#54233 = CARTESIAN_POINT ( 'NONE',  ( -4.589925132946514275, -63.93473983707485786, 3.864926970398267603 ) ) ;
#54234 = CARTESIAN_POINT ( 'NONE',  ( 51.48757442383973881, 38.95383793068620548, -37.45149417477089315 ) ) ;
#54235 = CARTESIAN_POINT ( 'NONE',  ( -40.15309039158411508, 485.1828724906129082, -4.320808352504673877 ) ) ;
#54236 = CARTESIAN_POINT ( 'NONE',  ( 7.737898857161403576, 302.4298210949973509, -10.02991386142804231 ) ) ;
#54237 = CARTESIAN_POINT ( 'NONE',  ( 62.59984008646965492, -56.86289542963405808, 88.13664758048848569 ) ) ;
#54238 = VERTEX_POINT ( 'NONE', #90437 ) ;
#54239 = FACE_OUTER_BOUND ( 'NONE', #92124, .T. ) ;
#54240 = CARTESIAN_POINT ( 'NONE',  ( -76.12537862032631608, -38.35598417008158378, -28.58435412235099804 ) ) ;
#54241 = CARTESIAN_POINT ( 'NONE',  ( -42.68083702883377839, 436.2686870323770449, 7.148029379848837905 ) ) ;
#54242 = CARTESIAN_POINT ( 'NONE',  ( -9.383347720677482684, 51.32558664833128148, 3.724917079647517948 ) ) ;
#54243 = AXIS2_PLACEMENT_3D ( 'NONE', #80493, #62751, #48655 ) ;
#54244 = ORIENTED_EDGE ( 'NONE', *, *, #53710, .F. ) ;
#54245 =( NAMED_UNIT ( * ) PLANE_ANGLE_UNIT ( ) SI_UNIT ( $, .RADIAN. ) );
#54246 = DIRECTION ( 'NONE',  ( 0.5735764363510491570, -0.8191520442889895781, 1.003171929053522035E-16 ) ) ;
#54247 = CARTESIAN_POINT ( 'NONE',  ( -72.10178200369317381, -60.00000000000000711, -25.50777580964439650 ) ) ;
#54248 = AXIS2_PLACEMENT_3D ( 'NONE', #55413, #76648, #79175 ) ;
#54249 = FACE_OUTER_BOUND ( 'NONE', #82041, .T. ) ;
#54250 = EDGE_CURVE ( 'NONE', #70585, #86317, #73253, .T. ) ;
#54251 = MECHANICAL_DESIGN_GEOMETRIC_PRESENTATION_REPRESENTATION (  '', ( #35371 ), #81817 ) ;
#54252 = FACE_OUTER_BOUND ( 'NONE', #95799, .T. ) ;
#54253 = VECTOR ( 'NONE', #14178, 1000.000000000000227 ) ;
#54254 = CARTESIAN_POINT ( 'NONE',  ( 5.727634848076682772, 4.575561887447793019, -6.326622577870439912 ) ) ;
#54255 = CARTESIAN_POINT ( 'NONE',  ( 86.05395271266333168, -39.20869856352000937, 187.0836467292549514 ) ) ;
#54256 = CARTESIAN_POINT ( 'NONE',  ( 67.48317336153286305, 6.856755485862130937E-15, 0.000000000000000000 ) ) ;
#54257 = CARTESIAN_POINT ( 'NONE',  ( -9.993721417938997931, 7.509139500188190652, 0.000000000000000000 ) ) ;
#54258 = CARTESIAN_POINT ( 'NONE',  ( 87.04245038058458306, 5.000000000000023093, 6.123233995736781074E-16 ) ) ;
#54259 = CARTESIAN_POINT ( 'NONE',  ( 61.40732561923240951, -29.45172577994906860, -24.51876011215350104 ) ) ;
#54260 = PRESENTATION_STYLE_ASSIGNMENT (( #96359 ) ) ;
#54261 = CARTESIAN_POINT ( 'NONE',  ( 5.947762761376474749, -2.501851166488376688, 6.500000000000000000 ) ) ;
#54262 = CARTESIAN_POINT ( 'NONE',  ( 34.17980567228813271, 435.1524039838096201, 10.79291224410167338 ) ) ;
#54263 =( BOUNDED_SURFACE ( )  B_SPLINE_SURFACE ( 3, 2, ( 
 ( #46301, #45765, #12322 ),
 ( #102944, #28553, #70581 ),
 ( #11786, #79190, #78126 ),
 ( #77605, #20493, #22041 ),
 ( #45247, #78641, #53331 ),
 ( #103988, #53848, #54352 ),
 ( #4245, #86779, #61434 ),
 ( #29108, #12848, #38234 ),
 ( #4779, #52787, #44716 ),
 ( #103468, #71098, #29617 ),
 ( #86250, #3723, #11247 ),
 ( #94330, #30132, #60898 ),
 ( #63018, #95916, #62489 ),
 ( #3179, #28029, #54897 ),
 ( #95380, #68994, #21518 ),
 ( #44176, #77065, #101869 ),
 ( #93788, #36653, #19947 ),
 ( #65666, #55942, #88881 ),
 ( #88359, #6888, #56492 ),
 ( #14970, #47867, #5827 ),
 ( #13907, #55426, #30673 ),
 ( #105069, #48403, #81293 ),
 ( #105584, #80773, #38748 ),
 ( #64610, #31724, #98547 ),
 ( #81819, #96970, #32249 ),
 ( #106641, #32792, #14435 ),
 ( #24698, #97479, #46821 ),
 ( #89421, #23634, #39809 ),
 ( #89936, #15513, #72683 ),
 ( #7409, #39283, #40322 ),
 ( #47345, #57022, #73199 ),
 ( #106101, #72161, #65130 ),
 ( #16043, #7943, #48923 ),
 ( #98026, #24178, #40849 ),
 ( #73742, #87828, #79718 ),
 ( #71617, #104519, #63559 ),
 ( #96452, #22589, #80237 ),
 ( #6341, #31209, #64094 ),
 ( #23105, #18200, #67794 ),
 ( #50521, #82374, #83971 ),
 ( #75337, #68332, #57548 ),
 ( #41914, #2513, #50006 ),
 ( #83436, #1438, #90469 ),
 ( #26320, #16581, #99615 ),
 ( #58648, #33319, #59717 ),
 ( #91550, #99072, #9534 ),
 ( #10082, #74800, #25236 ),
 ( #17658, #92592, #67275 ),
 ( #9008, #75879, #42446 ),
 ( #51597, #18748, #42991 ),
 ( #34399, #100155, #59181 ),
 ( #1979, #8481, #92060 ),
 ( #84516, #66191, #49467 ),
 ( #10605, #66731, #34926 ),
 ( #882, #100680, #33859 ),
 ( #51054, #26846, #43523 ),
 ( #76399, #58093, #91022 ),
 ( #35460, #101229, #41386 ),
 ( #74277, #17128, #351 ),
 ( #25792, #82911, #11126 ),
 ( #94748, #20898, #53210 ),
 ( #78530, #70458, #94200 ),
 ( #3055, #53732, #37056 ),
 ( #12730, #45133, #44596 ),
 ( #61851, #68877, #86660 ),
 ( #103355, #77486, #3598 ),
 ( #101750, #102282, #86130 ),
 ( #36535, #69400, #19304 ),
 ( #27384, #36005, #44052 ),
 ( #27920, #20370, #45653 ),
 ( #28430, #60783, #93673 ),
 ( #4661, #12203, #28985 ),
 ( #19824, #60264, #78010 ),
 ( #61311, #4127, #52659 ),
 ( #69924, #85590, #37595 ),
 ( #29503, #93133, #102823 ),
 ( #11664, #52128, #85044 ),
 ( #76942, #51393, #91868 ),
 ( #27170, #50330, #51925 ),
 ( #101555, #17993, #50854 ) ),
 .UNSPECIFIED., .F., .F., .F. ) 
 B_SPLINE_SURFACE_WITH_KNOTS ( ( 4, 2, 2, 2, 2, 2, 2, 2, 2, 2, 2, 2, 2, 2, 2, 2, 2, 2, 2, 2, 2, 2, 2, 2, 2, 2, 2, 2, 2, 2, 2, 2, 2, 2, 2, 2, 2, 2, 2, 4 ),
 ( 3, 3 ),
 ( 0.07172314469012842919, 0.08973265255323484291, 0.1077421604163412705, 0.1257516682794476703, 0.1347564222110008703, 0.1437611761425540979, 0.1617706840056605255, 0.1707754379372137254, 0.1797801918687669254, 0.1820313803516552253, 0.1842825688345435253, 0.1887849458003201253, 0.1932873227660967252, 0.1955385112489850252, 0.1977896997318733252, 0.1989152939733174752, 0.1994780910940395502, 0.2000408882147616252, 0.2022920766976499252, 0.2045432651805382251, 0.2051060623012603001, 0.2053874608616213515, 0.2056688594219823751, 0.2067944536634265251, 0.2079200479048706751, 0.2080607471850511869, 0.2082014464652316987, 0.2084828450255927501, 0.2090456421463148251, 0.2101712363877589751, 0.2104526349481199987, 0.2107340335084810501, 0.2112968306292031251, 0.2124224248706472751, 0.2129852219913693501, 0.2130555716314596060, 0.2131259212715498896, 0.2132666205517304014, 0.2135480191120914251, 0.2157992075949797528 ),
 ( 0.000000000000000000, 1.000000000000000000 ),
 .UNSPECIFIED. ) 
 GEOMETRIC_REPRESENTATION_ITEM ( )  RATIONAL_B_SPLINE_SURFACE ( (
 ( 1.000000000000000000, 0.7071066916777324352, 1.000000000000000000),
 ( 1.000000000000000000, 0.7071066384723879716, 1.000000000000000000),
 ( 1.000000000000000000, 0.7071067819036740421, 1.000000000000000000),
 ( 1.000000000000000000, 0.7071067819036740421, 1.000000000000000000),
 ( 1.000000000000000000, 0.7071067821253883556, 1.000000000000000000),
 ( 1.000000000000000000, 0.7071067821253883556, 1.000000000000000000),
 ( 1.000000000000000000, 0.7071082347912200916, 1.000000000000000000),
 ( 1.000000000000000000, 0.7071090860269371170, 1.000000000000000000),
 ( 1.000000000000000000, 0.7071085999063239091, 1.000000000000000000),
 ( 1.000000000000000000, 0.7071071393025897267, 1.000000000000000000),
 ( 1.000000000000000000, 0.7071064603873742360, 1.000000000000000000),
 ( 1.000000000000000000, 0.7071084468636777975, 1.000000000000000000),
 ( 1.000000000000000000, 0.7071099459167716761, 1.000000000000000000),
 ( 1.000000000000000000, 0.7071070620195699652, 1.000000000000000000),
 ( 1.000000000000000000, 0.7071067638254444621, 1.000000000000000000),
 ( 1.000000000000000000, 0.7071094983174432969, 1.000000000000000000),
 ( 1.000000000000000000, 0.7071073521351076696, 1.000000000000000000),
 ( 1.000000000000000000, 0.7071067110094644281, 1.000000000000000000),
 ( 1.000000000000000000, 0.7071074718365022438, 1.000000000000000000),
 ( 1.000000000000000000, 0.7071137944410639253, 1.000000000000000000),
 ( 1.000000000000000000, 0.7071181761060342241, 1.000000000000000000),
 ( 1.000000000000000000, 0.7071288868279509421, 1.000000000000000000),
 ( 1.000000000000000000, 0.7071314869358752420, 1.000000000000000000),
 ( 1.000000000000000000, 0.7071211158780618122, 1.000000000000000000),
 ( 1.000000000000000000, 0.7071075228484042796, 1.000000000000000000),
 ( 1.000000000000000000, 0.7071064472611667817, 1.000000000000000000),
 ( 1.000000000000000000, 0.7071094939932405232, 1.000000000000000000),
 ( 1.000000000000000000, 0.7071117979890746419, 1.000000000000000000),
 ( 1.000000000000000000, 0.7071112387139774080, 1.000000000000000000),
 ( 1.000000000000000000, 0.7071089882604711940, 1.000000000000000000),
 ( 1.000000000000000000, 0.7071080815320003321, 1.000000000000000000),
 ( 1.000000000000000000, 0.7071071532410159177, 1.000000000000000000),
 ( 1.000000000000000000, 0.7071069183921528944, 1.000000000000000000),
 ( 1.000000000000000000, 0.7071067316882134746, 1.000000000000000000),
 ( 1.000000000000000000, 0.7071072160745824897, 1.000000000000000000),
 ( 1.000000000000000000, 0.7071281552871109266, 1.000000000000000000),
 ( 1.000000000000000000, 0.7071788308493717201, 1.000000000000000000),
 ( 1.000000000000000000, 0.7072040914959526470, 1.000000000000000000),
 ( 1.000000000000000000, 0.7071729554399738271, 1.000000000000000000),
 ( 1.000000000000000000, 0.7071271541534743799, 1.000000000000000000),
 ( 1.000000000000000000, 0.7071184695976129309, 1.000000000000000000),
 ( 1.000000000000000000, 0.7071100320398184813, 1.000000000000000000),
 ( 1.000000000000000000, 0.7071080004622726234, 1.000000000000000000),
 ( 1.000000000000000000, 0.7071063588341449657, 1.000000000000000000),
 ( 1.000000000000000000, 0.7071068098800528112, 1.000000000000000000),
 ( 1.000000000000000000, 0.7071083434742995166, 1.000000000000000000),
 ( 1.000000000000000000, 0.7071118442609979349, 1.000000000000000000),
 ( 1.000000000000000000, 0.7071122315782686352, 1.000000000000000000),
 ( 1.000000000000000000, 0.7071084657487585190, 1.000000000000000000),
 ( 1.000000000000000000, 0.7071069086593241293, 1.000000000000000000),
 ( 1.000000000000000000, 0.7071067970953980319, 1.000000000000000000),
 ( 1.000000000000000000, 0.7071067683750767996, 1.000000000000000000),
 ( 1.000000000000000000, 0.7071066806290805529, 1.000000000000000000),
 ( 1.000000000000000000, 0.7071060773180442016, 1.000000000000000000),
 ( 1.000000000000000000, 0.7071053327435640190, 1.000000000000000000),
 ( 1.000000000000000000, 0.7071028992638964672, 1.000000000000000000),
 ( 1.000000000000000000, 0.7071010927699721282, 1.000000000000000000),
 ( 1.000000000000000000, 0.7070987750015783613, 1.000000000000000000),
 ( 1.000000000000000000, 0.7071026859636611039, 1.000000000000000000),
 ( 1.000000000000000000, 0.7071061702207726007, 1.000000000000000000),
 ( 1.000000000000000000, 0.7071067000110781153, 1.000000000000000000),
 ( 1.000000000000000000, 0.7071068455174084333, 1.000000000000000000),
 ( 1.000000000000000000, 0.7071077971994959022, 1.000000000000000000),
 ( 1.000000000000000000, 0.7071127875002619634, 1.000000000000000000),
 ( 1.000000000000000000, 0.7071176651463569884, 1.000000000000000000),
 ( 1.000000000000000000, 0.7071258132918983863, 1.000000000000000000),
 ( 1.000000000000000000, 0.7071208017052891259, 1.000000000000000000),
 ( 1.000000000000000000, 0.7071102148083360239, 1.000000000000000000),
 ( 1.000000000000000000, 0.7071068024654432183, 1.000000000000000000),
 ( 1.000000000000000000, 0.7071067786309011005, 1.000000000000000000),
 ( 1.000000000000000000, 0.7071068737807520987, 1.000000000000000000),
 ( 1.000000000000000000, 0.7071072399035752687, 1.000000000000000000),
 ( 1.000000000000000000, 0.7071075080362204668, 1.000000000000000000),
 ( 1.000000000000000000, 0.7071085168092843265, 1.000000000000000000),
 ( 1.000000000000000000, 0.7071094604126808569, 1.000000000000000000),
 ( 1.000000000000000000, 0.7071127524153103527, 1.000000000000000000),
 ( 1.000000000000000000, 0.7071155430753355287, 1.000000000000000000),
 ( 1.000000000000000000, 0.7071398610474239899, 1.000000000000000000),
 ( 1.000000000000000000, 0.7071223203621870290, 1.000000000000000000),
 ( 1.000000000000000000, 0.7071067811865479058, 1.000000000000000000) ) ) 
 REPRESENTATION_ITEM ( '' )  SURFACE ( )  );
#54264 = CARTESIAN_POINT ( 'NONE',  ( -100.8172700586428618, -29.99999999999999645, 180.0901824726140035 ) ) ;
#54265 = EDGE_CURVE ( 'NONE', #41982, #42449, #91851, .T. ) ;
#54266 = CARTESIAN_POINT ( 'NONE',  ( -32.17646412119387378, 464.6980787822280377, 10.84896803612861227 ) ) ;
#54267 = CARTESIAN_POINT ( 'NONE',  ( 19.20286887953066923, -57.67181979952086124, 42.11251578178057287 ) ) ;
#54268 = CARTESIAN_POINT ( 'NONE',  ( 10.12220134229128732, 44.02984809270889599, 12.90779740156146538 ) ) ;
#54269 = CARTESIAN_POINT ( 'NONE',  ( -19.51721550458913512, 41.98713167543638036, -83.66826477877489765 ) ) ;
#54270 = FACE_OUTER_BOUND ( 'NONE', #24020, .T. ) ;
#54271 = CARTESIAN_POINT ( 'NONE',  ( 2.848917157793759055E-13, 44.08548369317517768, 16.24999999999732836 ) ) ;
#54272 = DIRECTION ( 'NONE',  ( 0.000000000000000000, 0.000000000000000000, -1.000000000000000000 ) ) ;
#54273 = DIRECTION ( 'NONE',  ( -0.000000000000000000, -1.000000000000000000, -0.000000000000000000 ) ) ;
#54274 = EDGE_CURVE ( 'NONE', #35120, #61182, #94580, .T. ) ;
#54275 = CARTESIAN_POINT ( 'NONE',  ( -86.77107750842486666, -57.39365593820878075, 193.7434059132478978 ) ) ;
#54276 = ORIENTED_EDGE ( 'NONE', *, *, #16673, .F. ) ;
#54277 = CARTESIAN_POINT ( 'NONE',  ( 38.94709829052286665, 485.6592143718137891, -4.427571171338303913 ) ) ;
#54278 = CARTESIAN_POINT ( 'NONE',  ( 42.10086803841213765, 435.6552064019005570, 19.95582312411065828 ) ) ;
#54279 = CARTESIAN_POINT ( 'NONE',  ( -12.35491406422132776, -35.99458353833710333, 29.94231072834120155 ) ) ;
#54280 = CIRCLE ( 'NONE', #35410, 60.00000000000000000 ) ;
#54281 = EDGE_CURVE ( 'NONE', #102808, #42645, #18160, .T. ) ;
#54283 = CARTESIAN_POINT ( 'NONE',  ( 40.53597741959072920, 485.1143729953953994, -4.195250914663321673 ) ) ;
#54282 = CARTESIAN_POINT ( 'NONE',  ( -103.9455512838813718, -60.00000000000002842, 141.2845372866246123 ) ) ;
#54284 = ORIENTED_EDGE ( 'NONE', *, *, #56506, .F. ) ;
#54286 =( NAMED_UNIT ( * ) PLANE_ANGLE_UNIT ( ) SI_UNIT ( $, .RADIAN. ) );
#54285 = B_SPLINE_CURVE_WITH_KNOTS ( 'NONE', 3,
 ( #55254, #54719, #27990, #5655 ),
 .UNSPECIFIED., .F., .F.,
 ( 4, 4 ),
 ( 0.000000000000000000, 0.001193002000561244275 ),
 .UNSPECIFIED. ) ;
#54287 = CARTESIAN_POINT ( 'NONE',  ( 42.61340452791776556, 486.8925439250688783, 7.464118458850346194 ) ) ;
#54288 = DIRECTION ( 'NONE',  ( -1.000000000000000000, -1.224606353822377258E-16, -0.000000000000000000 ) ) ;
#54289 = CARTESIAN_POINT ( 'NONE',  ( 53.78349330513380266, -4.000000000000000888, 4.898587196589422689E-16 ) ) ;
#54290 = VERTEX_POINT ( 'NONE', #59677 ) ;
#54291 = CARTESIAN_POINT ( 'NONE',  ( 32.45420636192083919, 439.3281579392075855, 23.70224716321920511 ) ) ;
#54292 = CARTESIAN_POINT ( 'NONE',  ( -34.62906189774859200, 434.6650141781096295, 8.921436296112648989 ) ) ;
#54294 = CYLINDRICAL_SURFACE ( 'NONE', #39056, 5.000000000000002665 ) ;
#54293 =( LENGTH_UNIT ( ) NAMED_UNIT ( * ) SI_UNIT ( .MILLI., .METRE. ) );
#54295 = DIRECTION ( 'NONE',  ( 0.000000000000000000, -1.000000000000000000, 0.000000000000000000 ) ) ;
#54296 = ORIENTED_EDGE ( 'NONE', *, *, #36439, .T. ) ;
#54297 = AXIS2_PLACEMENT_3D ( 'NONE', #27682, #93444, #61079 ) ;
#54298 = ADVANCED_FACE ( 'NONE', ( #35424 ), #90980, .T. ) ;
#54299 = VERTEX_POINT ( 'NONE', #17627 ) ;
#54300 = CARTESIAN_POINT ( 'NONE',  ( -28.61915886549734367, 318.3715675768729056, 12.26331061709428205 ) ) ;
#54301 = VERTEX_POINT ( 'NONE', #101190 ) ;
#54302 = PRESENTATION_STYLE_ASSIGNMENT (( #21464 ) ) ;
#54303 = CARTESIAN_POINT ( 'NONE',  ( 21.08349330513380693, 1.593028355512270962E-15, 0.000000000000000000 ) ) ;
#54304 = CARTESIAN_POINT ( 'NONE',  ( 27.33349330513380693, 1.593028355512270962E-15, 0.000000000000000000 ) ) ;
#54305 = ORIENTED_EDGE ( 'NONE', *, *, #98498, .F. ) ;
#54306 = AXIS2_PLACEMENT_3D ( 'NONE', #32253, #25242, #49474 ) ;
#54307 = DIRECTION ( 'NONE',  ( -1.000000000000000000, -1.224606353822377258E-16, -0.000000000000000000 ) ) ;
#54308 = CARTESIAN_POINT ( 'NONE',  ( -6.914762185086790858, 41.79847498657338889, -69.55926089113090427 ) ) ;
#54309 = CARTESIAN_POINT ( 'NONE',  ( -76.85716460373025427, -60.00000000000000711, 196.0240674832539582 ) ) ;
#54310 = CARTESIAN_POINT ( 'NONE',  ( 17.81438722625302518, 5.000000000000003553, 0.000000000000000000 ) ) ;
#54311 = CARTESIAN_POINT ( 'NONE',  ( 24.77227526506132094, -60.00000000000001421, 41.10247213741922678 ) ) ;
#54312 = DIRECTION ( 'NONE',  ( 0.5735764363510468256, 0.8191520442889913545, 0.000000000000000000 ) ) ;
#54313 = CARTESIAN_POINT ( 'NONE',  ( -6.340295924924054916, 41.77218093381596020, -58.92363190012176233 ) ) ;
#54314 = AXIS2_PLACEMENT_3D ( 'NONE', #86097, #93640, #19789 ) ;
#54316 = CARTESIAN_POINT ( 'NONE',  ( 11.44797993206735853, -49.91577255025450199, 32.23882742997456319 ) ) ;
#54315 = CARTESIAN_POINT ( 'NONE',  ( -109.5929118004772818, -60.00000000000001421, 123.9174817212569621 ) ) ;
#54317 = CYLINDRICAL_SURFACE ( 'NONE', #91326, 5.000000000000002665 ) ;
#54318 = CARTESIAN_POINT ( 'NONE',  ( -48.17436038642846796, -56.82532612053482524, 53.30083711335295504 ) ) ;
#54319 = CARTESIAN_POINT ( 'NONE',  ( -7.109733192396789470, 41.69026681596732686, -59.69141549319190432 ) ) ;
#54320 = VERTEX_POINT ( 'NONE', #51019 ) ;
#54321 = CARTESIAN_POINT ( 'NONE',  ( 1.248924154308308054, 10.99719009875376230, -50.37041816597272259 ) ) ;
#54322 = AXIS2_PLACEMENT_3D ( 'NONE', #98499, #16527, #104473 ) ;
#54323 = CONICAL_SURFACE ( 'NONE', #95705, 3.309500000000001663, 0.9599310885968770357 ) ;
#54324 = DIRECTION ( 'NONE',  ( -0.000000000000000000, -0.000000000000000000, -1.000000000000000000 ) ) ;
#54325 = CARTESIAN_POINT ( 'NONE',  ( 4.472135954999580498, -10.00000000000000888, 4.000000000000000000 ) ) ;
#54326 = ORIENTED_EDGE ( 'NONE', *, *, #57418, .F. ) ;
#54327 = CARTESIAN_POINT ( 'NONE',  ( -5.719235665873437569, -7.817867488105560092, 13.77080619359168878 ) ) ;
#54328 = AXIS2_PLACEMENT_3D ( 'NONE', #21495, #23617, #39262 ) ;
#54329 = ORIENTED_EDGE ( 'NONE', *, *, #21272, .F. ) ;
#54330 = CARTESIAN_POINT ( 'NONE',  ( 89.79167478614425590, -30.00000000002385647, -11.58638050850938761 ) ) ;
#54331 = CARTESIAN_POINT ( 'NONE',  ( 46.00000000000000000, 459.9277931459794786, 6.461582622334601567 ) ) ;
#54332 = CARTESIAN_POINT ( 'NONE',  ( 0.000000000000000000, 0.000000000000000000, -6.418875477074183600 ) ) ;
#54333 = AXIS2_PLACEMENT_3D ( 'NONE', #65443, #56801, #89727 ) ;
#54334 = CARTESIAN_POINT ( 'NONE',  ( 51.76085035120648570, 42.00000000008225953, -29.83308852628573860 ) ) ;
#54335 = CARTESIAN_POINT ( 'NONE',  ( 100.1645178837010377, -30.00000000000000355, 184.8515023625643323 ) ) ;
#54336 = EDGE_CURVE ( 'NONE', #6761, #36922, #52267, .T. ) ;
#54337 = DIRECTION ( 'NONE',  ( -1.000000000000000000, -0.000000000000000000, -0.000000000000000000 ) ) ;
#54338 = ORIENTED_EDGE ( 'NONE', *, *, #90893, .T. ) ;
#54339 = VERTEX_POINT ( 'NONE', #100646 ) ;
#54340 = VERTEX_POINT ( 'NONE', #28808 ) ;
#54341 = CARTESIAN_POINT ( 'NONE',  ( -27.85348497893874509, 36.60125607490498112, 7.792768389110043437 ) ) ;
#54342 = LINE ( 'NONE', #96441, #95540 ) ;
#54343 = EDGE_CURVE ( 'NONE', #4192, #68930, #4014, .T. ) ;
#54344 = CARTESIAN_POINT ( 'NONE',  ( 3.364021409948656505, 294.8518027753228807, 9.936999415087239385 ) ) ;
#54345 = EDGE_LOOP ( 'NONE', ( #99023, #46376, #37145, #52782, #58958 ) ) ;
#54346 = DIRECTION ( 'NONE',  ( 0.000000000000000000, 0.000000000000000000, 1.000000000000000000 ) ) ;
#54347 = ORIENTED_EDGE ( 'NONE', *, *, #23274, .T. ) ;
#54348 = CARTESIAN_POINT ( 'NONE',  ( 101.7179331410454637, -38.44840262328585112, 199.8206546545780498 ) ) ;
#54349 = CARTESIAN_POINT ( 'NONE',  ( 11.60150500652189187, 15.64056042777739108, 9.649354197112575804 ) ) ;
#54350 = CARTESIAN_POINT ( 'NONE',  ( 86.16765823093783183, -60.13206058599219261, 8.614730465306884355 ) ) ;
#54351 = CARTESIAN_POINT ( 'NONE',  ( 6.169949891408688991, -6.308465495018778846, 2.073417244831591955 ) ) ;
#54352 = CARTESIAN_POINT ( 'NONE',  ( 42.78192394157753142, 397.2994584770452775, 19.86614811632973598 ) ) ;
#54353 = DIRECTION ( 'NONE',  ( -1.000000000000000000, -1.224606353822377258E-16, -0.000000000000000000 ) ) ;
#54354 = CARTESIAN_POINT ( 'NONE',  ( 0.000000000000000000, 4.000000000000003553, -10.00000000000003730 ) ) ;
#54355 = AXIS2_PLACEMENT_3D ( 'NONE', #56847, #105929, #6172 ) ;
#54356 = CARTESIAN_POINT ( 'NONE',  ( 3.105144143682717406, -0.5701562126480363979, 103.2828762868857098 ) ) ;
#54357 = ORIENTED_EDGE ( 'NONE', *, *, #32190, .T. ) ;
#54358 = ADVANCED_FACE ( 'NONE', ( #17091 ), #48800, .T. ) ;
#54359 = CARTESIAN_POINT ( 'NONE',  ( -3.313708498984765161, -10.15625000409677092, 7.999999999999998224 ) ) ;
#54360 = CARTESIAN_POINT ( 'NONE',  ( 57.70539558375507738, 6.856755485862130937E-15, 0.000000000000000000 ) ) ;
#54361 = CARTESIAN_POINT ( 'NONE',  ( -3.794355794024275585, 18.81003929889839554, 5.000000000000000000 ) ) ;
#54362 = ORIENTED_EDGE ( 'NONE', *, *, #58663, .F. ) ;
#54363 = DIRECTION ( 'NONE',  ( 0.000000000000000000, -1.000000000000000000, 0.000000000000000000 ) ) ;
#54364 = CARTESIAN_POINT ( 'NONE',  ( -33.40011937205945713, 300.9684309835628824, 3.319491984095645609 ) ) ;
#54365 = CARTESIAN_POINT ( 'NONE',  ( 26.84999999999999787, -3.309499999999999886, 4.475777889183790779E-16 ) ) ;
#54366 = SURFACE_SIDE_STYLE ('',( #99759 ) ) ;
#54367 = CARTESIAN_POINT ( 'NONE',  ( -3.313708498984760720, -21.03124999999999645, -8.000000000000000000 ) ) ;
#54368 = CARTESIAN_POINT ( 'NONE',  ( -37.98285244702580599, -27.77434865196162406, 44.84875665863523153 ) ) ;
#54369 = EDGE_CURVE ( 'NONE', #38361, #7404, #42408, .T. ) ;
#54370 = DIRECTION ( 'NONE',  ( 0.000000000000000000, -1.000000000000000000, 0.000000000000000000 ) ) ;
#54371 = VERTEX_POINT ( 'NONE', #1398 ) ;
#54372 = CARTESIAN_POINT ( 'NONE',  ( 84.73931994313983296, -39.38290620261815889, 182.5232074107245239 ) ) ;
#54373 = CARTESIAN_POINT ( 'NONE',  ( -37.72638201607069419, 27.54978895746880951, 13.45617127781066813 ) ) ;
#54374 = EDGE_CURVE ( 'NONE', #10253, #92720, #40990, .T. ) ;
#54375 = VECTOR ( 'NONE', #2039, 1000.000000000000000 ) ;
#54376 = DIRECTION ( 'NONE',  ( -1.000000000000000000, -1.224606353822377258E-16, -0.000000000000000000 ) ) ;
#54377 = VERTEX_POINT ( 'NONE', #38465 ) ;
#54378 = CARTESIAN_POINT ( 'NONE',  ( 94.43512559729094846, -57.67054883863127657, -0.6433801497298585748 ) ) ;
#54379 = DIRECTION ( 'NONE',  ( 0.4999999999999993339, 0.000000000000000000, 0.8660254037844390407 ) ) ;
#54380 = CARTESIAN_POINT ( 'NONE',  ( 11.46641754970814020, -5.000000000000002665, -75.26692388747053997 ) ) ;
#54381 = CARTESIAN_POINT ( 'NONE',  ( 3.490407211888509836E-12, -4.332980043422162808, 17.83347932686506354 ) ) ;
#54382 = CARTESIAN_POINT ( 'NONE',  ( 29.59409995734579368, 13.24979100942362109, 39.60535821593451544 ) ) ;
#54383 = EDGE_CURVE ( 'NONE', #80103, #72660, #9147, .T. ) ;
#54384 = AXIS2_PLACEMENT_3D ( 'NONE', #45278, #37204, #5345 ) ;
#54385 = DIRECTION ( 'NONE',  ( 0.04963565690953686271, 2.337787107298208023E-22, 0.9987673911192530563 ) ) ;
#54386 = AXIS2_PLACEMENT_3D ( 'NONE', #85011, #11095, #3023 ) ;
#54387 = CARTESIAN_POINT ( 'NONE',  ( 21.47514250170511474, -26.66870654467904345, 37.19702469120311150 ) ) ;
#54388 = SURFACE_STYLE_USAGE ( .BOTH. , #95411 ) ;
#54389 = CARTESIAN_POINT ( 'NONE',  ( 49.62245147187759642, -29.61487503896438156, 46.01461058099387458 ) ) ;
#54391 = CARTESIAN_POINT ( 'NONE',  ( -13.36211432089984008, 5.554967171257831460, 6.704703839142655220 ) ) ;
#54390 = DIRECTION ( 'NONE',  ( 0.000000000000000000, 0.000000000000000000, -1.000000000000000000 ) ) ;
#54392 = CARTESIAN_POINT ( 'NONE',  ( 42.99999999999997158, 487.9285348210859752, 8.903916466042435474 ) ) ;
#54393 = CARTESIAN_POINT ( 'NONE',  ( -15.39919601875319444, 44.07709767825076597, -5.261523372194803372 ) ) ;
#54394 = FACE_OUTER_BOUND ( 'NONE', #6775, .T. ) ;
#54395 = DIRECTION ( 'NONE',  ( 0.000000000000000000, 0.000000000000000000, 1.000000000000000000 ) ) ;
#54396 = AXIS2_PLACEMENT_3D ( 'NONE', #66409, #58324, #48618 ) ;
#54397 = MECHANICAL_DESIGN_GEOMETRIC_PRESENTATION_REPRESENTATION (  '', ( #83680 ), #81971 ) ;
#54398 = CARTESIAN_POINT ( 'NONE',  ( -84.68040789762383724, -38.00000000000000711, 42.85769669637753765 ) ) ;
#54399 = PRODUCT_DEFINITION_SHAPE ( 'NONE', 'NONE',  #106798 ) ;
#54400 = ORIENTED_EDGE ( 'NONE', *, *, #15396, .T. ) ;
#54401 = CARTESIAN_POINT ( 'NONE',  ( -9.784430647098096401, -3.383477514783840956, 15.02353616751815402 ) ) ;
#54402 = CARTESIAN_POINT ( 'NONE',  ( 1.224646799147357595E-15, 4.000000000000003553, 10.00000000000003730 ) ) ;
#54403 = CIRCLE ( 'NONE', #39058, 1.000000000000002887 ) ;
#54404 = DIRECTION ( 'NONE',  ( 0.000000000000000000, -1.000000000000000000, 0.000000000000000000 ) ) ;
#54405 = EDGE_CURVE ( 'NONE', #64598, #99558, #14314, .T. ) ;
#54407 = CARTESIAN_POINT ( 'NONE',  ( -9.323832755003198969, -21.77035872086719337, -30.31131560807224901 ) ) ;
#54406 = FACE_OUTER_BOUND ( 'NONE', #68603, .T. ) ;
#54408 = B_SPLINE_CURVE_WITH_KNOTS ( 'NONE', 3,
 ( #16528, #18148, #17611, #26794 ),
 .UNSPECIFIED., .F., .F.,
 ( 4, 4 ),
 ( 1.430489624538199204E-17, 0.001025896622541432783 ),
 .UNSPECIFIED. ) ;
#54409 = ORIENTED_EDGE ( 'NONE', *, *, #1301, .T. ) ;
#54410 = DIRECTION ( 'NONE',  ( -1.000000000000000000, -0.000000000000000000, -0.000000000000000000 ) ) ;
#54411 = DIRECTION ( 'NONE',  ( 0.000000000000000000, 0.8802307401770304018, 0.4745459346021176361 ) ) ;
#54412 = EDGE_LOOP ( 'NONE', ( #67969, #92428 ) ) ;
#54413 = ADVANCED_FACE ( 'NONE', ( #30373 ), #29330, .T. ) ;
#54414 = CARTESIAN_POINT ( 'NONE',  ( 6.289692432696588398, 5.239086202714920759, 4.583616368337912306 ) ) ;
#54415 = DIRECTION ( 'NONE',  ( 0.000000000000000000, -1.000000000000000000, 0.000000000000000000 ) ) ;
#54416 = CARTESIAN_POINT ( 'NONE',  ( -92.61211680020106485, -60.00000000000000000, -10.18716978393410599 ) ) ;
#54417 = VERTEX_POINT ( 'NONE', #46014 ) ;
#54418 = DIRECTION ( 'NONE',  ( 0.000000000000000000, -1.000000000000000000, 0.000000000000000000 ) ) ;
#54419 = SURFACE_SIDE_STYLE ('',( #21584 ) ) ;
#54420 = CARTESIAN_POINT ( 'NONE',  ( -9.334514330295430540, 28.21377262318213042, -3.588704711590614771 ) ) ;
#54421 = CARTESIAN_POINT ( 'NONE',  ( 13.58349330513380160, 1.593028355512270567E-15, 0.000000000000000000 ) ) ;
#54422 = CARTESIAN_POINT ( 'NONE',  ( -84.44835114658116026, -29.00614591161477662, 166.8971789934990682 ) ) ;
#54423 = VERTEX_POINT ( 'NONE', #78893 ) ;
#54424 = FACE_OUTER_BOUND ( 'NONE', #80495, .T. ) ;
#54425 = EDGE_CURVE ( 'NONE', #55271, #63533, #62220, .T. ) ;
#54426 = ORIENTED_EDGE ( 'NONE', *, *, #54948, .F. ) ;
#54427 = MECHANICAL_DESIGN_GEOMETRIC_PRESENTATION_REPRESENTATION (  '', ( #981 ), #9707 ) ;
#54428 = ORIENTED_EDGE ( 'NONE', *, *, #13163, .F. ) ;
#54429 = FACE_OUTER_BOUND ( 'NONE', #64970, .T. ) ;
#54430 = CARTESIAN_POINT ( 'NONE',  ( -6.060168961275133270, -62.82544565322023544, 14.37957135237512674 ) ) ;
#54431 = ORIENTED_EDGE ( 'NONE', *, *, #97106, .F. ) ;
#54432 =( LENGTH_UNIT ( ) NAMED_UNIT ( * ) SI_UNIT ( .MILLI., .METRE. ) );
#54433 = LINE ( 'NONE', #46893, #73643 ) ;
#54434 = CARTESIAN_POINT ( 'NONE',  ( -113.8744714263418842, -57.67115484533559311, 181.1306260539751918 ) ) ;
#54435 = CARTESIAN_POINT ( 'NONE',  ( -5.477432325710315908, -68.16479535570475434, 2.459915882346688232 ) ) ;
#54436 = CARTESIAN_POINT ( 'NONE',  ( 0.000000000000000000, -48.44948974278317877, 120.5000000000000000 ) ) ;
#54437 = CARTESIAN_POINT ( 'NONE',  ( -9.797372177749755551, 101.5349050515243619, 2.014953862275849161 ) ) ;
#54438 = CARTESIAN_POINT ( 'NONE',  ( -13.45079846400083312, -54.00000000000000711, 23.11721482942554928 ) ) ;
#54439 = CARTESIAN_POINT ( 'NONE',  ( -17.86230688873610006, 36.34004572609662631, -23.65428218925779902 ) ) ;
#54440 = CARTESIAN_POINT ( 'NONE',  ( 86.58060678326373250, -14.21045842199439235, 15.94037124058900901 ) ) ;
#54441 = CARTESIAN_POINT ( 'NONE',  ( -37.55014638933011639, -30.00000000000003553, 45.10809268468624111 ) ) ;
#54442 = CARTESIAN_POINT ( 'NONE',  ( -54.63826354663243734, -32.56309779981316410, 56.78580405707901235 ) ) ;
#54443 = ORIENTED_EDGE ( 'NONE', *, *, #52806, .F. ) ;
#54444 = CARTESIAN_POINT ( 'NONE',  ( 5.744562646538029504, 13.27049502477010101, -4.000000000000000000 ) ) ;
#54445 = ORIENTED_EDGE ( 'NONE', *, *, #36894, .T. ) ;
#54446 = CARTESIAN_POINT ( 'NONE',  ( -101.0425723163289007, -45.26379046336233358, 191.2487722153988727 ) ) ;
#54447 = CARTESIAN_POINT ( 'NONE',  ( -0.7854097470862259067, 51.35442182215429341, 9.986069114443392181 ) ) ;
#54448 = ORIENTED_EDGE ( 'NONE', *, *, #19349, .T. ) ;
#54449 = CARTESIAN_POINT ( 'NONE',  ( 18.93747938551456755, 49.20024086922183670, 62.06708146542941762 ) ) ;
#54450 = PRESENTATION_LAYER_ASSIGNMENT (  '', '', ( #73395 ) ) ;
#54451 = CARTESIAN_POINT ( 'NONE',  ( -11.28908492393962959, -60.00000000000002132, 39.66396576309020361 ) ) ;
#54452 = CARTESIAN_POINT ( 'NONE',  ( 9.165151389911681434, 85.00000000000001421, -4.000000000000000000 ) ) ;
#54453 = CARTESIAN_POINT ( 'NONE',  ( -7.188101187500000044, -15.78125000204838635, -8.802885111219163269E-16 ) ) ;
#54454 =( NAMED_UNIT ( * ) SI_UNIT ( $, .STERADIAN. ) SOLID_ANGLE_UNIT ( ) );
#54455 = PRESENTATION_STYLE_ASSIGNMENT (( #63119 ) ) ;
#54456 = CARTESIAN_POINT ( 'NONE',  ( -38.68218982724705057, 320.0845437455996603, 16.10279619727025135 ) ) ;
#54457 = CARTESIAN_POINT ( 'NONE',  ( -9.144505990959208575, 13.07246590495299721, 1.301042606982603743E-15 ) ) ;
#54458 = CARTESIAN_POINT ( 'NONE',  ( -1.100320091651754373, 34.84262691055438665, 27.88550462674917796 ) ) ;
#54459 = EDGE_CURVE ( 'NONE', #67790, #17802, #12714, .T. ) ;
#54460 = AXIS2_PLACEMENT_3D ( 'NONE', #34831, #66624, #68228 ) ;
#54461 = CARTESIAN_POINT ( 'NONE',  ( 5.656854249492378806, -24.68749999999999289, 5.656854249492381470 ) ) ;
#54462 = CARTESIAN_POINT ( 'NONE',  ( -26.45657344687305113, -18.61827304227935898, 28.46810496584365779 ) ) ;
#54463 = ORIENTED_EDGE ( 'NONE', *, *, #60113, .F. ) ;
#54464 = ORIENTED_EDGE ( 'NONE', *, *, #73366, .F. ) ;
#54465 = CARTESIAN_POINT ( 'NONE',  ( 48.15947195856908536, -22.22280960889669998, 42.58632823541661594 ) ) ;
#54466 = AXIS2_PLACEMENT_3D ( 'NONE', #75492, #34548, #65814 ) ;
#54467 = DIRECTION ( 'NONE',  ( 0.000000000000000000, 0.000000000000000000, 1.000000000000000000 ) ) ;
#54468 = EDGE_CURVE ( 'NONE', #34259, #45881, #16086, .T. ) ;
#54469 = CARTESIAN_POINT ( 'NONE',  ( 104.3757837139179117, -2.002967142162725287E-29, 5.000000000000011546 ) ) ;
#54470 = CARTESIAN_POINT ( 'NONE',  ( -104.5228042232798060, -38.40271399333908420, 197.9462138014538652 ) ) ;
#54471 = CIRCLE ( 'NONE', #20066, 3.309499999999999886 ) ;
#54472 = ORIENTED_EDGE ( 'NONE', *, *, #59776, .T. ) ;
#54473 = CONICAL_SURFACE ( 'NONE', #64814, 3.309500000000001663, 0.9599310885968770357 ) ;
#54474 = CARTESIAN_POINT ( 'NONE',  ( 89.02348576509739075, -38.38241123853795500, -18.01053637648232097 ) ) ;
#54475 = CARTESIAN_POINT ( 'NONE',  ( 12.29569164674513715, 5.691851931703239664, -8.450287346665382060 ) ) ;
#54476 = FACE_OUTER_BOUND ( 'NONE', #20209, .T. ) ;
#54477 = SURFACE_STYLE_USAGE ( .BOTH. , #97081 ) ;
#54479 =( LENGTH_UNIT ( ) NAMED_UNIT ( * ) SI_UNIT ( .MILLI., .METRE. ) );
#54478 = AXIS2_PLACEMENT_3D ( 'NONE', #46686, #54226, #96322 ) ;
#54480 = CARTESIAN_POINT ( 'NONE',  ( 5.231947904347590494, 41.12212780562299486, -70.85062122746499824 ) ) ;
#54481 = CARTESIAN_POINT ( 'NONE',  ( -32.10935363747667992, 436.4604647151550125, 19.52607623436714235 ) ) ;
#54482 =( GEOMETRIC_REPRESENTATION_CONTEXT ( 3 ) GLOBAL_UNCERTAINTY_ASSIGNED_CONTEXT ( ( #54740 ) ) GLOBAL_UNIT_ASSIGNED_CONTEXT ( ( #42655, #59935, #67478 ) ) REPRESENTATION_CONTEXT ( 'NONE', 'WORKASPACE' ) );
#54483 = CARTESIAN_POINT ( 'NONE',  ( -32.94539137533611495, 488.0149952105289799, 9.145905951731817751 ) ) ;
#54484 = CARTESIAN_POINT ( 'NONE',  ( 12.50000000000000711, -3.000000000000000000, -79.51734232575269345 ) ) ;
#54485 = CARTESIAN_POINT ( 'NONE',  ( 87.14226255876803862, -60.00000000000000000, 201.0601579501399385 ) ) ;
#54486 = VECTOR ( 'NONE', #79877, 1000.000000000000000 ) ;
#54487 =( NAMED_UNIT ( * ) SI_UNIT ( $, .STERADIAN. ) SOLID_ANGLE_UNIT ( ) );
#54488 = ORIENTED_EDGE ( 'NONE', *, *, #58723, .T. ) ;
#54489 = CARTESIAN_POINT ( 'NONE',  ( -33.79918201874539818, 300.9799874190337050, -0.6176716706728464512 ) ) ;
#54490 = EDGE_CURVE ( 'NONE', #35664, #55329, #3233, .T. ) ;
#54491 = CARTESIAN_POINT ( 'NONE',  ( 7.551892080562057075, 33.00987702539382695, 2.647003822403975359 ) ) ;
#54492 = CARTESIAN_POINT ( 'NONE',  ( -7.003653396366583905, 28.94293794440322642, -3.866846144092863202 ) ) ;
#54493 = VERTEX_POINT ( 'NONE', #27552 ) ;
#54495 = CARTESIAN_POINT ( 'NONE',  ( -6.231493956936419387, 147.8264543773111654, -5.000000000000000000 ) ) ;
#54494 = CARTESIAN_POINT ( 'NONE',  ( -91.47160050282491284, -38.38034665535289491, -5.985717668559722426 ) ) ;
#54496 = CARTESIAN_POINT ( 'NONE',  ( 46.00000000000000000, 438.4646224975062978, 9.895601460515761616 ) ) ;
#54497 = CARTESIAN_POINT ( 'NONE',  ( 5.947762761376473861, -4.378239541354662201, 5.416666666666666963 ) ) ;
#54498 = AXIS2_PLACEMENT_3D ( 'NONE', #43777, #76665, #65928 ) ;
#54499 = CARTESIAN_POINT ( 'NONE',  ( 5.290067270632322405, -1.200000000000000030E-05, 7.281152949374479100 ) ) ;
#54500 = CARTESIAN_POINT ( 'NONE',  ( 4.401442555609581635E-16, -11.65625000204838635, -7.188101187500000044 ) ) ;
#54501 = CARTESIAN_POINT ( 'NONE',  ( 8.737863884121436442, -3.000000000000002665, -90.03618980231149749 ) ) ;
#54502 = PRESENTATION_STYLE_ASSIGNMENT (( #70187 ) ) ;
#54504 = ORIENTED_EDGE ( 'NONE', *, *, #64030, .T. ) ;
#54503 = CARTESIAN_POINT ( 'NONE',  ( 6.575925811255158848, -3.850887307289502459, 6.669932470447524686 ) ) ;
#54505 = CARTESIAN_POINT ( 'NONE',  ( 82.99793886178632363, -42.97529097282338739, 175.1910793254024838 ) ) ;
#54507 = CIRCLE ( 'NONE', #8096, 0.5000000000000004441 ) ;
#54506 = CARTESIAN_POINT ( 'NONE',  ( 8.959992805873426391, 136.1288340877951839, -1.733336949948533988E-30 ) ) ;
#54508 = B_SPLINE_CURVE_WITH_KNOTS ( 'NONE', 3,
 ( #103819, #38578, #31036, #6715 ),
 .UNSPECIFIED., .F., .F.,
 ( 4, 4 ),
 ( 0.000000000000000000, 1.000000000000000000 ),
 .UNSPECIFIED. ) ;
#54509 = CARTESIAN_POINT ( 'NONE',  ( -34.79310559888947552, 439.9468627087276786, 24.33501443703186595 ) ) ;
#54510 = ORIENTED_EDGE ( 'NONE', *, *, #106717, .T. ) ;
#54511 = CARTESIAN_POINT ( 'NONE',  ( -37.61437702004904793, 372.0126153848854074, 4.442514472280413962 ) ) ;
#54512 = CARTESIAN_POINT ( 'NONE',  ( -46.77666182531606154, 18.74137236369755755, 15.58806238567861158 ) ) ;
#54513 = DIRECTION ( 'NONE',  ( 1.000000000000000000, -0.000000000000000000, -0.000000000000000000 ) ) ;
#54514 = DIRECTION ( 'NONE',  ( 0.000000000000000000, 0.000000000000000000, 1.000000000000000000 ) ) ;
#54515 = CARTESIAN_POINT ( 'NONE',  ( -34.19924320383960037, 42.71174251760211860, -63.48381379246026768 ) ) ;
#54516 = AXIS2_PLACEMENT_3D ( 'NONE', #46398, #46911, #104621 ) ;
#54517 = CYLINDRICAL_SURFACE ( 'NONE', #66361, 7.500000000000000000 ) ;
#54518 = EDGE_CURVE ( 'NONE', #21525, #2814, #21291, .T. ) ;
#54519 = ORIENTED_EDGE ( 'NONE', *, *, #76351, .F. ) ;
#54520 = CARTESIAN_POINT ( 'NONE',  ( -5.286264417172181318, 298.2069408986629355, 8.503413131156435156 ) ) ;
#54521 = CARTESIAN_POINT ( 'NONE',  ( 31.08349330513380337, 1.593028355512270567E-15, 0.000000000000000000 ) ) ;
#54522 = DIRECTION ( 'NONE',  ( 0.000000000000000000, 1.224646799147353207E-16, 1.000000000000000000 ) ) ;
#54524 = CARTESIAN_POINT ( 'NONE',  ( -13.46505580176244443, 5.376787718356499823, -6.519559750597839098 ) ) ;
#54523 = CARTESIAN_POINT ( 'NONE',  ( 34.86892506086162058, 473.1724825694047354, 16.84267233553793730 ) ) ;
#54525 = CARTESIAN_POINT ( 'NONE',  ( 2.977408999572650927, -21.87500000204838813, -7.188101187500001821 ) ) ;
#54526 = CARTESIAN_POINT ( 'NONE',  ( 9.789044728060206424, 294.6486233851416614, -2.043184600578050070 ) ) ;
#54527 = DIRECTION ( 'NONE',  ( -0.9133097175882186614, 0.1295276157526884797, -0.3861190962855272080 ) ) ;
#54528 = PRESENTATION_LAYER_ASSIGNMENT (  '', '', ( #95920 ) ) ;
#54529 = ITEM_DEFINED_TRANSFORMATION ( 'NONE', 'NONE', #95513,  #10728 ) ;
#54530 = EDGE_LOOP ( 'NONE', ( #23820, #27378, #69918, #72584 ) ) ;
#54531 = FILL_AREA_STYLE ('',( #21697 ) ) ;
#54532 = DIRECTION ( 'NONE',  ( 0.1091179629861610406, 0.9940288075069810825, 0.000000000000000000 ) ) ;
#54533 = CARTESIAN_POINT ( 'NONE',  ( -9.875464623904795403, 7.754124812996235683, -5.000000000000000000 ) ) ;
#54534 = CARTESIAN_POINT ( 'NONE',  ( 44.78945892759311675, 1.340359594676612611E-15, 0.000000000000000000 ) ) ;
#54535 = ADVANCED_FACE ( 'NONE', ( #36175, #102993 ), #68509, .F. ) ;
#54536 = CARTESIAN_POINT ( 'NONE',  ( -15.26104615578577928, 3.717029890783185575, 4.293899008437970899 ) ) ;
#54537 = ORIENTED_EDGE ( 'NONE', *, *, #73138, .T. ) ;
#54538 = SURFACE_STYLE_FILL_AREA ( #6003 ) ;
#54539 = DIRECTION ( 'NONE',  ( -0.8660191070795881796, -2.771849051803015643E-05, -0.5000109052858326963 ) ) ;
#54540 = CIRCLE ( 'NONE', #76898, 4.000000000000000888 ) ;
#54541 = VERTEX_POINT ( 'NONE', #4294 ) ;
#54542 = ADVANCED_FACE ( 'NONE', ( #52840 ), #33362, .T. ) ;
#54543 = LINE ( 'NONE', #87486, #16166 ) ;
#54544 = CARTESIAN_POINT ( 'NONE',  ( -3.473068986403389236, -0.8450860966016455755, 103.7454523020564920 ) ) ;
#54545 = CARTESIAN_POINT ( 'NONE',  ( -37.21429643540999876, 40.15975205826806160, -56.67536727291939513 ) ) ;
#54546 = UNCERTAINTY_MEASURE_WITH_UNIT (LENGTH_MEASURE( 1.000000000000000082E-05 ), #1217, 'distance_accuracy_value', 'NONE');
#54547 = CARTESIAN_POINT ( 'NONE',  ( -111.0778047984082804, -60.00000000000001421, 152.9011151817173015 ) ) ;
#54548 = PRODUCT_DEFINITION_SHAPE ( 'NONE', 'NONE',  #106817 ) ;
#54549 = VECTOR ( 'NONE', #37853, 1000.000000000000000 ) ;
#54550 = CIRCLE ( 'NONE', #83909, 3.500000000000000000 ) ;
#54551 = DIRECTION ( 'NONE',  ( -1.000000000000000000, -1.224606353822377258E-16, -0.000000000000000000 ) ) ;
#54552 = AXIS2_PLACEMENT_3D ( 'NONE', #106180, #47948, #14514 ) ;
#54553 = DIRECTION ( 'NONE',  ( 0.5735764363510554853, 0.8191520442889852482, 0.000000000000000000 ) ) ;
#54554 = DIRECTION ( 'NONE',  ( 0.000000000000000000, 0.000000000000000000, -1.000000000000000000 ) ) ;
#54555 = B_SPLINE_CURVE_WITH_KNOTS ( 'NONE', 3,
 ( #64254, #16741, #48027, #49632, #73363, #49087, #63725, #22746, #105227, #41545, #39447, #30840, #31373, #89577, #55583, #15146, #81989, #80937, #72836, #105747 ),
 .UNSPECIFIED., .F., .F.,
 ( 4, 2, 2, 2, 2, 2, 2, 2, 2, 4 ),
 ( 0.002407757697027169443, 0.002911641504507399801, 0.003415525311987630593, 0.004423292926948105622, 0.004927176734428342919, 0.005179118638168462435, 0.005431060541908580216, 0.005683002445648699733, 0.005934944349388818381, 0.006438828156869064352 ),
 .UNSPECIFIED. ) ;
#54556 = CARTESIAN_POINT ( 'NONE',  ( -13.00000000000003730, -10.00000000000000888, -4.000000000000000000 ) ) ;
#54557 = CARTESIAN_POINT ( 'NONE',  ( -82.22483725259803578, -60.77147558768366054, 188.6628005082894788 ) ) ;
#54558 = CARTESIAN_POINT ( 'NONE',  ( 39.07650750593464295, 42.03392408367576394, -56.77868393786336298 ) ) ;
#54559 = EDGE_CURVE ( 'NONE', #90625, #68858, #60432, .T. ) ;
#54560 = AXIS2_PLACEMENT_3D ( 'NONE', #85358, #59500, #92373 ) ;
#54561 =( BOUNDED_SURFACE ( )  B_SPLINE_SURFACE ( 3, 3, ( 
 ( #55993, #87351, #104038, #80286 ),
 ( #94920, #86826, #63613, #15025 ),
 ( #96502, #12895, #72730, #21057 ),
 ( #78696, #6399, #95427, #55472 ),
 ( #53896, #72215, #88934, #14480 ),
 ( #31773, #39334, #79766, #63069 ) ),
 .UNSPECIFIED., .F., .F., .F. ) 
 B_SPLINE_SURFACE_WITH_KNOTS ( ( 4, 1, 1, 4 ),
 ( 4, 4 ),
 ( 0.000000000000000000, 0.4213833399777465738, 0.5213833399777465516, 0.9843640123765011740 ),
 ( 0.000000000000000000, 1.000000000000000000 ),
 .UNSPECIFIED. ) 
 GEOMETRIC_REPRESENTATION_ITEM ( )  RATIONAL_B_SPLINE_SURFACE ( (
 ( 1.000000000000000000, 0.3333333333333334259, 0.3333333333333334259, 1.000000000000000000),
 ( 1.000000000000000000, 0.3333333333333334259, 0.3333333333333334259, 1.000000000000000000),
 ( 1.000000000000000000, 0.3333333333333334259, 0.3333333333333334259, 1.000000000000000000),
 ( 1.000000000000000000, 0.3333333333333334259, 0.3333333333333334259, 1.000000000000000000),
 ( 1.000000000000000000, 0.3333333333333334259, 0.3333333333333334259, 1.000000000000000000),
 ( 1.000000000000000000, 0.3333333333333334259, 0.3333333333333334259, 1.000000000000000000) ) ) 
 REPRESENTATION_ITEM ( '' )  SURFACE ( )  );
#54562 = ORIENTED_EDGE ( 'NONE', *, *, #79405, .T. ) ;
#54563 = DIRECTION ( 'NONE',  ( 1.000000000000000000, -0.000000000000000000, -0.000000000000000000 ) ) ;
#54564 = DIRECTION ( 'NONE',  ( 0.000000000000000000, -1.000000000000000000, 0.000000000000000000 ) ) ;
#54565 = CARTESIAN_POINT ( 'NONE',  ( -86.03344881383972620, -52.70846120426877235, 32.67016257065858298 ) ) ;
#54566 = CARTESIAN_POINT ( 'NONE',  ( -31.96880777819857045, 486.7849213999251674, 6.761697820930809399 ) ) ;
#54567 = CARTESIAN_POINT ( 'NONE',  ( -3.208653136615946977, 114.8595236971249705, -4.999999999999998224 ) ) ;
#54568 = CARTESIAN_POINT ( 'NONE',  ( 3.363266691732269109, 121.3108357054893958, -5.000000000000000000 ) ) ;
#54569 = CARTESIAN_POINT ( 'NONE',  ( -5.022013495303277786, 18.64316884711714550, 38.36535705883633085 ) ) ;
#54570 = CARTESIAN_POINT ( 'NONE',  ( 103.0033180414816343, -14.21045842199429643, 193.8537495780579150 ) ) ;
#54571 = CARTESIAN_POINT ( 'NONE',  ( -110.8742113967375928, -60.00000000000001421, 132.3764718065442594 ) ) ;
#54572 = CARTESIAN_POINT ( 'NONE',  ( -62.04700422542156701, -60.34632947214632992, 88.28556169221526773 ) ) ;
#54573 = VERTEX_POINT ( 'NONE', #85209 ) ;
#54574 = CARTESIAN_POINT ( 'NONE',  ( -62.81225381387285722, 38.95404345811080304, -10.80315792554570109 ) ) ;
#54575 = CARTESIAN_POINT ( 'NONE',  ( 100.7783224761645045, -60.00000000000495959, 204.1744434044741467 ) ) ;
#54576 = VERTEX_POINT ( 'NONE', #35637 ) ;
#54577 = CARTESIAN_POINT ( 'NONE',  ( 20.00100000000000122, 12.99999999999999289, 4.000000000000000000 ) ) ;
#54578 = CARTESIAN_POINT ( 'NONE',  ( -7.188101187500000933, -18.87500000204838457, -2.977408999572651371 ) ) ;
#54579 = CARTESIAN_POINT ( 'NONE',  ( 15.11650669486618881, 1.474610560812782335E-15, 0.000000000000000000 ) ) ;
#54580 = ORIENTED_EDGE ( 'NONE', *, *, #93204, .F. ) ;
#54581 = CARTESIAN_POINT ( 'NONE',  ( -8.000000000000000000, -27.03125000409677270, -3.313708498984762496 ) ) ;
#54582 = EDGE_LOOP ( 'NONE', ( #27922, #50471, #90561, #29828 ) ) ;
#54583 = DIRECTION ( 'NONE',  ( 0.000000000000000000, 0.000000000000000000, -1.000000000000000000 ) ) ;
#54584 = CARTESIAN_POINT ( 'NONE',  ( -40.66024587926896317, 485.8034863302605686, -4.843677042986813674 ) ) ;
#54585 = CARTESIAN_POINT ( 'NONE',  ( -92.04536671911790791, -60.00000000000000000, 5.198000682803741945 ) ) ;
#54586 = CARTESIAN_POINT ( 'NONE',  ( 36.36817526240515974, 355.1924107066273564, 1.711800795617328674 ) ) ;
#54587 = CARTESIAN_POINT ( 'NONE',  ( 7.188101187500001821, -31.43750000204839168, -2.977408999572650483 ) ) ;
#54588 = CARTESIAN_POINT ( 'NONE',  ( 32.10528697966002909, 486.1671898930081852, 5.449875171707255106 ) ) ;
#54589 = AXIS2_PLACEMENT_3D ( 'NONE', #19159, #10997, #36923 ) ;
#54590 = FACE_OUTER_BOUND ( 'NONE', #49562, .T. ) ;
#54591 = CARTESIAN_POINT ( 'NONE',  ( 7.996668422910687468, 48.00000000000000000, -78.85453279917973646 ) ) ;
#54592 = CARTESIAN_POINT ( 'NONE',  ( -7.002619243997878939, 106.0500731801381704, -3.868708944012999140 ) ) ;
#54593 = EDGE_CURVE ( 'NONE', #37271, #29166, #75761, .T. ) ;
#54594 = CARTESIAN_POINT ( 'NONE',  ( 30.49216875706506613, 308.5483047407621484, -8.695710891432577583 ) ) ;
#54595 = ORIENTED_EDGE ( 'NONE', *, *, #84019, .F. ) ;
#54596 = CARTESIAN_POINT ( 'NONE',  ( -9.306447067397133566, 53.68077726991365495, -1.766059074214993974 ) ) ;
#54597 = PRESENTATION_STYLE_ASSIGNMENT (( #79427 ) ) ;
#54598 = CARTESIAN_POINT ( 'NONE',  ( 33.35568202832040896, -42.96150302412274868, 35.15671921136284084 ) ) ;
#54599 = CARTESIAN_POINT ( 'NONE',  ( -17.78317311657527000, -3.867350551647862515E-12, 13.66642973271121342 ) ) ;
#54600 = ORIENTED_EDGE ( 'NONE', *, *, #1884, .F. ) ;
#54601 = ADVANCED_FACE ( 'NONE', ( #60949 ), #74591, .T. ) ;
#54602 = EDGE_CURVE ( 'NONE', #104211, #2575, #77119, .T. ) ;
#54603 = ORIENTED_EDGE ( 'NONE', *, *, #81449, .T. ) ;
#54605 = DIRECTION ( 'NONE',  ( -1.000000000000000000, -0.000000000000000000, -0.000000000000000000 ) ) ;
#54604 = CARTESIAN_POINT ( 'NONE',  ( 7.435358954047280200, -4.999999999999999112, -15.55677955364923726 ) ) ;
#54606 = DIRECTION ( 'NONE',  ( -1.000000000000000000, -1.224606353822377258E-16, -0.000000000000000000 ) ) ;
#54607 =( NAMED_UNIT ( * ) SI_UNIT ( $, .STERADIAN. ) SOLID_ANGLE_UNIT ( ) );
#54609 = CONICAL_SURFACE ( 'NONE', #87364, 4.000000000000001776, 0.9599310885968808105 ) ;
#54608 = CARTESIAN_POINT ( 'NONE',  ( -49.24259736700098244, 13.36037099746783596, -15.29523612018324741 ) ) ;
#54610 = DIRECTION ( 'NONE',  ( -1.000000000000000000, -1.224606353822377258E-16, -0.000000000000000000 ) ) ;
#54611 = ORIENTED_EDGE ( 'NONE', *, *, #93699, .T. ) ;
#54612 = CARTESIAN_POINT ( 'NONE',  ( 100.7803950627615279, -60.00000000000000711, 85.61164634517442096 ) ) ;
#54613 = DIRECTION ( 'NONE',  ( 0.000000000000000000, 0.000000000000000000, 1.000000000000000000 ) ) ;
#54614 = CARTESIAN_POINT ( 'NONE',  ( 106.4000000000000057, 0.000000000000000000, 4.171999999999999709 ) ) ;
#54615 = DIRECTION ( 'NONE',  ( 0.000000000000000000, -1.000000000000000000, 0.000000000000000000 ) ) ;
#54616 = CARTESIAN_POINT ( 'NONE',  ( -12.90950653571874440, 8.668901470952793176, -9.019737229616362484 ) ) ;
#54617 = ORIENTED_EDGE ( 'NONE', *, *, #52938, .T. ) ;
#54618 = EDGE_CURVE ( 'NONE', #62868, #8297, #53381, .T. ) ;
#54619 = CARTESIAN_POINT ( 'NONE',  ( -90.65468487766462147, -30.00000000010611956, 35.87486351368138315 ) ) ;
#54620 = ORIENTED_EDGE ( 'NONE', *, *, #16070, .T. ) ;
#54621 = SURFACE_STYLE_FILL_AREA ( #46559 ) ;
#54622 =( NAMED_UNIT ( * ) PLANE_ANGLE_UNIT ( ) SI_UNIT ( $, .RADIAN. ) );
#54623 = DIRECTION ( 'NONE',  ( 0.000000000000000000, -1.000000000000000000, 0.000000000000000000 ) ) ;
#54624 = CARTESIAN_POINT ( 'NONE',  ( 16.14328335387614644, 20.70972091798899228, -4.174903250152583567 ) ) ;
#54626 = SURFACE_STYLE_FILL_AREA ( #20757 ) ;
#54625 = CIRCLE ( 'NONE', #4692, 5.000000000000000888 ) ;
#54627 = CONICAL_SURFACE ( 'NONE', #75264, 4.172000000000009479, 0.9599310885968813656 ) ;
#54628 = CARTESIAN_POINT ( 'NONE',  ( -5.082755093536325042, -29.46875000204838813, -5.082755093536325930 ) ) ;
#54629 = CARTESIAN_POINT ( 'NONE',  ( 25.53945892759312031, 1.340359594676612611E-15, 0.000000000000000000 ) ) ;
#54630 = DIRECTION ( 'NONE',  ( 0.000000000000000000, -1.000000000000000000, 0.000000000000000000 ) ) ;
#54631 = EDGE_CURVE ( 'NONE', #80260, #3027, #10637, .T. ) ;
#54632 = DIRECTION ( 'NONE',  ( -0.000000000000000000, -0.000000000000000000, -1.000000000000000000 ) ) ;
#54633 = VERTEX_POINT ( 'NONE', #85622 ) ;
#54634 = PRESENTATION_LAYER_ASSIGNMENT (  '', '', ( #101162 ) ) ;
#54635 = VECTOR ( 'NONE', #62291, 1000.000000000000000 ) ;
#54636 =( GEOMETRIC_REPRESENTATION_CONTEXT ( 3 ) GLOBAL_UNCERTAINTY_ASSIGNED_CONTEXT ( ( #67505 ) ) GLOBAL_UNIT_ASSIGNED_CONTEXT ( ( #27572, #18392, #93327 ) ) REPRESENTATION_CONTEXT ( 'NONE', 'WORKASPACE' ) );
#54637 = CONICAL_SURFACE ( 'NONE', #28924, 4.000000000000001776, 0.9599310885968808105 ) ;
#54639 = ORIENTED_EDGE ( 'NONE', *, *, #26635, .F. ) ;
#54638 = DIRECTION ( 'NONE',  ( 0.000000000000000000, -1.000000000000000000, 0.000000000000000000 ) ) ;
#54640 = CARTESIAN_POINT ( 'NONE',  ( 76.89198577027414672, -56.84083229141209159, 144.4104520508552696 ) ) ;
#54641 = CARTESIAN_POINT ( 'NONE',  ( 14.59561887823619131, 1.699647480220895179, -3.448601310181623081 ) ) ;
#54642 = ORIENTED_EDGE ( 'NONE', *, *, #84789, .F. ) ;
#54643 = CARTESIAN_POINT ( 'NONE',  ( -12.50000000000000533, 35.89804743376623719, -55.74191270041429647 ) ) ;
#54644 = CONICAL_SURFACE ( 'NONE', #68459, 3.309500000000001663, 0.9599310885968770357 ) ;
#54645 = CARTESIAN_POINT ( 'NONE',  ( 7.212994264445060644, -87.01711344340040455, 3.463766307298588032 ) ) ;
#54646 = CARTESIAN_POINT ( 'NONE',  ( -7.188101187500000933, -21.50000000204839523, -2.977408999572651371 ) ) ;
#54647 = CARTESIAN_POINT ( 'NONE',  ( -4.852941176470598528, -3.000000000000002665, -70.80672828634229177 ) ) ;
#54648 = FACE_OUTER_BOUND ( 'NONE', #41453, .T. ) ;
#54649 = ORIENTED_EDGE ( 'NONE', *, *, #16241, .F. ) ;
#54650 = SURFACE_STYLE_USAGE ( .BOTH. , #78945 ) ;
#54651 = DIRECTION ( 'NONE',  ( 0.000000000000000000, 1.000000000000000000, 0.000000000000000000 ) ) ;
#54652 = CARTESIAN_POINT ( 'NONE',  ( -5.192560085536414682, -12.64305442631242826, 3.013051918867554413 ) ) ;
#54653 = CARTESIAN_POINT ( 'NONE',  ( -9.165151389911683211, 84.73289218717086158, -3.999999999999998224 ) ) ;
#54654 = DIRECTION ( 'NONE',  ( 0.000000000000000000, -0.9846968979781752784, 0.1742756985702797745 ) ) ;
#54655 = AXIS2_PLACEMENT_3D ( 'NONE', #83817, #50907, #51451 ) ;
#54656 = CARTESIAN_POINT ( 'NONE',  ( -5.656854249492381470, -10.25000000409677092, 5.656854249492379694 ) ) ;
#54657 = CARTESIAN_POINT ( 'NONE',  ( -33.81503581996810226, -23.50581328268117076, 33.08946069656037992 ) ) ;
#54658 = FACE_OUTER_BOUND ( 'NONE', #15850, .T. ) ;
#54659 = DIRECTION ( 'NONE',  ( 0.000000000000000000, -1.000000000000000000, 0.000000000000000000 ) ) ;
#54660 = VECTOR ( 'NONE', #91115, 1000.000000000000000 ) ;
#54661 = B_SPLINE_CURVE_WITH_KNOTS ( 'NONE', 3,
 ( #16805, #49146, #41610, #33015, #1114, #17883 ),
 .UNSPECIFIED., .F., .F.,
 ( 4, 2, 4 ),
 ( 0.01390592816464531790, 0.01784842065628996707, 0.02179091314793461798 ),
 .UNSPECIFIED. ) ;
#54662 = CARTESIAN_POINT ( 'NONE',  ( 7.499999999943863571, 33.41357786079682768, -51.06910100954272735 ) ) ;
#54663 = DIRECTION ( 'NONE',  ( -0.9576481418713199689, -0.1523715402840224442, 0.2443214073344433801 ) ) ;
#54664 = APPLICATION_PROTOCOL_DEFINITION ( 'draft international standard', 'automotive_design', 1998, #38327 ) ;
#54665 = CARTESIAN_POINT ( 'NONE',  ( -9.624613452210644127, -12.93026283660781317, 16.83029889311164240 ) ) ;
#54666 = EDGE_LOOP ( 'NONE', ( #83967, #68986, #14962, #89143, #29867, #60994 ) ) ;
#54667 = CARTESIAN_POINT ( 'NONE',  ( -2.996823056566161547, -53.47853005769305668, 40.67684663563603209 ) ) ;
#54668 = DIRECTION ( 'NONE',  ( 1.000000000000000000, 0.000000000000000000, -3.673940397442057649E-17 ) ) ;
#54669 = CIRCLE ( 'NONE', #4726, 4.172000000000001485 ) ;
#54670 = CARTESIAN_POINT ( 'NONE',  ( -1.313689454042652249, 14.06550833390138777, -6.880078840050021682 ) ) ;
#54671 = CARTESIAN_POINT ( 'NONE',  ( 27.22613109232188933, -23.01811225391248072, -37.39308776158987513 ) ) ;
#54672 = CARTESIAN_POINT ( 'NONE',  ( -66.94430381114793249, -30.00000000000000000, 85.89596885270491100 ) ) ;
#54673 = CARTESIAN_POINT ( 'NONE',  ( 7.122964895856751077, -30.00000000000000355, -0.9654893961775683486 ) ) ;
#54674 = EDGE_CURVE ( 'NONE', #84521, #5811, #55633, .T. ) ;
#54675 = EDGE_LOOP ( 'NONE', ( #53262, #11387 ) ) ;
#54676 = DIRECTION ( 'NONE',  ( -1.734723475976807094E-16, -0.000000000000000000, -1.000000000000000000 ) ) ;
#54677 = CARTESIAN_POINT ( 'NONE',  ( 87.40653855078360834, -57.59069015034623362, 203.2446439553187076 ) ) ;
#54678 = CARTESIAN_POINT ( 'NONE',  ( 63.67661289323277174, -60.22834765982614869, -28.64704440831590659 ) ) ;
#54679 = EDGE_CURVE ( 'NONE', #337, #104099, #102171, .T. ) ;
#54680 =( GEOMETRIC_REPRESENTATION_CONTEXT ( 3 ) GLOBAL_UNCERTAINTY_ASSIGNED_CONTEXT ( ( #5989 ) ) GLOBAL_UNIT_ASSIGNED_CONTEXT ( ( #90708, #50745, #58329 ) ) REPRESENTATION_CONTEXT ( 'NONE', 'WORKASPACE' ) );
#54681 = ADVANCED_FACE ( 'NONE', ( #12237 ), #43653, .T. ) ;
#54682 = CARTESIAN_POINT ( 'NONE',  ( -0.8808064505793062882, -6.997019658119252306, -5.875704392893994488 ) ) ;
#54683 = PLANE ( 'NONE',  #79384 ) ;
#54684 = LINE ( 'NONE', #78445, #82206 ) ;
#54685 = CARTESIAN_POINT ( 'NONE',  ( -68.90087116575429604, -60.00000000000000711, 135.5803340585387389 ) ) ;
#54686 = FILL_AREA_STYLE_COLOUR ( '', #52017 ) ;
#54687 = CARTESIAN_POINT ( 'NONE',  ( 32.33349330513380693, 1.593028355512270962E-15, 0.000000000000000000 ) ) ;
#54688 = EDGE_CURVE ( 'NONE', #56644, #25211, #28233, .T. ) ;
#54689 = CARTESIAN_POINT ( 'NONE',  ( 62.59524157948160905, 49.99999999997998401, 18.50207713769105311 ) ) ;
#54690 = CARTESIAN_POINT ( 'NONE',  ( -85.61816920359592586, -42.90765739005369994, 187.3767756352330309 ) ) ;
#54691 = VERTEX_POINT ( 'NONE', #10117 ) ;
#54692 = CARTESIAN_POINT ( 'NONE',  ( 35.53798519183398952, 391.1361556355759603, 6.673662436208735116 ) ) ;
#54693 = ADVANCED_FACE ( 'NONE', ( #20403 ), #59986, .T. ) ;
#54694 = ADVANCED_FACE ( 'NONE', ( #21430 ), #30580, .F. ) ;
#54695 = CARTESIAN_POINT ( 'NONE',  ( 12.13202714166731155, -4.667418019610191315, -76.82053255073324749 ) ) ;
#54696 = CARTESIAN_POINT ( 'NONE',  ( -82.96269021345402450, -45.26010578133133322, -14.54628423973963613 ) ) ;
#54697 = DIRECTION ( 'NONE',  ( -1.000000000000000000, -1.224606353822377258E-16, -0.000000000000000000 ) ) ;
#54698 = FACE_OUTER_BOUND ( 'NONE', #7775, .T. ) ;
#54699 = CONICAL_SURFACE ( 'NONE', #23721, 4.000000000000007105, 0.9599310885968835860 ) ;
#54700 = ORIENTED_EDGE ( 'NONE', *, *, #66250, .T. ) ;
#54701 = AXIS2_PLACEMENT_3D ( 'NONE', #90550, #10156, #50596 ) ;
#54702 = CARTESIAN_POINT ( 'NONE',  ( 19.11706402096854873, 50.00000000000000711, 60.42677271361581148 ) ) ;
#54703 = CARTESIAN_POINT ( 'NONE',  ( 13.51444770131055506, 24.63227180702373076, 1.633238822480681751 ) ) ;
#54704 = CARTESIAN_POINT ( 'NONE',  ( -11.19959342721765694, -8.673617379884035472E-16, 19.43146043914803300 ) ) ;
#54705 = CARTESIAN_POINT ( 'NONE',  ( -36.29689614689283417, 464.0084101677746844, 19.58142058293961796 ) ) ;
#54706 = CARTESIAN_POINT ( 'NONE',  ( 73.45964196357411424, -30.00000000000000355, -28.33384050355910588 ) ) ;
#54707 = CARTESIAN_POINT ( 'NONE',  ( -78.24281470800275429, -46.43791216846317127, 142.3052197231980642 ) ) ;
#54708 = ORIENTED_EDGE ( 'NONE', *, *, #12450, .T. ) ;
#54709 = CARTESIAN_POINT ( 'NONE',  ( 42.51305782314333470, 484.3273291304252552, -1.912516135257525063 ) ) ;
#54710 = CARTESIAN_POINT ( 'NONE',  ( 4.472135954999578722, 249.9999999999999432, 4.000000000000002665 ) ) ;
#54711 = CARTESIAN_POINT ( 'NONE',  ( 97.15025092940463480, -57.62288696014798006, 204.4334119669128143 ) ) ;
#54712 = CIRCLE ( 'NONE', #52966, 4.000000000000007105 ) ;
#54713 = CONICAL_SURFACE ( 'NONE', #32431, 4.000000000000001776, 0.9599310885968808105 ) ;
#54714 = CARTESIAN_POINT ( 'NONE',  ( 62.27995339080301562, 50.00000000000000711, 9.818926026722518685 ) ) ;
#54715 = CARTESIAN_POINT ( 'NONE',  ( 37.19218851650311564, 306.1703911487554137, 0.6387774021538068503 ) ) ;
#54716 = CARTESIAN_POINT ( 'NONE',  ( 0.000000000000000000, 0.000000000000000000, -6.499999999999999112 ) ) ;
#54717 = ORIENTED_EDGE ( 'NONE', *, *, #14774, .F. ) ;
#54718 = CARTESIAN_POINT ( 'NONE',  ( 41.85000000000000142, -3.309499999999999886, 4.475777889183790779E-16 ) ) ;
#54719 = CARTESIAN_POINT ( 'NONE',  ( 41.98109406947479272, 462.0607394890938622, 3.143716936936550965 ) ) ;
#54720 = CARTESIAN_POINT ( 'NONE',  ( 15.70480526265250987, 44.04604958794632807, 4.578183157293787886 ) ) ;
#54721 = CARTESIAN_POINT ( 'NONE',  ( -2.977408999572654480, -25.62500000204838813, 7.188101187499999156 ) ) ;
#54722 = EDGE_LOOP ( 'NONE', ( #75198, #4229, #94356, #57367, #83310, #70962, #74639, #39681, #63862 ) ) ;
#54723 = CARTESIAN_POINT ( 'NONE',  ( -33.00000000000000000, 490.5636507776930557, 7.413185101875094496 ) ) ;
#54724 = CIRCLE ( 'NONE', #63397, 2.000000000000001776 ) ;
#54725 = DIRECTION ( 'NONE',  ( -0.5735764363510494901, -0.8191520442889894671, 0.000000000000000000 ) ) ;
#54726 = CARTESIAN_POINT ( 'NONE',  ( 9.349999999999997868, 1.533819458162526451E-15, 0.000000000000000000 ) ) ;
#54727 = CARTESIAN_POINT ( 'NONE',  ( 26.34246982073403487, 37.12886783033192728, 7.802669617497731913 ) ) ;
#54728 = CARTESIAN_POINT ( 'NONE',  ( 4.898587196589412829E-16, -13.81250000409676915, -8.000000000000000000 ) ) ;
#54729 = CIRCLE ( 'NONE', #68543, 13.50000000000000000 ) ;
#54730 = CARTESIAN_POINT ( 'NONE',  ( 17.26604493211178593, 43.28473347087221157, -6.503856858636642535 ) ) ;
#54731 = EDGE_LOOP ( 'NONE', ( #37808, #70137, #103587, #32442, #41688, #55469 ) ) ;
#54732 = DIRECTION ( 'NONE',  ( 1.000000000000000000, 1.224606353822377258E-16, 0.000000000000000000 ) ) ;
#54734 = CARTESIAN_POINT ( 'NONE',  ( 27.64130989961823914, -32.52850770992262852, 31.18481338930833857 ) ) ;
#54733 = CARTESIAN_POINT ( 'NONE',  ( -52.32131825073019371, -14.21045842199420584, 63.24190059944674402 ) ) ;
#54735 = CARTESIAN_POINT ( 'NONE',  ( 24.46939029779937158, 27.46660112286070188, -31.99934855281030721 ) ) ;
#54736 = MANIFOLD_SOLID_BREP ( 'Fillet3', #42920 ) ;
#54737 = ORIENTED_EDGE ( 'NONE', *, *, #60022, .F. ) ;
#54738 = ADVANCED_FACE ( 'NONE', ( #5227 ), #72071, .T. ) ;
#54739 = STYLED_ITEM ( 'NONE', ( #103182 ), #42201 ) ;
#54740 = UNCERTAINTY_MEASURE_WITH_UNIT (LENGTH_MEASURE( 1.000000000000000082E-05 ), #42655, 'distance_accuracy_value', 'NONE');
#54741 = ORIENTED_EDGE ( 'NONE', *, *, #63229, .F. ) ;
#54742 = CARTESIAN_POINT ( 'NONE',  ( -16.66764709352487372, -4.285714285714296246, -19.00223544648545015 ) ) ;
#54743 = CARTESIAN_POINT ( 'NONE',  ( 5.796661515964135868E-15, 60.00000000000000000, -23.66666666666665719 ) ) ;
#54744 = CARTESIAN_POINT ( 'NONE',  ( 7.126148245860624009, 41.12758397993106740, -58.55282951229289523 ) ) ;
#54745 = CARTESIAN_POINT ( 'NONE',  ( 14.54015256618498242, 142.2617268803927288, 0.000000000000000000 ) ) ;
#54746 =( LENGTH_UNIT ( ) NAMED_UNIT ( * ) SI_UNIT ( .MILLI., .METRE. ) );
#54747 = DIRECTION ( 'NONE',  ( 0.000000000000000000, 0.000000000000000000, 1.000000000000000000 ) ) ;
#54749 = ORIENTED_EDGE ( 'NONE', *, *, #44874, .T. ) ;
#54748 = COLOUR_RGB ( '', 0.40784314, 0.44705882, 0.49803922) ;
#54750 = CARTESIAN_POINT ( 'NONE',  ( 17.50000000000002487, 46.94999999999998153, 62.61746187599675295 ) ) ;
#54751 = CARTESIAN_POINT ( 'NONE',  ( 20.19615384615384457, 1.411358822780289120E-15, 0.000000000000000000 ) ) ;
#54752 = CARTESIAN_POINT ( 'NONE',  ( -10.14845555286485634, 12.14994169254081413, -10.55496323469460940 ) ) ;
#54753 = DIRECTION ( 'NONE',  ( -1.224646799147353207E-16, 1.000000000000000000, 0.000000000000000000 ) ) ;
#54754 = CARTESIAN_POINT ( 'NONE',  ( 81.59386212306293373, -29.99999999999999289, -6.572264366181854278 ) ) ;
#54755 = DIRECTION ( 'NONE',  ( -0.5166563581656308246, 0.4014477553983988312, -0.7562446080816809246 ) ) ;
#54756 = ORIENTED_EDGE ( 'NONE', *, *, #18507, .T. ) ;
#54757 = ORIENTED_EDGE ( 'NONE', *, *, #58917, .T. ) ;
#54758 = B_SPLINE_CURVE_WITH_KNOTS ( 'NONE', 3,
 ( #41874, #1938, #59675, #34889, #35421, #842, #103183, #100643, #26802, #92555, #18704, #84474, #27348, #80472, #39517, #21237, #29851, #7118, #22816, #6585, #87012, #54067, #38982, #37952, #97193, #31442, #13615, #88587, #54594, #13082, #72393, #5538, #96153, #70811, #64321, #71856, #104761, #38463, #63261, #103704, #46012, #62728, #78891, #14668, #46530, #5018, #72908, #71330, #22286, #105297, #96678, #23339 ),
 .UNSPECIFIED., .F., .F.,
 ( 4, 2, 2, 2, 2, 2, 2, 2, 2, 2, 2, 2, 2, 2, 2, 2, 2, 2, 2, 2, 2, 2, 2, 2, 2, 4 ),
 ( 0.0004542633818371057141, 0.01826920472356173900, 0.03608414606528637103, 0.05389908740701100653, 0.06280655807787331735, 0.07171402874873562816, 0.08952897009046026366, 0.09843644076132258836, 0.1073439114321848992, 0.1162513821030472100, 0.1207051174384784625, 0.1251588527739097012, 0.1273857204416252442, 0.1296125881093407872, 0.1318394557770563302, 0.1329528896109141711, 0.1340663234447720120, 0.1351797572786298252, 0.1362931911124876661, 0.1385200587802032646, 0.1396334926140610777, 0.1407469264479188908, 0.1418603602817767317, 0.1424170771987056106, 0.1426954356571700777, 0.1429737941156345449 ),
 .UNSPECIFIED. ) ;
#54759 = VERTEX_POINT ( 'NONE', #104981 ) ;
#54760 = CARTESIAN_POINT ( 'NONE',  ( 0.000000000000000000, 0.000000000000000000, -10.42450674750459072 ) ) ;
#54761 = LINE ( 'NONE', #53199, #44921 ) ;
#54762 = CARTESIAN_POINT ( 'NONE',  ( 44.46823338009918558, -5.000000000000000888, 6.123233995736769241E-16 ) ) ;
#54763 = DIRECTION ( 'NONE',  ( -1.000000000000000000, -1.224606353822377258E-16, -0.000000000000000000 ) ) ;
#54764 = CARTESIAN_POINT ( 'NONE',  ( -19.99999999999999289, 4.000000000000000888, -1.500000000000001332 ) ) ;
#54765 = CARTESIAN_POINT ( 'NONE',  ( 6.562934840145646653, -7.579717272840345466, 0.5631738335430743758 ) ) ;
#54766 = AXIS2_PLACEMENT_3D ( 'NONE', #57529, #331, #74255 ) ;
#54767 = ORIENTED_EDGE ( 'NONE', *, *, #50152, .F. ) ;
#54768 = EDGE_CURVE ( 'NONE', #29831, #45028, #51295, .T. ) ;
#54769 = CARTESIAN_POINT ( 'NONE',  ( 7.996668422910687468, 48.00000000000000000, -78.85453279917973646 ) ) ;
#54770 = ORIENTED_EDGE ( 'NONE', *, *, #57320, .F. ) ;
#54771 = CYLINDRICAL_SURFACE ( 'NONE', #63904, 5.000000000000002665 ) ;
#54772 = DIRECTION ( 'NONE',  ( -0.3820442156493231156, 0.000000000000000000, -0.9241440457465999181 ) ) ;
#54773 = DIRECTION ( 'NONE',  ( 0.000000000000000000, 0.000000000000000000, 1.000000000000000000 ) ) ;
#54774 = VECTOR ( 'NONE', #38315, 1000.000000000000000 ) ;
#54776 = EDGE_CURVE ( 'NONE', #36626, #86195, #84745, .T. ) ;
#54775 = B_SPLINE_CURVE_WITH_KNOTS ( 'NONE', 3,
 ( #34744, #76214, #58455, #2321, #92936, #67082, #99965, #25598, #43333, #67616, #68135, #66541, #35809, #84322, #35265, #43856, #101029, #51938 ),
 .UNSPECIFIED., .F., .F.,
 ( 4, 2, 2, 2, 2, 2, 2, 2, 4 ),
 ( 0.007188321694818354014, 0.007693711742174220297, 0.008199101789530087447, 0.008704491836885952863, 0.009209881884241818278, 0.009715271931597681959, 0.01022066197895354737, 0.01072605202630941626, 0.01123144207366528168 ),
 .UNSPECIFIED. ) ;
#54777 = CARTESIAN_POINT ( 'NONE',  ( 3.010530670969122191, 299.5657343207403756, -10.00571837425012056 ) ) ;
#54778 = CARTESIAN_POINT ( 'NONE',  ( 63.15375676826720763, -53.38644956618764326, 87.98034761718228935 ) ) ;
#54779 = AXIS2_PLACEMENT_3D ( 'NONE', #41544, #74957, #100834 ) ;
#54780 = EDGE_LOOP ( 'NONE', ( #85695, #74139, #80881, #68255, #29365, #89290 ) ) ;
#54781 = CARTESIAN_POINT ( 'NONE',  ( 41.30899790313412723, 464.6556986078166460, 16.43539577153557474 ) ) ;
#54782 = DIRECTION ( 'NONE',  ( 0.000000000000000000, -1.000000000000000000, 0.000000000000000000 ) ) ;
#54783 = CARTESIAN_POINT ( 'NONE',  ( -6.984567718307133077, 9.026830075772876327, 0.5333114754527584767 ) ) ;
#54784 = DIRECTION ( 'NONE',  ( -1.000000000000000000, -1.224606353822377258E-16, -0.000000000000000000 ) ) ;
#54785 = ORIENTED_EDGE ( 'NONE', *, *, #56927, .T. ) ;
#54786 = SURFACE_SIDE_STYLE ('',( #21936 ) ) ;
#54787 = CARTESIAN_POINT ( 'NONE',  ( 29.83349330513380337, -4.000000000000000000, 4.898587196589415787E-16 ) ) ;
#54788 = CARTESIAN_POINT ( 'NONE',  ( -13.27149476923476712, -60.00000000000002842, -36.51807098106452543 ) ) ;
#54789 = AXIS2_PLACEMENT_3D ( 'NONE', #67868, #84051, #3675 ) ;
#54790 = VECTOR ( 'NONE', #30729, 1000.000000000000000 ) ;
#54791 = DIRECTION ( 'NONE',  ( 1.000000000000000000, 0.000000000000000000, 0.000000000000000000 ) ) ;
#54792 = CARTESIAN_POINT ( 'NONE',  ( -1.469576158976823947E-15, -29.56250000409677270, 8.000000000000000000 ) ) ;
#54793 = CARTESIAN_POINT ( 'NONE',  ( 8.000000000000000000, -4.999999999999998224, -2.094395098902536834 ) ) ;
#54794 = CIRCLE ( 'NONE', #78980, 5.000000000000002665 ) ;
#54795 = CARTESIAN_POINT ( 'NONE',  ( 86.46880582727897036, -17.03922905361648077, 183.6885730758262412 ) ) ;
#54796 = CARTESIAN_POINT ( 'NONE',  ( 0.000000000000000000, 15.00000000000000000, 0.000000000000000000 ) ) ;
#54797 = CARTESIAN_POINT ( 'NONE',  ( -8.757836645904029993, 19.71581191399078037, -6.344007692567969030E-13 ) ) ;
#54798 = CARTESIAN_POINT ( 'NONE',  ( -18.99999999999999645, 4.000000000000000888, -2.500000000000000000 ) ) ;
#54799 = CARTESIAN_POINT ( 'NONE',  ( 50.48997130883752504, -27.63153651148716250, -27.86727969785274084 ) ) ;
#54800 = CARTESIAN_POINT ( 'NONE',  ( 6.632170054159806760, 303.7449822509489081, 9.914291111224208919 ) ) ;
#54801 = VERTEX_POINT ( 'NONE', #106553 ) ;
#54802 = CARTESIAN_POINT ( 'NONE',  ( 13.66195738444678831, -51.55796608476862986, 23.93843443166228724 ) ) ;
#54803 = CARTESIAN_POINT ( 'NONE',  ( 34.25394585371702050, 436.6001602354167517, 6.438439818649023039 ) ) ;
#54804 = CARTESIAN_POINT ( 'NONE',  ( -99.16400268747783286, -30.00000000000000355, 146.3272739617164859 ) ) ;
#54805 =( GEOMETRIC_REPRESENTATION_CONTEXT ( 3 ) GLOBAL_UNCERTAINTY_ASSIGNED_CONTEXT ( ( #38764 ) ) GLOBAL_UNIT_ASSIGNED_CONTEXT ( ( #93981, #52991, #102603 ) ) REPRESENTATION_CONTEXT ( 'NONE', 'WORKASPACE' ) );
#54806 = EDGE_CURVE ( 'NONE', #38839, #51964, #1018, .T. ) ;
#54807 = CARTESIAN_POINT ( 'NONE',  ( -37.20102314025923107, 438.1443282426989185, 4.012575796191243604 ) ) ;
#54808 = CARTESIAN_POINT ( 'NONE',  ( 45.09708299774578677, -57.68305803399005072, 65.37286121897045632 ) ) ;
#54810 = CARTESIAN_POINT ( 'NONE',  ( 92.53532739719321398, 1.030564683017419500E-14, 0.000000000000000000 ) ) ;
#54809 = CARTESIAN_POINT ( 'NONE',  ( -0.1699383547153779650, 25.17130188398262192, -40.74124215288320272 ) ) ;
#54811 = EDGE_CURVE ( 'NONE', #70572, #45089, #17882, .T. ) ;
#54812 = EDGE_CURVE ( 'NONE', #28267, #41081, #94661, .T. ) ;
#54813 = CIRCLE ( 'NONE', #47954, 2.000000000000000000 ) ;
#54814 = CARTESIAN_POINT ( 'NONE',  ( -40.85671901238235648, 460.0093920008615100, 2.030256043170402869 ) ) ;
#54815 = CARTESIAN_POINT ( 'NONE',  ( -17.75781974272246444, 50.00000000000000000, 62.25693441398608741 ) ) ;
#54816 = SURFACE_STYLE_USAGE ( .BOTH. , #103906 ) ;
#54817 = CARTESIAN_POINT ( 'NONE',  ( -18.99999999999999289, -4.000000000000000000, -1.500000000000001332 ) ) ;
#54818 = FILL_AREA_STYLE_COLOUR ( '', #64732 ) ;
#54819 = APPLICATION_CONTEXT ( 'automotive_design' ) ;
#54820 = DIRECTION ( 'NONE',  ( 1.000000000000000000, 1.224606353822377258E-16, 0.000000000000000000 ) ) ;
#54821 = DIRECTION ( 'NONE',  ( 0.000000000000000000, 1.000000000000000000, 0.000000000000000000 ) ) ;
#54822 = VERTEX_POINT ( 'NONE', #39068 ) ;
#54823 = SURFACE_STYLE_USAGE ( .BOTH. , #95838 ) ;
#54824 = CARTESIAN_POINT ( 'NONE',  ( -1.896692290086544386, -49.86802981722174621, 102.2313487884823076 ) ) ;
#54825 = CARTESIAN_POINT ( 'NONE',  ( -11.32722631842166017, -39.47613668441685064, 30.49643211446674584 ) ) ;
#54826 = ADVANCED_FACE ( 'NONE', ( #20806 ), #85085, .T. ) ;
#54828 = CARTESIAN_POINT ( 'NONE',  ( 4.154708322984369194E-08, -57.67120202538961138, 41.61186700422869933 ) ) ;
#54827 = CARTESIAN_POINT ( 'NONE',  ( -106.0333887696626078, -59.99999999999998579, 181.9111336990339680 ) ) ;
#54829 = VERTEX_POINT ( 'NONE', #103261 ) ;
#54830 = CARTESIAN_POINT ( 'NONE',  ( 98.31310517497099966, 1.030564683017419500E-14, 0.000000000000000000 ) ) ;
#54831 = CONICAL_SURFACE ( 'NONE', #22153, 3.309500000000001663, 0.9599310885968770357 ) ;
#54832 = DIRECTION ( 'NONE',  ( -1.000000000000000000, -1.224606353822377258E-16, -0.000000000000000000 ) ) ;
#54833 = VECTOR ( 'NONE', #55283, 1000.000000000000000 ) ;
#54834 = CARTESIAN_POINT ( 'NONE',  ( 15.05785784214663003, 3.824195276769948748, -4.604276673498405970 ) ) ;
#54835 = CARTESIAN_POINT ( 'NONE',  ( 69.44492854271774718, -60.00000000000000711, 138.4067570271645025 ) ) ;
#54836 = CARTESIAN_POINT ( 'NONE',  ( -39.24156521425334176, 307.7088117867400001, -7.003459073692002157 ) ) ;
#54837 = ORIENTED_EDGE ( 'NONE', *, *, #72954, .F. ) ;
#54838 = CARTESIAN_POINT ( 'NONE',  ( 0.000000000000000000, 0.000000000000000000, 4.000000000000000000 ) ) ;
#54839 = SURFACE_SIDE_STYLE ('',( #39744 ) ) ;
#54840 = AXIS2_PLACEMENT_3D ( 'NONE', #24136, #100106, #41868 ) ;
#54841 = FILL_AREA_STYLE ('',( #93732 ) ) ;
#54842 = DIRECTION ( 'NONE',  ( 0.000000000000000000, 0.000000000000000000, 1.000000000000000000 ) ) ;
#54843 = CARTESIAN_POINT ( 'NONE',  ( -3.857142857142854986, -1.200583151104943846, 103.1763305333244176 ) ) ;
#54844 = VERTEX_POINT ( 'NONE', #103781 ) ;
#54845 = VERTEX_POINT ( 'NONE', #47130 ) ;
#54846 = CARTESIAN_POINT ( 'NONE',  ( -24.03059336844976457, 306.3081475125345605, 9.259463793422938238 ) ) ;
#54847 = VERTEX_POINT ( 'NONE', #63878 ) ;
#54848 = CARTESIAN_POINT ( 'NONE',  ( 19.73463816634111012, 304.7971333121959105, 8.925379062039139555 ) ) ;
#54849 = CARTESIAN_POINT ( 'NONE',  ( -41.50820411079202188, 461.5963371455320612, 2.703439750996428081 ) ) ;
#54850 =( NAMED_UNIT ( * ) SI_UNIT ( $, .STERADIAN. ) SOLID_ANGLE_UNIT ( ) );
#54851 = ORIENTED_EDGE ( 'NONE', *, *, #13664, .T. ) ;
#54852 = CARTESIAN_POINT ( 'NONE',  ( -6.192998293236303908, 41.95244004339406274, -69.88363007943512173 ) ) ;
#54853 = CARTESIAN_POINT ( 'NONE',  ( -110.5746535952040972, -60.00000000005854872, 130.2065959066731011 ) ) ;
#54854 = CARTESIAN_POINT ( 'NONE',  ( 46.00000000000000000, 488.0072389889706983, 1.487873763369907731 ) ) ;
#54855 = CARTESIAN_POINT ( 'NONE',  ( 92.33617079703029162, -59.99999999999995737, 202.4045417339447397 ) ) ;
#54856 = DIRECTION ( 'NONE',  ( 0.5735764363510466035, -0.8191520442889914655, 1.003171929053524500E-16 ) ) ;
#54857 = CARTESIAN_POINT ( 'NONE',  ( 13.69330508143927538, 1.340359594676612611E-15, 0.000000000000000000 ) ) ;
#54858 = AXIS2_PLACEMENT_3D ( 'NONE', #106176, #56027, #98625 ) ;
#54860 = CARTESIAN_POINT ( 'NONE',  ( 11.08465001081330925, -18.58647777032097181, 27.00989251387364476 ) ) ;
#54859 = CARTESIAN_POINT ( 'NONE',  ( -100.4058209406884856, -60.00000000000003553, 69.07134566225379047 ) ) ;
#54861 = AXIS2_PLACEMENT_3D ( 'NONE', #17664, #92600, #85054 ) ;
#54862 = CARTESIAN_POINT ( 'NONE',  ( -7.566827944241370396, 52.14989601952419207, 2.016859383240065196 ) ) ;
#54863 = EDGE_CURVE ( 'NONE', #34686, #87879, #38601, .T. ) ;
#54864 = CARTESIAN_POINT ( 'NONE',  ( -44.62962198081419984, -32.61883708493877521, 41.38836346102954167 ) ) ;
#54865 = CARTESIAN_POINT ( 'NONE',  ( -6.738100187484505454, 41.71798639774085160, -59.05424569925489209 ) ) ;
#54866 = ORIENTED_EDGE ( 'NONE', *, *, #7740, .F. ) ;
#54867 = CARTESIAN_POINT ( 'NONE',  ( 40.85671901238074355, 460.0093920008611121, 2.030256043169934799 ) ) ;
#54868 = CIRCLE ( 'NONE', #27385, 4.000000000000001776 ) ;
#54869 = FACE_OUTER_BOUND ( 'NONE', #74788, .T. ) ;
#54870 = CARTESIAN_POINT ( 'NONE',  ( 42.23079339798727716, 460.7352525929352964, 2.726051457480584972 ) ) ;
#54871 = ORIENTED_EDGE ( 'NONE', *, *, #89579, .F. ) ;
#54872 = CARTESIAN_POINT ( 'NONE',  ( -10.66614630375940109, -11.24660294604464461, 17.92171734272679018 ) ) ;
#54873 = VERTEX_POINT ( 'NONE', #37503 ) ;
#54874 = CARTESIAN_POINT ( 'NONE',  ( 81.20698152405282144, -30.00000000003515055, 192.9746070141664234 ) ) ;
#54875 = DIRECTION ( 'NONE',  ( -1.000000000000000000, -0.000000000000000000, -0.000000000000000000 ) ) ;
#54876 = DIRECTION ( 'NONE',  ( -1.000000000000000000, -1.224606353822377258E-16, -0.000000000000000000 ) ) ;
#54877 =( NAMED_UNIT ( * ) SI_UNIT ( $, .STERADIAN. ) SOLID_ANGLE_UNIT ( ) );
#54878 = CARTESIAN_POINT ( 'NONE',  ( 98.91475564777206841, -30.00000000000000000, 189.0293257016073483 ) ) ;
#54879 = ADVANCED_FACE ( 'NONE', ( #46091 ), #37945, .F. ) ;
#54880 = CARTESIAN_POINT ( 'NONE',  ( -0.3375650005721265723, 36.31234776228274086, 29.71522679684275658 ) ) ;
#54881 = ORIENTED_EDGE ( 'NONE', *, *, #36673, .T. ) ;
#54882 = TOROIDAL_SURFACE ( 'NONE', #106545, 11.00000000000000533, 4.000000000000000000 ) ;
#54883 = ORIENTED_EDGE ( 'NONE', *, *, #28750, .T. ) ;
#54884 = ORIENTED_EDGE ( 'NONE', *, *, #84729, .T. ) ;
#54886 = AXIS2_PLACEMENT_3D ( 'NONE', #40355, #98057, #72198 ) ;
#54885 = CARTESIAN_POINT ( 'NONE',  ( 14.83349330513380337, 1.593028355512270567E-15, 0.000000000000000000 ) ) ;
#54887 = CARTESIAN_POINT ( 'NONE',  ( -7.500000000000000000, 4.330127018922188320, -10.00000000000000000 ) ) ;
#54888 = CARTESIAN_POINT ( 'NONE',  ( 20.17756551592414738, 302.8253764644769035, 1.931382329378719565 ) ) ;
#54889 = ORIENTED_EDGE ( 'NONE', *, *, #88197, .F. ) ;
#54890 = CARTESIAN_POINT ( 'NONE',  ( -16.01731089354314364, 3.899811580358419238, -1.614417983583379623 ) ) ;
#54891 = ORIENTED_EDGE ( 'NONE', *, *, #17907, .T. ) ;
#54892 = CARTESIAN_POINT ( 'NONE',  ( 14.85284876471456350, 1.482358050883964840E-15, 0.000000000000000000 ) ) ;
#54893 = CARTESIAN_POINT ( 'NONE',  ( 95.07921971528816130, -38.48855209000599586, 201.2237972424360635 ) ) ;
#54894 = FACE_OUTER_BOUND ( 'NONE', #69446, .T. ) ;
#54895 = CARTESIAN_POINT ( 'NONE',  ( 83.25488535439697557, -37.82197581851302459, -5.752366542783479808 ) ) ;
#54896 = CARTESIAN_POINT ( 'NONE',  ( 73.65690706782872610, -38.00000000000002842, 114.0709836083384658 ) ) ;
#54897 = CARTESIAN_POINT ( 'NONE',  ( 42.19505042255748606, 346.2110904243742198, 13.96664619797273765 ) ) ;
#54898 = DIRECTION ( 'NONE',  ( -0.2276885448028014569, 0.1882482561681204369, 0.9553640775197926871 ) ) ;
#54899 = EDGE_CURVE ( 'NONE', #97033, #90932, #72970, .T. ) ;
#54900 = CIRCLE ( 'NONE', #46303, 4.000000000000001776 ) ;
#54901 = EDGE_CURVE ( 'NONE', #94858, #71278, #97086, .T. ) ;
#54902 = DIRECTION ( 'NONE',  ( -1.000000000000000000, -1.224606353822377258E-16, -0.000000000000000000 ) ) ;
#54903 = CARTESIAN_POINT ( 'NONE',  ( -39.69724611604759446, 460.7042697230087356, 2.103486822546675405 ) ) ;
#54905 = EDGE_LOOP ( 'NONE', ( #43036, #90735, #21400, #79347, #47271 ) ) ;
#54904 =( BOUNDED_SURFACE ( )  B_SPLINE_SURFACE ( 3, 2, ( 
 ( #78127, #87295, #105070 ),
 ( #37718, #13908, #46302 ),
 ( #71099, #86780, #61977 ),
 ( #102946, #5315, #46822 ) ),
 .UNSPECIFIED., .F., .F., .F. ) 
 B_SPLINE_SURFACE_WITH_KNOTS ( ( 4, 4 ),
 ( 3, 3 ),
 ( -6.748074321549779597E-16, 0.001833990318204585914 ),
 ( 0.000000000000000000, 1.000000000000000000 ),
 .UNSPECIFIED. ) 
 GEOMETRIC_REPRESENTATION_ITEM ( )  RATIONAL_B_SPLINE_SURFACE ( (
 ( 1.000000000000000000, 0.7977970988453257917, 1.000000000000000000),
 ( 1.000000000000000000, 0.7897979397240961763, 1.000000000000000000),
 ( 1.000000000000000000, 0.7817839364700170934, 1.000000000000000000),
 ( 1.000000000000000000, 0.7737149417968423037, 1.000000000000000000) ) ) 
 REPRESENTATION_ITEM ( '' )  SURFACE ( )  );
#54906 = EDGE_CURVE ( 'NONE', #1493, #105760, #29380, .T. ) ;
#54907 = CARTESIAN_POINT ( 'NONE',  ( -43.00000000000000000, 450.0000000000002274, -1.797577426246302013 ) ) ;
#54908 = CARTESIAN_POINT ( 'NONE',  ( -37.24172479535138791, 460.4836853723022614, 2.466600708395719987 ) ) ;
#54909 = CARTESIAN_POINT ( 'NONE',  ( -2.845099737707079246, 79.92971061019304102, 5.000000000000000000 ) ) ;
#54910 = VERTEX_POINT ( 'NONE', #22896 ) ;
#54911 = CARTESIAN_POINT ( 'NONE',  ( 0.000000000000000000, 0.000000000000000000, -6.838999999999999524 ) ) ;
#54912 = CONICAL_SURFACE ( 'NONE', #36034, 4.250000000000000000, 0.9599310885968754814 ) ;
#54913 = CARTESIAN_POINT ( 'NONE',  ( -24.95548294633412922, 304.5552599523065851, 10.31336939286802057 ) ) ;
#54914 = CARTESIAN_POINT ( 'NONE',  ( -3.352941176470589646, -48.79941684889505638, 104.5794940929807524 ) ) ;
#54915 = UNCERTAINTY_MEASURE_WITH_UNIT (LENGTH_MEASURE( 1.000000000000000082E-05 ), #57288, 'distance_accuracy_value', 'NONE');
#54916 = CARTESIAN_POINT ( 'NONE',  ( -8.000000000000000000, -16.34374999999999289, -3.313708498984762496 ) ) ;
#54917 = CARTESIAN_POINT ( 'NONE',  ( -12.85249586701553071, -16.98649936182289721, 34.86928669122507074 ) ) ;
#54918 = B_SPLINE_CURVE_WITH_KNOTS ( 'NONE', 3,
 ( #101800, #70509, #103397, #27966, #62420, #87224, #60831, #21446, #52711, #43568, #85639, #11712, #23033, #38677, #5240, #30065, #48325, #46751 ),
 .UNSPECIFIED., .F., .F.,
 ( 4, 2, 2, 2, 2, 2, 2, 2, 4 ),
 ( 9.813077866773594792E-18, 0.001533449630763184185, 0.003066899261526358830, 0.004600348892289532823, 0.006133798523052707251, 0.007667248153815881678, 0.009200697784579056973, 0.01073414741534223227, 0.01226759704610540583 ),
 .UNSPECIFIED. ) ;
#54920 = VECTOR ( 'NONE', #84356, 999.9999999999998863 ) ;
#54919 = DIRECTION ( 'NONE',  ( 0.000000000000000000, -1.000000000000000000, 0.000000000000000000 ) ) ;
#54921 = ORIENTED_EDGE ( 'NONE', *, *, #66094, .F. ) ;
#54922 = CARTESIAN_POINT ( 'NONE',  ( 85.02428816751515228, -39.35071464379650052, 183.7559687439404854 ) ) ;
#54923 = CARTESIAN_POINT ( 'NONE',  ( -49.27018817646332849, 7.792903869376758053, 15.76322754694117378 ) ) ;
#54924 = AXIS2_PLACEMENT_3D ( 'NONE', #64779, #90646, #73914 ) ;
#54925 = PRESENTATION_STYLE_ASSIGNMENT (( #22613 ) ) ;
#54926 = EDGE_LOOP ( 'NONE', ( #46175, #54770 ) ) ;
#54927 = CARTESIAN_POINT ( 'NONE',  ( 93.86644721295161276, -57.67548266447655436, 8.769766783338946325 ) ) ;
#54928 = CARTESIAN_POINT ( 'NONE',  ( 0.000000000000000000, 0.000000000000000000, -4.289342857142857568 ) ) ;
#54929 = DIRECTION ( 'NONE',  ( -0.5735764363510497121, 0.8191520442889892450, 1.003171929053521665E-16 ) ) ;
#54930 = CARTESIAN_POINT ( 'NONE',  ( -3.503743025706806513, -21.47813235944761345, -38.54973997311672207 ) ) ;
#54931 = CARTESIAN_POINT ( 'NONE',  ( 19.42789538572690233, -25.34295863529625592, 36.70993147433372883 ) ) ;
#54932 = CARTESIAN_POINT ( 'NONE',  ( 10.00000000000000000, -5.000000000000000000, 2.617993873628172263 ) ) ;
#54933 = CARTESIAN_POINT ( 'NONE',  ( 49.52626439931135138, -29.59496896688949619, 45.86522708161003692 ) ) ;
#54934 = CIRCLE ( 'NONE', #84285, 5.000000000000011546 ) ;
#54936 = CARTESIAN_POINT ( 'NONE',  ( -12.81127490048529616, 6.521419762692401534, 7.655175377805322867 ) ) ;
#54935 = CARTESIAN_POINT ( 'NONE',  ( 33.85195725564128821, 465.2464970902066739, 17.18122764674265568 ) ) ;
#54937 = SURFACE_STYLE_FILL_AREA ( #80812 ) ;
#54938 = CARTESIAN_POINT ( 'NONE',  ( 39.13885763974980136, 324.4948203046521371, 17.18769520460729439 ) ) ;
#54939 = CARTESIAN_POINT ( 'NONE',  ( -14.17377942356327125, -24.37016208792438121, -30.50618185950635564 ) ) ;
#54940 = CARTESIAN_POINT ( 'NONE',  ( -3.898086217683917276, 13.33789614101572418, -12.77952306666689886 ) ) ;
#54941 = AXIS2_PLACEMENT_3D ( 'NONE', #77666, #69050, #52847 ) ;
#54942 = CARTESIAN_POINT ( 'NONE',  ( -102.6774475846397650, -37.99999999999999289, 166.4555440054269013 ) ) ;
#54943 = ORIENTED_EDGE ( 'NONE', *, *, #37072, .F. ) ;
#54944 = CARTESIAN_POINT ( 'NONE',  ( -9.474490489458172959, -1.979363373267127857, 15.47598927252669654 ) ) ;
#54945 = DIRECTION ( 'NONE',  ( 0.000000000000000000, -1.000000000000000000, 0.000000000000000000 ) ) ;
#54946 = EDGE_CURVE ( 'NONE', #74465, #87270, #91934, .T. ) ;
#54947 = CARTESIAN_POINT ( 'NONE',  ( 5.728413875956868573, -61.41935773546600785, 1.802282772585246384 ) ) ;
#54948 = EDGE_CURVE ( 'NONE', #93080, #19141, #69537, .T. ) ;
#54949 = CARTESIAN_POINT ( 'NONE',  ( -43.48600344072682589, -21.77010246326202036, -26.80835130359935192 ) ) ;
#54950 = VERTEX_POINT ( 'NONE', #71406 ) ;
#54951 = AXIS2_PLACEMENT_3D ( 'NONE', #17192, #37119, #11721 ) ;
#54952 = DIRECTION ( 'NONE',  ( -0.000000000000000000, -0.000000000000000000, 1.000000000000000000 ) ) ;
#54953 = AXIS2_PLACEMENT_3D ( 'NONE', #51088, #66221, #18784 ) ;
#54954 = VERTEX_POINT ( 'NONE', #104304 ) ;
#54955 = ADVANCED_FACE ( 'NONE', ( #30454 ), #45484, .F. ) ;
#54956 = CARTESIAN_POINT ( 'NONE',  ( 30.04470542674661360, 7.904892719711591020, -42.05337092467530624 ) ) ;
#54957 = CYLINDRICAL_SURFACE ( 'NONE', #63291, 4.000000000000002665 ) ;
#54958 = CARTESIAN_POINT ( 'NONE',  ( -91.91080975627225769, -59.99999999999999289, -14.28697677751371842 ) ) ;
#54959 = VERTEX_POINT ( 'NONE', #64401 ) ;
#54960 = CARTESIAN_POINT ( 'NONE',  ( 8.000000000000000000, -27.68750000409677270, 0.000000000000000000 ) ) ;
#54961 =( NAMED_UNIT ( * ) SI_UNIT ( $, .STERADIAN. ) SOLID_ANGLE_UNIT ( ) );
#54962 = CARTESIAN_POINT ( 'NONE',  ( -4.284822031654945462, -48.90716638558773610, 104.4267991316944943 ) ) ;
#54964 = PLANE ( 'NONE',  #32352 ) ;
#54963 = DIRECTION ( 'NONE',  ( -0.000000000000000000, -1.000000000000000000, -0.000000000000000000 ) ) ;
#54965 = CARTESIAN_POINT ( 'NONE',  ( -79.19495016516171404, -60.32924324703077446, 166.8371806976799974 ) ) ;
#54966 = ORIENTED_EDGE ( 'NONE', *, *, #71544, .F. ) ;
#54967 = CARTESIAN_POINT ( 'NONE',  ( -40.43320803012392162, 490.2964122661026067, 11.44029694117851470 ) ) ;
#54968 = ORIENTED_EDGE ( 'NONE', *, *, #56763, .F. ) ;
#54969 = EDGE_LOOP ( 'NONE', ( #30971, #64466, #5776, #49128 ) ) ;
#54970 = FACE_OUTER_BOUND ( 'NONE', #37398, .T. ) ;
#54971 = FACE_OUTER_BOUND ( 'NONE', #51341, .T. ) ;
#54972 = ORIENTED_EDGE ( 'NONE', *, *, #68350, .T. ) ;
#54973 = CARTESIAN_POINT ( 'NONE',  ( 15.43446081147247106, 46.13172121994917063, -5.765148793919847137 ) ) ;
#54974 = CARTESIAN_POINT ( 'NONE',  ( -9.606080321247050691, 15.83563386295778308, -2.802461721338014300 ) ) ;
#54975 = CARTESIAN_POINT ( 'NONE',  ( -106.5151323516585649, -57.65184864013982491, 200.5412705504392079 ) ) ;
#54976 = CARTESIAN_POINT ( 'NONE',  ( -4.472135954999578722, -65.00000000000000000, 4.000000000000002665 ) ) ;
#54977 = AXIS2_PLACEMENT_3D ( 'NONE', #2117, #26987, #93280 ) ;
#54978 = CARTESIAN_POINT ( 'NONE',  ( 0.000000000000000000, 0.000000000000000000, 0.000000000000000000 ) ) ;
#54979 = CARTESIAN_POINT ( 'NONE',  ( 46.00000000000000000, 488.3725375423206287, 3.127739281036224117 ) ) ;
#54980 = CARTESIAN_POINT ( 'NONE',  ( 91.01458086108723933, -60.00000000000020606, -21.64996939806972520 ) ) ;
#54981 = CARTESIAN_POINT ( 'NONE',  ( -46.52099778141491271, -60.00000000000009948, 69.35786614446448084 ) ) ;
#54982 = EDGE_CURVE ( 'NONE', #59572, #63953, #67833, .T. ) ;
#54983 = CARTESIAN_POINT ( 'NONE',  ( -54.73520214394920202, -60.32528689200320571, 68.31679214792625032 ) ) ;
#54984 = AXIS2_PLACEMENT_3D ( 'NONE', #46523, #63786, #69748 ) ;
#54985 = ORIENTED_EDGE ( 'NONE', *, *, #102067, .F. ) ;
#54986 = SURFACE_SIDE_STYLE ('',( #78735 ) ) ;
#54987 = ORIENTED_EDGE ( 'NONE', *, *, #60017, .F. ) ;
#54988 = CARTESIAN_POINT ( 'NONE',  ( -100.2331735737419507, -45.25801489425005997, 192.3635796437690146 ) ) ;
#54989 = CARTESIAN_POINT ( 'NONE',  ( -30.00306714711500433, 17.76853250946121676, -39.63934773235520481 ) ) ;
#54990 = PRESENTATION_LAYER_ASSIGNMENT (  '', '', ( #18945 ) ) ;
#54991 = VERTEX_POINT ( 'NONE', #49243 ) ;
#54992 = CARTESIAN_POINT ( 'NONE',  ( 18.93607640110042212, 49.18420685015853167, 62.07208393010721892 ) ) ;
#54993 = CARTESIAN_POINT ( 'NONE',  ( 84.77039385422880002, -38.35861834270041015, -23.06278009602441514 ) ) ;
#54994 = FILL_AREA_STYLE_COLOUR ( '', #36444 ) ;
#54995 = CARTESIAN_POINT ( 'NONE',  ( 7.188101187500001821, -10.43750000204838457, -2.977408999572650483 ) ) ;
#54996 = DIRECTION ( 'NONE',  ( 0.000000000000000000, -1.000000000000000000, 0.000000000000000000 ) ) ;
#54997 = CARTESIAN_POINT ( 'NONE',  ( -40.93435977689158989, 414.3154843149413296, 27.72243992809649527 ) ) ;
#54998 = DIRECTION ( 'NONE',  ( 0.000000000000000000, -1.000000000000000000, 0.000000000000000000 ) ) ;
#54999 = ADVANCED_FACE ( 'NONE', ( #99380 ), #97803, .F. ) ;
#55000 = CARTESIAN_POINT ( 'NONE',  ( -0.8400705922950577609, 34.28427440775693924, 29.42928587081339487 ) ) ;
#55001 = ADVANCED_FACE ( 'NONE', ( #35779 ), #70985, .F. ) ;
#55002 = CARTESIAN_POINT ( 'NONE',  ( 82.70911704725124025, 1.016364837396684119E-14, 0.000000000000000000 ) ) ;
#55003 = CARTESIAN_POINT ( 'NONE',  ( -28.09024253349489086, -42.96081926787068994, 33.13080107984512068 ) ) ;
#55004 = EDGE_LOOP ( 'NONE', ( #93244, #27916, #47398, #71225, #103107 ) ) ;
#55005 = EDGE_LOOP ( 'NONE', ( #66777, #14855, #20109, #68964, #85093 ) ) ;
#55006 = CARTESIAN_POINT ( 'NONE',  ( 47.84836796458573360, -60.27567004627039893, 53.82506687556728764 ) ) ;
#55007 = CARTESIAN_POINT ( 'NONE',  ( 8.455951367436818379E-15, 13.70447791526914294, 49.24999999999998579 ) ) ;
#55008 = CIRCLE ( 'NONE', #32662, 4.000000000000000888 ) ;
#55009 = CARTESIAN_POINT ( 'NONE',  ( 15.75384615384615294, 1.411358822780289120E-15, 0.000000000000000000 ) ) ;
#55010 = CARTESIAN_POINT ( 'NONE',  ( -108.8686793369359691, -38.35655312135317985, 190.5485178590994337 ) ) ;
#55011 = ORIENTED_EDGE ( 'NONE', *, *, #66554, .F. ) ;
#55012 = CARTESIAN_POINT ( 'NONE',  ( 89.32126971945325522, -38.38618640067141285, -17.46414196423140908 ) ) ;
#55013 = CARTESIAN_POINT ( 'NONE',  ( 10.02943974854914622, 14.35851092449367528, -10.48560778031837692 ) ) ;
#55014 = CARTESIAN_POINT ( 'NONE',  ( -19.40660811090403826, 49.94503873469690092, 60.93944725389842176 ) ) ;
#55015 = CARTESIAN_POINT ( 'NONE',  ( 13.50000000000000533, -7.794228634059977345, -1.205771365940065953 ) ) ;
#55016 = DIRECTION ( 'NONE',  ( 0.000000000000000000, -0.000000000000000000, 1.000000000000000000 ) ) ;
#55017 = CARTESIAN_POINT ( 'NONE',  ( 0.000000000000000000, 6.123233995736770227E-16, -5.000000000000002665 ) ) ;
#55018 = VECTOR ( 'NONE', #64982, 1000.000000000000000 ) ;
#55019 = CARTESIAN_POINT ( 'NONE',  ( 22.88936581297007677, 28.17682283790767173, 30.74716342950124570 ) ) ;
#55020 = CARTESIAN_POINT ( 'NONE',  ( 33.47662383457161184, 484.3276029205048872, 3.198141044865411509 ) ) ;
#55021 = CARTESIAN_POINT ( 'NONE',  ( 3.313708498984799800, -16.90625000409677270, -7.999999999999961808 ) ) ;
#55022 = CARTESIAN_POINT ( 'NONE',  ( 10.50000000000000000, -5.000000000000000000, -8.595933841506987250 ) ) ;
#55023 = CARTESIAN_POINT ( 'NONE',  ( 94.29025393882723449, -60.00000000000000711, 202.5621357744927025 ) ) ;
#55024 = ADVANCED_FACE ( 'NONE', ( #35231 ), #67052, .T. ) ;
#55025 = CARTESIAN_POINT ( 'NONE',  ( -16.12403420814926491, 34.43109856403526692, 24.14991543090281567 ) ) ;
#55026 = EDGE_LOOP ( 'NONE', ( #62782, #7062 ) ) ;
#55027 = CARTESIAN_POINT ( 'NONE',  ( 58.81832265629508782, -42.96300998799636517, 70.77614602442089620 ) ) ;
#55028 = EDGE_CURVE ( 'NONE', #63428, #105869, #58960, .T. ) ;
#55029 = CARTESIAN_POINT ( 'NONE',  ( -33.01596977466600435, 300.1579362232981225, -0.8105850584072464837 ) ) ;
#55030 = CARTESIAN_POINT ( 'NONE',  ( 3.498313567329702778, -49.14282678961173900, 104.2430177423136826 ) ) ;
#55031 = AXIS2_PLACEMENT_3D ( 'NONE', #42926, #50463, #83373 ) ;
#55032 = CARTESIAN_POINT ( 'NONE',  ( -13.50000000000000000, -7.794228634059985339, -11.79422863405993382 ) ) ;
#55033 = EDGE_LOOP ( 'NONE', ( #69472, #35454, #80145, #60372 ) ) ;
#55035 = CARTESIAN_POINT ( 'NONE',  ( -9.901632022247257581, -50.20920921090512934, 28.42038564161779135 ) ) ;
#55034 = CARTESIAN_POINT ( 'NONE',  ( -110.9034503428022589, -38.35606005712202204, 177.3331091593476287 ) ) ;
#55036 = CARTESIAN_POINT ( 'NONE',  ( -7.500000000000001776, 0.000000000000000000, 5.000000000000000000 ) ) ;
#55037 = CARTESIAN_POINT ( 'NONE',  ( 25.96281893151035547, 308.9845124497657594, 9.902154178306897592 ) ) ;
#55038 = SURFACE_SIDE_STYLE ('',( #35188 ) ) ;
#55039 = CARTESIAN_POINT ( 'NONE',  ( 8.000000000000000000, -30.49999999999999645, 0.000000000000000000 ) ) ;
#55040 = CARTESIAN_POINT ( 'NONE',  ( 6.145467200820246667, -3.000000000000002665, -92.99666842291070168 ) ) ;
#55041 = EDGE_CURVE ( 'NONE', #93551, #29166, #33442, .T. ) ;
#55042 = CIRCLE ( 'NONE', #84399, 3.000000000000025313 ) ;
#55043 = EDGE_CURVE ( 'NONE', #42532, #32237, #9223, .T. ) ;
#55044 = CARTESIAN_POINT ( 'NONE',  ( 30.64177940627106977, 12.99790429510469281, -41.66010176663461095 ) ) ;
#55045 = STYLED_ITEM ( 'NONE', ( #54455 ), #32445 ) ;
#55046 = EDGE_LOOP ( 'NONE', ( #21485, #39123, #94564, #87959 ) ) ;
#55047 = CARTESIAN_POINT ( 'NONE',  ( 82.82797534076844670, -46.49035231702586657, 178.5343783493842693 ) ) ;
#55048 = CARTESIAN_POINT ( 'NONE',  ( 8.350192200756456629, 120.7540425153082424, -0.000000000000000000 ) ) ;
#55049 = CARTESIAN_POINT ( 'NONE',  ( 12.33349330513380693, 1.593028355512270962E-15, 0.000000000000000000 ) ) ;
#55050 = ORIENTED_EDGE ( 'NONE', *, *, #19197, .F. ) ;
#55051 = CARTESIAN_POINT ( 'NONE',  ( -34.73480652773373833, 320.8284291698271318, -5.623717432936989447 ) ) ;
#55052 = CARTESIAN_POINT ( 'NONE',  ( 6.904524730080239259, -5.000000000010798473, -16.27804637754277550 ) ) ;
#55053 = FACE_OUTER_BOUND ( 'NONE', #72983, .T. ) ;
#55054 = SURFACE_SIDE_STYLE ('',( #49083 ) ) ;
#55055 = CARTESIAN_POINT ( 'NONE',  ( -4.472135954999578722, 249.9999999999999432, -4.000000000000002665 ) ) ;
#55056 = CIRCLE ( 'NONE', #68884, 5.000000000000001776 ) ;
#55057 = ORIENTED_EDGE ( 'NONE', *, *, #24679, .T. ) ;
#55058 =( NAMED_UNIT ( * ) PLANE_ANGLE_UNIT ( ) SI_UNIT ( $, .RADIAN. ) );
#55059 = VECTOR ( 'NONE', #49767, 1000.000000000000000 ) ;
#55060 = CARTESIAN_POINT ( 'NONE',  ( -81.59233676157388970, -29.99999999999999289, -7.131517857166998375 ) ) ;
#55061 = CARTESIAN_POINT ( 'NONE',  ( -5.000000000000000000, -25.25113514762997013, -2.443230580349978531 ) ) ;
#55062 = CARTESIAN_POINT ( 'NONE',  ( 14.61381071247569885, 22.25732077882019411, -3.894453577683311352 ) ) ;
#55064 = CARTESIAN_POINT ( 'NONE',  ( -11.40808538165298991, 18.21887386053882452, -8.554671220380841490 ) ) ;
#55063 = CARTESIAN_POINT ( 'NONE',  ( -1.778128680800643568, -18.09823649448113159, 35.01458484713825925 ) ) ;
#55065 = AXIS2_PLACEMENT_3D ( 'NONE', #82751, #73579, #59020 ) ;
#55066 = CARTESIAN_POINT ( 'NONE',  ( -2.977408999572654480, -19.62500000204838457, 7.188101187499999156 ) ) ;
#55067 = FACE_OUTER_BOUND ( 'NONE', #89886, .T. ) ;
#55068 = CARTESIAN_POINT ( 'NONE',  ( 8.572527594031464315E-16, 60.00000000000000000, -6.999999999999992895 ) ) ;
#55069 = CIRCLE ( 'NONE', #67188, 1.000000000000000000 ) ;
#55070 = VERTEX_POINT ( 'NONE', #96099 ) ;
#55071 = DIRECTION ( 'NONE',  ( 0.000000000000000000, -1.000000000000000000, 0.000000000000000000 ) ) ;
#55072 = DIRECTION ( 'NONE',  ( 0.000000000000000000, -1.000000000000000000, 0.000000000000000000 ) ) ;
#55073 = CARTESIAN_POINT ( 'NONE',  ( -3.309912378723064652, 32.69790338586646072, -5.000000000000000000 ) ) ;
#55074 = CARTESIAN_POINT ( 'NONE',  ( -4.250000000000000000, 5.204748896376250699E-16, -10.00000000000000000 ) ) ;
#55075 = EDGE_CURVE ( 'NONE', #30348, #39260, #71284, .T. ) ;
#55076 = CARTESIAN_POINT ( 'NONE',  ( -15.36579003345534034, 3.191525062052813499, 3.226546488166880611 ) ) ;
#55077 = ORIENTED_EDGE ( 'NONE', *, *, #99242, .F. ) ;
#55078 = CARTESIAN_POINT ( 'NONE',  ( 11.46409645960816626, 12.99999999999817923, -10.00000000000000178 ) ) ;
#55079 = LINE ( 'NONE', #64269, #99565 ) ;
#55080 = EDGE_LOOP ( 'NONE', ( #17010, #83818, #87559, #84606, #42621, #31968 ) ) ;
#55081 = CIRCLE ( 'NONE', #105087, 6.499999999999999112 ) ;
#55082 = EDGE_CURVE ( 'NONE', #42431, #64475, #77795, .T. ) ;
#55083 = MANIFOLD_SOLID_BREP ( 'Fillet1', #46316 ) ;
#55084 =( NAMED_UNIT ( * ) PLANE_ANGLE_UNIT ( ) SI_UNIT ( $, .RADIAN. ) );
#55085 = DIRECTION ( 'NONE',  ( 0.000000000000000000, -1.000000000000000000, 0.000000000000000000 ) ) ;
#55086 = CARTESIAN_POINT ( 'NONE',  ( 6.692429545713704186, 4.002214399422197033, -6.852332219948823244 ) ) ;
#55087 = CARTESIAN_POINT ( 'NONE',  ( -111.0802930874671404, -59.99999999999999289, 152.9258238175857514 ) ) ;
#55088 = FACE_OUTER_BOUND ( 'NONE', #33844, .T. ) ;
#55089 = CARTESIAN_POINT ( 'NONE',  ( 6.463178677061750754, 2.643201791673480905, 6.839998497243177766 ) ) ;
#55090 = CARTESIAN_POINT ( 'NONE',  ( 5.290067270632157204, 54.20842449845687838, -6.031152949374584793 ) ) ;
#55091 = CARTESIAN_POINT ( 'NONE',  ( -85.58345756656004255, -25.26006554871649357, 173.5983781047130776 ) ) ;
#55092 = ORIENTED_EDGE ( 'NONE', *, *, #34064, .F. ) ;
#55093 = CARTESIAN_POINT ( 'NONE',  ( 36.39385630396220250, 42.41148509302271208, -60.46671959672418950 ) ) ;
#55094 = VERTEX_POINT ( 'NONE', #70231 ) ;
#55095 = CARTESIAN_POINT ( 'NONE',  ( -19.99999999999999289, 5.000000000000000888, 25.00000000000000000 ) ) ;
#55096 = EDGE_CURVE ( 'NONE', #69241, #46447, #48867, .T. ) ;
#55097 = CARTESIAN_POINT ( 'NONE',  ( 24.83349330513380337, 1.593028355512270567E-15, 0.000000000000000000 ) ) ;
#55098 = B_SPLINE_CURVE_WITH_KNOTS ( 'NONE', 3,
 ( #65998, #105912, #41193, #90815, #74078, #163, #40130, #49808, #73008, #98873 ),
 .UNSPECIFIED., .F., .F.,
 ( 4, 2, 2, 2, 4 ),
 ( 0.000000000000000000, 0.2500000000000000000, 0.5000000000000000000, 0.7500000000000000000, 1.000000000000000000 ),
 .UNSPECIFIED. ) ;
#55099 = CARTESIAN_POINT ( 'NONE',  ( -82.46547003015899691, -37.82730713131258682, 15.76482451545277819 ) ) ;
#55101 = B_SPLINE_CURVE_WITH_KNOTS ( 'NONE', 3,
 ( #23035, #95846, #5759, #87226, #31657, #55356, #88285, #21976, #46753, #71027 ),
 .UNSPECIFIED., .F., .F.,
 ( 4, 2, 2, 2, 4 ),
 ( 9.528354594820111479E-17, 0.002534017993125006665, 0.003167522491406251500, 0.003801026989687495469, 0.005068035986249990778 ),
 .UNSPECIFIED. ) ;
#55100 = CARTESIAN_POINT ( 'NONE',  ( -80.00000000000000000, -52.00000000000000000, -21.09707704303352926 ) ) ;
#55102 = CARTESIAN_POINT ( 'NONE',  ( -7.212994264445060644, -62.98288655659961677, 3.463766307298588920 ) ) ;
#55103 = CARTESIAN_POINT ( 'NONE',  ( 9.075140000865630441, 14.05259049545391115, -5.000000000000000888 ) ) ;
#55104 = SURFACE_STYLE_USAGE ( .BOTH. , #86465 ) ;
#55105 = CARTESIAN_POINT ( 'NONE',  ( 7.754160006507071046, 42.00000000000000711, -59.23741894013591036 ) ) ;
#55106 = CARTESIAN_POINT ( 'NONE',  ( 111.5326445490954228, -59.99999999999995737, 193.8609935400126005 ) ) ;
#55107 = VECTOR ( 'NONE', #80677, 1000.000000000000000 ) ;
#55108 = CARTESIAN_POINT ( 'NONE',  ( -106.4977058212534189, -30.00000000000001776, 137.1023255444873428 ) ) ;
#55109 = EDGE_CURVE ( 'NONE', #80390, #52295, #43477, .T. ) ;
#55110 = CARTESIAN_POINT ( 'NONE',  ( -64.25203903599586397, -36.00863644870968727, 82.20997637332776264 ) ) ;
#55111 = ORIENTED_EDGE ( 'NONE', *, *, #49160, .T. ) ;
#55112 = CARTESIAN_POINT ( 'NONE',  ( 52.56491209535275289, 39.42572890907100458, -38.23519342730396176 ) ) ;
#55113 = CARTESIAN_POINT ( 'NONE',  ( 72.30394896831228380, -59.99999999998524203, 178.8862666714183831 ) ) ;
#55114 = ORIENTED_EDGE ( 'NONE', *, *, #31611, .F. ) ;
#55115 = CARTESIAN_POINT ( 'NONE',  ( 13.45844644947841751, -54.52725136547403650, 23.14343646736056570 ) ) ;
#55116 = CARTESIAN_POINT ( 'NONE',  ( -2.977408999572650039, -22.06250000204838813, -7.188101187500000933 ) ) ;
#55117 = CARTESIAN_POINT ( 'NONE',  ( 32.17606763898039191, 486.0066785907656026, 5.076925403379587642 ) ) ;
#55118 = VERTEX_POINT ( 'NONE', #5494 ) ;
#55119 = CARTESIAN_POINT ( 'NONE',  ( -11.07117956952426319, 45.30041971330288675, 15.14528042430103660 ) ) ;
#55120 = ORIENTED_EDGE ( 'NONE', *, *, #2297, .T. ) ;
#55121 = CARTESIAN_POINT ( 'NONE',  ( 27.33349330513380337, 1.593028355512270567E-15, 0.000000000000000000 ) ) ;
#55122 = SURFACE_SIDE_STYLE ('',( #103694 ) ) ;
#55123 = CARTESIAN_POINT ( 'NONE',  ( -91.48089212003628745, -59.99999999999998579, -15.71179409066253108 ) ) ;
#55124 = CARTESIAN_POINT ( 'NONE',  ( 16.14595037822608603, 7.274337365584589321, 6.616591826375515240 ) ) ;
#55125 = CARTESIAN_POINT ( 'NONE',  ( -5.082755093536326818, -24.59375000204838813, 5.082755093536325042 ) ) ;
#55126 = AXIS2_PLACEMENT_3D ( 'NONE', #11176, #44104, #76995 ) ;
#55127 = CARTESIAN_POINT ( 'NONE',  ( 0.000000000000000000, 0.000000000000000000, -12.27439246179028309 ) ) ;
#55128 = DIRECTION ( 'NONE',  ( 1.000000000000000000, 0.000000000000000000, 0.000000000000000000 ) ) ;
#55129 = VECTOR ( 'NONE', #64464, 1000.000000000000000 ) ;
#55130 = CARTESIAN_POINT ( 'NONE',  ( 1.224646799147352073E-15, 49.99999999999999289, -75.00000000000001421 ) ) ;
#55131 = DIRECTION ( 'NONE',  ( 0.000000000000000000, 0.000000000000000000, -1.000000000000000000 ) ) ;
#55132 = EDGE_CURVE ( 'NONE', #48079, #106696, #4967, .T. ) ;
#55133 = CARTESIAN_POINT ( 'NONE',  ( -36.01341068374667742, 304.0053153259133296, 0.1072131788699336868 ) ) ;
#55134 = CARTESIAN_POINT ( 'NONE',  ( 104.5753504995763166, -60.00000000000000711, 189.2153576413880387 ) ) ;
#55135 = CARTESIAN_POINT ( 'NONE',  ( -37.15836322851141915, -42.97305262937527459, 37.35069024152737427 ) ) ;
#55136 = EDGE_LOOP ( 'NONE', ( #1446, #18069, #11319, #101629 ) ) ;
#55137 = CARTESIAN_POINT ( 'NONE',  ( -34.88193003739208820, 463.4309577930944783, 4.853706708583048979 ) ) ;
#55138 = CARTESIAN_POINT ( 'NONE',  ( 34.47736779890171732, -36.03285718270048932, 34.37443323975536913 ) ) ;
#55139 = CARTESIAN_POINT ( 'NONE',  ( 17.01589776168603407, -1.734723475976807094E-15, 2.227375807149028386 ) ) ;
#55140 = VERTEX_POINT ( 'NONE', #95569 ) ;
#55141 = CARTESIAN_POINT ( 'NONE',  ( 6.333820801329765438, -4.275724398228747170, 5.594228103109105454 ) ) ;
#55142 = AXIS2_PLACEMENT_3D ( 'NONE', #76675, #50274, #9805 ) ;
#55143 = CARTESIAN_POINT ( 'NONE',  ( -67.69295672967986377, -38.33449906752677094, 124.1936149075851006 ) ) ;
#55144 = VERTEX_POINT ( 'NONE', #21706 ) ;
#55146 = CARTESIAN_POINT ( 'NONE',  ( 45.49982102694234953, 388.3127959276886827, 7.886590035822850453 ) ) ;
#55145 = CARTESIAN_POINT ( 'NONE',  ( 6.229963766635606248, -5.000000000000000000, -15.35262140457759727 ) ) ;
#55147 = CARTESIAN_POINT ( 'NONE',  ( 16.42383576958776814, 37.18011179812619105, 21.84794872343109517 ) ) ;
#55148 = CARTESIAN_POINT ( 'NONE',  ( -3.250000000000016431, 5.629165124598842773, 1.734723475976807094E-15 ) ) ;
#55149 = CARTESIAN_POINT ( 'NONE',  ( 0.7775032979944270783, 43.98141867996192644, -16.51775870502402910 ) ) ;
#55150 = FACE_OUTER_BOUND ( 'NONE', #68557, .T. ) ;
#55151 = CARTESIAN_POINT ( 'NONE',  ( 5.092539576892242792, -87.44323467208434408, 3.177249149099057313 ) ) ;
#55152 = CYLINDRICAL_SURFACE ( 'NONE', #2152, 4.000000000000000000 ) ;
#55153 = PRESENTATION_LAYER_ASSIGNMENT (  '', '', ( #41388 ) ) ;
#55154 = CARTESIAN_POINT ( 'NONE',  ( 94.32990217694337787, -60.00000000000000711, 43.96823495280933969 ) ) ;
#55155 = CARTESIAN_POINT ( 'NONE',  ( 64.78349330513380266, 4.898587196589294500E-16, -4.000000000000007105 ) ) ;
#55156 = CARTESIAN_POINT ( 'NONE',  ( 0.000000000000000000, 0.000000000000000000, 5.000000000000000000 ) ) ;
#55157 = CARTESIAN_POINT ( 'NONE',  ( 20.19615384615384457, -4.171999999999999709, 5.616230220889763424E-16 ) ) ;
#55158 = ORIENTED_EDGE ( 'NONE', *, *, #97255, .F. ) ;
#55159 = EDGE_CURVE ( 'NONE', #44939, #98423, #54543, .T. ) ;
#55160 = CARTESIAN_POINT ( 'NONE',  ( -89.26045497392905759, -30.00000000002656364, 8.412000526470205131 ) ) ;
#55161 = VERTEX_POINT ( 'NONE', #46483 ) ;
#55162 = DIRECTION ( 'NONE',  ( 1.224646799147353454E-16, 0.000000000000000000, -1.000000000000000000 ) ) ;
#55163 = CARTESIAN_POINT ( 'NONE',  ( -16.04721880643867493, 4.604982429972173996, -3.436919038178856578 ) ) ;
#55164 = CARTESIAN_POINT ( 'NONE',  ( 8.224453817188688731, 36.45934599358540140, 5.000000000000000888 ) ) ;
#55165 = CARTESIAN_POINT ( 'NONE',  ( 32.14348086320123343, 424.2599792281723126, 25.05014283909958550 ) ) ;
#55166 = FACE_OUTER_BOUND ( 'NONE', #5844, .T. ) ;
#55167 = CARTESIAN_POINT ( 'NONE',  ( 7.188101187499999156, -30.12500000204838813, 2.977408999572654924 ) ) ;
#55168 = VECTOR ( 'NONE', #94510, 1000.000000000000000 ) ;
#55169 = CARTESIAN_POINT ( 'NONE',  ( -18.44955509589851061, 45.00000000000001421, 62.33994477147084723 ) ) ;
#55170 = DIRECTION ( 'NONE',  ( 1.000000000000000000, 0.000000000000000000, 0.000000000000000000 ) ) ;
#55172 = ADVANCED_FACE ( 'NONE', ( #79372 ), #69616, .T. ) ;
#55171 = FILL_AREA_STYLE_COLOUR ( '', #8103 ) ;
#55173 = ORIENTED_EDGE ( 'NONE', *, *, #65392, .F. ) ;
#55174 = AXIS2_PLACEMENT_3D ( 'NONE', #12318, #69514, #71093 ) ;
#55176 = ORIENTED_EDGE ( 'NONE', *, *, #40524, .F. ) ;
#55175 = DIRECTION ( 'NONE',  ( -0.2107607412277919534, 0.000000000000000000, 0.9775376770013071148 ) ) ;
#55177 = CARTESIAN_POINT ( 'NONE',  ( 79.54531020092385063, -46.43426362482939851, 150.5956621145262488 ) ) ;
#55178 = DIRECTION ( 'NONE',  ( 0.5735764363510490460, 0.8191520442889896891, 0.000000000000000000 ) ) ;
#55179 = VERTEX_POINT ( 'NONE', #80422 ) ;
#55180 = EDGE_CURVE ( 'NONE', #15986, #39611, #6532, .T. ) ;
#55181 = CARTESIAN_POINT ( 'NONE',  ( -12.50000000000000355, 41.59226156894883530, -76.70843802411151557 ) ) ;
#55182 = PRESENTATION_STYLE_ASSIGNMENT (( #19835 ) ) ;
#55183 = CARTESIAN_POINT ( 'NONE',  ( -1.320432766682874540E-15, -10.53125000204838457, 7.188101187500000044 ) ) ;
#55184 = CARTESIAN_POINT ( 'NONE',  ( -9.856791769558052252, -57.67120557387264768, 41.61776228975389813 ) ) ;
#55185 = CARTESIAN_POINT ( 'NONE',  ( 9.846493085561697001, 302.6513179331840320, 9.894389155799661495 ) ) ;
#55186 = ORIENTED_EDGE ( 'NONE', *, *, #718, .T. ) ;
#55187 = CIRCLE ( 'NONE', #32821, 8.400000000000000355 ) ;
#55188 =( LENGTH_UNIT ( ) NAMED_UNIT ( * ) SI_UNIT ( .MILLI., .METRE. ) );
#55189 = FILL_AREA_STYLE_COLOUR ( '', #30327 ) ;
#55190 = CARTESIAN_POINT ( 'NONE',  ( -5.728413875956869461, -13.58064226453400281, 1.802282772585246828 ) ) ;
#55191 = CARTESIAN_POINT ( 'NONE',  ( 7.176875381352203931, 41.55694707671359112, -59.30926837872168988 ) ) ;
#55192 = DIRECTION ( 'NONE',  ( 0.000000000000000000, -0.3420201433256725987, -0.9396926207859068736 ) ) ;
#55193 = ORIENTED_EDGE ( 'NONE', *, *, #71799, .F. ) ;
#55194 = CARTESIAN_POINT ( 'NONE',  ( 5.656854249492378806, -11.37500000409677092, 5.656854249492381470 ) ) ;
#55195 = AXIS2_PLACEMENT_3D ( 'NONE', #85220, #59367, #84163 ) ;
#55196 = CARTESIAN_POINT ( 'NONE',  ( 8.099999999999999645, 1.041268927496807532E-15, -8.400000000000000355 ) ) ;
#55197 = CARTESIAN_POINT ( 'NONE',  ( 9.341953373613241851, 15.21714514899092485, 3.572352985695210759 ) ) ;
#55198 = DIRECTION ( 'NONE',  ( -0.000000000000000000, 1.000000000000000000, -0.000000000000000000 ) ) ;
#55199 = DIRECTION ( 'NONE',  ( 0.000000000000000000, -1.000000000000000000, 0.000000000000000000 ) ) ;
#55200 = DIRECTION ( 'NONE',  ( -1.000000000000000000, -1.224606353822377258E-16, -0.000000000000000000 ) ) ;
#55201 = DIRECTION ( 'NONE',  ( 1.000000000000000000, 0.000000000000000000, 0.000000000000000000 ) ) ;
#55202 = FACE_OUTER_BOUND ( 'NONE', #102421, .T. ) ;
#55203 = ORIENTED_EDGE ( 'NONE', *, *, #17173, .T. ) ;
#55204 = CARTESIAN_POINT ( 'NONE',  ( 11.52549757438868028, 43.45827012614538631, 13.79275970915428218 ) ) ;
#55205 = AXIS2_PLACEMENT_3D ( 'NONE', #26704, #34791, #2900 ) ;
#55206 = DIRECTION ( 'NONE',  ( -0.000000000000000000, -0.000000000000000000, 1.000000000000000000 ) ) ;
#55208 = DIRECTION ( 'NONE',  ( -0.5735764363510497121, 0.8191520442889892450, 1.003171929053521665E-16 ) ) ;
#55207 =( BOUNDED_SURFACE ( )  B_SPLINE_SURFACE ( 3, 2, ( 
 ( #299, #106593, #97975 ),
 ( #24126, #56971, #33266 ),
 ( #106048, #42392, #32743 ),
 ( #99018, #66138, #1381 ),
 ( #90422, #57499, #58040 ),
 ( #82319, #15998, #17073 ),
 ( #25182, #90965, #24649 ),
 ( #34349, #17609, #49950 ),
 ( #65077, #8956, #67222 ),
 ( #65613, #32201, #89887 ) ),
 .UNSPECIFIED., .F., .F., .F. ) 
 B_SPLINE_SURFACE_WITH_KNOTS ( ( 4, 2, 2, 2, 4 ),
 ( 3, 3 ),
 ( -1.704365815147212970E-16, 0.002113969294778948911, 0.004227938589558067825, 0.006341907884337186739, 0.008455877179116305653 ),
 ( 0.000000000000000000, 1.000000000000000000 ),
 .UNSPECIFIED. ) 
 GEOMETRIC_REPRESENTATION_ITEM ( )  RATIONAL_B_SPLINE_SURFACE ( (
 ( 1.000000000000000000, 0.8812198548864833558, 1.000000000000000000),
 ( 1.000000000000000000, 0.8727879050781297554, 1.000000000000000000),
 ( 1.000000000000000000, 0.8622329439289413422, 1.000000000000000000),
 ( 1.000000000000000000, 0.8382107008196204578, 1.000000000000000000),
 ( 1.000000000000000000, 0.8245773560043481165, 1.000000000000000000),
 ( 1.000000000000000000, 0.7968578133382318018, 1.000000000000000000),
 ( 1.000000000000000000, 0.7826775888808733539, 1.000000000000000000),
 ( 1.000000000000000000, 0.7555830611713857392, 1.000000000000000000),
 ( 1.000000000000000000, 0.7430233494878055733, 1.000000000000000000),
 ( 1.000000000000000000, 0.7328671738315102324, 1.000000000000000000) ) ) 
 REPRESENTATION_ITEM ( '' )  SURFACE ( )  );
#55209 = AXIS2_PLACEMENT_3D ( 'NONE', #91014, #56068, #31334 ) ;
#55210 = CARTESIAN_POINT ( 'NONE',  ( 5.000000000000000888, 6.123233995736767268E-16, -5.000000000000000000 ) ) ;
#55211 = CARTESIAN_POINT ( 'NONE',  ( -83.66754629239434848, -30.00000000000000000, 158.1039837908334391 ) ) ;
#55212 = CARTESIAN_POINT ( 'NONE',  ( 5.500000000000006217, 42.00000000000000000, -58.69229087761227248 ) ) ;
#55213 = EDGE_CURVE ( 'NONE', #16368, #102350, #91052, .T. ) ;
#55214 = VERTEX_POINT ( 'NONE', #535 ) ;
#55215 = CARTESIAN_POINT ( 'NONE',  ( -25.85826872225150552, 37.16337633890192649, -8.997803431316897971 ) ) ;
#55216 = CARTESIAN_POINT ( 'NONE',  ( 89.63106980978587046, -57.60730104231549831, 203.9042347144641951 ) ) ;
#55217 = CARTESIAN_POINT ( 'NONE',  ( 61.40955143832069751, -47.40894800045192881, -27.09024030718980924 ) ) ;
#55218 = EDGE_CURVE ( 'NONE', #59988, #46183, #28303, .T. ) ;
#55219 = AXIS2_PLACEMENT_3D ( 'NONE', #101368, #91170, #35064 ) ;
#55220 = CARTESIAN_POINT ( 'NONE',  ( -14.89085744133982558, 23.12183015427705612, -0.5456866263935301609 ) ) ;
#55221 = CARTESIAN_POINT ( 'NONE',  ( -6.308454306367740294, 53.41350920378196321, 8.025121516174188230 ) ) ;
#55222 = CARTESIAN_POINT ( 'NONE',  ( -75.24012889104587032, -60.00000000000000000, 182.9205892844746870 ) ) ;
#55223 = DIRECTION ( 'NONE',  ( -1.000000000000000000, -1.224606353822377258E-16, -0.000000000000000000 ) ) ;
#55224 = ADVANCED_FACE ( 'NONE', ( #97664 ), #15165, .T. ) ;
#55225 = CONICAL_SURFACE ( 'NONE', #104980, 5.000000000000001776, 0.9599310885968803664 ) ;
#55226 = CARTESIAN_POINT ( 'NONE',  ( 42.35263604940418958, 50.00000000000000000, 46.99568999590452734 ) ) ;
#55227 = CARTESIAN_POINT ( 'NONE',  ( -84.00149967252067995, -61.04795672767421877, 192.3141443173471998 ) ) ;
#55228 = ORIENTED_EDGE ( 'NONE', *, *, #20423, .T. ) ;
#55229 = CARTESIAN_POINT ( 'NONE',  ( 35.03733779313870400, 344.2465118914557820, -0.5854008046465184467 ) ) ;
#55230 = CARTESIAN_POINT ( 'NONE',  ( 32.28930913498017929, 488.2717154064768579, 9.213726894932253941 ) ) ;
#55231 = EDGE_CURVE ( 'NONE', #70351, #58206, #64785, .T. ) ;
#55232 = DIRECTION ( 'NONE',  ( 1.000000000000000000, 0.000000000000000000, -0.000000000000000000 ) ) ;
#55233 = CARTESIAN_POINT ( 'NONE',  ( -81.92182049364998875, -37.79510036308117549, -13.91368132035993455 ) ) ;
#55234 = DIRECTION ( 'NONE',  ( 0.000000000000000000, -1.000000000000000000, 0.000000000000000000 ) ) ;
#55235 = CARTESIAN_POINT ( 'NONE',  ( -1.469576158976823947E-15, -26.37499999999999645, 8.000000000000000000 ) ) ;
#55236 = ORIENTED_EDGE ( 'NONE', *, *, #11088, .T. ) ;
#55237 = CONICAL_SURFACE ( 'NONE', #8750, 5.000000000000010658, 0.9599310885968697082 ) ;
#55238 = CARTESIAN_POINT ( 'NONE',  ( 18.33022316120833750, 50.00000000000000000, 61.47368443700771934 ) ) ;
#55239 = CARTESIAN_POINT ( 'NONE',  ( 11.43292703283759337, 7.596344060119427866, 9.480118827291864392 ) ) ;
#55240 = CARTESIAN_POINT ( 'NONE',  ( 20.16952962162183738, -4.285714285713005722, -15.50035291838722884 ) ) ;
#55241 = CARTESIAN_POINT ( 'NONE',  ( -37.31252934617396022, 464.0480400141152018, 19.52723141531950191 ) ) ;
#55242 = CARTESIAN_POINT ( 'NONE',  ( 89.66268371970539874, -30.00000000000002487, 1.291492552605954858 ) ) ;
#55243 = AXIS2_PLACEMENT_3D ( 'NONE', #41383, #49464, #100677 ) ;
#55244 = CARTESIAN_POINT ( 'NONE',  ( -79.28778576954361768, -42.96893229327703523, 145.0288265907346386 ) ) ;
#55245 = ORIENTED_EDGE ( 'NONE', *, *, #76092, .F. ) ;
#55246 = CARTESIAN_POINT ( 'NONE',  ( 12.46466094585187889, -29.99999999999991118, 37.03825901911487506 ) ) ;
#55247 = DIRECTION ( 'NONE',  ( 0.000000000000000000, 0.000000000000000000, -1.000000000000000000 ) ) ;
#55248 = CARTESIAN_POINT ( 'NONE',  ( 74.06814223428997934, -57.60986418767995332, 187.4363434323835804 ) ) ;
#55249 = CARTESIAN_POINT ( 'NONE',  ( 62.90157831112001929, 50.00000000000000000, -3.733503276916400715 ) ) ;
#55250 = CARTESIAN_POINT ( 'NONE',  ( 37.74156130160795897, 305.1789513982170092, -7.619069046267780365 ) ) ;
#55251 = DIRECTION ( 'NONE',  ( 0.9576481418713256311, -0.1523715402840490341, 0.2443214073344040227 ) ) ;
#55252 = EDGE_LOOP ( 'NONE', ( #74599, #77551 ) ) ;
#55253 = DIRECTION ( 'NONE',  ( 0.000000000000000000, -0.000000000000000000, 1.000000000000000000 ) ) ;
#55254 = CARTESIAN_POINT ( 'NONE',  ( 42.19180677453719142, 462.2931784592651638, 3.389262873192005809 ) ) ;
#55256 = CARTESIAN_POINT ( 'NONE',  ( -100.0016765554683928, -37.82064696691352879, 139.8630582154185049 ) ) ;
#55255 = CARTESIAN_POINT ( 'NONE',  ( 35.59999999999999432, 1.533819458162526451E-15, 0.000000000000000000 ) ) ;
#55257 = CARTESIAN_POINT ( 'NONE',  ( 5.082755093536325930, -18.96875000204838457, -5.082755093536325042 ) ) ;
#55258 = DIRECTION ( 'NONE',  ( 0.000000000000000000, 1.000000000000000000, -2.311253228826401127E-16 ) ) ;
#55259 = CARTESIAN_POINT ( 'NONE',  ( -3.313708498984798467, -24.03124999999998934, -7.999999999999961808 ) ) ;
#55260 = DIRECTION ( 'NONE',  ( 0.000000000000000000, -1.000000000000000000, 0.000000000000000000 ) ) ;
#55261 = LINE ( 'NONE', #38584, #99598 ) ;
#55262 = CYLINDRICAL_SURFACE ( 'NONE', #11699, 1.250000000000001110 ) ;
#55263 = MECHANICAL_DESIGN_GEOMETRIC_PRESENTATION_REPRESENTATION (  '', ( #48327 ), #10457 ) ;
#55264 = CARTESIAN_POINT ( 'NONE',  ( -24.29659155877464372, 27.70505434333144379, -31.30545107321098541 ) ) ;
#55265 = VERTEX_POINT ( 'NONE', #49652 ) ;
#55266 = TOROIDAL_SURFACE ( 'NONE', #29462, 10.00000000000000000, 4.000000000000000000 ) ;
#55268 = CARTESIAN_POINT ( 'NONE',  ( 27.32589341038793052, -39.47960534280331046, 32.30614241192893132 ) ) ;
#55267 = CARTESIAN_POINT ( 'NONE',  ( 0.7145311798163270778, 9.237604307034018802, 2.885982852862873934E-16 ) ) ;
#55269 = CARTESIAN_POINT ( 'NONE',  ( 0.000000000000000000, 44.00000000000000711, 61.00000000000000000 ) ) ;
#55270 = MANIFOLD_SOLID_BREP ( 'ThdSchPat', #75632 ) ;
#55271 = VERTEX_POINT ( 'NONE', #90655 ) ;
#55272 = EDGE_LOOP ( 'NONE', ( #105284, #34883, #83490, #99529 ) ) ;
#55273 = CARTESIAN_POINT ( 'NONE',  ( 1.013458338643688394, 51.43252368279713238, 9.749812615651872960 ) ) ;
#55274 = DIRECTION ( 'NONE',  ( 0.000000000000000000, 0.000000000000000000, -1.000000000000000000 ) ) ;
#55275 = DIRECTION ( 'NONE',  ( -1.000000000000000000, -1.224606353822377258E-16, -0.000000000000000000 ) ) ;
#55276 = CARTESIAN_POINT ( 'NONE',  ( -0.4154390169121289778, 51.29111456655304124, -10.18190877321939958 ) ) ;
#55277 = EDGE_LOOP ( 'NONE', ( #22426, #56607, #8984, #18402 ) ) ;
#55278 = CARTESIAN_POINT ( 'NONE',  ( 1.405425595346621037E-06, -60.00000000000000000, -42.63907915653317104 ) ) ;
#55279 = B_SPLINE_CURVE_WITH_KNOTS ( 'NONE', 3,
 ( #97765, #89697, #82112, #47619, #55699, #7164, #8232, #65417, #81562, #32005, #104812, #7691, #48678, #65943, #40602, #31489 ),
 .UNSPECIFIED., .F., .F.,
 ( 4, 2, 2, 2, 2, 2, 2, 4 ),
 ( 9.697399036122160616E-19, 0.001337001954499136835, 0.002674003908998272803, 0.005348007817996543872, 0.006685009772495679840, 0.008022011726994815808, 0.009359013681493952644, 0.01069601563599308948 ),
 .UNSPECIFIED. ) ;
#55280 = CARTESIAN_POINT ( 'NONE',  ( 88.15283761886021807, -30.00000000000000000, 187.1385865483707960 ) ) ;
#55281 = CARTESIAN_POINT ( 'NONE',  ( -10.07715742286756821, 12.79177078999071604, -10.57225269177452631 ) ) ;
#55283 = DIRECTION ( 'NONE',  ( -1.000000000000000000, -0.000000000000000000, -0.000000000000000000 ) ) ;
#55282 = CIRCLE ( 'NONE', #105260, 4.000000000000000888 ) ;
#55284 = CARTESIAN_POINT ( 'NONE',  ( -9.609938133626268808, -5.000000000000000000, -77.63956163934031451 ) ) ;
#55285 = CIRCLE ( 'NONE', #57051, 5.000000000000001776 ) ;
#55286 = CARTESIAN_POINT ( 'NONE',  ( 6.500000000000007105, -3.752776749732581685, -0.7999999999999977129 ) ) ;
#55287 = ORIENTED_EDGE ( 'NONE', *, *, #90040, .T. ) ;
#55288 = EDGE_CURVE ( 'NONE', #40289, #22931, #24884, .T. ) ;
#55289 = B_SPLINE_CURVE_WITH_KNOTS ( 'NONE', 3,
 ( #87754, #21443, #88279, #14892 ),
 .UNSPECIFIED., .F., .F.,
 ( 4, 4 ),
 ( 0.000000000000000000, 0.002232172794141575132 ),
 .UNSPECIFIED. ) ;
#55290 = EDGE_CURVE ( 'NONE', #12734, #12822, #727, .T. ) ;
#55291 = ORIENTED_EDGE ( 'NONE', *, *, #52062, .F. ) ;
#55292 = ORIENTED_EDGE ( 'NONE', *, *, #30086, .T. ) ;
#55293 = CARTESIAN_POINT ( 'NONE',  ( 5.290067270632161645, -1.200000000000000030E-05, -6.031152949374595451 ) ) ;
#55294 = CARTESIAN_POINT ( 'NONE',  ( 52.56483885390522914, 40.83906611471594061, -38.23529411764711483 ) ) ;
#55295 = CARTESIAN_POINT ( 'NONE',  ( -42.10086803841218739, 435.6552064019005002, 19.95582312411058368 ) ) ;
#55296 = DIRECTION ( 'NONE',  ( 0.000000000000000000, 1.000000000000000000, 0.000000000000000000 ) ) ;
#55298 = MECHANICAL_DESIGN_GEOMETRIC_PRESENTATION_REPRESENTATION (  '', ( #24320 ), #17444 ) ;
#55297 = DIRECTION ( 'NONE',  ( 0.000000000000000000, -1.000000000000000000, 0.000000000000000000 ) ) ;
#55299 = DIRECTION ( 'NONE',  ( -1.000000000000000000, -0.000000000000000000, -0.000000000000000000 ) ) ;
#55300 = VERTEX_POINT ( 'NONE', #43172 ) ;
#55302 = ADVANCED_FACE ( 'NONE', ( #66920 ), #60443, .F. ) ;
#55301 = CARTESIAN_POINT ( 'NONE',  ( -8.737863884121431113, 48.00000000000000000, -79.96381019768850251 ) ) ;
#55303 = ORIENTED_EDGE ( 'NONE', *, *, #7586, .T. ) ;
#55304 = DIRECTION ( 'NONE',  ( 0.000000000000000000, 0.000000000000000000, 1.000000000000000000 ) ) ;
#55305 = CARTESIAN_POINT ( 'NONE',  ( 4.898587196589412829E-16, -12.12499999999999289, -8.000000000000000000 ) ) ;
#55306 = CARTESIAN_POINT ( 'NONE',  ( -41.50869271558325124, 485.4378639541363896, -3.633045570221354659 ) ) ;
#55307 = CARTESIAN_POINT ( 'NONE',  ( -79.71008617727251533, -60.00000000000007816, 171.5468452086663262 ) ) ;
#55308 = CARTESIAN_POINT ( 'NONE',  ( 63.37350735021203718, -49.91027513827258133, 86.82604463955132701 ) ) ;
#55309 = VERTEX_POINT ( 'NONE', #67454 ) ;
#55310 = EDGE_CURVE ( 'NONE', #3257, #54238, #95470, .T. ) ;
#55311 = CARTESIAN_POINT ( 'NONE',  ( -34.88900972249400212, 464.6206820655984870, 18.69027339340994232 ) ) ;
#55312 = CARTESIAN_POINT ( 'NONE',  ( -33.00000000000000000, 500.0000000000002274, 0.000000000000000000 ) ) ;
#55313 = DIRECTION ( 'NONE',  ( -2.312964634635742898E-14, 0.9952410070626638294, -0.09744402424415100905 ) ) ;
#55314 = CARTESIAN_POINT ( 'NONE',  ( -0.01431428620034891179, -57.67120202577072519, -44.61186648040676772 ) ) ;
#55315 = VERTEX_POINT ( 'NONE', #83610 ) ;
#55316 = AXIS2_PLACEMENT_3D ( 'NONE', #49394, #17594, #23571 ) ;
#55317 =( NAMED_UNIT ( * ) SI_UNIT ( $, .STERADIAN. ) SOLID_ANGLE_UNIT ( ) );
#55318 = CARTESIAN_POINT ( 'NONE',  ( 0.000000000000000000, 0.000000000000000000, -3.024963890361733743 ) ) ;
#55319 = CARTESIAN_POINT ( 'NONE',  ( 24.34055539606506002, -60.00000000000002842, -35.71097672886680385 ) ) ;
#55320 = PRESENTATION_LAYER_ASSIGNMENT (  '', '', ( #72574 ) ) ;
#55321 = DIRECTION ( 'NONE',  ( 0.000000000000000000, -1.000000000000000000, 0.000000000000000000 ) ) ;
#55322 = CARTESIAN_POINT ( 'NONE',  ( -3.313708498984760720, -28.71875000409677625, -8.000000000000000000 ) ) ;
#55323 = CARTESIAN_POINT ( 'NONE',  ( -8.000000000000000000, -4.999999999999998224, 2.094395098902548824 ) ) ;
#55324 = CARTESIAN_POINT ( 'NONE',  ( 86.11264096538754131, -53.80573175718830470, 192.0612798401426176 ) ) ;
#55325 = FILL_AREA_STYLE ('',( #24069 ) ) ;
#55326 = UNCERTAINTY_MEASURE_WITH_UNIT (LENGTH_MEASURE( 1.000000000000000082E-05 ), #12742, 'distance_accuracy_value', 'NONE');
#55327 = CARTESIAN_POINT ( 'NONE',  ( -4.091067340831425092, 13.63436032547001631, 4.999999999999999112 ) ) ;
#55328 = CARTESIAN_POINT ( 'NONE',  ( 7.212408192734264034, -7.984829106796318854, -3.465038817813885341 ) ) ;
#55329 = VERTEX_POINT ( 'NONE', #76581 ) ;
#55330 = SURFACE_SIDE_STYLE ('',( #31112 ) ) ;
#55331 = DIRECTION ( 'NONE',  ( -1.000000000000000000, -1.224606353822377258E-16, -0.000000000000000000 ) ) ;
#55332 = CARTESIAN_POINT ( 'NONE',  ( 25.60766401561201278, -60.00000000000000000, 41.33855483581840673 ) ) ;
#55333 = CARTESIAN_POINT ( 'NONE',  ( -99.97669482139977504, -30.00000000000000000, 185.6954798495859222 ) ) ;
#55334 = EDGE_CURVE ( 'NONE', #65995, #93762, #31744, .T. ) ;
#55335 = AXIS2_PLACEMENT_3D ( 'NONE', #5172, #103850, #29998 ) ;
#55336 = CARTESIAN_POINT ( 'NONE',  ( -41.14976906663522271, 484.9007963630877498, -3.779285786479841480 ) ) ;
#55337 = CARTESIAN_POINT ( 'NONE',  ( 45.24179637743248605, -57.68290370260588418, 65.68885952698795450 ) ) ;
#55339 = CARTESIAN_POINT ( 'NONE',  ( 43.02661387979662067, 465.7449615347606482, 11.43319743843943392 ) ) ;
#55338 = CARTESIAN_POINT ( 'NONE',  ( 9.502264916438665665, 44.08945810161099388, 13.16974031357852226 ) ) ;
#55340 = EDGE_CURVE ( 'NONE', #55094, #72439, #18383, .T. ) ;
#55341 = EDGE_CURVE ( 'NONE', #29736, #63378, #92003, .T. ) ;
#55342 = CARTESIAN_POINT ( 'NONE',  ( -27.00467402917412585, 41.40534817802205936, -70.25900587838104627 ) ) ;
#55343 = CARTESIAN_POINT ( 'NONE',  ( -18.15598277398370541, 50.00000000000001421, 61.69040288260701033 ) ) ;
#55344 = PRESENTATION_STYLE_ASSIGNMENT (( #54816 ) ) ;
#55345 = CARTESIAN_POINT ( 'NONE',  ( -16.35932222714940920, -60.00000000000000000, 39.87631610020545736 ) ) ;
#55346 = CARTESIAN_POINT ( 'NONE',  ( -87.47245207465813621, -39.05729538259036104, 189.8431066894454773 ) ) ;
#55347 = CIRCLE ( 'NONE', #64016, 6.500000000000000888 ) ;
#55348 = AXIS2_PLACEMENT_3D ( 'NONE', #47880, #46833, #96467 ) ;
#55349 = VERTEX_POINT ( 'NONE', #2154 ) ;
#55350 = CARTESIAN_POINT ( 'NONE',  ( 17.50000000000004974, 49.99999999999836575, 59.91915230424464767 ) ) ;
#55351 = CARTESIAN_POINT ( 'NONE',  ( -15.30569569889779302, -18.58753576952222630, 27.14328885328878016 ) ) ;
#55352 = COLOUR_RGB ( '', 0.09019608, 0.27058824, 0.51372549) ;
#55354 = DIRECTION ( 'NONE',  ( -1.000000000000000000, -1.224606353822377258E-16, -0.000000000000000000 ) ) ;
#55353 = CARTESIAN_POINT ( 'NONE',  ( -104.7817843546067564, -60.00000000000002842, 188.6132346340173740 ) ) ;
#55355 = ORIENTED_EDGE ( 'NONE', *, *, #90372, .T. ) ;
#55356 = CARTESIAN_POINT ( 'NONE',  ( -43.72576364275317218, 464.6794755336276808, 7.643080537327061386 ) ) ;
#55357 = CARTESIAN_POINT ( 'NONE',  ( -7.499994653025497726, -2.925861026131086007, -20.99866594782981011 ) ) ;
#55358 = CARTESIAN_POINT ( 'NONE',  ( 0.2565376335216150161, -2.516992571280034952, -6.500000000000001776 ) ) ;
#55359 = AXIS2_PLACEMENT_3D ( 'NONE', #60333, #88827, #89370 ) ;
#55360 = DIRECTION ( 'NONE',  ( 0.000000000000000000, 0.000000000000000000, -1.000000000000000000 ) ) ;
#55361 = ADVANCED_FACE ( 'NONE', ( #67973, #10774 ), #100862, .F. ) ;
#55362 = CIRCLE ( 'NONE', #22698, 5.000000000000001776 ) ;
#55363 = CARTESIAN_POINT ( 'NONE',  ( 15.93923796801722581, 3.103382665672758112, -0.7338764874896186452 ) ) ;
#55364 = CARTESIAN_POINT ( 'NONE',  ( 73.43745472883394143, -60.00000000000001421, 166.5727501461540214 ) ) ;
#55365 = CARTESIAN_POINT ( 'NONE',  ( -1.251035332617614015, 53.76709749943464089, -9.149874701752242601 ) ) ;
#55366 = EDGE_LOOP ( 'NONE', ( #439, #13625, #70865, #10148 ) ) ;
#55367 = DIRECTION ( 'NONE',  ( -1.000000000000000000, -0.000000000000000000, -0.000000000000000000 ) ) ;
#55368 = FILL_AREA_STYLE_COLOUR ( '', #9229 ) ;
#55370 = CARTESIAN_POINT ( 'NONE',  ( 1.544427540536530710E-15, -4.285714285714290916, -25.22241582816893057 ) ) ;
#55369 = CARTESIAN_POINT ( 'NONE',  ( 4.154910845142357978, -29.99999999999994316, 36.99135396797706932 ) ) ;
#55371 = ADVANCED_FACE ( 'NONE', ( #91725, #92774 ), #2697, .T. ) ;
#55372 = CARTESIAN_POINT ( 'NONE',  ( 30.11650669486618881, -3.999999999999998224, 0.000000000000000000 ) ) ;
#55373 =( LENGTH_UNIT ( ) NAMED_UNIT ( * ) SI_UNIT ( .MILLI., .METRE. ) );
#55374 = EDGE_LOOP ( 'NONE', ( #61908, #3284, #13174, #103102, #49463, #101876 ) ) ;
#55375 = EDGE_LOOP ( 'NONE', ( #56989, #101305, #86519, #1855 ) ) ;
#55376 = CARTESIAN_POINT ( 'NONE',  ( -27.18509476864008079, 312.1746170569358583, 10.69926602037820196 ) ) ;
#55377 = ORIENTED_EDGE ( 'NONE', *, *, #55109, .T. ) ;
#55378 = DIRECTION ( 'NONE',  ( 0.000000000000000000, 0.000000000000000000, -1.000000000000000000 ) ) ;
#55379 = CARTESIAN_POINT ( 'NONE',  ( 6.936184427528457874, 0.000000000000000000, 0.000000000000000000 ) ) ;
#55380 = ORIENTED_EDGE ( 'NONE', *, *, #103836, .T. ) ;
#55381 = PRESENTATION_STYLE_ASSIGNMENT (( #22539 ) ) ;
#55382 = PRESENTATION_STYLE_ASSIGNMENT (( #104477 ) ) ;
#55384 = CARTESIAN_POINT ( 'NONE',  ( -107.3965502307806901, -59.99999999998781419, 200.2794665723340586 ) ) ;
#55383 = AXIS2_PLACEMENT_3D ( 'NONE', #59936, #101437, #85250 ) ;
#55385 = CARTESIAN_POINT ( 'NONE',  ( 75.69572031415813740, -60.00000000000000000, 185.6113820405912236 ) ) ;
#55386 = FACE_OUTER_BOUND ( 'NONE', #69732, .T. ) ;
#55387 = FILL_AREA_STYLE ('',( #63516 ) ) ;
#55388 = AXIS2_PLACEMENT_3D ( 'NONE', #75443, #59279, #92154 ) ;
#55390 = CARTESIAN_POINT ( 'NONE',  ( 9.087783854787057081, -25.54846076700239976, 28.14888778420710835 ) ) ;
#55389 = CARTESIAN_POINT ( 'NONE',  ( -105.3891558216856339, -14.21045842199431064, 188.2119682431835486 ) ) ;
#55391 = CARTESIAN_POINT ( 'NONE',  ( 102.8126250176293013, -38.00000000000001421, 170.8513491865694505 ) ) ;
#55392 = CARTESIAN_POINT ( 'NONE',  ( -7.306464488495704401, 52.17307787027569788, 2.638989770206940477 ) ) ;
#55393 = CARTESIAN_POINT ( 'NONE',  ( -47.00499629171626026, -22.23575002398623113, 41.16886872908139594 ) ) ;
#55394 = CARTESIAN_POINT ( 'NONE',  ( -21.23076943214345391, 18.64284798593011061, 32.03398753740776783 ) ) ;
#55395 = VERTEX_POINT ( 'NONE', #26495 ) ;
#55396 = CARTESIAN_POINT ( 'NONE',  ( 1.167761364413894221, 9.591040725253717980, -50.96251430281557049 ) ) ;
#55397 = CARTESIAN_POINT ( 'NONE',  ( -18.99999999999999289, 4.000000000000000888, 25.00000000000000000 ) ) ;
#55398 = FACE_OUTER_BOUND ( 'NONE', #21896, .T. ) ;
#55399 = CARTESIAN_POINT ( 'NONE',  ( 3.416848052085409204, 304.8518027757643267, -9.000000000397495370 ) ) ;
#55400 = CARTESIAN_POINT ( 'NONE',  ( 34.94338628507543376, 342.5355909536760350, -0.9693026116843473927 ) ) ;
#55401 = EDGE_LOOP ( 'NONE', ( #71751, #97256, #11063, #94922 ) ) ;
#55402 = CARTESIAN_POINT ( 'NONE',  ( -11.87184877076866485, -7.546347915368680326, 19.57404110235124151 ) ) ;
#55403 = ORIENTED_EDGE ( 'NONE', *, *, #96884, .T. ) ;
#55404 = CARTESIAN_POINT ( 'NONE',  ( 89.85535138209283446, -29.99999999996537525, 199.2189362433487076 ) ) ;
#55405 = CARTESIAN_POINT ( 'NONE',  ( 4.802676810931882923E-16, -0.7818963811860507596, -8.000000000000000000 ) ) ;
#55406 = CARTESIAN_POINT ( 'NONE',  ( 1.836601268058451273E-15, 1.005902684993158047, 14.99698745252234566 ) ) ;
#55407 = CARTESIAN_POINT ( 'NONE',  ( 90.45918241757048861, -30.00000000000000000, 91.17802396393395270 ) ) ;
#55408 = DIRECTION ( 'NONE',  ( 0.000000000000000000, 0.000000000000000000, 1.000000000000000000 ) ) ;
#55409 = ORIENTED_EDGE ( 'NONE', *, *, #39965, .T. ) ;
#55410 = EDGE_CURVE ( 'NONE', #22594, #88800, #105772, .T. ) ;
#55411 = ORIENTED_EDGE ( 'NONE', *, *, #90889, .F. ) ;
#55412 = ORIENTED_EDGE ( 'NONE', *, *, #68196, .T. ) ;
#55413 = CARTESIAN_POINT ( 'NONE',  ( -10.00000000000000355, 85.00000000000000000, 0.000000000000000000 ) ) ;
#55414 = CARTESIAN_POINT ( 'NONE',  ( -44.20877944490916178, 435.3144825228398531, 11.13781432399559890 ) ) ;
#55415 = DIRECTION ( 'NONE',  ( 0.000000000000000000, -1.000000000000000000, 0.000000000000000000 ) ) ;
#55416 = EDGE_CURVE ( 'NONE', #102006, #82194, #11067, .T. ) ;
#55417 = ORIENTED_EDGE ( 'NONE', *, *, #23345, .T. ) ;
#55419 = EDGE_CURVE ( 'NONE', #47033, #45637, #59366, .T. ) ;
#55418 = CARTESIAN_POINT ( 'NONE',  ( 25.21823338009918203, 1.482358050883964840E-15, 0.000000000000000000 ) ) ;
#55420 = ORIENTED_EDGE ( 'NONE', *, *, #23480, .F. ) ;
#55421 = CARTESIAN_POINT ( 'NONE',  ( 31.14131030317610538, 1.482358050883964840E-15, 0.000000000000000000 ) ) ;
#55422 = CARTESIAN_POINT ( 'NONE',  ( 104.1038336098137478, -38.40903114083004510, 198.3374114307139280 ) ) ;
#55423 = CARTESIAN_POINT ( 'NONE',  ( 29.98176661990081371, 1.340359594676612611E-15, 0.000000000000000000 ) ) ;
#55424 = CARTESIAN_POINT ( 'NONE',  ( 84.05541200475410335, -45.28723854143181882, 1.855072029239146936 ) ) ;
#55425 = CARTESIAN_POINT ( 'NONE',  ( 68.83552688692435595, -38.00000000000000000, 97.13860410137628776 ) ) ;
#55426 = CARTESIAN_POINT ( 'NONE',  ( 39.22194103031748824, 325.7770611439928530, 17.47603589310227434 ) ) ;
#55427 = CARTESIAN_POINT ( 'NONE',  ( 5.656854249492378806, -24.87500000409677270, 5.656854249492381470 ) ) ;
#55428 = CARTESIAN_POINT ( 'NONE',  ( -15.00099999999999767, 12.99999999999999289, 0.000000000000000000 ) ) ;
#55429 = AXIS2_PLACEMENT_3D ( 'NONE', #21680, #45407, #46455 ) ;
#55430 = ADVANCED_FACE ( 'NONE', ( #92229 ), #88544, .T. ) ;
#55431 = PRESENTATION_STYLE_ASSIGNMENT (( #80778 ) ) ;
#55432 = AXIS2_PLACEMENT_3D ( 'NONE', #74291, #99089, #97493 ) ;
#55433 = CARTESIAN_POINT ( 'NONE',  ( 1.112351485006119578, -1.486542822431297095E-16, 101.1532825174488579 ) ) ;
#55434 = VERTEX_POINT ( 'NONE', #101411 ) ;
#55435 = CARTESIAN_POINT ( 'NONE',  ( -26.12491014859622851, 36.99816777972599624, 9.598909272560698369 ) ) ;
#55436 = VERTEX_POINT ( 'NONE', #77128 ) ;
#55437 = CARTESIAN_POINT ( 'NONE',  ( -35.42017376419228469, 370.0793824939161141, 4.722754217616025763 ) ) ;
#55438 = CARTESIAN_POINT ( 'NONE',  ( -26.18007569671338786, 305.7834980030482370, 10.60090293758347535 ) ) ;
#55439 = CARTESIAN_POINT ( 'NONE',  ( 8.559508646656350805, 53.68473964988125857, -4.031152949374623873 ) ) ;
#55440 = DIRECTION ( 'NONE',  ( -0.000000000000000000, -1.000000000000000000, -0.000000000000000000 ) ) ;
#55441 = CARTESIAN_POINT ( 'NONE',  ( -5.656854249492381470, -13.06249999999999467, 5.656854249492379694 ) ) ;
#55442 = CARTESIAN_POINT ( 'NONE',  ( 35.86766554461611634, -26.86117697613646627, 42.80318219311200068 ) ) ;
#55443 = AXIS2_PLACEMENT_3D ( 'NONE', #97851, #41742, #67093 ) ;
#55444 = MANIFOLD_SOLID_BREP ( 'Cut-Extrude1', #56674 ) ;
#55445 = AXIS2_PLACEMENT_3D ( 'NONE', #78043, #69956, #29531 ) ;
#55446 = SURFACE_STYLE_USAGE ( .BOTH. , #31743 ) ;
#55447 = ORIENTED_EDGE ( 'NONE', *, *, #83337, .F. ) ;
#55448 = CARTESIAN_POINT ( 'NONE',  ( 83.48300417591265443, -57.35605306953866744, 189.6652105889277777 ) ) ;
#55449 = DIRECTION ( 'NONE',  ( 0.000000000000000000, 0.000000000000000000, 1.000000000000000000 ) ) ;
#55450 = ORIENTED_EDGE ( 'NONE', *, *, #65172, .F. ) ;
#55451 = CARTESIAN_POINT ( 'NONE',  ( 95.57936171141837178, -57.67169793798020550, 37.86718902071597626 ) ) ;
#55452 = CARTESIAN_POINT ( 'NONE',  ( 35.65219468668975367, 436.9652430364860720, 4.678245027581728444 ) ) ;
#55453 = CARTESIAN_POINT ( 'NONE',  ( 17.11334244676965000, -4.333298119783723479, -5.314533759803898860 ) ) ;
#55454 = SURFACE_SIDE_STYLE ('',( #48954 ) ) ;
#55455 = CONICAL_SURFACE ( 'NONE', #5589, 4.000000000000001776, 0.9599310885968808105 ) ;
#55456 = VECTOR ( 'NONE', #18447, 1000.000000000000000 ) ;
#55457 = CARTESIAN_POINT ( 'NONE',  ( -85.96552653199317717, -37.99999999999979394, 186.3819002138399412 ) ) ;
#55458 = CARTESIAN_POINT ( 'NONE',  ( 8.000000000000000000, -4.999999999999998224, -2.094395098902536834 ) ) ;
#55459 = CARTESIAN_POINT ( 'NONE',  ( 31.36650669486618881, 1.474610560812782335E-15, 0.000000000000000000 ) ) ;
#55461 = CARTESIAN_POINT ( 'NONE',  ( -15.79117028497290676, 4.455738443839065255, 5.224106130487632171 ) ) ;
#55460 = CARTESIAN_POINT ( 'NONE',  ( 5.000000000000000000, 0.000000000000000000, 0.000000000000000000 ) ) ;
#55462 = EDGE_CURVE ( 'NONE', #7306, #91765, #19475, .T. ) ;
#55463 = AXIS2_PLACEMENT_3D ( 'NONE', #91462, #101136, #35918 ) ;
#55464 = CARTESIAN_POINT ( 'NONE',  ( 4.472135954999579610, -85.00000000000000000, -4.000000000000001776 ) ) ;
#55465 = DIRECTION ( 'NONE',  ( 0.000000000000000000, 0.000000000000000000, -1.000000000000000000 ) ) ;
#55466 = CARTESIAN_POINT ( 'NONE',  ( -34.12349128637492157, 490.1895789250393705, 12.63944770676173057 ) ) ;
#55467 = STYLED_ITEM ( 'NONE', ( #79453 ), #10508 ) ;
#55468 = CARTESIAN_POINT ( 'NONE',  ( -82.11800378195846406, -37.99999999999997868, -13.62076433111584883 ) ) ;
#55469 = ORIENTED_EDGE ( 'NONE', *, *, #17952, .F. ) ;
#55470 = DIRECTION ( 'NONE',  ( -1.000000000000000000, -0.000000000000000000, -0.000000000000000000 ) ) ;
#55471 = CARTESIAN_POINT ( 'NONE',  ( -21.03575760287767693, -18.85229723311598349, -33.58254685689154684 ) ) ;
#55473 = CARTESIAN_POINT ( 'NONE',  ( -60.63884085839525540, -34.58948043286759599, -25.08978428314187781 ) ) ;
#55472 = CARTESIAN_POINT ( 'NONE',  ( 2.422472278927138205E-15, -0.1944580884125578779, 19.78098730681987405 ) ) ;
#55474 = ORIENTED_EDGE ( 'NONE', *, *, #2655, .T. ) ;
#55475 = B_SPLINE_CURVE_WITH_KNOTS ( 'NONE', 3,
 ( #47913, #5364, #6933, #62538, #39856, #89466, #4826, #13424 ),
 .UNSPECIFIED., .F., .F.,
 ( 4, 2, 2, 4 ),
 ( 0.004673709593152168724, 0.005837709341827655544, 0.007001709090503143232, 0.009329708587854116872 ),
 .UNSPECIFIED. ) ;
#55476 = FACE_OUTER_BOUND ( 'NONE', #28000, .T. ) ;
#55477 = EDGE_LOOP ( 'NONE', ( #73694, #66604, #47477, #76132, #70510 ) ) ;
#55478 = CARTESIAN_POINT ( 'NONE',  ( 6.445370176741849200, 7.262437273738760801, 1.101027156348632685 ) ) ;
#55479 = CARTESIAN_POINT ( 'NONE',  ( 0.5805565836007582359, 3.752776749732553263, -6.499999999999999112 ) ) ;
#55480 = CARTESIAN_POINT ( 'NONE',  ( -92.53051596449445526, -59.99999999999998579, -1.702129118078903547 ) ) ;
#55481 = ORIENTED_EDGE ( 'NONE', *, *, #63842, .F. ) ;
#55482 = CARTESIAN_POINT ( 'NONE',  ( 3.313708498984742512, -27.40625000409677270, -8.000000000000019540 ) ) ;
#55483 = CARTESIAN_POINT ( 'NONE',  ( 96.70244981892803082, -60.35942960495466991, 196.8117809302864316 ) ) ;
#55484 = B_SPLINE_CURVE_WITH_KNOTS ( 'NONE', 3,
 ( #62989, #37147, #102911, #20982, #45222, #22556, #21487, #5282, #54867, #12293, #87795, #29077, #38717, #45735 ),
 .UNSPECIFIED., .F., .F.,
 ( 4, 2, 2, 2, 2, 2, 4 ),
 ( 1.710314408003578897E-16, 0.001025149392783061874, 0.001537724089174507267, 0.002050298785565952443, 0.002562873481957398270, 0.003075448178348843230, 0.004100597571131750496 ),
 .UNSPECIFIED. ) ;
#55485 = CARTESIAN_POINT ( 'NONE',  ( 0.000000000000000000, 55.00000000000000000, 0.000000000000000000 ) ) ;
#55486 = EDGE_CURVE ( 'NONE', #79845, #49899, #105515, .T. ) ;
#55487 = CARTESIAN_POINT ( 'NONE',  ( -81.09797583371168628, -46.44412491365037710, 163.0375973178554432 ) ) ;
#55488 = EDGE_LOOP ( 'NONE', ( #72276, #25108, #86388, #88433, #3278, #79849 ) ) ;
#55489 = CIRCLE ( 'NONE', #53823, 11.00000000000000000 ) ;
#55490 = ORIENTED_EDGE ( 'NONE', *, *, #58352, .F. ) ;
#55491 = ORIENTED_EDGE ( 'NONE', *, *, #22347, .T. ) ;
#55492 = CARTESIAN_POINT ( 'NONE',  ( -2.352990130084491319E-16, 7.505553499465148271, -6.064240316920404439 ) ) ;
#55493 = CARTESIAN_POINT ( 'NONE',  ( -5.000000000000000000, -14.13517361223578916, 11.83579766571232206 ) ) ;
#55494 = LINE ( 'NONE', #14506, #100034 ) ;
#55495 = ORIENTED_EDGE ( 'NONE', *, *, #1342, .T. ) ;
#55496 = DIRECTION ( 'NONE',  ( 0.000000000000000000, 0.000000000000000000, 1.000000000000000000 ) ) ;
#55497 = CARTESIAN_POINT ( 'NONE',  ( -9.435590127033085750, 15.92795519102023860, -3.316968746323878836 ) ) ;
#55498 = CARTESIAN_POINT ( 'NONE',  ( -113.5594301016874539, -57.67117831481159840, 184.0234983118591856 ) ) ;
#55499 = CARTESIAN_POINT ( 'NONE',  ( -9.819056950928635175, 294.6481068335448299, 1.893705519456528652 ) ) ;
#55500 = CARTESIAN_POINT ( 'NONE',  ( 30.00000000000000000, 1.347111479062088405E-15, 11.00000000000000000 ) ) ;
#55501 = CARTESIAN_POINT ( 'NONE',  ( 27.99999999999999645, 0.000000000000000000, -13.00000000000000000 ) ) ;
#55502 = CARTESIAN_POINT ( 'NONE',  ( 0.000000000000000000, 15.00000000000000000, -9.999999999999998224 ) ) ;
#55503 = AXIS2_PLACEMENT_3D ( 'NONE', #18981, #60493, #61013 ) ;
#55504 = CARTESIAN_POINT ( 'NONE',  ( 89.66801957890137942, -59.99999999999992895, -23.31517609469964469 ) ) ;
#55505 = CARTESIAN_POINT ( 'NONE',  ( -69.35428882245668092, -14.21045842199431064, 113.5922931172439263 ) ) ;
#55506 = B_SPLINE_CURVE_WITH_KNOTS ( 'NONE', 3,
 ( #11931, #3860, #85303, #4920, #28699, #20630 ),
 .UNSPECIFIED., .F., .F.,
 ( 4, 2, 4 ),
 ( 2.255140518769848915E-17, 0.002095085863784774613, 0.004190171727569526675 ),
 .UNSPECIFIED. ) ;
#55507 = CARTESIAN_POINT ( 'NONE',  ( -52.65234607686913648, -46.44195135248897799, 58.10028993942689368 ) ) ;
#55508 = ORIENTED_EDGE ( 'NONE', *, *, #70117, .T. ) ;
#55509 = CARTESIAN_POINT ( 'NONE',  ( -5.290067270632269114, -1.200000000000000030E-05, -8.531152949374520844 ) ) ;
#55510 = ORIENTED_EDGE ( 'NONE', *, *, #85792, .F. ) ;
#55511 = CARTESIAN_POINT ( 'NONE',  ( -101.8606233574472526, -52.71812712487817976, 192.2808579428766507 ) ) ;
#55512 = CARTESIAN_POINT ( 'NONE',  ( -30.93371285580958130, 14.00361151752278666, -40.91601221254722276 ) ) ;
#55513 = ORIENTED_EDGE ( 'NONE', *, *, #63940, .F. ) ;
#55514 = CARTESIAN_POINT ( 'NONE',  ( 19.09871521262170546, 49.67080660516045043, 61.74181558515030588 ) ) ;
#55515 = CARTESIAN_POINT ( 'NONE',  ( 107.9104760785782560, -38.35877191852540591, 193.0889224582925294 ) ) ;
#55516 = FILL_AREA_STYLE ('',( #54994 ) ) ;
#55517 = DIRECTION ( 'NONE',  ( 1.000000000000000000, -0.000000000000000000, -0.000000000000000000 ) ) ;
#55518 = FILL_AREA_STYLE_COLOUR ( '', #44474 ) ;
#55519 = CARTESIAN_POINT ( 'NONE',  ( -42.36162206505707672, 485.1874691988857649, -2.398526663485948340 ) ) ;
#55520 = CARTESIAN_POINT ( 'NONE',  ( -37.51854390953261742, 313.5286481325095451, 14.45587837336505999 ) ) ;
#55521 =( BOUNDED_SURFACE ( )  B_SPLINE_SURFACE ( 3, 2, ( 
 ( #39228, #71559, #54843 ),
 ( #87772, #65073, #48343 ),
 ( #89363, #81238, #97422 ),
 ( #30612, #104466, #79131 ),
 ( #88302, #79662, #14376 ),
 ( #72102, #64038, #24122 ),
 ( #7355, #96916, #105009 ),
 ( #105530, #55885, #88820 ),
 ( #71042, #73140, #47285 ),
 ( #62961, #14915, #40265 ),
 ( #95861, #106043, #80713 ),
 ( #64554, #46766, #6829 ) ),
 .UNSPECIFIED., .F., .F., .F. ) 
 B_SPLINE_SURFACE_WITH_KNOTS ( ( 4, 2, 2, 2, 2, 4 ),
 ( 3, 3 ),
 ( -3.903127820947815962E-18, 0.001187588843296127862, 0.001781383264944193853, 0.002375177686592259627, 0.003562766529888391608, 0.004750355373184523590 ),
 ( 0.000000000000000000, 1.000000000000000000 ),
 .UNSPECIFIED. ) 
 GEOMETRIC_REPRESENTATION_ITEM ( )  RATIONAL_B_SPLINE_SURFACE ( (
 ( 1.000000000000000000, 0.9359444767143314525, 1.000000000000000000),
 ( 1.000000000000000000, 0.9295581727144297535, 1.000000000000000000),
 ( 1.000000000000000000, 0.9234593375675015370, 1.000000000000000000),
 ( 1.000000000000000000, 0.9150808072273350913, 1.000000000000000000),
 ( 1.000000000000000000, 0.9124161408737702095, 1.000000000000000000),
 ( 1.000000000000000000, 0.9074047588826502642, 1.000000000000000000),
 ( 1.000000000000000000, 0.9050663310860240784, 1.000000000000000000),
 ( 1.000000000000000000, 0.8987692007139229666, 1.000000000000000000),
 ( 1.000000000000000000, 0.8954627112850603865, 1.000000000000000000),
 ( 1.000000000000000000, 0.8909338199771259514, 1.000000000000000000),
 ( 1.000000000000000000, 0.8897377579433781714, 1.000000000000000000),
 ( 1.000000000000000000, 0.8897565210026093796, 1.000000000000000000) ) ) 
 REPRESENTATION_ITEM ( '' )  SURFACE ( )  );
#55522 = AXIS2_PLACEMENT_3D ( 'NONE', #85474, #84407, #34287 ) ;
#55523 = DIRECTION ( 'NONE',  ( -1.000000000000000000, -1.224606353822377258E-16, -0.000000000000000000 ) ) ;
#55524 = CARTESIAN_POINT ( 'NONE',  ( -3.352941176470582985, -48.79941684889506348, 104.5794940929807382 ) ) ;
#55525 = FACE_OUTER_BOUND ( 'NONE', #4499, .T. ) ;
#55526 = CARTESIAN_POINT ( 'NONE',  ( -36.69878522477553418, 484.6513904560026162, -2.872853880317824071 ) ) ;
#55527 = UNCERTAINTY_MEASURE_WITH_UNIT (LENGTH_MEASURE( 1.000000000000000082E-05 ), #17837, 'distance_accuracy_value', 'NONE');
#55528 =( GEOMETRIC_REPRESENTATION_CONTEXT ( 3 ) GLOBAL_UNCERTAINTY_ASSIGNED_CONTEXT ( ( #91714 ) ) GLOBAL_UNIT_ASSIGNED_CONTEXT ( ( #85601, #26331, #2523 ) ) REPRESENTATION_CONTEXT ( 'NONE', 'WORKASPACE' ) );
#55529 = ORIENTED_EDGE ( 'NONE', *, *, #38045, .T. ) ;
#55530 = ORIENTED_EDGE ( 'NONE', *, *, #34724, .F. ) ;
#55531 = CARTESIAN_POINT ( 'NONE',  ( 49.37742207085376123, -36.05361790536632327, 48.61349652102713748 ) ) ;
#55532 = AXIS2_PLACEMENT_3D ( 'NONE', #105827, #101990, #35709 ) ;
#55533 = DIRECTION ( 'NONE',  ( 0.000000000000000000, 1.000000000000000000, 0.000000000000000000 ) ) ;
#55534 = CARTESIAN_POINT ( 'NONE',  ( -5.817469134863317848, 13.92717135920117499, -3.893337541178055972 ) ) ;
#55535 = EDGE_CURVE ( 'NONE', #87544, #73615, #73041, .T. ) ;
#55536 = CARTESIAN_POINT ( 'NONE',  ( -104.5277147594802756, -38.40261826923566701, 197.9417711179345645 ) ) ;
#55537 = ORIENTED_EDGE ( 'NONE', *, *, #84423, .T. ) ;
#55538 = CARTESIAN_POINT ( 'NONE',  ( 91.07270688230414635, -38.34878623222908089, 1.164067527244401656 ) ) ;
#55539 = CARTESIAN_POINT ( 'NONE',  ( 10.70645837388809696, 12.39743528853116850, -10.00073793910723730 ) ) ;
#55540 = CARTESIAN_POINT ( 'NONE',  ( -19.48790983171578617, 49.99824972418149116, 60.16135127412848504 ) ) ;
#55541 = CARTESIAN_POINT ( 'NONE',  ( 29.99999999999919709, 464.1079104336375849, 10.87617013709114744 ) ) ;
#55542 = CARTESIAN_POINT ( 'NONE',  ( 93.17606065420541483, -37.84849057407753037, 97.15365511994282599 ) ) ;
#55543 = CARTESIAN_POINT ( 'NONE',  ( -31.45742208051316169, 439.3234620524921752, 23.14668034959422727 ) ) ;
#55544 = DIRECTION ( 'NONE',  ( 0.000000000000000000, 0.000000000000000000, 1.000000000000000000 ) ) ;
#55545 = CARTESIAN_POINT ( 'NONE',  ( -35.72342988946527242, 379.5409829981540497, 4.793340659205911791 ) ) ;
#55546 = FILL_AREA_STYLE ('',( #80362 ) ) ;
#55547 = AXIS2_PLACEMENT_3D ( 'NONE', #11516, #13112, #63287 ) ;
#55548 = CARTESIAN_POINT ( 'NONE',  ( 80.84005111079980566, -60.00000000000000000, 196.9542464304632290 ) ) ;
#55549 = ADVANCED_FACE ( 'NONE', ( #6816 ), #30054, .T. ) ;
#55550 =( NAMED_UNIT ( * ) PLANE_ANGLE_UNIT ( ) SI_UNIT ( $, .RADIAN. ) );
#55551 = ORIENTED_EDGE ( 'NONE', *, *, #60950, .T. ) ;
#55552 = CARTESIAN_POINT ( 'NONE',  ( 58.77133666112784027, -29.07347965779057120, 64.41413915537998491 ) ) ;
#55553 = EDGE_CURVE ( 'NONE', #37125, #19635, #35882, .T. ) ;
#55554 = CARTESIAN_POINT ( 'NONE',  ( -29.42522989588877635, 307.1650680246546017, -9.025740850171580121 ) ) ;
#55555 = DIRECTION ( 'NONE',  ( 1.000000000000000000, 0.000000000000000000, 0.000000000000000000 ) ) ;
#55556 = CARTESIAN_POINT ( 'NONE',  ( -7.801777176595948049, 26.41172014187366202, -1.786991866639918491 ) ) ;
#55557 = EDGE_LOOP ( 'NONE', ( #52799, #80345, #101816, #4313, #39656, #29148 ) ) ;
#55559 = CARTESIAN_POINT ( 'NONE',  ( -14.88762942959811575, 23.11179094003107792, 0.4991395141700474825 ) ) ;
#55558 = CARTESIAN_POINT ( 'NONE',  ( -98.14959585606926851, -38.47957152706085537, 200.9671316718450385 ) ) ;
#55560 = DIRECTION ( 'NONE',  ( -1.000000000000000000, 0.000000000000000000, 0.000000000000000000 ) ) ;
#55561 = CARTESIAN_POINT ( 'NONE',  ( 21.16904338951196962, 305.0382894998002143, 8.976822404920172360 ) ) ;
#55562 = CARTESIAN_POINT ( 'NONE',  ( -27.10511071441192144, 36.60571256639527604, -10.05698433968589178 ) ) ;
#55563 = CARTESIAN_POINT ( 'NONE',  ( 4.898587196589412829E-16, -31.62499999999999289, -8.000000000000000000 ) ) ;
#55564 = CARTESIAN_POINT ( 'NONE',  ( -2.617478844992338516, -5.000000000000015099, -94.73972676610841859 ) ) ;
#55565 = LINE ( 'NONE', #16186, #68 ) ;
#55566 = AXIS2_PLACEMENT_3D ( 'NONE', #40944, #88970, #57636 ) ;
#55567 = EDGE_LOOP ( 'NONE', ( #1791, #53813 ) ) ;
#55568 = CARTESIAN_POINT ( 'NONE',  ( 85.62085174182965375, -21.92232634333130292, 167.5821520937073785 ) ) ;
#55569 = CARTESIAN_POINT ( 'NONE',  ( 37.61650669486618881, 4.898587196589411843E-16, -4.000000000000000888 ) ) ;
#55570 = CARTESIAN_POINT ( 'NONE',  ( 36.32012801257089052, 28.16013746738074630, 12.39738870050804209 ) ) ;
#55571 = ORIENTED_EDGE ( 'NONE', *, *, #54518, .F. ) ;
#55572 = AXIS2_PLACEMENT_3D ( 'NONE', #25819, #26871, #41409 ) ;
#55573 = CARTESIAN_POINT ( 'NONE',  ( -27.45361451126541752, 305.3287645444004852, -9.452926980072254182 ) ) ;
#55574 = CARTESIAN_POINT ( 'NONE',  ( 7.500141383065412448, -5.000000000000024869, -20.99866593659988823 ) ) ;
#55575 = CYLINDRICAL_SURFACE ( 'NONE', #45560, 60.00000000000000000 ) ;
#55576 = CARTESIAN_POINT ( 'NONE',  ( -7.360624614890398654, 50.00000000000001421, -94.61012438779899014 ) ) ;
#55577 = DIRECTION ( 'NONE',  ( 0.000000000000000000, 0.000000000000000000, 1.000000000000000000 ) ) ;
#55578 = PRESENTATION_LAYER_ASSIGNMENT (  '', '', ( #76228 ) ) ;
#55579 = CARTESIAN_POINT ( 'NONE',  ( -28.49094055106828449, 13.12977990610419532, -40.46781900651360075 ) ) ;
#55580 = EDGE_LOOP ( 'NONE', ( #5717, #25522, #23498, #28405 ) ) ;
#55581 =( LENGTH_UNIT ( ) NAMED_UNIT ( * ) SI_UNIT ( .MILLI., .METRE. ) );
#55582 = CARTESIAN_POINT ( 'NONE',  ( 38.38780340174425731, 25.23068935580986150, 13.15235269662653828 ) ) ;
#55583 = CARTESIAN_POINT ( 'NONE',  ( 0.7775251346576579348, 25.97784539287345851, 38.51776489545537885 ) ) ;
#55585 = CARTESIAN_POINT ( 'NONE',  ( -10.23665139305246008, 16.32373278757852120, -10.09226983855738347 ) ) ;
#55584 = CARTESIAN_POINT ( 'NONE',  ( 0.000000000000000000, 0.000000000000000000, -5.710657142857142432 ) ) ;
#55586 = EDGE_CURVE ( 'NONE', #44580, #37591, #55101, .T. ) ;
#55587 = CARTESIAN_POINT ( 'NONE',  ( 5.082755093536325930, -20.46875000204838813, -5.082755093536325042 ) ) ;
#55588 = CARTESIAN_POINT ( 'NONE',  ( -28.88579667808738805, 18.87341229088492511, -39.88979553324844574 ) ) ;
#55589 = CARTESIAN_POINT ( 'NONE',  ( -6.828042834505471781, 41.63841151066672808, -58.95291702778770571 ) ) ;
#55590 = ORIENTED_EDGE ( 'NONE', *, *, #71793, .T. ) ;
#55591 = LINE ( 'NONE', #39973, #104288 ) ;
#55592 = DIRECTION ( 'NONE',  ( 0.000000000000000000, 0.000000000000000000, 1.000000000000000000 ) ) ;
#55593 = CARTESIAN_POINT ( 'NONE',  ( -9.514962460608897388, 142.5298273665900979, -4.999999999999041655 ) ) ;
#55594 = AXIS2_PLACEMENT_3D ( 'NONE', #45551, #71931, #95161 ) ;
#55595 = ADVANCED_FACE ( 'NONE', ( #28087 ), #21435, .F. ) ;
#55596 = CARTESIAN_POINT ( 'NONE',  ( -43.38825400968192980, 436.1092026048715411, 18.83721859163727430 ) ) ;
#55597 = DIRECTION ( 'NONE',  ( 0.000000000000000000, 0.000000000000000000, 1.000000000000000000 ) ) ;
#55598 = ORIENTED_EDGE ( 'NONE', *, *, #36833, .T. ) ;
#55599 = CARTESIAN_POINT ( 'NONE',  ( 37.06438722625302518, 1.482358050883964840E-15, 0.000000000000000000 ) ) ;
#55600 = CARTESIAN_POINT ( 'NONE',  ( 43.00000000000000000, 500.0000000000002274, 0.000000000000000000 ) ) ;
#55601 = VERTEX_POINT ( 'NONE', #23567 ) ;
#55602 = FILL_AREA_STYLE ('',( #21707 ) ) ;
#55603 = SURFACE_SIDE_STYLE ('',( #46486 ) ) ;
#55604 = UNCERTAINTY_MEASURE_WITH_UNIT (LENGTH_MEASURE( 1.000000000000000082E-05 ), #29536, 'distance_accuracy_value', 'NONE');
#55605 = CARTESIAN_POINT ( 'NONE',  ( -106.9148777809588893, -60.00000000000000000, 122.1078712977356275 ) ) ;
#55606 = DIRECTION ( 'NONE',  ( 0.000000000000000000, 1.000000000000000000, 0.000000000000000000 ) ) ;
#55607 = CARTESIAN_POINT ( 'NONE',  ( 25.21823338009918203, 5.000000000000003553, 0.000000000000000000 ) ) ;
#55608 = DIRECTION ( 'NONE',  ( -1.000000000000000000, -0.000000000000000000, -0.000000000000000000 ) ) ;
#55609 = DIRECTION ( 'NONE',  ( -1.000000000000000000, 0.000000000000000000, 0.000000000000000000 ) ) ;
#55610 = EDGE_CURVE ( 'NONE', #41052, #55434, #30067, .T. ) ;
#55611 = CARTESIAN_POINT ( 'NONE',  ( -81.58353690299945526, -57.03497744733997621, 182.7981024581307850 ) ) ;
#55612 = ORIENTED_EDGE ( 'NONE', *, *, #4591, .F. ) ;
#55613 = SURFACE_STYLE_FILL_AREA ( #19 ) ;
#55614 = VERTEX_POINT ( 'NONE', #14361 ) ;
#55615 = DIRECTION ( 'NONE',  ( 0.000000000000000000, -0.000000000000000000, 1.000000000000000000 ) ) ;
#55616 = EDGE_CURVE ( 'NONE', #45510, #31296, #85161, .T. ) ;
#55617 = CARTESIAN_POINT ( 'NONE',  ( 5.858824175751780494, -68.78579060872358752, -1.318356988357134441 ) ) ;
#55618 = CARTESIAN_POINT ( 'NONE',  ( -82.88211207980042161, -37.82423770264409058, 24.55814771371032634 ) ) ;
#55619 = CARTESIAN_POINT ( 'NONE',  ( 36.08349330513379982, 1.593028355512270567E-15, 0.000000000000000000 ) ) ;
#55620 = CARTESIAN_POINT ( 'NONE',  ( -7.151597709147948123, -63.21070734947785752, 3.587174531012142342 ) ) ;
#55621 = CARTESIAN_POINT ( 'NONE',  ( 4.678819457397442427, 8.078722181090824961, -5.000000000000000000 ) ) ;
#55622 = DIRECTION ( 'NONE',  ( 0.000000000000000000, 0.000000000000000000, 1.000000000000000000 ) ) ;
#55623 = CARTESIAN_POINT ( 'NONE',  ( 44.78945892759311675, 1.340359594676612611E-15, 0.000000000000000000 ) ) ;
#55624 = CARTESIAN_POINT ( 'NONE',  ( 110.6388055374740276, -59.99999999999995026, 195.8051704144367591 ) ) ;
#55625 = CARTESIAN_POINT ( 'NONE',  ( -100.4058209406884856, -60.00000000000003553, 69.07134566225379047 ) ) ;
#55626 = CARTESIAN_POINT ( 'NONE',  ( -60.69105336276258100, -60.34595984108710098, 84.28698886197565798 ) ) ;
#55627 = ORIENTED_EDGE ( 'NONE', *, *, #79053, .T. ) ;
#55628 = CARTESIAN_POINT ( 'NONE',  ( 43.67028230287913004, 39.42405813808058923, 48.51753365052933020 ) ) ;
#55629 = CARTESIAN_POINT ( 'NONE',  ( 73.60417151696405824, -59.99999999999506173, 187.5411878019601204 ) ) ;
#55630 = ORIENTED_EDGE ( 'NONE', *, *, #90793, .T. ) ;
#55631 = CARTESIAN_POINT ( 'NONE',  ( 3.060910634449126366, -49.91567764747507141, 32.20382334822807024 ) ) ;
#55632 = CARTESIAN_POINT ( 'NONE',  ( -2.977408999572654480, -20.00000000204838457, 7.188101187499999156 ) ) ;
#55633 = CIRCLE ( 'NONE', #41881, 33.82893434829264123 ) ;
#55634 = SURFACE_STYLE_FILL_AREA ( #96663 ) ;
#55635 = ORIENTED_EDGE ( 'NONE', *, *, #2196, .T. ) ;
#55636 = CARTESIAN_POINT ( 'NONE',  ( -3.313708498984779371, -27.21875000409677270, -7.999999999999981348 ) ) ;
#55637 = ORIENTED_EDGE ( 'NONE', *, *, #104139, .F. ) ;
#55638 = FACE_OUTER_BOUND ( 'NONE', #44705, .T. ) ;
#55639 = PRESENTATION_LAYER_ASSIGNMENT (  '', '', ( #74595 ) ) ;
#55640 = LINE ( 'NONE', #47036, #55779 ) ;
#55641 = CARTESIAN_POINT ( 'NONE',  ( -109.7211485432284803, -60.00000000000001421, 192.0136906049105505 ) ) ;
#55642 = CARTESIAN_POINT ( 'NONE',  ( 36.28838933700914282, 352.2791627080521835, 1.187119259579878738 ) ) ;
#55643 = CARTESIAN_POINT ( 'NONE',  ( 7.188101187499999156, -24.12500000204838457, 2.977408999572654924 ) ) ;
#55644 = DIRECTION ( 'NONE',  ( 0.000000000000000000, 1.000000000000000000, 0.000000000000000000 ) ) ;
#55645 = CARTESIAN_POINT ( 'NONE',  ( -3.013510815085704841, 20.49548354705801501, -6.321220078560170208 ) ) ;
#55646 = DIRECTION ( 'NONE',  ( 0.000000000000000000, 1.000000000000000000, 0.000000000000000000 ) ) ;
#55647 = CARTESIAN_POINT ( 'NONE',  ( -5.036189802313092656, 48.00000000000000000, -93.73786388412078452 ) ) ;
#55648 = CARTESIAN_POINT ( 'NONE',  ( 11.36457253998776551, -9.486455709443886164, 18.81580886345433967 ) ) ;
#55649 = DIRECTION ( 'NONE',  ( 0.000000000000000000, 0.000000000000000000, 1.000000000000000000 ) ) ;
#55650 = CARTESIAN_POINT ( 'NONE',  ( 101.7378945492313562, -60.00000000000000000, 194.4303705058995604 ) ) ;
#55651 = CARTESIAN_POINT ( 'NONE',  ( -37.69739591874598972, -53.35635198386449929, 39.83913967554838109 ) ) ;
#55652 = ORIENTED_EDGE ( 'NONE', *, *, #56761, .T. ) ;
#55653 =( LENGTH_UNIT ( ) NAMED_UNIT ( * ) SI_UNIT ( .MILLI., .METRE. ) );
#55654 = CIRCLE ( 'NONE', #86737, 5.000000000000002665 ) ;
#55655 = CARTESIAN_POINT ( 'NONE',  ( 40.76590610560279515, -53.34231791925814292, 42.49342577743990290 ) ) ;
#55656 = CARTESIAN_POINT ( 'NONE',  ( 13.66642973271503081, -8.673617379884035472E-16, -17.78317311657917088 ) ) ;
#55657 = VERTEX_POINT ( 'NONE', #3244 ) ;
#55658 = FACE_OUTER_BOUND ( 'NONE', #50657, .T. ) ;
#55659 = CARTESIAN_POINT ( 'NONE',  ( -62.11818655019798996, -38.34127833389678841, 103.2225466343185047 ) ) ;
#55660 = EDGE_LOOP ( 'NONE', ( #38901, #41280, #21501, #65200, #98525 ) ) ;
#55662 = CARTESIAN_POINT ( 'NONE',  ( -31.11679462788039530, 441.4271381875185511, 23.27438508043199406 ) ) ;
#55661 = CARTESIAN_POINT ( 'NONE',  ( 8.435052862587294698, -4.999999999999999112, -16.32561095844542720 ) ) ;
#55663 = CARTESIAN_POINT ( 'NONE',  ( 15.73424097804762489, 37.19149822104526493, 22.31191215652642867 ) ) ;
#55664 = CARTESIAN_POINT ( 'NONE',  ( 0.000000000000000000, 34.00000000000000000, 0.000000000000000000 ) ) ;
#55665 = CARTESIAN_POINT ( 'NONE',  ( 2.099928008175702901E-23, 44.08548369317413318, -16.25000000000000000 ) ) ;
#55666 = LINE ( 'NONE', #73995, #79083 ) ;
#55667 = CARTESIAN_POINT ( 'NONE',  ( -49.28001195564456083, 13.04047724765254301, -15.62422648184040064 ) ) ;
#55668 = CARTESIAN_POINT ( 'NONE',  ( -3.647056030525466674, -49.00888714197444074, 43.86785402897538688 ) ) ;
#55669 = CARTESIAN_POINT ( 'NONE',  ( 97.95620506833432728, -59.99999999999999289, 68.65487923523417635 ) ) ;
#55670 = AXIS2_PLACEMENT_3D ( 'NONE', #83984, #35476, #68346 ) ;
#55671 = AXIS2_PLACEMENT_3D ( 'NONE', #103735, #53593, #19681 ) ;
#55672 = DIRECTION ( 'NONE',  ( -0.000000000000000000, -1.000000000000000000, -0.000000000000000000 ) ) ;
#55673 = CARTESIAN_POINT ( 'NONE',  ( 9.500000000000003553, -5.000000000000000000, -68.91429205785459544 ) ) ;
#55674 = ORIENTED_EDGE ( 'NONE', *, *, #16127, .F. ) ;
#55675 = EDGE_CURVE ( 'NONE', #91175, #30104, #98913, .T. ) ;
#55676 = PRESENTATION_LAYER_ASSIGNMENT (  '', '', ( #9175 ) ) ;
#55677 = CONICAL_SURFACE ( 'NONE', #89733, 4.000000000000001776, 0.9599310885968808105 ) ;
#55678 = CARTESIAN_POINT ( 'NONE',  ( -80.61473454522898408, -29.99999999998848565, -24.48213655620298113 ) ) ;
#55679 = VERTEX_POINT ( 'NONE', #13841 ) ;
#55680 = CARTESIAN_POINT ( 'NONE',  ( -9.996020202094923590, -57.99966105432783792, 27.38654800878193996 ) ) ;
#55681 = CARTESIAN_POINT ( 'NONE',  ( -15.89812512823622015, 3.583431000110255837, 3.067165457295355946 ) ) ;
#55682 = CARTESIAN_POINT ( 'NONE',  ( 3.168323364909926720, 39.18318371059633876, 5.000000000000000000 ) ) ;
#55683 = CARTESIAN_POINT ( 'NONE',  ( 15.64030048137865592, 21.26710225494213091, 5.626279437277405648 ) ) ;
#55684 = CARTESIAN_POINT ( 'NONE',  ( -6.499999999999996447, 1.286902272306384987, -0.09436334093185638761 ) ) ;
#55685 = AXIS2_PLACEMENT_3D ( 'NONE', #101358, #52798, #18883 ) ;
#55686 = CARTESIAN_POINT ( 'NONE',  ( -2.977408999572654480, -26.00000000204839168, 7.188101187499999156 ) ) ;
#55688 = EDGE_CURVE ( 'NONE', #60190, #36049, #102700, .T. ) ;
#55687 = DIRECTION ( 'NONE',  ( 0.000000000000000000, 0.000000000000000000, 1.000000000000000000 ) ) ;
#55689 = CARTESIAN_POINT ( 'NONE',  ( 36.48461538461538822, 4.172000000000003261, 5.109226446042759579E-16 ) ) ;
#55690 = SHAPE_REPRESENTATION ( '7. Anchor', ( #10728 ), #38490 ) ;
#55691 = CARTESIAN_POINT ( 'NONE',  ( 7.126323127734462304, 41.48433382013136139, -70.04207035317314478 ) ) ;
#55692 = ORIENTED_EDGE ( 'NONE', *, *, #64545, .T. ) ;
#55694 = ORIENTED_EDGE ( 'NONE', *, *, #98224, .F. ) ;
#55693 = CARTESIAN_POINT ( 'NONE',  ( 4.898587196589412829E-16, -9.312500004096769146, -8.000000000000000000 ) ) ;
#55695 = CARTESIAN_POINT ( 'NONE',  ( 78.76512178856368962, -60.31316846768228856, 162.6500093631206312 ) ) ;
#55696 = LINE ( 'NONE', #15264, #23093 ) ;
#55697 = ORIENTED_EDGE ( 'NONE', *, *, #70424, .T. ) ;
#55698 = CARTESIAN_POINT ( 'NONE',  ( -12.50000000000000355, 34.57130022983270834, -53.73004006193110627 ) ) ;
#55699 = CARTESIAN_POINT ( 'NONE',  ( -14.68532172034886507, 1.589195250049053598, 3.050719247027746217 ) ) ;
#55700 = CARTESIAN_POINT ( 'NONE',  ( -2.977408999572654480, -13.62500000204838457, 7.188101187499999156 ) ) ;
#55701 = DIRECTION ( 'NONE',  ( -0.000000000000000000, -1.000000000000000000, -0.000000000000000000 ) ) ;
#55702 = CARTESIAN_POINT ( 'NONE',  ( -70.46077158043857480, -57.68242143155622159, 157.6729293506350018 ) ) ;
#55703 = CARTESIAN_POINT ( 'NONE',  ( 6.289572920342628493, -5.584521518880464441, -3.985288806461544375 ) ) ;
#55704 = ORIENTED_EDGE ( 'NONE', *, *, #95708, .F. ) ;
#55705 =( NAMED_UNIT ( * ) PLANE_ANGLE_UNIT ( ) SI_UNIT ( $, .RADIAN. ) );
#55706 = CARTESIAN_POINT ( 'NONE',  ( 4.898587196589412829E-16, -12.31250000409676915, -8.000000000000000000 ) ) ;
#55707 = DIRECTION ( 'NONE',  ( 0.000000000000000000, -0.000000000000000000, 1.000000000000000000 ) ) ;
#55708 = CARTESIAN_POINT ( 'NONE',  ( 16.84999999999999787, 1.533819458162526451E-15, 0.000000000000000000 ) ) ;
#55709 = CARTESIAN_POINT ( 'NONE',  ( -6.499999999999999112, -3.752776749732587902, -6.064240316920403551 ) ) ;
#55710 = EDGE_CURVE ( 'NONE', #77744, #88227, #74404, .T. ) ;
#55711 = EDGE_LOOP ( 'NONE', ( #62628, #100527, #97496 ) ) ;
#55712 = CARTESIAN_POINT ( 'NONE',  ( -1.469576158976823947E-15, -11.56250000409677092, 8.000000000000000000 ) ) ;
#55713 = CARTESIAN_POINT ( 'NONE',  ( -4.871453668401689791E-08, -12.57758911513053413, 32.18678843846154081 ) ) ;
#55714 = SURFACE_STYLE_FILL_AREA ( #63855 ) ;
#55715 = AXIS2_PLACEMENT_3D ( 'NONE', #5618, #38541, #61765 ) ;
#55716 = CARTESIAN_POINT ( 'NONE',  ( 32.85555225121232326, 465.7063523440039603, 11.00064571225391852 ) ) ;
#55717 = CARTESIAN_POINT ( 'NONE',  ( -9.221249107921748234, 86.04821371498486826, 3.869340886054257300 ) ) ;
#55718 = AXIS2_PLACEMENT_3D ( 'NONE', #63497, #87235, #23044 ) ;
#55719 = APPLICATION_PROTOCOL_DEFINITION ( 'draft international standard', 'automotive_design', 1998, #74819 ) ;
#55720 = CARTESIAN_POINT ( 'NONE',  ( 38.66062501847530086, 27.30206768824636754, 12.83416379226657789 ) ) ;
#55721 = ORIENTED_EDGE ( 'NONE', *, *, #106116, .T. ) ;
#55722 = CARTESIAN_POINT ( 'NONE',  ( -6.835997281635401102, -47.84397377247658767, 39.21766570620285108 ) ) ;
#55723 = CARTESIAN_POINT ( 'NONE',  ( -3.827754797006214016, 15.98931925350938243, 9.240220675753590740 ) ) ;
#55724 = CIRCLE ( 'NONE', #85023, 4.000000000000001776 ) ;
#55725 = CARTESIAN_POINT ( 'NONE',  ( -3.787270392904598992, 16.53964648752899791, -5.888179741704394843 ) ) ;
#55726 = CARTESIAN_POINT ( 'NONE',  ( -72.67357598896492732, -38.32474216590297544, -30.15551316088291856 ) ) ;
#55727 = CARTESIAN_POINT ( 'NONE',  ( 11.84999999999999787, 1.533819458162526451E-15, 0.000000000000000000 ) ) ;
#55728 = ADVANCED_FACE ( 'NONE', ( #40248 ), #56948, .T. ) ;
#55729 = CARTESIAN_POINT ( 'NONE',  ( 7.500000000000007105, 40.00000000000000000, -58.69229087761227248 ) ) ;
#55730 = EDGE_LOOP ( 'NONE', ( #40543, #71787, #59399, #102785, #60824 ) ) ;
#55731 = CARTESIAN_POINT ( 'NONE',  ( -25.89567525304408946, 37.13054467105123280, -9.163018210787793549 ) ) ;
#55732 = CARTESIAN_POINT ( 'NONE',  ( 101.8619292074444616, -57.63174066258962824, 203.3235957780899525 ) ) ;
#55733 = CARTESIAN_POINT ( 'NONE',  ( 70.79744548977303964, -21.77034749440733563, -19.10173070115413552 ) ) ;
#55734 = CARTESIAN_POINT ( 'NONE',  ( -4.444974277458374701, -4.939246403833604582, -5.720331885005381700 ) ) ;
#55735 = CARTESIAN_POINT ( 'NONE',  ( 85.59800593614014019, 1.016364837396684119E-14, 0.000000000000000000 ) ) ;
#55736 = CARTESIAN_POINT ( 'NONE',  ( -5.290067270632215823, 53.47475093287481229, 8.531152949374556371 ) ) ;
#55737 = CARTESIAN_POINT ( 'NONE',  ( -73.06098663455794906, -60.00000000000000000, 163.0166479149870042 ) ) ;
#55738 = CARTESIAN_POINT ( 'NONE',  ( -42.09210974227526947, 317.4093497706929270, -4.557617623460385126 ) ) ;
#55739 = LINE ( 'NONE', #80559, #82061 ) ;
#55740 = CARTESIAN_POINT ( 'NONE',  ( -60.62677696746660416, 49.99999999999999289, 24.18439665019479179 ) ) ;
#55741 = CARTESIAN_POINT ( 'NONE',  ( -83.62637298746453496, -57.37962585073366739, 189.9592516013256613 ) ) ;
#55743 = ORIENTED_EDGE ( 'NONE', *, *, #106717, .F. ) ;
#55742 = VECTOR ( 'NONE', #100565, 1000.000000000000000 ) ;
#55744 = CARTESIAN_POINT ( 'NONE',  ( 35.76699745686483567, 397.0856500282078514, 5.951853049970027065 ) ) ;
#55745 = ORIENTED_EDGE ( 'NONE', *, *, #42075, .T. ) ;
#55746 = DIRECTION ( 'NONE',  ( -1.000000000000000000, -1.224606353822377258E-16, -0.000000000000000000 ) ) ;
#55747 = EDGE_CURVE ( 'NONE', #39953, #14796, #58014, .T. ) ;
#55748 = CARTESIAN_POINT ( 'NONE',  ( -21.32035683309257124, 303.9777306799145435, -9.973210722144571605 ) ) ;
#55749 = CARTESIAN_POINT ( 'NONE',  ( -82.80220596410995881, -45.26056562500249925, -14.83041380441539481 ) ) ;
#55750 = CARTESIAN_POINT ( 'NONE',  ( 42.61650669486618881, 4.898587196589411843E-16, -4.000000000000000888 ) ) ;
#55751 = AXIS2_PLACEMENT_3D ( 'NONE', #99769, #66884, #32411 ) ;
#55752 = VERTEX_POINT ( 'NONE', #90941 ) ;
#55753 = EDGE_CURVE ( 'NONE', #61515, #21783, #9371, .T. ) ;
#55754 = CARTESIAN_POINT ( 'NONE',  ( 18.11660520461541068, 50.00000000000000711, 61.73928013098095846 ) ) ;
#55755 = CARTESIAN_POINT ( 'NONE',  ( 12.27263865982193991, 5.738677695749484720, 8.480951842185072920 ) ) ;
#55756 = EDGE_CURVE ( 'NONE', #5970, #89905, #49957, .T. ) ;
#55757 = CARTESIAN_POINT ( 'NONE',  ( -13.60704923275580924, -1.734723475976807094E-15, -10.45706415777457465 ) ) ;
#55758 = CARTESIAN_POINT ( 'NONE',  ( -33.21585456068780928, 485.3968598107930461, 4.030361751305823859 ) ) ;
#55759 = CARTESIAN_POINT ( 'NONE',  ( 63.50796903478703115, -60.00000000000007816, -37.13796669901890368 ) ) ;
#55760 = CARTESIAN_POINT ( 'NONE',  ( -79.97615926384021634, -39.50033131370128814, 145.6677927735757976 ) ) ;
#55761 = ORIENTED_EDGE ( 'NONE', *, *, #56973, .T. ) ;
#55762 = CARTESIAN_POINT ( 'NONE',  ( 12.83322425571993186, -59.99999999999995737, 42.04720346242444151 ) ) ;
#55763 = CARTESIAN_POINT ( 'NONE',  ( 84.69632291683485903, -57.55696416148584404, 202.1270370136284953 ) ) ;
#55764 = CARTESIAN_POINT ( 'NONE',  ( 0.06682554136337939821, 6.264794173742277650, 2.149058192116895860 ) ) ;
#55765 = CARTESIAN_POINT ( 'NONE',  ( 30.92869529702126385, 309.2766731770143451, -8.518754327849393349 ) ) ;
#55766 = CARTESIAN_POINT ( 'NONE',  ( 0.4042117618287688896, -3.141900367811087502, -6.500000000000000000 ) ) ;
#55767 = EDGE_LOOP ( 'NONE', ( #78150, #35264 ) ) ;
#55768 = CARTESIAN_POINT ( 'NONE',  ( -22.57534922171806357, 26.08024732591615802, 30.87069056292416391 ) ) ;
#55769 = EDGE_CURVE ( 'NONE', #22401, #71702, #97235, .T. ) ;
#55770 = ADVANCED_FACE ( 'NONE', ( #8937, #811 ), #86138, .F. ) ;
#55771 = CARTESIAN_POINT ( 'NONE',  ( -12.50000000000000178, -1.322513981592677412, -16.28752265597966087 ) ) ;
#55773 = CARTESIAN_POINT ( 'NONE',  ( -104.1865559966542634, -52.71019955170553573, 153.9800267041457005 ) ) ;
#55772 = CARTESIAN_POINT ( 'NONE',  ( -15.90864490579666679, 37.20836975595027241, 22.13037531087898557 ) ) ;
#55774 = CARTESIAN_POINT ( 'NONE',  ( 2.977408999572651815, -17.93750000204838457, 7.188101187500000933 ) ) ;
#55775 = CARTESIAN_POINT ( 'NONE',  ( 8.099999999999999645, 3.752776749732565253, 6.499999999999997335 ) ) ;
#55776 = CARTESIAN_POINT ( 'NONE',  ( 9.918010731619574472, 81.20848315156776209, -1.300854425901574185 ) ) ;
#55777 = CARTESIAN_POINT ( 'NONE',  ( 0.1684925962546267031, 35.08181111624586634, 27.25000000000001066 ) ) ;
#55778 = CARTESIAN_POINT ( 'NONE',  ( 33.86650669486618881, 1.474610560812782335E-15, 0.000000000000000000 ) ) ;
#55779 = VECTOR ( 'NONE', #56166, 1000.000000000000000 ) ;
#55780 = ORIENTED_EDGE ( 'NONE', *, *, #79789, .F. ) ;
#55781 = CARTESIAN_POINT ( 'NONE',  ( 43.46689911038843235, 485.4921130118005408, 4.095024577346555894 ) ) ;
#55783 = CARTESIAN_POINT ( 'NONE',  ( 26.60165167295768640, -22.09540625163044325, 29.10608926666087726 ) ) ;
#55782 = CARTESIAN_POINT ( 'NONE',  ( -28.84153870763153904, -30.00000000000004619, 39.52238898731670247 ) ) ;
#55784 = CARTESIAN_POINT ( 'NONE',  ( -4.506590204516032649, 52.18349789241705139, -6.292748301456810189 ) ) ;
#55785 = ORIENTED_EDGE ( 'NONE', *, *, #100644, .F. ) ;
#55786 = UNCERTAINTY_MEASURE_WITH_UNIT (LENGTH_MEASURE( 1.000000000000000082E-05 ), #40850, 'distance_accuracy_value', 'NONE');
#55787 = ORIENTED_EDGE ( 'NONE', *, *, #79121, .F. ) ;
#55789 = CARTESIAN_POINT ( 'NONE',  ( 37.72113205395461222, 461.3706430627456712, 2.610878261945020373 ) ) ;
#55788 = DIRECTION ( 'NONE',  ( 0.000000000000000000, 0.000000000000000000, 1.000000000000000000 ) ) ;
#55790 =( NAMED_UNIT ( * ) PLANE_ANGLE_UNIT ( ) SI_UNIT ( $, .RADIAN. ) );
#55791 =( GEOMETRIC_REPRESENTATION_CONTEXT ( 3 ) GLOBAL_UNCERTAINTY_ASSIGNED_CONTEXT ( ( #71804 ) ) GLOBAL_UNIT_ASSIGNED_CONTEXT ( ( #55870, #54286, #101927 ) ) REPRESENTATION_CONTEXT ( 'NONE', 'WORKASPACE' ) );
#55792 = DIRECTION ( 'NONE',  ( 0.000000000000000000, -1.000000000000000000, 0.000000000000000000 ) ) ;
#55793 = FILL_AREA_STYLE ('',( #5681 ) ) ;
#55794 = ORIENTED_EDGE ( 'NONE', *, *, #45173, .F. ) ;
#55795 = B_SPLINE_CURVE_WITH_KNOTS ( 'NONE', 3,
 ( #106049, #106594, #57501, #74751, #40273, #7891, #15457, #73147, #8957, #33802, #32202, #300 ),
 .UNSPECIFIED., .F., .F.,
 ( 4, 2, 2, 2, 2, 4 ),
 ( 0.000000000000000000, 0.0007243314081738727811, 0.001086497112260805323, 0.001448662816347737973, 0.002172994224521602839, 0.002897325632695468139 ),
 .UNSPECIFIED. ) ;
#55796 = CARTESIAN_POINT ( 'NONE',  ( 52.74623303553200060, -60.00000000000001421, -37.36890884799756662 ) ) ;
#55797 = DIRECTION ( 'NONE',  ( 0.000000000000000000, -1.000000000000000000, 0.000000000000000000 ) ) ;
#55798 = CIRCLE ( 'NONE', #23132, 4.000000000000001776 ) ;
#55799 = CARTESIAN_POINT ( 'NONE',  ( 0.000000000000000000, 44.00000000000000711, 61.50000000000000000 ) ) ;
#55800 = CARTESIAN_POINT ( 'NONE',  ( 0.000000000000000000, 0.000000000000000000, -5.185501489199872083 ) ) ;
#55801 = CARTESIAN_POINT ( 'NONE',  ( 47.24160628166276865, 11.75468494072138625, -16.58444347056465062 ) ) ;
#55802 = ORIENTED_EDGE ( 'NONE', *, *, #19549, .T. ) ;
#55803 = EDGE_CURVE ( 'NONE', #94714, #35053, #85226, .T. ) ;
#55804 = ORIENTED_EDGE ( 'NONE', *, *, #72338, .T. ) ;
#55805 = ORIENTED_EDGE ( 'NONE', *, *, #2102, .F. ) ;
#55806 = DIRECTION ( 'NONE',  ( 0.000000000000000000, 0.000000000000000000, 1.000000000000000000 ) ) ;
#55807 = CARTESIAN_POINT ( 'NONE',  ( 43.95556679493488872, 485.1369594940165371, -0.2799375260811446942 ) ) ;
#55808 = DIRECTION ( 'NONE',  ( 0.000000000000000000, 0.000000000000000000, 1.000000000000000000 ) ) ;
#55809 = CARTESIAN_POINT ( 'NONE',  ( -35.26357035561092346, 324.0757595391598329, -4.811724253201282053 ) ) ;
#55810 = CARTESIAN_POINT ( 'NONE',  ( -2.531139591009138989, -70.38595913997060904, 13.22873017836408494 ) ) ;
#55811 = FACE_OUTER_BOUND ( 'NONE', #22047, .T. ) ;
#55813 = EDGE_CURVE ( 'NONE', #81667, #76808, #33588, .T. ) ;
#55812 = FACE_OUTER_BOUND ( 'NONE', #68751, .T. ) ;
#55814 = EDGE_LOOP ( 'NONE', ( #6408, #28786, #66739, #54603, #32574, #71353 ) ) ;
#55815 = CARTESIAN_POINT ( 'NONE',  ( 0.000000000000000000, 0.000000000000000000, 0.000000000000000000 ) ) ;
#55816 = VERTEX_POINT ( 'NONE', #27309 ) ;
#55817 = CARTESIAN_POINT ( 'NONE',  ( 0.000000000000000000, 0.000000000000000000, 0.000000000000000000 ) ) ;
#55818 = CARTESIAN_POINT ( 'NONE',  ( -38.94709829050781735, 485.6592143718707462, -4.427571171334746758 ) ) ;
#55819 = CARTESIAN_POINT ( 'NONE',  ( -16.68757544607984755, -59.99999999999999289, 34.10598086550765373 ) ) ;
#55820 = CARTESIAN_POINT ( 'NONE',  ( 66.03004151298199531, -39.48245408485600194, 89.23762064710109598 ) ) ;
#55821 = AXIS2_PLACEMENT_3D ( 'NONE', #36684, #102438, #29136 ) ;
#55822 = EDGE_LOOP ( 'NONE', ( #50397, #42644, #53465, #56053, #2909, #47643 ) ) ;
#55823 = CARTESIAN_POINT ( 'NONE',  ( 31.36650669486618881, 1.474610560812782335E-15, 0.000000000000000000 ) ) ;
#55824 = CARTESIAN_POINT ( 'NONE',  ( 1.235538725728271446E-15, -5.788408252967909284, -2.974182810908597929 ) ) ;
#55825 =( BOUNDED_SURFACE ( )  B_SPLINE_SURFACE ( 3, 2, ( 
 ( #68062, #9807, #10345 ),
 ( #41659, #51866, #17935 ),
 ( #1163, #99340, #2243 ),
 ( #58375, #1720, #27653 ) ),
 .UNSPECIFIED., .F., .F., .F. ) 
 B_SPLINE_SURFACE_WITH_KNOTS ( ( 4, 4 ),
 ( 3, 3 ),
 ( 0.01809742499366328097, 0.04402311302153927297 ),
 ( 0.000000000000000000, 1.000000000000000000 ),
 .UNSPECIFIED. ) 
 GEOMETRIC_REPRESENTATION_ITEM ( )  RATIONAL_B_SPLINE_SURFACE ( (
 ( 1.000000000000000000, 0.8381406085707386877, 1.000000000000000000),
 ( 1.000000000000000000, 0.8381408009587134611, 1.000000000000000000),
 ( 1.000000000000000000, 0.8381407633130539825, 1.000000000000000000),
 ( 1.000000000000000000, 0.8381405729626264511, 1.000000000000000000) ) ) 
 REPRESENTATION_ITEM ( '' )  SURFACE ( )  );
#55826 = STYLED_ITEM ( 'NONE', ( #76022 ), #98511 ) ;
#55827 = DIRECTION ( 'NONE',  ( -0.000000000000000000, -0.000000000000000000, 1.000000000000000000 ) ) ;
#55828 = EDGE_CURVE ( 'NONE', #78737, #61410, #76894, .T. ) ;
#55829 = COLOUR_RGB ( '', 0.08235294, 0.09019608, 0.10196078) ;
#55831 = ORIENTED_EDGE ( 'NONE', *, *, #27246, .T. ) ;
#55830 = CIRCLE ( 'NONE', #100667, 4.000000000000000888 ) ;
#55832 = FILL_AREA_STYLE_COLOUR ( '', #14195 ) ;
#55833 = CARTESIAN_POINT ( 'NONE',  ( 46.77678417914661679, 18.74709138458479529, 15.58010501040359586 ) ) ;
#55834 = DIRECTION ( 'NONE',  ( 0.000000000000000000, 0.000000000000000000, -1.000000000000000000 ) ) ;
#55835 = B_SPLINE_CURVE_WITH_KNOTS ( 'NONE', 3,
 ( #68957, #36613, #29578, #11741, #46783, #94826 ),
 .UNSPECIFIED., .F., .F.,
 ( 4, 2, 4 ),
 ( -4.698498716302674511E-06, 0.0003457374136927991335, 0.0006961733261019009255 ),
 .UNSPECIFIED. ) ;
#55836 = CARTESIAN_POINT ( 'NONE',  ( 8.000000000000000000, -32.18750000409676915, 0.000000000000000000 ) ) ;
#55837 = CARTESIAN_POINT ( 'NONE',  ( -2.617993873628327250, -5.000000000000000000, 10.00000000000000000 ) ) ;
#55838 = CARTESIAN_POINT ( 'NONE',  ( 86.94434408382100798, -28.02298374760003341, 186.6917276570115121 ) ) ;
#55839 = DIRECTION ( 'NONE',  ( -0.000000000000000000, -0.000000000000000000, -1.000000000000000000 ) ) ;
#55840 = CARTESIAN_POINT ( 'NONE',  ( -9.996167984597942535, 7.505519767266282116, 0.000000000000000000 ) ) ;
#55841 = CARTESIAN_POINT ( 'NONE',  ( 3.334874873180000421, 304.8518027755578146, 8.936999414886647841 ) ) ;
#55842 = ORIENTED_EDGE ( 'NONE', *, *, #43040, .F. ) ;
#55843 = CARTESIAN_POINT ( 'NONE',  ( 26.36650669486618881, 4.898587196589411843E-16, -4.000000000000000888 ) ) ;
#55844 = CARTESIAN_POINT ( 'NONE',  ( 0.2578475836320663905, 4.367703157927318891, -5.434916218090831030 ) ) ;
#55845 = CARTESIAN_POINT ( 'NONE',  ( 33.36523397932889878, -60.00000000000000000, 45.10737781336894159 ) ) ;
#55846 = CARTESIAN_POINT ( 'NONE',  ( -100.3771068072541652, -30.00000000000000000, 157.7691867327778539 ) ) ;
#55847 = AXIS2_PLACEMENT_3D ( 'NONE', #62224, #64, #73982 ) ;
#55848 = CARTESIAN_POINT ( 'NONE',  ( 0.000000000000000000, 0.000000000000000000, 5.000000000000000888 ) ) ;
#55849 = CARTESIAN_POINT ( 'NONE',  ( 52.17722917352445222, -57.67658636093570834, 83.19373642209534125 ) ) ;
#55851 = CARTESIAN_POINT ( 'NONE',  ( 44.11327388758706292, 464.4313852428374503, 9.822198357557169857 ) ) ;
#55850 = CARTESIAN_POINT ( 'NONE',  ( 0.000000000000000000, 15.00000000000000000, 10.00000000000000000 ) ) ;
#55852 = CARTESIAN_POINT ( 'NONE',  ( 7.500000000000000000, 4.330127018922189208, -10.00000000000000000 ) ) ;
#55853 = CARTESIAN_POINT ( 'NONE',  ( -32.20917000857141943, 464.7502426416677395, 11.12081798558170753 ) ) ;
#55854 = CARTESIAN_POINT ( 'NONE',  ( -43.70848695378470694, 435.5669781845214743, 16.96397918787651449 ) ) ;
#55855 = CARTESIAN_POINT ( 'NONE',  ( -9.265796308445876761, -59.99999999999999289, 39.64115480165225591 ) ) ;
#55856 = CIRCLE ( 'NONE', #47595, 5.000000000000002665 ) ;
#55857 = MECHANICAL_DESIGN_GEOMETRIC_PRESENTATION_REPRESENTATION (  '', ( #66282 ), #83454 ) ;
#55858 = AXIS2_PLACEMENT_3D ( 'NONE', #95746, #87663, #13744 ) ;
#55859 = FILL_AREA_STYLE_COLOUR ( '', #103681 ) ;
#55860 = STYLED_ITEM ( 'NONE', ( #97719 ), #85645 ) ;
#55861 = PRESENTATION_STYLE_ASSIGNMENT (( #30058 ) ) ;
#55862 = VERTEX_POINT ( 'NONE', #19750 ) ;
#55863 = CARTESIAN_POINT ( 'NONE',  ( 17.50000000000004974, 51.99999999999999289, 59.86364615470024830 ) ) ;
#55864 = CARTESIAN_POINT ( 'NONE',  ( 39.30282183805196894, 437.8662848125126175, 22.91975680305879948 ) ) ;
#55865 = CARTESIAN_POINT ( 'NONE',  ( -12.31021798142609747, -32.51299227848760864, 29.36066974128064544 ) ) ;
#55867 = FACE_OUTER_BOUND ( 'NONE', #36348, .T. ) ;
#55866 = CARTESIAN_POINT ( 'NONE',  ( -105.5472279711990069, -60.00000000000000711, 185.2932126898874969 ) ) ;
#55868 = EDGE_CURVE ( 'NONE', #98655, #65067, #35297, .T. ) ;
#55869 = ORIENTED_EDGE ( 'NONE', *, *, #47456, .T. ) ;
#55870 =( LENGTH_UNIT ( ) NAMED_UNIT ( * ) SI_UNIT ( .MILLI., .METRE. ) );
#55871 = EDGE_CURVE ( 'NONE', #696, #942, #97505, .T. ) ;
#55872 = CARTESIAN_POINT ( 'NONE',  ( -5.079306836894615707, -4.308466644846057569, -17.11871833148123301 ) ) ;
#55873 = FACE_OUTER_BOUND ( 'NONE', #33511, .T. ) ;
#55874 = EDGE_CURVE ( 'NONE', #16503, #90846, #98983, .T. ) ;
#55875 = ADVANCED_FACE ( 'NONE', ( #53656 ), #86588, .F. ) ;
#55876 = CARTESIAN_POINT ( 'NONE',  ( -7.801642220026312025, -81.41203173850968255, 1.787233835843583751 ) ) ;
#55877 = CARTESIAN_POINT ( 'NONE',  ( 73.07796749574373507, -60.00000000000000711, 163.1709902845379077 ) ) ;
#55878 = DIRECTION ( 'NONE',  ( -1.000000000000000000, -1.224606353822377258E-16, -0.000000000000000000 ) ) ;
#55879 = ORIENTED_EDGE ( 'NONE', *, *, #85442, .T. ) ;
#55880 = CARTESIAN_POINT ( 'NONE',  ( -43.04469050570867239, 434.7734435962895532, 9.248231035232468145 ) ) ;
#55881 = CARTESIAN_POINT ( 'NONE',  ( 0.000000000000000000, 0.000000000000000000, 5.000000000000002665 ) ) ;
#55883 = CARTESIAN_POINT ( 'NONE',  ( 4.919733272805031810, -1.562181361514374034, 104.2477112191710802 ) ) ;
#55882 = CARTESIAN_POINT ( 'NONE',  ( 28.47648766833107103, -14.21045842199436926, 36.49840447651481412 ) ) ;
#55884 = CARTESIAN_POINT ( 'NONE',  ( 4.678819457397416670, 143.9212778189090614, -5.000000000000000000 ) ) ;
#55885 = CARTESIAN_POINT ( 'NONE',  ( -4.844458925424343754, -2.858988884355133209, 103.3760426044467380 ) ) ;
#55886 = ORIENTED_EDGE ( 'NONE', *, *, #9395, .T. ) ;
#55887 = ADVANCED_FACE ( 'NONE', ( #31537 ), #67528, .F. ) ;
#55888 = CARTESIAN_POINT ( 'NONE',  ( -25.08362175616396073, 307.4904678873484158, 9.538446063109352835 ) ) ;
#55889 = VERTEX_POINT ( 'NONE', #40652 ) ;
#55890 = CYLINDRICAL_SURFACE ( 'NONE', #3511, 8.000000000000000000 ) ;
#55891 = VECTOR ( 'NONE', #27271, 1000.000000000000114 ) ;
#55892 = LINE ( 'NONE', #47813, #102628 ) ;
#55893 = DIRECTION ( 'NONE',  ( 0.000000000000000000, 0.000000000000000000, 1.000000000000000000 ) ) ;
#55894 = ORIENTED_EDGE ( 'NONE', *, *, #37845, .T. ) ;
#55895 = CARTESIAN_POINT ( 'NONE',  ( -15.74020471409081168, -23.10826456785950356, 36.04230649636249950 ) ) ;
#55896 = FILL_AREA_STYLE ('',( #95873 ) ) ;
#55897 = CARTESIAN_POINT ( 'NONE',  ( -10.00000000000000000, 7.499999999999984901, -0.3301471707461320904 ) ) ;
#55898 = CARTESIAN_POINT ( 'NONE',  ( -93.89671634583459081, -60.00000000000852651, 204.9703477895711217 ) ) ;
#55899 = CARTESIAN_POINT ( 'NONE',  ( 46.00000000000000711, 486.3992880160790264, 3.759606857460338958 ) ) ;
#55900 = CARTESIAN_POINT ( 'NONE',  ( 54.58065226052892882, -60.00000000000002842, 84.04142156818011244 ) ) ;
#55901 = CARTESIAN_POINT ( 'NONE',  ( 1.219713087837473786, 25.73165379248329998, -39.18301856506552383 ) ) ;
#55903 = CARTESIAN_POINT ( 'NONE',  ( 13.66819726461015705, -53.39670533342206227, 32.87928641480030478 ) ) ;
#55902 = CARTESIAN_POINT ( 'NONE',  ( -106.9108898249343156, -14.21045842199431242, 176.0583478801969193 ) ) ;
#55904 = CARTESIAN_POINT ( 'NONE',  ( 82.87101461148294845, -37.99999999999997868, 1.285415469843371294 ) ) ;
#55905 = SURFACE_SIDE_STYLE ('',( #65630 ) ) ;
#55906 = CARTESIAN_POINT ( 'NONE',  ( -47.75002082045136831, -29.14752499694496990, 44.14896982249094037 ) ) ;
#55907 = CARTESIAN_POINT ( 'NONE',  ( -0.3346257469825759667, 34.18677894913321325, -29.70731069098821209 ) ) ;
#55908 = ORIENTED_EDGE ( 'NONE', *, *, #90598, .T. ) ;
#55909 = CARTESIAN_POINT ( 'NONE',  ( 0.000000000000000000, 16.00000000000000000, 0.000000000000000000 ) ) ;
#55910 = CARTESIAN_POINT ( 'NONE',  ( -43.78304604341450812, 434.3019790015192143, 13.50139152689284749 ) ) ;
#55911 = CARTESIAN_POINT ( 'NONE',  ( -0.3586102644459059907, 18.74914751208079267, 49.30103893526906234 ) ) ;
#55912 = CARTESIAN_POINT ( 'NONE',  ( 6.499999999999999112, 3.752776749732595452, -0.7999999999999977129 ) ) ;
#55913 = DIRECTION ( 'NONE',  ( -1.000000000000000000, -1.224606353822377258E-16, -0.000000000000000000 ) ) ;
#55914 = ORIENTED_EDGE ( 'NONE', *, *, #35335, .T. ) ;
#55915 = CARTESIAN_POINT ( 'NONE',  ( 19.34999999999999787, 1.533819458162526451E-15, 0.000000000000000000 ) ) ;
#55916 = ORIENTED_EDGE ( 'NONE', *, *, #62948, .T. ) ;
#55917 = CARTESIAN_POINT ( 'NONE',  ( 85.05745714698613824, -29.99999999998833644, 197.1808723821329465 ) ) ;
#55918 = DIRECTION ( 'NONE',  ( 0.000000000000000000, -1.000000000000000000, 0.000000000000000000 ) ) ;
#55919 = CARTESIAN_POINT ( 'NONE',  ( 6.570529166336707583, 41.93002594905234304, -59.71599377568048794 ) ) ;
#55920 = CARTESIAN_POINT ( 'NONE',  ( 106.4000000000000057, 5.616230220889761452E-16, -4.171999999999999709 ) ) ;
#55921 = CARTESIAN_POINT ( 'NONE',  ( 94.39176720276513777, -30.00000000000000000, 114.3184923802386521 ) ) ;
#55922 = CARTESIAN_POINT ( 'NONE',  ( 6.928203230275509661, 105.0000000000000000, 4.000000000000001776 ) ) ;
#55923 = EDGE_LOOP ( 'NONE', ( #10598, #71020, #19641, #48200 ) ) ;
#55924 = EDGE_CURVE ( 'NONE', #74451, #53134, #36997, .T. ) ;
#55925 = CIRCLE ( 'NONE', #97288, 5.000000000000002665 ) ;
#55926 = ORIENTED_EDGE ( 'NONE', *, *, #53296, .T. ) ;
#55927 = ORIENTED_EDGE ( 'NONE', *, *, #5995, .T. ) ;
#55928 = DIRECTION ( 'NONE',  ( 0.000000000000000000, -1.000000000000000000, 0.000000000000000000 ) ) ;
#55929 = CARTESIAN_POINT ( 'NONE',  ( 43.40846727559856078, 434.3587631105147011, 15.36753962297099996 ) ) ;
#55930 = CARTESIAN_POINT ( 'NONE',  ( -40.82244327980126286, 464.4949134188678954, 17.11270441416877475 ) ) ;
#55931 = EDGE_CURVE ( 'NONE', #57008, #26114, #64528, .T. ) ;
#55932 = EDGE_CURVE ( 'NONE', #41710, #101089, #57386, .T. ) ;
#55933 = ORIENTED_EDGE ( 'NONE', *, *, #32633, .F. ) ;
#55934 = CARTESIAN_POINT ( 'NONE',  ( 86.17777777777776294, 4.172000000000019249, 0.000000000000000000 ) ) ;
#55935 = ORIENTED_EDGE ( 'NONE', *, *, #5503, .T. ) ;
#55936 = DIRECTION ( 'NONE',  ( 0.000000000000000000, 0.000000000000000000, 1.000000000000000000 ) ) ;
#55937 = CARTESIAN_POINT ( 'NONE',  ( 78.83138536026389431, -38.67202492304706141, 190.5315074774399307 ) ) ;
#55938 = FACE_OUTER_BOUND ( 'NONE', #23234, .T. ) ;
#55939 = CARTESIAN_POINT ( 'NONE',  ( 84.48650984408737941, -45.28710619378168900, -5.682957750312108480 ) ) ;
#55940 = CARTESIAN_POINT ( 'NONE',  ( 74.07777777777778283, 6.915964383211875250E-15, 0.000000000000000000 ) ) ;
#55941 = CIRCLE ( 'NONE', #21583, 1.999999999999994227 ) ;
#55942 = CARTESIAN_POINT ( 'NONE',  ( 39.48390856328317966, 328.8151482415006512, 18.19106243202422846 ) ) ;
#55943 = PRESENTATION_LAYER_ASSIGNMENT (  '', '', ( #74965 ) ) ;
#55944 = LINE ( 'NONE', #98027, #103950 ) ;
#55945 =( GEOMETRIC_REPRESENTATION_CONTEXT ( 3 ) GLOBAL_UNCERTAINTY_ASSIGNED_CONTEXT ( ( #87144 ) ) GLOBAL_UNIT_ASSIGNED_CONTEXT ( ( #36460, #43448, #103275 ) ) REPRESENTATION_CONTEXT ( 'NONE', 'WORKASPACE' ) );
#55946 = EDGE_CURVE ( 'NONE', #106540, #91293, #35666, .T. ) ;
#55947 = CARTESIAN_POINT ( 'NONE',  ( 56.96666666666666856, 6.915964383211875250E-15, 0.000000000000000000 ) ) ;
#55948 = CIRCLE ( 'NONE', #64614, 5.000000000000001776 ) ;
#55949 = VECTOR ( 'NONE', #18060, 1000.000000000000000 ) ;
#55950 = PRESENTATION_STYLE_ASSIGNMENT (( #60905 ) ) ;
#55951 = CARTESIAN_POINT ( 'NONE',  ( 41.84005600619870791, 337.9971086773677484, 12.28340151619240572 ) ) ;
#55952 = ORIENTED_EDGE ( 'NONE', *, *, #91607, .F. ) ;
#55953 = FACE_OUTER_BOUND ( 'NONE', #55366, .T. ) ;
#55954 = ADVANCED_FACE ( 'NONE', ( #8811 ), #106436, .T. ) ;
#55955 = CARTESIAN_POINT ( 'NONE',  ( 0.000000000000000000, 0.000000000000000000, 4.000000000000000888 ) ) ;
#55956 = CARTESIAN_POINT ( 'NONE',  ( -25.85875814313400411, 37.16303024043016023, 8.999254728584531904 ) ) ;
#55957 = ORIENTED_EDGE ( 'NONE', *, *, #28672, .F. ) ;
#55958 = LINE ( 'NONE', #5325, #69938 ) ;
#55960 = CARTESIAN_POINT ( 'NONE',  ( -32.75974658096314585, 300.2740040294210644, 3.156099462989093940 ) ) ;
#55959 =( NAMED_UNIT ( * ) PLANE_ANGLE_UNIT ( ) SI_UNIT ( $, .RADIAN. ) );
#55961 = CARTESIAN_POINT ( 'NONE',  ( -12.49999999999998757, -3.165118404322636803, -76.70900766830885686 ) ) ;
#55962 = UNCERTAINTY_MEASURE_WITH_UNIT (LENGTH_MEASURE( 1.000000000000000082E-05 ), #19870, 'distance_accuracy_value', 'NONE');
#55963 = CARTESIAN_POINT ( 'NONE',  ( 30.00000000000000000, 500.0000000000002274, 0.000000000000000000 ) ) ;
#55964 = CARTESIAN_POINT ( 'NONE',  ( -8.000000000000001776, -14.65624999999999289, 3.313708498984758943 ) ) ;
#55965 = CARTESIAN_POINT ( 'NONE',  ( 18.00000000000000355, 12.99999999999999467, -7.500000000000000000 ) ) ;
#55966 = EDGE_CURVE ( 'NONE', #86773, #48676, #26683, .T. ) ;
#55967 = FILL_AREA_STYLE_COLOUR ( '', #88038 ) ;
#55968 = ORIENTED_EDGE ( 'NONE', *, *, #99117, .T. ) ;
#55969 = CARTESIAN_POINT ( 'NONE',  ( 83.59514486132030697, -60.99987548644057966, 191.7053679419932735 ) ) ;
#55970 = ADVANCED_FACE ( 'NONE', ( #48202 ), #104684, .F. ) ;
#55971 = CYLINDRICAL_SURFACE ( 'NONE', #13587, 4.000000000000003553 ) ;
#55972 = CARTESIAN_POINT ( 'NONE',  ( 3.964299495115819916, -1.290159053846382520, 103.9028936078240832 ) ) ;
#55973 = ORIENTED_EDGE ( 'NONE', *, *, #22873, .F. ) ;
#55974 = CARTESIAN_POINT ( 'NONE',  ( 95.81300639422605059, -57.67160901947544005, 39.88044211767749658 ) ) ;
#55975 = CARTESIAN_POINT ( 'NONE',  ( 35.50215413662375141, 437.6258544849006284, 4.714593920600838040 ) ) ;
#55976 = FACE_OUTER_BOUND ( 'NONE', #19118, .T. ) ;
#55977 = AXIS2_PLACEMENT_3D ( 'NONE', #18367, #16746, #27005 ) ;
#55978 = CARTESIAN_POINT ( 'NONE',  ( -69.67520780818028925, -37.99999999999996447, 100.0064218607845277 ) ) ;
#55979 = CARTESIAN_POINT ( 'NONE',  ( -5.219866590718559962, -5.000000000000000000, 8.922269033012391048 ) ) ;
#55980 = DIRECTION ( 'NONE',  ( 0.000000000000000000, -1.000000000000000000, 0.000000000000000000 ) ) ;
#55982 = CARTESIAN_POINT ( 'NONE',  ( -13.67323925869998646, 5.035284030722468884, 6.079275982674877454 ) ) ;
#55981 = CARTESIAN_POINT ( 'NONE',  ( 42.60801198157294323, 467.2314309137090049, 12.94843827108660150 ) ) ;
#55983 = VERTEX_POINT ( 'NONE', #102070 ) ;
#55984 = CARTESIAN_POINT ( 'NONE',  ( -12.50000000000000000, -3.000000000000000000, -11.21398294031087062 ) ) ;
#55985 = CARTESIAN_POINT ( 'NONE',  ( 10.47796581435272145, -5.000000000000000000, -91.06180813480403913 ) ) ;
#55986 = CARTESIAN_POINT ( 'NONE',  ( 9.151133496029800085, 15.07443463110313076, -4.034557488804713543 ) ) ;
#55987 = CARTESIAN_POINT ( 'NONE',  ( 5.363597346073513350, 41.33266196706048845, -58.39526881795627844 ) ) ;
#55988 = CARTESIAN_POINT ( 'NONE',  ( -81.98196232622828461, -37.99999999999996447, -13.86369433938586582 ) ) ;
#55989 = CIRCLE ( 'NONE', #44026, 4.000000000000000888 ) ;
#55990 = VERTEX_POINT ( 'NONE', #44925 ) ;
#55991 = LINE ( 'NONE', #87349, #91716 ) ;
#55992 = CARTESIAN_POINT ( 'NONE',  ( 23.58349330513380337, 4.898587196589405926E-16, -4.000000000000001776 ) ) ;
#55994 = CARTESIAN_POINT ( 'NONE',  ( -56.92527863508112063, -47.40887414813248313, -28.31673470188760788 ) ) ;
#55993 = CARTESIAN_POINT ( 'NONE',  ( 0.000000000000000000, -19.99999999999998934, 0.000000000000000000 ) ) ;
#55995 = EDGE_CURVE ( 'NONE', #83974, #57077, #67982, .T. ) ;
#55996 = ORIENTED_EDGE ( 'NONE', *, *, #90778, .F. ) ;
#55997 = ORIENTED_EDGE ( 'NONE', *, *, #39210, .F. ) ;
#55998 = AXIS2_PLACEMENT_3D ( 'NONE', #62363, #62888, #61294 ) ;
#55999 = ADVANCED_FACE ( 'NONE', ( #77276 ), #21519, .F. ) ;
#56000 = EDGE_CURVE ( 'NONE', #93546, #32972, #24971, .T. ) ;
#56001 = CARTESIAN_POINT ( 'NONE',  ( 11.51372298711423880, 43.27656282359909312, -14.44600693944211933 ) ) ;
#56002 = CARTESIAN_POINT ( 'NONE',  ( 36.36650669486618881, 1.474610560812782335E-15, 0.000000000000000000 ) ) ;
#56003 = VECTOR ( 'NONE', #81893, 1000.000000000000227 ) ;
#56004 = CARTESIAN_POINT ( 'NONE',  ( -90.41325670661385061, -60.00000000000002132, -18.10141139825902101 ) ) ;
#56005 = ORIENTED_EDGE ( 'NONE', *, *, #68111, .F. ) ;
#56006 = CYLINDRICAL_SURFACE ( 'NONE', #6689, 63.00000000000000000 ) ;
#56007 = AXIS2_PLACEMENT_3D ( 'NONE', #47714, #106480, #64974 ) ;
#56008 =( NAMED_UNIT ( * ) PLANE_ANGLE_UNIT ( ) SI_UNIT ( $, .RADIAN. ) );
#56009 = AXIS2_PLACEMENT_3D ( 'NONE', #45324, #44798, #95993 ) ;
#56010 = CARTESIAN_POINT ( 'NONE',  ( 97.15172723662661269, -52.81671128251268499, 195.3014279785832343 ) ) ;
#56011 = COLOUR_RGB ( '', 0.40784314, 0.44705882, 0.49803922) ;
#56012 = DIRECTION ( 'NONE',  ( 0.000000000000000000, 0.000000000000000000, 1.000000000000000000 ) ) ;
#56013 = EDGE_CURVE ( 'NONE', #102336, #84625, #16314, .T. ) ;
#56014 = CARTESIAN_POINT ( 'NONE',  ( -82.39702631368088248, -39.49694748076612427, 164.1908697851564796 ) ) ;
#56015 = VERTEX_POINT ( 'NONE', #69199 ) ;
#56016 = PRESENTATION_LAYER_ASSIGNMENT (  '', '', ( #62995 ) ) ;
#56017 = EDGE_CURVE ( 'NONE', #17242, #10104, #49761, .T. ) ;
#56018 = EDGE_CURVE ( 'NONE', #94625, #19102, #89705, .T. ) ;
#56019 = ORIENTED_EDGE ( 'NONE', *, *, #95544, .T. ) ;
#56020 = CIRCLE ( 'NONE', #6085, 4.000000000000000888 ) ;
#56021 = ORIENTED_EDGE ( 'NONE', *, *, #54077, .T. ) ;
#56022 = CARTESIAN_POINT ( 'NONE',  ( 9.235395886531431551E-16, -3.000000000000000000, -8.000000000000000000 ) ) ;
#56023 = CARTESIAN_POINT ( 'NONE',  ( -5.000000000000000000, -13.99860067247083073, 11.59399192991872596 ) ) ;
#56024 = SURFACE_SIDE_STYLE ('',( #48476 ) ) ;
#56025 = ORIENTED_EDGE ( 'NONE', *, *, #96434, .T. ) ;
#56026 = DIRECTION ( 'NONE',  ( 0.000000000000000000, 1.000000000000000000, 0.000000000000000000 ) ) ;
#56027 = DIRECTION ( 'NONE',  ( -1.000000000000000000, -1.224606353822377258E-16, -0.000000000000000000 ) ) ;
#56028 = CARTESIAN_POINT ( 'NONE',  ( -9.571198553003062770, 15.30040232763797547, -2.918503601031004813 ) ) ;
#56029 = CARTESIAN_POINT ( 'NONE',  ( -105.2191501062491881, -57.64508961356604999, 201.5420537206667291 ) ) ;
#56030 = CARTESIAN_POINT ( 'NONE',  ( 6.936184427528457874, 0.000000000000000000, -8.605212085995399107 ) ) ;
#56031 = CARTESIAN_POINT ( 'NONE',  ( -21.29975379448946171, 294.8969325209483259, -1.990407376643346327 ) ) ;
#56032 = CARTESIAN_POINT ( 'NONE',  ( -0.7841117270647198767, 25.97962594934760716, 38.51284013075863299 ) ) ;
#56033 = FACE_OUTER_BOUND ( 'NONE', #88903, .T. ) ;
#56034 = CARTESIAN_POINT ( 'NONE',  ( -65.68019474265784652, -30.00000000000001776, -31.25134080541240422 ) ) ;
#56035 = CARTESIAN_POINT ( 'NONE',  ( -34.60361718403136422, -60.00000000000001421, 49.20626982406709971 ) ) ;
#56036 = CARTESIAN_POINT ( 'NONE',  ( -52.62903541624970671, -32.57446218424134798, 52.90420147508846327 ) ) ;
#56037 = B_SPLINE_CURVE_WITH_KNOTS ( 'NONE', 3,
 ( #80710, #80182, #15451, #106586, #6289, #39226, #88819, #48870 ),
 .UNSPECIFIED., .F., .F.,
 ( 4, 2, 2, 4 ),
 ( 0.000000000000000000, 0.0002494395879357873573, 0.0004988791758715747145, 0.0009977583517431533322 ),
 .UNSPECIFIED. ) ;
#56038 = ORIENTED_EDGE ( 'NONE', *, *, #20361, .T. ) ;
#56039 = CARTESIAN_POINT ( 'NONE',  ( -96.24129786307111090, -45.25353125910449847, 194.1168147664394610 ) ) ;
#56040 = CARTESIAN_POINT ( 'NONE',  ( -13.50000000000000000, 7.794228634059933825, -13.00000000000000000 ) ) ;
#56041 = VERTEX_POINT ( 'NONE', #62694 ) ;
#56042 = CARTESIAN_POINT ( 'NONE',  ( 19.46222512963864304, 49.98514627502216712, 60.50669264090301880 ) ) ;
#56043 = CARTESIAN_POINT ( 'NONE',  ( 81.42364061245054074, -38.35622654735483650, -25.61884919812055372 ) ) ;
#56044 = CARTESIAN_POINT ( 'NONE',  ( 25.11650669486618881, 1.474610560812782335E-15, 0.000000000000000000 ) ) ;
#56045 = LINE ( 'NONE', #79289, #59462 ) ;
#56046 = CIRCLE ( 'NONE', #11322, 4.000000000000007105 ) ;
#56047 = DIRECTION ( 'NONE',  ( -0.9995674975569808218, -0.02876390015675800785, -0.006120120541885477189 ) ) ;
#56048 = CARTESIAN_POINT ( 'NONE',  ( 84.55162599420341962, -29.99999999999999645, 166.0629177430633092 ) ) ;
#56049 = DIRECTION ( 'NONE',  ( 0.000000000000000000, -1.000000000000000000, 0.000000000000000000 ) ) ;
#56050 = CARTESIAN_POINT ( 'NONE',  ( 35.80932576324499905, 491.2997492151453116, 12.22805875982020041 ) ) ;
#56051 = CARTESIAN_POINT ( 'NONE',  ( -1.249981344408581885, 34.67482971135811454, 28.34062085008046949 ) ) ;
#56052 = DIRECTION ( 'NONE',  ( -1.000000000000000000, -1.224606353822377258E-16, -0.000000000000000000 ) ) ;
#56053 = ORIENTED_EDGE ( 'NONE', *, *, #14830, .F. ) ;
#56054 = ORIENTED_EDGE ( 'NONE', *, *, #6401, .F. ) ;
#56055 = CARTESIAN_POINT ( 'NONE',  ( 49.01001383078526175, -39.51698039974216670, 49.15479020084767114 ) ) ;
#56056 = CARTESIAN_POINT ( 'NONE',  ( 0.000000000000000000, 0.000000000000000000, -1.581124522925831499 ) ) ;
#56057 = DIRECTION ( 'NONE',  ( 1.000000000000000000, 0.000000000000000000, 0.000000000000000000 ) ) ;
#56058 = EDGE_CURVE ( 'NONE', #55990, #58778, #71435, .T. ) ;
#56059 = CARTESIAN_POINT ( 'NONE',  ( -106.2167736919956837, -38.37611417361867439, 196.0685381891890700 ) ) ;
#56060 = ORIENTED_EDGE ( 'NONE', *, *, #58191, .F. ) ;
#56061 = CARTESIAN_POINT ( 'NONE',  ( 96.41480450689181225, -38.35574263741993661, 66.97822750028046812 ) ) ;
#56062 = CARTESIAN_POINT ( 'NONE',  ( 11.22447282797537227, 19.86299956823604163, -8.519236578064418808 ) ) ;
#56063 = CARTESIAN_POINT ( 'NONE',  ( -8.000000000000000000, 0.000000000000000000, -11.12471428571428689 ) ) ;
#56064 = CARTESIAN_POINT ( 'NONE',  ( 9.797174393178825657E-16, -14.49999999999999822, -8.000000000000000000 ) ) ;
#56065 = CARTESIAN_POINT ( 'NONE',  ( 99.21197506481942696, -60.15124926635865421, 110.4799484367256923 ) ) ;
#56066 = CARTESIAN_POINT ( 'NONE',  ( 23.21751746555303342, 27.38103382803677377, 33.20617127781017075 ) ) ;
#56067 = DIRECTION ( 'NONE',  ( 0.000000000000000000, -1.000000000000000000, 0.000000000000000000 ) ) ;
#56068 = DIRECTION ( 'NONE',  ( -0.000000000000000000, 1.000000000000000000, -0.000000000000000000 ) ) ;
#56069 = SURFACE_STYLE_FILL_AREA ( #88484 ) ;
#56070 = CARTESIAN_POINT ( 'NONE',  ( 101.7954163560313816, -60.00000000000000711, 201.2573263482775303 ) ) ;
#56071 = VERTEX_POINT ( 'NONE', #46496 ) ;
#56072 = CARTESIAN_POINT ( 'NONE',  ( 56.04098195827219797, -22.14826547861250461, 55.49373265869978411 ) ) ;
#56073 = CARTESIAN_POINT ( 'NONE',  ( -27.00275465088504134, 305.0213443944945197, -9.522733346438251090 ) ) ;
#56074 = CARTESIAN_POINT ( 'NONE',  ( -89.99999999999997158, -38.00000000001091394, 196.0238439516549818 ) ) ;
#56075 = VECTOR ( 'NONE', #44181, 1000.000000000000114 ) ;
#56076 = CARTESIAN_POINT ( 'NONE',  ( -7.744168461338430731, 26.53745938284842154, 2.019395720771554714 ) ) ;
#56077 = ORIENTED_EDGE ( 'NONE', *, *, #23603, .F. ) ;
#56079 = CARTESIAN_POINT ( 'NONE',  ( -9.864453787710772303, -50.40643955470380178, 25.34106120123098549 ) ) ;
#56078 = CARTESIAN_POINT ( 'NONE',  ( -106.3530780054166343, -38.37121618136543333, 195.8661688634274469 ) ) ;
#56080 = DIRECTION ( 'NONE',  ( -0.000000000000000000, -0.000000000000000000, -1.000000000000000000 ) ) ;
#56081 = CARTESIAN_POINT ( 'NONE',  ( 27.96090922204301421, 315.0246767492035360, 11.41898043927315243 ) ) ;
#56082 = DIRECTION ( 'NONE',  ( 0.000000000000000000, -1.000000000000000000, 0.000000000000000000 ) ) ;
#56083 = CARTESIAN_POINT ( 'NONE',  ( -3.313708498984765161, -33.96875000000000000, 7.999999999999998224 ) ) ;
#56084 = COLOUR_RGB ( '', 0.31764706, 0.68627451, 0.89019608) ;
#56085 = CARTESIAN_POINT ( 'NONE',  ( -18.91791044776116237, 44.85000000000000853, 62.18611311450883505 ) ) ;
#56086 = EDGE_CURVE ( 'NONE', #86709, #77600, #71514, .T. ) ;
#56087 = STYLED_ITEM ( 'NONE', ( #45707 ), #88291 ) ;
#56088 = CIRCLE ( 'NONE', #69925, 14.00000000000000178 ) ;
#56089 = DIRECTION ( 'NONE',  ( 0.000000000000000000, -1.000000000000000000, 0.000000000000000000 ) ) ;
#56090 = CIRCLE ( 'NONE', #81892, 5.000000000000011546 ) ;
#56091 = EDGE_LOOP ( 'NONE', ( #91241, #1057 ) ) ;
#56092 = CARTESIAN_POINT ( 'NONE',  ( 86.07226235559976146, -18.39178924599106324, 166.6779042990540063 ) ) ;
#56093 = EDGE_CURVE ( 'NONE', #6495, #35284, #7759, .T. ) ;
#56094 = CARTESIAN_POINT ( 'NONE',  ( 44.10119824970315960, 485.7576817097466915, 4.111374810962455939 ) ) ;
#56095 = CARTESIAN_POINT ( 'NONE',  ( 36.56751284714513872, 28.18319525971078576, 11.43687960009742177 ) ) ;
#56096 = ORIENTED_EDGE ( 'NONE', *, *, #24339, .T. ) ;
#56097 = CARTESIAN_POINT ( 'NONE',  ( 12.44963615882576491, -4.333246069852155991, -12.76855431082354997 ) ) ;
#56098 = VECTOR ( 'NONE', #73017, 1000.000000000000000 ) ;
#56099 = CARTESIAN_POINT ( 'NONE',  ( 7.731157688189080446, -4.999999999993458566, -17.87147387709585900 ) ) ;
#56100 = DIRECTION ( 'NONE',  ( 0.000000000000000000, -1.000000000000000000, 0.000000000000000000 ) ) ;
#56101 = CARTESIAN_POINT ( 'NONE',  ( 102.6464385083043283, 1.030564683017419500E-14, 0.000000000000000000 ) ) ;
#56102 = CARTESIAN_POINT ( 'NONE',  ( -42.46496487705343270, 41.57317828158753059, -52.12032522017845082 ) ) ;
#56103 = AXIS2_PLACEMENT_3D ( 'NONE', #48705, #49235, #63870 ) ;
#56104 = DIRECTION ( 'NONE',  ( -1.000000000000000000, -1.224606353822377258E-16, -0.000000000000000000 ) ) ;
#56105 = ORIENTED_EDGE ( 'NONE', *, *, #93899, .F. ) ;
#56106 =( LENGTH_UNIT ( ) NAMED_UNIT ( * ) SI_UNIT ( .MILLI., .METRE. ) );
#56107 = CARTESIAN_POINT ( 'NONE',  ( 38.69245764546075605, 25.17153636228211511, 12.75614855080256405 ) ) ;
#56108 = CARTESIAN_POINT ( 'NONE',  ( 0.000000000000000000, 0.000000000000000000, 0.000000000000000000 ) ) ;
#56110 = CARTESIAN_POINT ( 'NONE',  ( -11.94205703464897717, 10.81404306920174463, -9.773533727217355249 ) ) ;
#56109 = FACE_OUTER_BOUND ( 'NONE', #819, .T. ) ;
#56111 = PRODUCT_RELATED_PRODUCT_CATEGORY ( 'part', '', ( #12205 ) ) ;
#56112 = CARTESIAN_POINT ( 'NONE',  ( -7.188101187500002709, -16.81250000204838457, 2.977408999572648707 ) ) ;
#56113 = CARTESIAN_POINT ( 'NONE',  ( -29.07939586085774408, 18.85565742903569486, -39.75811902752995763 ) ) ;
#56114 = VERTEX_POINT ( 'NONE', #45451 ) ;
#56115 = DIRECTION ( 'NONE',  ( -0.5516836157922510031, 0.3133352674422950623, -0.7729593768389471098 ) ) ;
#56116 = CARTESIAN_POINT ( 'NONE',  ( 24.06092750555239590, 25.16990051853040811, 32.88256764606778404 ) ) ;
#56117 = PRESENTATION_LAYER_ASSIGNMENT (  '', '', ( #81927 ) ) ;
#56118 = CARTESIAN_POINT ( 'NONE',  ( -9.291918545757502201, 140.5484994665301599, 0.000000000000000000 ) ) ;
#56119 = CARTESIAN_POINT ( 'NONE',  ( -10.00000000000000355, 105.0000000000000000, 0.000000000000000000 ) ) ;
#56120 = CARTESIAN_POINT ( 'NONE',  ( -14.68864207889024520, 1.585199049508030367, 3.034365436914247205 ) ) ;
#56121 = ORIENTED_EDGE ( 'NONE', *, *, #33718, .T. ) ;
#56122 = ADVANCED_FACE ( 'NONE', ( #30333 ), #12518, .F. ) ;
#56123 = CARTESIAN_POINT ( 'NONE',  ( 56.22793774957824553, 4.000000000000014211, 0.000000000000000000 ) ) ;
#56124 = ORIENTED_EDGE ( 'NONE', *, *, #102924, .T. ) ;
#56125 = EDGE_CURVE ( 'NONE', #7878, #19325, #33516, .T. ) ;
#56126 = FILL_AREA_STYLE ('',( #23832 ) ) ;
#56127 = DIRECTION ( 'NONE',  ( -1.000000000000000000, 0.000000000000000000, 0.000000000000000000 ) ) ;
#56128 = CARTESIAN_POINT ( 'NONE',  ( -109.0665197127778754, -60.00000000000001421, 136.4503932063792320 ) ) ;
#56129 = DIRECTION ( 'NONE',  ( 0.2277538186084659411, 0.3726643368264558887, 0.8995829534661936577 ) ) ;
#56130 = CARTESIAN_POINT ( 'NONE',  ( -6.744191224192673140, 304.7396466505883268, -9.023845512521328160 ) ) ;
#56131 = FACE_OUTER_BOUND ( 'NONE', #63300, .T. ) ;
#56133 = CARTESIAN_POINT ( 'NONE',  ( 35.64643974835689022, 491.6938676210180006, 12.49042095397455832 ) ) ;
#56132 = CARTESIAN_POINT ( 'NONE',  ( -11.99999999999999467, -5.000000000000002665, -86.57079632497431021 ) ) ;
#56134 = CARTESIAN_POINT ( 'NONE',  ( -84.42293876102274908, -32.44484160355589353, 172.3670057701875749 ) ) ;
#56135 = AXIS2_PLACEMENT_3D ( 'NONE', #19359, #29045, #3660 ) ;
#56136 = ORIENTED_EDGE ( 'NONE', *, *, #104685, .T. ) ;
#56137 = FILL_AREA_STYLE_COLOUR ( '', #91800 ) ;
#56138 = ADVANCED_FACE ( 'NONE', ( #56693 ), #59332, .F. ) ;
#56139 = ORIENTED_EDGE ( 'NONE', *, *, #94290, .T. ) ;
#56140 =( BOUNDED_SURFACE ( )  B_SPLINE_SURFACE ( 3, 2, ( 
 ( #15630, #80895, #7006 ),
 ( #39926, #46936, #79835 ),
 ( #5433, #48523, #71736 ),
 ( #81414, #7525, #106221 ),
 ( #32383, #24297, #5941 ),
 ( #65255, #98145, #57146 ),
 ( #104110, #30254, #63683 ),
 ( #38868, #104645, #30797 ),
 ( #96571, #55543, #74917 ),
 ( #9125, #98666, #76934 ),
 ( #58219, #3045, #52650 ),
 ( #91144, #28422, #11656 ),
 ( #85034, #25358, #102273 ),
 ( #1001, #99195, #57670 ),
 ( #32911, #44586, #69390 ),
 ( #17254, #25913, #8602 ) ),
 .UNSPECIFIED., .F., .F., .T. ) 
 B_SPLINE_SURFACE_WITH_KNOTS ( ( 4, 2, 2, 2, 2, 2, 2, 4 ),
 ( 3, 3 ),
 ( 5.453536927602087303E-17, 0.0004174911443143812235, 0.0008349822886287079117, 0.001252473432943034546, 0.001669964577257361180, 0.002087455721571688030, 0.002504946865886014448, 0.003339929154514667715 ),
 ( 0.000000000000000000, 1.000000000000000000 ),
 .UNSPECIFIED. ) 
 GEOMETRIC_REPRESENTATION_ITEM ( )  RATIONAL_B_SPLINE_SURFACE ( (
 ( 1.000000000000000000, 0.9103180234519283598, 1.000000000000000000),
 ( 1.000000000000000000, 0.9132534515339265635, 1.000000000000000000),
 ( 1.000000000000000000, 0.9163167995291866541, 1.000000000000000000),
 ( 1.000000000000000000, 0.9224552667423359109, 1.000000000000000000),
 ( 1.000000000000000000, 0.9255672299892768740, 1.000000000000000000),
 ( 1.000000000000000000, 0.9311188777562252605, 1.000000000000000000),
 ( 1.000000000000000000, 0.9335889460075816881, 1.000000000000000000),
 ( 1.000000000000000000, 0.9372750707310617546, 1.000000000000000000),
 ( 1.000000000000000000, 0.9384199839903416551, 1.000000000000000000),
 ( 1.000000000000000000, 0.9386115400575140155, 1.000000000000000000),
 ( 1.000000000000000000, 0.9376241860046977683, 1.000000000000000000),
 ( 1.000000000000000000, 0.9330615520477972824, 1.000000000000000000),
 ( 1.000000000000000000, 0.9294866642001711199, 1.000000000000000000),
 ( 1.000000000000000000, 0.9147413655461451576, 1.000000000000000000),
 ( 1.000000000000000000, 0.9000454066029738298, 1.000000000000000000),
 ( 1.000000000000000000, 0.8805984182417286865, 1.000000000000000000) ) ) 
 REPRESENTATION_ITEM ( '' )  SURFACE ( )  );
#56141 = EDGE_CURVE ( 'NONE', #13350, #49340, #82028, .T. ) ;
#56142 = VECTOR ( 'NONE', #45796, 1000.000000000000000 ) ;
#56143 = DIRECTION ( 'NONE',  ( 0.000000000000000000, 0.000000000000000000, -1.000000000000000000 ) ) ;
#56144 = EDGE_CURVE ( 'NONE', #65357, #93970, #81820, .T. ) ;
#56145 = CARTESIAN_POINT ( 'NONE',  ( 30.00000000000000355, 461.9728594894706362, 12.10976292102180274 ) ) ;
#56146 = CARTESIAN_POINT ( 'NONE',  ( -11.20285577171231139, -4.999999999999999112, -78.29797948823949127 ) ) ;
#56147 = CARTESIAN_POINT ( 'NONE',  ( 32.80207110003819082, 464.7310103173837774, 6.970203097363561362 ) ) ;
#56148 = CARTESIAN_POINT ( 'NONE',  ( 110.8743008064580664, -59.99999999999998579, 132.3768192050824268 ) ) ;
#56149 = CARTESIAN_POINT ( 'NONE',  ( -97.22630358410161477, -59.99999999999998579, 47.92073696641181613 ) ) ;
#56150 = CARTESIAN_POINT ( 'NONE',  ( -61.96503433816666728, -39.48828635186461611, 77.49540155723640567 ) ) ;
#56151 = AXIS2_PLACEMENT_3D ( 'NONE', #52120, #105971, #7277 ) ;
#56152 = ORIENTED_EDGE ( 'NONE', *, *, #28311, .T. ) ;
#56153 = CARTESIAN_POINT ( 'NONE',  ( -43.52075891743682234, 484.7805561108189636, 4.063293749114582631 ) ) ;
#56154 = CARTESIAN_POINT ( 'NONE',  ( 95.39352241366582064, -60.00000000000974865, 32.59770702840283718 ) ) ;
#56155 = VECTOR ( 'NONE', #60772, 1000.000000000000000 ) ;
#56157 = ORIENTED_EDGE ( 'NONE', *, *, #98829, .T. ) ;
#56156 = CIRCLE ( 'NONE', #95794, 1.999999999999998224 ) ;
#56158 = CARTESIAN_POINT ( 'NONE',  ( 3.437958683066990667E-06, -25.54837915214530852, 28.14771315162659349 ) ) ;
#56160 = TOROIDAL_SURFACE ( 'NONE', #49251, 7.500000000000000888, 5.000000000000000000 ) ;
#56159 = CARTESIAN_POINT ( 'NONE',  ( -7.188101187500000044, -20.28125000204838813, -8.802885111219163269E-16 ) ) ;
#56161 = CARTESIAN_POINT ( 'NONE',  ( 32.94021323899732323, 485.0599191339522349, 5.361609822540970072 ) ) ;
#56162 = EDGE_LOOP ( 'NONE', ( #62020, #64878, #64663, #103145 ) ) ;
#56163 = DIRECTION ( 'NONE',  ( 0.000000000000000000, -1.000000000000000000, 0.000000000000000000 ) ) ;
#56164 = ORIENTED_EDGE ( 'NONE', *, *, #24690, .T. ) ;
#56165 = CARTESIAN_POINT ( 'NONE',  ( 13.50000000000000533, -7.794228634059977345, -1.205771365940065953 ) ) ;
#56166 = DIRECTION ( 'NONE',  ( -1.000000000000000000, -0.000000000000000000, -0.000000000000000000 ) ) ;
#56168 = AXIS2_PLACEMENT_3D ( 'NONE', #5000, #28247, #103688 ) ;
#56167 = CARTESIAN_POINT ( 'NONE',  ( -104.0851100789305690, -59.99999999999997158, 199.9324485923847021 ) ) ;
#56169 = CARTESIAN_POINT ( 'NONE',  ( -4.073826509764605142, -1.047876529904877785, 104.5376934966490268 ) ) ;
#56170 = CARTESIAN_POINT ( 'NONE',  ( 2.977408999572651815, -27.31250000204838457, 7.188101187500000933 ) ) ;
#56171 = CARTESIAN_POINT ( 'NONE',  ( 46.00000000000000000, 461.5923978621210608, 9.841791816131641113 ) ) ;
#56172 = AXIS2_PLACEMENT_3D ( 'NONE', #60951, #94383, #29154 ) ;
#56173 = CARTESIAN_POINT ( 'NONE',  ( -5.620533092652015839, 53.42269982616544866, -8.489555698183893995 ) ) ;
#56174 = CARTESIAN_POINT ( 'NONE',  ( 7.000000000000000000, 0.000000000000000000, -4.425378966781146950 ) ) ;
#56175 = CARTESIAN_POINT ( 'NONE',  ( 5.036189802309444907, 49.99999999999999289, -76.26213611588271135 ) ) ;
#56176 = CARTESIAN_POINT ( 'NONE',  ( 15.71253448772373673, -4.310224761972015983, 14.37944430768630255 ) ) ;
#56177 = CYLINDRICAL_SURFACE ( 'NONE', #15094, 8.000000000000000000 ) ;
#56178 = CARTESIAN_POINT ( 'NONE',  ( 98.03244328573691746, -59.99999999999997868, 196.4906452546746038 ) ) ;
#56179 = CARTESIAN_POINT ( 'NONE',  ( -33.35600173507818056, -42.96555714314101948, 35.15763485665254962 ) ) ;
#56180 = VERTEX_POINT ( 'NONE', #105786 ) ;
#56181 = CARTESIAN_POINT ( 'NONE',  ( -14.90155535903825701, 42.58002643001272958, -90.01374837838967835 ) ) ;
#56182 = AXIS2_PLACEMENT_3D ( 'NONE', #95518, #53974, #78787 ) ;
#56183 = CARTESIAN_POINT ( 'NONE',  ( 39.00479706145522840, -36.05733951926574576, 37.16496500682296755 ) ) ;
#56184 = CARTESIAN_POINT ( 'NONE',  ( -22.23822744035697241, -8.673617379884035472E-16, -2.910977163147234759 ) ) ;
#56185 = VERTEX_POINT ( 'NONE', #64801 ) ;
#56186 = FACE_OUTER_BOUND ( 'NONE', #4770, .T. ) ;
#56187 = ADVANCED_FACE ( 'NONE', ( #73403 ), #97686, .T. ) ;
#56188 = CARTESIAN_POINT ( 'NONE',  ( -67.70953212967587831, -38.33447372670084263, 124.2643868202984976 ) ) ;
#56189 = ORIENTED_EDGE ( 'NONE', *, *, #93477, .F. ) ;
#56191 = CARTESIAN_POINT ( 'NONE',  ( -31.02212611900126760, 360.5725590293961318, 22.12937154125974715 ) ) ;
#56190 = CARTESIAN_POINT ( 'NONE',  ( 6.144360409390458244, -5.000000000000002665, -15.35739152976048594 ) ) ;
#56192 = DIRECTION ( 'NONE',  ( 0.000000000000000000, -1.000000000000000000, 0.000000000000000000 ) ) ;
#56193 = DIRECTION ( 'NONE',  ( -1.000000000000000000, -1.224606353822377258E-16, -0.000000000000000000 ) ) ;
#56194 = PLANE ( 'NONE',  #7985 ) ;
#56195 = CARTESIAN_POINT ( 'NONE',  ( 55.00571552735602410, -1.232595164407830946E-29, 4.000000000000007105 ) ) ;
#56196 = CARTESIAN_POINT ( 'NONE',  ( -31.41956809189580468, 380.3364241731395055, 23.41894105902489542 ) ) ;
#56197 = CARTESIAN_POINT ( 'NONE',  ( -4.882603763050360257, -46.97189056336372914, 42.72181775637868384 ) ) ;
#56198 = CIRCLE ( 'NONE', #99240, 15.00000000000001421 ) ;
#56199 = CARTESIAN_POINT ( 'NONE',  ( 94.32674073916098223, -60.00000000000001421, 43.94342970808462923 ) ) ;
#56200 = CARTESIAN_POINT ( 'NONE',  ( -43.51067860848493751, 485.4417974898085504, 3.909400899866710688 ) ) ;
#56201 = AXIS2_PLACEMENT_3D ( 'NONE', #18553, #78348, #84329 ) ;
#56202 = CARTESIAN_POINT ( 'NONE',  ( 0.4042117618284652436, -3.141900367810030126, 6.500000000000000000 ) ) ;
#56203 = CARTESIAN_POINT ( 'NONE',  ( -34.64166250171400918, 490.4813561613901811, 11.60003975507708951 ) ) ;
#56204 = EDGE_CURVE ( 'NONE', #61302, #79890, #81487, .T. ) ;
#56205 = VERTEX_POINT ( 'NONE', #65335 ) ;
#56206 = CARTESIAN_POINT ( 'NONE',  ( -78.07839977982523294, -30.00000000000002132, 124.9873134342141867 ) ) ;
#56207 = ORIENTED_EDGE ( 'NONE', *, *, #45008, .F. ) ;
#56208 = CARTESIAN_POINT ( 'NONE',  ( 26.36650669486618881, -3.999999999999998224, 0.000000000000000000 ) ) ;
#56209 = CARTESIAN_POINT ( 'NONE',  ( -15.35975064870708984, 2.980508189496250182, 2.732879807911750447 ) ) ;
#56210 =( LENGTH_UNIT ( ) NAMED_UNIT ( * ) SI_UNIT ( .MILLI., .METRE. ) );
#56211 = PLANE ( 'NONE',  #88024 ) ;
#56212 = CARTESIAN_POINT ( 'NONE',  ( 9.699016383038316036, 26.82361828551655947, 2.444973590251030782 ) ) ;
#56213 = CARTESIAN_POINT ( 'NONE',  ( -2.977408999572650039, -28.06250000204838813, -7.188101187500001821 ) ) ;
#56214 = CARTESIAN_POINT ( 'NONE',  ( 0.000000000000000000, 0.000000000000000000, 5.000000000000002665 ) ) ;
#56215 = CARTESIAN_POINT ( 'NONE',  ( 7.013017687956457635, 40.92324830026397819, -70.84400559921924412 ) ) ;
#56216 = VERTEX_POINT ( 'NONE', #8153 ) ;
#56217 = APPLICATION_CONTEXT ( 'automotive_design' ) ;
#56219 = ORIENTED_EDGE ( 'NONE', *, *, #56141, .T. ) ;
#56218 = CARTESIAN_POINT ( 'NONE',  ( -7.251493771303348268, 41.03131504527001283, -58.65725810227473858 ) ) ;
#56220 = CARTESIAN_POINT ( 'NONE',  ( 81.58097494048502085, -36.02867041663544256, 152.4525182214984511 ) ) ;
#56221 = ADVANCED_FACE ( 'NONE', ( #74470 ), #33662, .T. ) ;
#56222 = CARTESIAN_POINT ( 'NONE',  ( -38.17830846319614579, 27.65673431820511752, -11.10453014817443318 ) ) ;
#56223 = VERTEX_POINT ( 'NONE', #41057 ) ;
#56224 = CARTESIAN_POINT ( 'NONE',  ( -12.50000000000000711, 30.94869521958284864, -48.87257972625063474 ) ) ;
#56225 = CARTESIAN_POINT ( 'NONE',  ( 7.801777176595948937, -88.58827985812634154, -1.786991866639921822 ) ) ;
#56226 = CARTESIAN_POINT ( 'NONE',  ( 2.977408999572652260, -13.43750000204838457, 7.188101187500000044 ) ) ;
#56227 = CARTESIAN_POINT ( 'NONE',  ( 7.801339272325195751, 26.41268528040299302, -1.788609912539669722 ) ) ;
#56228 = CARTESIAN_POINT ( 'NONE',  ( -30.75663703201544408, -57.68613454458090217, 45.71164565728040685 ) ) ;
#56229 = EDGE_CURVE ( 'NONE', #53023, #93010, #35373, .T. ) ;
#56230 = CARTESIAN_POINT ( 'NONE',  ( 9.047629367966660396, 302.6745984409856760, 9.899357940741596806 ) ) ;
#56231 = AXIS2_PLACEMENT_3D ( 'NONE', #1873, #76303, #33752 ) ;
#56232 = ADVANCED_BREP_SHAPE_REPRESENTATION ( '', ( #89707, #10728 ), #79579 ) ;
#56233 = ORIENTED_EDGE ( 'NONE', *, *, #17612, .T. ) ;
#56234 = EDGE_CURVE ( 'NONE', #101925, #93035, #65860, .T. ) ;
#56235 =( LENGTH_UNIT ( ) NAMED_UNIT ( * ) SI_UNIT ( .MILLI., .METRE. ) );
#56236 = AXIS2_PLACEMENT_3D ( 'NONE', #69331, #78464, #61237 ) ;
#56237 = CARTESIAN_POINT ( 'NONE',  ( 89.99999999999997158, -52.00000000000000000, 196.0238439516549818 ) ) ;
#56238 = CARTESIAN_POINT ( 'NONE',  ( 7.251694438969768619, 41.54830556103024719, -59.82648080958256287 ) ) ;
#56239 = CARTESIAN_POINT ( 'NONE',  ( 58.67238219402268840, 4.898587196589294500E-16, -4.000000000000007105 ) ) ;
#56240 = ORIENTED_EDGE ( 'NONE', *, *, #93282, .T. ) ;
#56241 = CARTESIAN_POINT ( 'NONE',  ( 7.999999999999998224, -12.78125000409676915, 3.313708498984766493 ) ) ;
#56242 = AXIS2_PLACEMENT_3D ( 'NONE', #90, #66458, #99334 ) ;
#56243 = CARTESIAN_POINT ( 'NONE',  ( -27.41612642967203328, -20.44246825615584839, 31.78064786534578445 ) ) ;
#56244 = COLOUR_RGB ( '', 0.72549020, 0.75294118, 0.79215686) ;
#56245 = CIRCLE ( 'NONE', #37376, 4.000000000000001776 ) ;
#56246 = AXIS2_PLACEMENT_3D ( 'NONE', #74480, #555, #66396 ) ;
#56247 = DIRECTION ( 'NONE',  ( 0.000000000000000000, 0.000000000000000000, 1.000000000000000000 ) ) ;
#56248 = CARTESIAN_POINT ( 'NONE',  ( -5.656854249492379694, -16.43749999999999289, -5.656854249492380582 ) ) ;
#56249 = CARTESIAN_POINT ( 'NONE',  ( 40.50010235193833097, 437.8098891827066268, 21.96267907499429128 ) ) ;
#56251 = EDGE_CURVE ( 'NONE', #2886, #38464, #41586, .T. ) ;
#56250 = APPLICATION_PROTOCOL_DEFINITION ( 'draft international standard', 'automotive_design', 1998, #72768 ) ;
#56252 = CARTESIAN_POINT ( 'NONE',  ( 0.000000000000000000, 0.000000000000000000, -1.161000000000000032 ) ) ;
#56253 = ORIENTED_EDGE ( 'NONE', *, *, #83418, .T. ) ;
#56255 = VECTOR ( 'NONE', #60205, 1000.000000000000114 ) ;
#56254 = CARTESIAN_POINT ( 'NONE',  ( -4.644779468754994589, -47.71105737603588182, 40.40507978762116892 ) ) ;
#56256 = CARTESIAN_POINT ( 'NONE',  ( 1.224646799147354440E-15, 15.00000000000000000, 9.999999999999998224 ) ) ;
#56257 = LINE ( 'NONE', #74578, #94589 ) ;
#56258 = CARTESIAN_POINT ( 'NONE',  ( 67.75539237747796051, -38.10441934046211543, -31.96820234319118370 ) ) ;
#56259 = DIRECTION ( 'NONE',  ( -1.000000000000000000, -1.224606353822377258E-16, -0.000000000000000000 ) ) ;
#56260 = CARTESIAN_POINT ( 'NONE',  ( 4.226620391573794039E-15, 29.56666008184760130, 34.51297463494397988 ) ) ;
#56261 = ORIENTED_EDGE ( 'NONE', *, *, #71720, .F. ) ;
#56262 = CARTESIAN_POINT ( 'NONE',  ( 21.09715123528542691, 1.340359594676612611E-15, 0.000000000000000000 ) ) ;
#56263 = CARTESIAN_POINT ( 'NONE',  ( 90.90101844823369959, -57.61245536370559961, 204.1559653898591193 ) ) ;
#56264 = CARTESIAN_POINT ( 'NONE',  ( 36.94903695760955742, 463.9900885034069802, 19.60515700096699021 ) ) ;
#56265 = CARTESIAN_POINT ( 'NONE',  ( -16.11139379967456620, 21.68073351268998294, -1.735103873195799284 ) ) ;
#56266 = CARTESIAN_POINT ( 'NONE',  ( 5.957442974983132800, 40.83906611472426817, 64.99999999999700151 ) ) ;
#56267 = CARTESIAN_POINT ( 'NONE',  ( -73.05954267193276053, -60.00000000000000000, 163.0034808650574405 ) ) ;
#56268 = CARTESIAN_POINT ( 'NONE',  ( -44.66387834505498944, 341.6072687625629101, 1.189588019127773677 ) ) ;
#56269 = FILL_AREA_STYLE_COLOUR ( '', #83846 ) ;
#56270 = CARTESIAN_POINT ( 'NONE',  ( -50.94745919686192082, 50.00000000000000000, -37.05882352941185331 ) ) ;
#56271 = AXIS2_PLACEMENT_3D ( 'NONE', #42798, #24529, #8830 ) ;
#56272 = CARTESIAN_POINT ( 'NONE',  ( -83.92159281446114960, -57.41240253432310681, 190.5303650487262814 ) ) ;
#56273 = ORIENTED_EDGE ( 'NONE', *, *, #53118, .T. ) ;
#56274 = CARTESIAN_POINT ( 'NONE',  ( 20.37278541768182549, 303.8378246129573768, -10.00297115033341910 ) ) ;
#56275 =( GEOMETRIC_REPRESENTATION_CONTEXT ( 3 ) GLOBAL_UNCERTAINTY_ASSIGNED_CONTEXT ( ( #21873 ) ) GLOBAL_UNIT_ASSIGNED_CONTEXT ( ( #52105, #43497, #77458 ) ) REPRESENTATION_CONTEXT ( 'NONE', 'WORKASPACE' ) );
#56276 = ADVANCED_FACE ( 'NONE', ( #50206 ), #27041, .F. ) ;
#56277 = ORIENTED_EDGE ( 'NONE', *, *, #14296, .T. ) ;
#56278 = CARTESIAN_POINT ( 'NONE',  ( -7.551437640244098581, -13.00872462522910133, -2.648272645923381408 ) ) ;
#56279 = EDGE_CURVE ( 'NONE', #23322, #49860, #48412, .T. ) ;
#56280 = CARTESIAN_POINT ( 'NONE',  ( -47.33333333333331439, 59.99999999999999289, 23.66666666666664653 ) ) ;
#56281 = CARTESIAN_POINT ( 'NONE',  ( 40.97069641804722551, 488.3783578779278969, 10.59734101651493532 ) ) ;
#56282 = DIRECTION ( 'NONE',  ( -1.000000000000000000, -1.224606353822377258E-16, -0.000000000000000000 ) ) ;
#56283 = CARTESIAN_POINT ( 'NONE',  ( 42.80674739067560353, 434.8200538645568827, 17.89665983759098467 ) ) ;
#56284 = EDGE_LOOP ( 'NONE', ( #11613, #39847, #82985, #53076 ) ) ;
#56285 = CARTESIAN_POINT ( 'NONE',  ( -3.040541989225158837, -0.8315988256275635981, 104.0108293352680988 ) ) ;
#56286 = EDGE_CURVE ( 'NONE', #87281, #75707, #16333, .T. ) ;
#56287 = CARTESIAN_POINT ( 'NONE',  ( 13.55593332801579010, 24.70634882861434178, -1.273199631155955025 ) ) ;
#56288 = CARTESIAN_POINT ( 'NONE',  ( 19.43146043915153953, -2.602085213965209853E-15, -11.19959342722011364 ) ) ;
#56289 = CARTESIAN_POINT ( 'NONE',  ( 0.4033376246892507178, 7.198601258566903027, -0.5316568767328684331 ) ) ;
#56290 = CARTESIAN_POINT ( 'NONE',  ( 84.89432107329884047, -60.00000000000002132, -27.59204247542200505 ) ) ;
#56291 = CARTESIAN_POINT ( 'NONE',  ( -78.18481269439429582, -39.49763340085283403, 135.4004602990579258 ) ) ;
#56292 = VERTEX_POINT ( 'NONE', #76071 ) ;
#56293 = CARTESIAN_POINT ( 'NONE',  ( 44.75958163560274272, -30.00000000000001776, 54.38364795613178870 ) ) ;
#56294 = CARTESIAN_POINT ( 'NONE',  ( 105.0394626471009758, -57.64423819974435759, 201.6665972083923748 ) ) ;
#56295 = DIRECTION ( 'NONE',  ( -0.000000000000000000, -1.000000000000000000, -0.000000000000000000 ) ) ;
#56296 =( GEOMETRIC_REPRESENTATION_CONTEXT ( 3 ) GLOBAL_UNCERTAINTY_ASSIGNED_CONTEXT ( ( #87933 ) ) GLOBAL_UNIT_ASSIGNED_CONTEXT ( ( #29028, #61892, #76981 ) ) REPRESENTATION_CONTEXT ( 'NONE', 'WORKASPACE' ) );
#56297 = CARTESIAN_POINT ( 'NONE',  ( 33.35692847815791851, 315.0479610517062952, -7.083729467381872702 ) ) ;
#56298 = DIRECTION ( 'NONE',  ( 1.000000000000000000, 0.000000000000000000, 0.000000000000000000 ) ) ;
#56299 = ORIENTED_EDGE ( 'NONE', *, *, #73735, .T. ) ;
#56300 = CONICAL_SURFACE ( 'NONE', #89052, 4.000000000000001776, 0.9599310885968774798 ) ;
#56301 = DIRECTION ( 'NONE',  ( -0.4165977904505313578, -0.000000000000000000, -0.9090909090909090606 ) ) ;
#56302 = DIRECTION ( 'NONE',  ( 0.000000000000000000, 0.000000000000000000, 1.000000000000000000 ) ) ;
#56303 = CARTESIAN_POINT ( 'NONE',  ( -16.58679117417358739, 36.41790041698920533, 24.30698433968611383 ) ) ;
#56304 = CARTESIAN_POINT ( 'NONE',  ( -5.082755093536326818, -16.71875000204838813, 5.082755093536325042 ) ) ;
#56305 = CARTESIAN_POINT ( 'NONE',  ( 0.000000000000000000, 0.000000000000000000, -0.4455245229258316120 ) ) ;
#56306 =( NAMED_UNIT ( * ) PLANE_ANGLE_UNIT ( ) SI_UNIT ( $, .RADIAN. ) );
#56307 = CARTESIAN_POINT ( 'NONE',  ( 1.098919214070069206, 34.84343022423479397, 27.88335111672935795 ) ) ;
#56308 = DIRECTION ( 'NONE',  ( -1.000000000000000000, -1.224606353822377258E-16, -0.000000000000000000 ) ) ;
#56309 =( NAMED_UNIT ( * ) PLANE_ANGLE_UNIT ( ) SI_UNIT ( $, .RADIAN. ) );
#56310 = ORIENTED_EDGE ( 'NONE', *, *, #25714, .T. ) ;
#56311 = CARTESIAN_POINT ( 'NONE',  ( -9.948401965501753538E-16, 0.6351314446025491112, 6.499999999999998224 ) ) ;
#56312 = AXIS2_PLACEMENT_3D ( 'NONE', #74855, #81351, #939 ) ;
#56313 = AXIS2_PLACEMENT_3D ( 'NONE', #106302, #97159, #30880 ) ;
#56315 = CARTESIAN_POINT ( 'NONE',  ( 29.33244438116370389, -42.95779854847726398, 33.51356301004039295 ) ) ;
#56314 = CYLINDRICAL_SURFACE ( 'NONE', #44051, 1.250000000000001110 ) ;
#56316 = CARTESIAN_POINT ( 'NONE',  ( -5.290067270634260410, 52.08006895350597176, -6.031152949369843697 ) ) ;
#56318 = ORIENTED_EDGE ( 'NONE', *, *, #65516, .T. ) ;
#56317 =( BOUNDED_SURFACE ( )  B_SPLINE_SURFACE ( 3, 2, ( 
 ( #7300, #773, #89837 ),
 ( #79216, #17018, #15938 ),
 ( #49893, #90360, #16472 ),
 ( #32689, #8373, #13404 ) ),
 .UNSPECIFIED., .F., .F., .F. ) 
 B_SPLINE_SURFACE_WITH_KNOTS ( ( 4, 4 ),
 ( 3, 3 ),
 ( 1.634976876108140686E-16, 0.002404295360965568069 ),
 ( 0.000000000000000000, 1.000000000000000000 ),
 .UNSPECIFIED. ) 
 GEOMETRIC_REPRESENTATION_ITEM ( )  RATIONAL_B_SPLINE_SURFACE ( (
 ( 1.000000000000000000, 0.7927020107002132887, 1.000000000000000000),
 ( 1.000000000000000000, 0.8018372346785949123, 1.000000000000000000),
 ( 1.000000000000000000, 0.8104306387029213132, 1.000000000000000000),
 ( 1.000000000000000000, 0.8162384603568832997, 1.000000000000000000) ) ) 
 REPRESENTATION_ITEM ( '' )  SURFACE ( )  );
#56319 = EDGE_CURVE ( 'NONE', #101726, #75387, #31829, .T. ) ;
#56320 = ORIENTED_EDGE ( 'NONE', *, *, #44240, .T. ) ;
#56321 = PRODUCT_DEFINITION_SHAPE ( 'NONE', 'NONE',  #106807 ) ;
#56322 = AXIS2_PLACEMENT_3D ( 'NONE', #40076, #56774, #57831 ) ;
#56324 = CARTESIAN_POINT ( 'NONE',  ( 1.248999938734115744, 51.75291198392519476, 8.833461820030818146 ) ) ;
#56323 = CARTESIAN_POINT ( 'NONE',  ( 28.58349330513380337, -7.703719777548943412E-31, 4.000000000000001776 ) ) ;
#56325 = AXIS2_PLACEMENT_3D ( 'NONE', #88924, #98067, #49513 ) ;
#56326 = CARTESIAN_POINT ( 'NONE',  ( -10.00000000000000355, 15.00000000000000000, -10.00000000000000000 ) ) ;
#56327 = CARTESIAN_POINT ( 'NONE',  ( -43.64002961914418677, 465.1123652286068477, 8.841020312859518171 ) ) ;
#56328 = CIRCLE ( 'NONE', #54552, 5.000000000000000888 ) ;
#56329 = CARTESIAN_POINT ( 'NONE',  ( 4.699999999999999289, 3.752776749732569694, 6.499999999999997335 ) ) ;
#56330 =( BOUNDED_SURFACE ( )  B_SPLINE_SURFACE ( 3, 2, ( 
 ( #28561, #36662, #77076 ),
 ( #86258, #19428, #101879 ),
 ( #59853, #69005, #68468 ),
 ( #19956, #61445, #28040 ) ),
 .UNSPECIFIED., .F., .F., .F. ) 
 B_SPLINE_SURFACE_WITH_KNOTS ( ( 4, 4 ),
 ( 3, 3 ),
 ( -5.399326818977812081E-17, 0.0009998946722929585862 ),
 ( 0.000000000000000000, 1.000000000000000000 ),
 .UNSPECIFIED. ) 
 GEOMETRIC_REPRESENTATION_ITEM ( )  RATIONAL_B_SPLINE_SURFACE ( (
 ( 1.000000000000000000, 0.9103180234519401282, 1.000000000000000000),
 ( 1.000000000000000000, 0.9095686419922741628, 1.000000000000000000),
 ( 1.000000000000000000, 0.9074000141362769112, 1.000000000000000000),
 ( 1.000000000000000000, 0.9039444415360021745, 1.000000000000000000) ) ) 
 REPRESENTATION_ITEM ( '' )  SURFACE ( )  );
#56331 = FILL_AREA_STYLE ('',( #45628 ) ) ;
#56332 = CARTESIAN_POINT ( 'NONE',  ( 6.162888688655347558, -7.505553499465142053, -3.129864801432410934E-16 ) ) ;
#56333 = VERTEX_POINT ( 'NONE', #100348 ) ;
#56334 = ADVANCED_FACE ( 'NONE', ( #1091 ), #16391, .T. ) ;
#56335 = CARTESIAN_POINT ( 'NONE',  ( 16.31486644108454342, -60.00000000000000711, -42.08170890485629201 ) ) ;
#56336 = CARTESIAN_POINT ( 'NONE',  ( 86.10514064236191700, -29.99999999999991473, 179.3049154362485353 ) ) ;
#56337 = CARTESIAN_POINT ( 'NONE',  ( 7.500000000000000888, 0.000000000000000000, 1.734723475976807094E-15 ) ) ;
#56338 = CARTESIAN_POINT ( 'NONE',  ( -1.591643166418952315, -5.000000000000000000, -73.00000000000002842 ) ) ;
#56339 = CARTESIAN_POINT ( 'NONE',  ( 47.55643143940710615, 10.90089820249353636, -16.76894861493112643 ) ) ;
#56340 = EDGE_CURVE ( 'NONE', #72737, #87634, #34065, .T. ) ;
#56341 = EDGE_LOOP ( 'NONE', ( #12629, #3667 ) ) ;
#56342 = VERTEX_POINT ( 'NONE', #51796 ) ;
#56343 = VERTEX_POINT ( 'NONE', #84708 ) ;
#56344 = CARTESIAN_POINT ( 'NONE',  ( 7.007095409419855762E-15, 45.00000000000000711, -57.21727615095610275 ) ) ;
#56345 = CARTESIAN_POINT ( 'NONE',  ( 31.48004117150884085, 41.29391029462509266, -67.22209853552702441 ) ) ;
#56346 = DIRECTION ( 'NONE',  ( 0.000000000000000000, 1.000000000000000000, -0.000000000000000000 ) ) ;
#56347 = CARTESIAN_POINT ( 'NONE',  ( 25.67074776827756111, 305.1949030138181911, 10.46162487402293628 ) ) ;
#56348 = CARTESIAN_POINT ( 'NONE',  ( -37.12084974767950740, 348.0368284732711572, 0.6131544078700962297 ) ) ;
#56349 = CARTESIAN_POINT ( 'NONE',  ( -4.744147290358121438, -64.75533526552750629, 13.06247057915002863 ) ) ;
#56350 = CARTESIAN_POINT ( 'NONE',  ( -46.00000000000000000, 487.9611973796579605, 0.4748239133093615782 ) ) ;
#56351 = CARTESIAN_POINT ( 'NONE',  ( 12.21253585067004543, 0.000000000000000000, 5.000000000000002665 ) ) ;
#56352 = ORIENTED_EDGE ( 'NONE', *, *, #91917, .F. ) ;
#56353 = CARTESIAN_POINT ( 'NONE',  ( -9.076500669139843325, 43.77048081941054392, 14.51057422361543559 ) ) ;
#56354 = ORIENTED_EDGE ( 'NONE', *, *, #41896, .T. ) ;
#56355 = DIRECTION ( 'NONE',  ( 0.000000000000000000, 0.000000000000000000, 1.000000000000000000 ) ) ;
#56356 = CARTESIAN_POINT ( 'NONE',  ( 0.000000000000000000, 273.9999999999999432, -7.999999999999983125 ) ) ;
#56357 = CARTESIAN_POINT ( 'NONE',  ( -40.72262571688549571, 485.0559992917259819, -4.084589505543824828 ) ) ;
#56358 =( GEOMETRIC_REPRESENTATION_CONTEXT ( 3 ) GLOBAL_UNCERTAINTY_ASSIGNED_CONTEXT ( ( #20331 ) ) GLOBAL_UNIT_ASSIGNED_CONTEXT ( ( #54050, #37405, #62203 ) ) REPRESENTATION_CONTEXT ( 'NONE', 'WORKASPACE' ) );
#56359 = CARTESIAN_POINT ( 'NONE',  ( -46.13314991754092631, -59.99999999999993605, 50.82605641278608033 ) ) ;
#56360 = CARTESIAN_POINT ( 'NONE',  ( 69.97227875550414922, -53.38154203728925751, 110.0492415815727014 ) ) ;
#56361 = ORIENTED_EDGE ( 'NONE', *, *, #90603, .T. ) ;
#56362 = CARTESIAN_POINT ( 'NONE',  ( 40.80994823946819139, 464.4919611264104446, 17.10586550060336819 ) ) ;
#56363 = CARTESIAN_POINT ( 'NONE',  ( 23.73746414932995208, -5.000000000000000000, 6.123233995736768255E-16 ) ) ;
#56364 = CARTESIAN_POINT ( 'NONE',  ( 6.683837171061806082, -3.955946848495971668, -6.851900933636991375 ) ) ;
#56365 = EDGE_CURVE ( 'NONE', #13321, #34748, #43963, .T. ) ;
#56366 = ORIENTED_EDGE ( 'NONE', *, *, #62756, .T. ) ;
#56367 = CARTESIAN_POINT ( 'NONE',  ( 47.50596275964315396, 17.89684634806513230, 14.46697959672304101 ) ) ;
#56368 = EDGE_CURVE ( 'NONE', #85320, #41603, #104239, .T. ) ;
#56369 = CIRCLE ( 'NONE', #63347, 0.9999999999999993339 ) ;
#56370 = CARTESIAN_POINT ( 'NONE',  ( 6.542037336788293800, 51.42598268746419876, -7.323096805894091510 ) ) ;
#56371 = B_SPLINE_CURVE_WITH_KNOTS ( 'NONE', 3,
 ( #42347, #57993, #34295, #48825, #40751, #82269, #25684, #25134, #67169, #73638, #90913, #8911 ),
 .UNSPECIFIED., .F., .F.,
 ( 4, 2, 2, 2, 2, 4 ),
 ( 0.002780326429443416222, 0.01490779258427995906, 0.02703525873911650362, 0.03916272489395304646, 0.04522645797137132828, 0.05129019104878961011 ),
 .UNSPECIFIED. ) ;
#56372 = CARTESIAN_POINT ( 'NONE',  ( -3.313708498984760720, -30.21875000409677980, -8.000000000000000000 ) ) ;
#56373 = EDGE_CURVE ( 'NONE', #90846, #98221, #20211, .T. ) ;
#56374 = CARTESIAN_POINT ( 'NONE',  ( 0.000000000000000000, -4.999999999999998224, 8.000000000000000000 ) ) ;
#56375 = CARTESIAN_POINT ( 'NONE',  ( 9.918325909156591180, 246.2076476829255967, 1.298699613733157232 ) ) ;
#56376 = CARTESIAN_POINT ( 'NONE',  ( -43.54152132068637115, 464.9591243096638777, 12.86066449444578907 ) ) ;
#56377 = CIRCLE ( 'NONE', #9888, 59.50000000000000000 ) ;
#56378 = CARTESIAN_POINT ( 'NONE',  ( -9.999733828778108347, 7.500380388546896704, 5.000000000000000888 ) ) ;
#56379 = CARTESIAN_POINT ( 'NONE',  ( 13.50000000000000355, 1.319989657865598298, -0.02800283339255059054 ) ) ;
#56380 =( LENGTH_UNIT ( ) NAMED_UNIT ( * ) SI_UNIT ( .MILLI., .METRE. ) );
#56381 = CARTESIAN_POINT ( 'NONE',  ( 11.59897338065259653, 303.6009977575001244, 9.883690276519013551 ) ) ;
#56382 = ORIENTED_EDGE ( 'NONE', *, *, #104401, .F. ) ;
#56383 = CARTESIAN_POINT ( 'NONE',  ( 91.37578371391791165, 1.016364837396684119E-14, 0.000000000000000000 ) ) ;
#56384 = CARTESIAN_POINT ( 'NONE',  ( 37.33349330513379982, 1.593028355512270962E-15, 0.000000000000000000 ) ) ;
#56385 = CARTESIAN_POINT ( 'NONE',  ( 8.529325899348924267, -60.00000000000000000, 39.63650018205241565 ) ) ;
#56386 = CARTESIAN_POINT ( 'NONE',  ( -97.57213534682868783, -30.00000000000000711, 190.8491232417298988 ) ) ;
#56387 = CONICAL_SURFACE ( 'NONE', #65032, 3.309500000000001663, 0.9599310885968770357 ) ;
#56388 = CARTESIAN_POINT ( 'NONE',  ( -41.46910480218704009, 484.7338956289818270, -3.418960549715579500 ) ) ;
#56389 = CIRCLE ( 'NONE', #25513, 5.000000000000000000 ) ;
#56390 = CARTESIAN_POINT ( 'NONE',  ( 40.74024583315892301, -57.69051585465551568, 56.90653008474016161 ) ) ;
#56391 = CARTESIAN_POINT ( 'NONE',  ( 89.99999999999997158, -38.00000000001091394, 188.5238439516623146 ) ) ;
#56392 = CARTESIAN_POINT ( 'NONE',  ( 19.25210312709571880, -25.56399626811505854, -38.49344732436618699 ) ) ;
#56393 = CARTESIAN_POINT ( 'NONE',  ( -9.999999999999998224, 15.00000000000000000, 1.734723475976807489E-15 ) ) ;
#56394 = DIRECTION ( 'NONE',  ( 0.000000000000000000, 1.000000000000000000, 0.000000000000000000 ) ) ;
#56395 = AXIS2_PLACEMENT_3D ( 'NONE', #17809, #50661, #43140 ) ;
#56396 = CARTESIAN_POINT ( 'NONE',  ( -19.98591378148901399, -59.99999999999998579, 40.21844962042136729 ) ) ;
#56397 = CIRCLE ( 'NONE', #21964, 4.000000000000001776 ) ;
#56398 = AXIS2_PLACEMENT_3D ( 'NONE', #105131, #87366, #56012 ) ;
#56399 = AXIS2_PLACEMENT_3D ( 'NONE', #35277, #75701, #100506 ) ;
#56400 = CARTESIAN_POINT ( 'NONE',  ( 12.39290798559944839, 18.01462319283537994, 8.658749452403840863 ) ) ;
#56401 = B_SPLINE_CURVE_WITH_KNOTS ( 'NONE', 3,
 ( #31020, #39624, #32066, #72496, #64427, #23452, #83763, #91355, #17469, #86332, #4324, #1229, #84311, #26642, #91870, #26128, #45327, #17996, #43322, #50857 ),
 .UNSPECIFIED., .F., .F.,
 ( 4, 2, 2, 2, 2, 2, 2, 2, 2, 4 ),
 ( 0.0009445086018700379026, 0.001449274952876525692, 0.001954041303883013482, 0.002458807654889501055, 0.002963574005895989062, 0.003468340356902477068, 0.003973106707908964641, 0.004225489883412212114, 0.004477873058915459586, 0.004982639409921949328 ),
 .UNSPECIFIED. ) ;
#56402 = CARTESIAN_POINT ( 'NONE',  ( -86.98677026252562428, -24.32171485741916683, 186.4285793591348579 ) ) ;
#56403 = VERTEX_POINT ( 'NONE', #10794 ) ;
#56404 = CARTESIAN_POINT ( 'NONE',  ( 17.50000000000308020, 49.96115704435360527, 61.85088014401689094 ) ) ;
#56405 = CARTESIAN_POINT ( 'NONE',  ( 3.313708498984722972, -12.21874999999999112, -8.000000000000040856 ) ) ;
#56406 = CARTESIAN_POINT ( 'NONE',  ( -12.17599302799778549, -22.06821926268190381, 27.61575194255241428 ) ) ;
#56407 = CARTESIAN_POINT ( 'NONE',  ( 0.000000000000000000, 4.898587196589412829E-16, -4.000000000000000000 ) ) ;
#56408 = CIRCLE ( 'NONE', #23746, 5.000000000000001776 ) ;
#56409 = CARTESIAN_POINT ( 'NONE',  ( 4.205882352941182845, -5.000000000000000000, -72.69916451482998809 ) ) ;
#56410 = EDGE_CURVE ( 'NONE', #55161, #58381, #43712, .T. ) ;
#56411 = ORIENTED_EDGE ( 'NONE', *, *, #106755, .T. ) ;
#56412 = DIRECTION ( 'NONE',  ( 0.5735764363510557073, -0.8191520442889850262, 1.003171929053516612E-16 ) ) ;
#56413 = B_SPLINE_CURVE_WITH_KNOTS ( 'NONE', 3,
 ( #88449, #438, #73837, #32880, #14521, #97051, #33409, #90025, #65755, #47433, #105153, #66278, #47955, #72251, #80862, #81915, #16131, #41473 ),
 .UNSPECIFIED., .F., .F.,
 ( 4, 2, 2, 2, 2, 2, 2, 2, 4 ),
 ( 1.303092495393577094E-20, 0.0008000025724062559277, 0.001600005144812511855, 0.002400007717218767891, 0.003200010289625023711, 0.004000012862031279530, 0.004800015434437535783, 0.005600018006843791168, 0.006400020579250047421 ),
 .UNSPECIFIED. ) ;
#56414 = VECTOR ( 'NONE', #45947, 1000.000000000000114 ) ;
#56415 = CARTESIAN_POINT ( 'NONE',  ( -4.903611268973031123, -5.000000000000039968, -16.52575844349512835 ) ) ;
#56416 = CARTESIAN_POINT ( 'NONE',  ( -29.68315524077004497, 8.302504244945346557, -42.10535821593474282 ) ) ;
#56417 = EDGE_CURVE ( 'NONE', #70351, #96436, #42254, .T. ) ;
#56418 = DIRECTION ( 'NONE',  ( -1.000000000000000000, -0.000000000000000000, -0.000000000000000000 ) ) ;
#56419 = CARTESIAN_POINT ( 'NONE',  ( 0.000000000000000000, 0.000000000000000000, -5.000000000000003553 ) ) ;
#56420 = CARTESIAN_POINT ( 'NONE',  ( 69.41260820018891309, -60.00000000000000711, 138.2351751275483878 ) ) ;
#56421 = CIRCLE ( 'NONE', #66848, 5.000000000000011546 ) ;
#56422 = CARTESIAN_POINT ( 'NONE',  ( -23.95564068939877345, 305.6666757346319514, -9.824255363916352124 ) ) ;
#56423 = ORIENTED_EDGE ( 'NONE', *, *, #102202, .T. ) ;
#56424 = DIRECTION ( 'NONE',  ( 0.000000000000000000, 0.000000000000000000, 1.000000000000000000 ) ) ;
#56425 = DIRECTION ( 'NONE',  ( 0.000000000000000000, 0.000000000000000000, -1.000000000000000000 ) ) ;
#56427 = DIRECTION ( 'NONE',  ( -0.000000000000000000, -0.000000000000000000, -1.000000000000000000 ) ) ;
#56426 = CARTESIAN_POINT ( 'NONE',  ( 16.35858893754161869, -14.21045842199445630, 34.55986707822809478 ) ) ;
#56429 = CONICAL_SURFACE ( 'NONE', #28955, 15.00000000000000000, 0.7509290623979402168 ) ;
#56428 = DIRECTION ( 'NONE',  ( 0.000000000000000000, -1.000000000000000000, 0.000000000000000000 ) ) ;
#56430 = VERTEX_POINT ( 'NONE', #62565 ) ;
#56432 = CARTESIAN_POINT ( 'NONE',  ( -26.74960312389934458, 311.3359961673855878, 11.49087433988725238 ) ) ;
#56431 = VECTOR ( 'NONE', #2999, 1000.000000000000227 ) ;
#56433 = ORIENTED_EDGE ( 'NONE', *, *, #93296, .F. ) ;
#56434 = DIRECTION ( 'NONE',  ( 0.000000000000000000, 0.000000000000000000, -1.000000000000000000 ) ) ;
#56435 = CARTESIAN_POINT ( 'NONE',  ( 3.884543032213806146, 15.13241195026071928, 9.216463528758731982 ) ) ;
#56436 = DIRECTION ( 'NONE',  ( 0.000000000000000000, -1.000000000000000000, 0.000000000000000000 ) ) ;
#56437 = SURFACE_STYLE_USAGE ( .BOTH. , #81245 ) ;
#56438 = ORIENTED_EDGE ( 'NONE', *, *, #76804, .F. ) ;
#56439 = ADVANCED_FACE ( 'NONE', ( #54971 ), #19915, .T. ) ;
#56440 = B_SPLINE_CURVE_WITH_KNOTS ( 'NONE', 3,
 ( #46116, #104877, #54170, #5121, #38565, #103804 ),
 .UNSPECIFIED., .F., .F.,
 ( 4, 2, 4 ),
 ( 2.475503369437265404E-07, 0.002222330217055646685, 0.004444412883774349725 ),
 .UNSPECIFIED. ) ;
#56441 = CARTESIAN_POINT ( 'NONE',  ( 5.000000000000000888, -12.28614229754743903, 10.41767341469848951 ) ) ;
#56442 = CARTESIAN_POINT ( 'NONE',  ( -101.0269275500464659, -60.00000000001482903, 204.0963534135034934 ) ) ;
#56443 = CARTESIAN_POINT ( 'NONE',  ( 44.20107474623475241, 485.5083548284977724, 3.133049558774994026 ) ) ;
#56444 = CARTESIAN_POINT ( 'NONE',  ( 78.98376820745889404, -60.00000000000002842, 194.5816734064725892 ) ) ;
#56445 = DIRECTION ( 'NONE',  ( -1.000000000000000000, 0.000000000000000000, -0.000000000000000000 ) ) ;
#56446 = DIRECTION ( 'NONE',  ( -1.000000000000000000, -1.224606353822377258E-16, -0.000000000000000000 ) ) ;
#56448 = CARTESIAN_POINT ( 'NONE',  ( 14.61249556130028004, -42.95373516407707370, 31.17290009735563316 ) ) ;
#56447 = CARTESIAN_POINT ( 'NONE',  ( -106.9593936918335544, -14.21045842199438880, 171.9682640579732436 ) ) ;
#56450 = CARTESIAN_POINT ( 'NONE',  ( 83.17395798262967332, -38.00000000000000000, -3.094716530419567402 ) ) ;
#56449 = PRODUCT_DEFINITION_CONTEXT ( 'detailed design', #30767, 'design' ) ;
#56451 = DIRECTION ( 'NONE',  ( 0.000000000000000000, 0.000000000000000000, 1.000000000000000000 ) ) ;
#56452 = CIRCLE ( 'NONE', #99494, 4.000000000000000888 ) ;
#56453 = CARTESIAN_POINT ( 'NONE',  ( -46.97696546697627440, -60.27403396181129835, 52.32368530384916738 ) ) ;
#56454 = EDGE_CURVE ( 'NONE', #103713, #85095, #87041, .T. ) ;
#56455 = CARTESIAN_POINT ( 'NONE',  ( -0.4139970039192563123, 35.05610801426639966, -27.31758834064758190 ) ) ;
#56456 = ORIENTED_EDGE ( 'NONE', *, *, #21221, .F. ) ;
#56457 = CARTESIAN_POINT ( 'NONE',  ( -29.00000000000000355, 6.123233995736765296E-16, -4.999999999999999112 ) ) ;
#56458 = CARTESIAN_POINT ( 'NONE',  ( 16.11142072793885305, 21.68022463236152930, 1.737955725794386730 ) ) ;
#56459 = LINE ( 'NONE', #44825, #48211 ) ;
#56460 = AXIS2_PLACEMENT_3D ( 'NONE', #54978, #31800, #46896 ) ;
#56461 = DIRECTION ( 'NONE',  ( 1.000000000000000000, 0.000000000000000000, 0.000000000000000000 ) ) ;
#56462 = CARTESIAN_POINT ( 'NONE',  ( 4.472135954999580498, -9.864207950534455094, 4.000000000000000888 ) ) ;
#56463 = CARTESIAN_POINT ( 'NONE',  ( 32.54922218626916930, 319.8023524069591303, -6.363686095274232457 ) ) ;
#56464 = EDGE_LOOP ( 'NONE', ( #58450, #28147, #30208, #46993 ) ) ;
#56465 = CARTESIAN_POINT ( 'NONE',  ( 60.63333333333333286, 6.915964383211875250E-15, 0.000000000000000000 ) ) ;
#56466 = AXIS2_PLACEMENT_3D ( 'NONE', #79084, #104960, #55321 ) ;
#56467 = EDGE_LOOP ( 'NONE', ( #58798, #8426, #6099, #89729, #24759 ) ) ;
#56468 = CARTESIAN_POINT ( 'NONE',  ( 104.4225999297474203, -29.99999999999820233, 196.1060340301228564 ) ) ;
#56469 = FACE_OUTER_BOUND ( 'NONE', #60110, .T. ) ;
#56470 = CARTESIAN_POINT ( 'NONE',  ( 6.771647573939279852, 41.86512692430649452, -59.59160515849491446 ) ) ;
#56471 = CARTESIAN_POINT ( 'NONE',  ( -2.979761111870779618E-15, 34.19642918197134662, -12.16579798332631412 ) ) ;
#56472 = CARTESIAN_POINT ( 'NONE',  ( 96.65141799564703717, -30.00000000000001066, 128.3146508404916801 ) ) ;
#56473 =( BOUNDED_SURFACE ( )  B_SPLINE_SURFACE ( 3, 2, ( 
 ( #71691, #30211, #39881 ),
 ( #95996, #105141, #56570 ),
 ( #81372, #104599, #15055 ),
 ( #7483, #22122, #104068 ),
 ( #55497, #97040, #5896 ),
 ( #54974, #56028, #15589 ),
 ( #31797, #73281, #32339 ),
 ( #89494, #23181, #46378 ),
 ( #47944, #65209, #13457 ),
 ( #98103, #47421, #13988 ) ),
 .UNSPECIFIED., .F., .F., .F. ) 
 B_SPLINE_SURFACE_WITH_KNOTS ( ( 4, 2, 2, 2, 4 ),
 ( 3, 3 ),
 ( 0.002450517525418903411, 0.003060732775749471640, 0.003670948026080039436, 0.004891378526741175028, 0.007332239528063447080 ),
 ( 0.000000000000000000, 1.000000000000000000 ),
 .UNSPECIFIED. ) 
 GEOMETRIC_REPRESENTATION_ITEM ( )  RATIONAL_B_SPLINE_SURFACE ( (
 ( 1.000000000000000000, 0.7071067811865481278, 1.000000000000000000),
 ( 1.000000000000000000, 0.7344063550101934679, 1.000000000000000000),
 ( 1.000000000000000000, 0.7590375248711017653, 1.000000000000000000),
 ( 1.000000000000000000, 0.8038331608704095688, 1.000000000000000000),
 ( 1.000000000000000000, 0.8240352460866353645, 1.000000000000000000),
 ( 1.000000000000000000, 0.8791017378332343091, 1.000000000000000000),
 ( 1.000000000000000000, 0.9085032776980891400, 1.000000000000000000),
 ( 1.000000000000000000, 0.9784170511696808070, 1.000000000000000000),
 ( 1.000000000000000000, 0.9996598051696591325, 1.000000000000000000),
 ( 1.000000000000000000, 1.000000000000000000, 1.000000000000000000) ) ) 
 REPRESENTATION_ITEM ( '' )  SURFACE ( )  );
#56474 = CARTESIAN_POINT ( 'NONE',  ( 6.928203230275507885, 104.7306907030446723, -4.000000000000001776 ) ) ;
#56475 = ADVANCED_FACE ( 'NONE', ( #85797 ), #63449, .F. ) ;
#56476 = ORIENTED_EDGE ( 'NONE', *, *, #19218, .T. ) ;
#56477 = EDGE_LOOP ( 'NONE', ( #11035, #77885, #30656, #24123, #91901, #78628 ) ) ;
#56478 = ORIENTED_EDGE ( 'NONE', *, *, #67267, .F. ) ;
#56479 = CIRCLE ( 'NONE', #71967, 4.000000000000000888 ) ;
#56480 = CARTESIAN_POINT ( 'NONE',  ( 1.833333333264058229, 42.00000000000000000, -60.21711271837359902 ) ) ;
#56481 = CARTESIAN_POINT ( 'NONE',  ( 22.43351772994257587, 26.08195184212913276, 30.96814220329011746 ) ) ;
#56482 = CIRCLE ( 'NONE', #9985, 7.999999999999994671 ) ;
#56483 = CARTESIAN_POINT ( 'NONE',  ( -40.05614242505708233, 464.9362658514420445, 17.76104857941754744 ) ) ;
#56484 = EDGE_LOOP ( 'NONE', ( #79933, #102080, #4214, #15726, #92550 ) ) ;
#56485 =( LENGTH_UNIT ( ) NAMED_UNIT ( * ) SI_UNIT ( .MILLI., .METRE. ) );
#56486 = ORIENTED_EDGE ( 'NONE', *, *, #80167, .T. ) ;
#56487 = LINE ( 'NONE', #23630, #22502 ) ;
#56488 = CARTESIAN_POINT ( 'NONE',  ( 77.54571322305440617, -38.51875396053564060, 186.6416166875725935 ) ) ;
#56489 = CARTESIAN_POINT ( 'NONE',  ( 0.000000000000000000, 0.000000000000000000, 0.000000000000000000 ) ) ;
#56490 = CARTESIAN_POINT ( 'NONE',  ( 81.10970025696315133, -37.99999999999997158, 151.4617437746981068 ) ) ;
#56491 = COLOUR_RGB ( '', 0.31764706, 0.68627451, 0.89019608) ;
#56492 = CARTESIAN_POINT ( 'NONE',  ( 41.26978454293845999, 329.6851661251676546, 10.40276537497734921 ) ) ;
#56493 = AXIS2_PLACEMENT_3D ( 'NONE', #68336, #13262, #40199 ) ;
#56494 = CARTESIAN_POINT ( 'NONE',  ( -41.17144925627792418, 461.2585203975968398, 2.461466063511708047 ) ) ;
#56495 = CARTESIAN_POINT ( 'NONE',  ( -5.437321008177769421, -47.65716784822934216, 104.0362115404849845 ) ) ;
#56496 = CARTESIAN_POINT ( 'NONE',  ( 31.08349330513380693, 1.593028355512270962E-15, 0.000000000000000000 ) ) ;
#56497 = EDGE_CURVE ( 'NONE', #11977, #81058, #84048, .T. ) ;
#56498 = ORIENTED_EDGE ( 'NONE', *, *, #76613, .T. ) ;
#56499 = MECHANICAL_DESIGN_GEOMETRIC_PRESENTATION_REPRESENTATION (  '', ( #96184 ), #54805 ) ;
#56500 = CARTESIAN_POINT ( 'NONE',  ( -35.50583740947284639, 381.5806922893717683, 5.955873595989558567 ) ) ;
#56501 = CARTESIAN_POINT ( 'NONE',  ( -31.32820169690777945, 299.5760797589559843, 10.99770074658509422 ) ) ;
#56502 = CARTESIAN_POINT ( 'NONE',  ( 37.33349330513379982, 4.898587196589405926E-16, -4.000000000000001776 ) ) ;
#56503 = DIRECTION ( 'NONE',  ( -1.000000000000000000, -1.224606353822377258E-16, -0.000000000000000000 ) ) ;
#56504 = CARTESIAN_POINT ( 'NONE',  ( 3.313708498984762496, -12.78124999999999289, 7.999999999999998224 ) ) ;
#56505 = CARTESIAN_POINT ( 'NONE',  ( -23.96426571639764092, -28.31959789768340130, 37.87134685329586148 ) ) ;
#56506 = EDGE_CURVE ( 'NONE', #27489, #96068, #12912, .T. ) ;
#56507 = FACE_OUTER_BOUND ( 'NONE', #18662, .T. ) ;
#56508 = AXIS2_PLACEMENT_3D ( 'NONE', #59960, #68574, #44287 ) ;
#56509 = DIRECTION ( 'NONE',  ( 0.000000000000000000, -0.000000000000000000, 1.000000000000000000 ) ) ;
#56510 = ORIENTED_EDGE ( 'NONE', *, *, #100290, .F. ) ;
#56511 = CARTESIAN_POINT ( 'NONE',  ( 86.40784132907582205, -17.71253999786838307, 176.2732639067367586 ) ) ;
#56512 = CIRCLE ( 'NONE', #13473, 4.000000000000007105 ) ;
#56513 = FACE_OUTER_BOUND ( 'NONE', #64456, .T. ) ;
#56514 = VERTEX_POINT ( 'NONE', #43588 ) ;
#56515 = CARTESIAN_POINT ( 'NONE',  ( 95.63906378175919087, -57.67167413368508022, 38.38847120207383767 ) ) ;
#56516 = EDGE_CURVE ( 'NONE', #29715, #100266, #100769, .T. ) ;
#56517 = CARTESIAN_POINT ( 'NONE',  ( 36.33173443512200862, 437.9974107914312640, 4.196572296725481266 ) ) ;
#56518 = DIRECTION ( 'NONE',  ( 1.000000000000000000, 0.000000000000000000, 0.000000000000000000 ) ) ;
#56519 = CIRCLE ( 'NONE', #104820, 3.400000000000000355 ) ;
#56520 = CARTESIAN_POINT ( 'NONE',  ( -79.29266753505190479, -38.00000000000007105, 139.9631112146612395 ) ) ;
#56521 =( NAMED_UNIT ( * ) PLANE_ANGLE_UNIT ( ) SI_UNIT ( $, .RADIAN. ) );
#56522 = CARTESIAN_POINT ( 'NONE',  ( -46.00000000000000000, 500.0000000000002274, 0.000000000000000000 ) ) ;
#56524 = CARTESIAN_POINT ( 'NONE',  ( -14.05151807610724646, 4.424082237322779498, 5.201963304297035684 ) ) ;
#56523 = PLANE ( 'NONE',  #43146 ) ;
#56525 = ORIENTED_EDGE ( 'NONE', *, *, #89578, .T. ) ;
#56526 = CARTESIAN_POINT ( 'NONE',  ( 9.549008551961874147, 295.0805096965325447, -10.04182235106940446 ) ) ;
#56527 = FILL_AREA_STYLE_COLOUR ( '', #104857 ) ;
#56528 = CARTESIAN_POINT ( 'NONE',  ( -27.71646321558792536, 36.65781963206741523, -7.705227733214372599 ) ) ;
#56529 = CARTESIAN_POINT ( 'NONE',  ( 9.606080321247246090, 15.83563386295778308, -2.802461721337421885 ) ) ;
#56530 = LINE ( 'NONE', #35499, #28850 ) ;
#56531 =( GEOMETRIC_REPRESENTATION_CONTEXT ( 3 ) GLOBAL_UNCERTAINTY_ASSIGNED_CONTEXT ( ( #22218 ) ) GLOBAL_UNIT_ASSIGNED_CONTEXT ( ( #37013, #102775, #19258 ) ) REPRESENTATION_CONTEXT ( 'NONE', 'WORKASPACE' ) );
#56532 = CARTESIAN_POINT ( 'NONE',  ( 68.90372024251841765, -29.95430108788154300, -21.28323659810347834 ) ) ;
#56533 =( GEOMETRIC_REPRESENTATION_CONTEXT ( 3 ) GLOBAL_UNCERTAINTY_ASSIGNED_CONTEXT ( ( #83915 ) ) GLOBAL_UNIT_ASSIGNED_CONTEXT ( ( #62526, #56521, #23139 ) ) REPRESENTATION_CONTEXT ( 'NONE', 'WORKASPACE' ) );
#56534 = ORIENTED_EDGE ( 'NONE', *, *, #92919, .T. ) ;
#56535 = CARTESIAN_POINT ( 'NONE',  ( 0.000000000000000000, 6.928203230275505220, -4.000000000000007994 ) ) ;
#56536 = DIRECTION ( 'NONE',  ( 0.000000000000000000, -1.000000000000000000, 0.000000000000000000 ) ) ;
#56538 = CARTESIAN_POINT ( 'NONE',  ( -28.05387351602792023, -21.77034952975806803, -28.92045250891730390 ) ) ;
#56537 = CARTESIAN_POINT ( 'NONE',  ( -2.212097561415799163, 14.31130214556278268, -0.5355294694855831095 ) ) ;
#56539 = ADVANCED_FACE ( 'NONE', ( #59790 ), #11196, .T. ) ;
#56540 = ORIENTED_EDGE ( 'NONE', *, *, #70245, .F. ) ;
#56541 = B_SPLINE_CURVE_WITH_KNOTS ( 'NONE', 3,
 ( #22124, #39364, #87907, #14512, #47423, #46895 ),
 .UNSPECIFIED., .F., .F.,
 ( 4, 2, 4 ),
 ( 0.008690415911505277452, 0.01102883712493079801, 0.01336725833835631684 ),
 .UNSPECIFIED. ) ;
#56542 = EDGE_LOOP ( 'NONE', ( #50074, #94538, #92448, #97055 ) ) ;
#56543 = CARTESIAN_POINT ( 'NONE',  ( -26.12980120306467313, 34.86887208967902296, 9.592984429938166357 ) ) ;
#56544 = CIRCLE ( 'NONE', #23888, 4.000000000000001776 ) ;
#56545 = EDGE_CURVE ( 'NONE', #40430, #81794, #90535, .T. ) ;
#56546 = CIRCLE ( 'NONE', #104771, 5.000000000000001776 ) ;
#56547 = EDGE_CURVE ( 'NONE', #99482, #64846, #81984, .T. ) ;
#56548 = CARTESIAN_POINT ( 'NONE',  ( 0.4037800551813721661, 4.058962678540097180, -5.969670414742690667 ) ) ;
#56549 = PLANE ( 'NONE',  #101150 ) ;
#56550 = CARTESIAN_POINT ( 'NONE',  ( -92.65848319411558975, -59.99999999999999289, -3.864875569882980866 ) ) ;
#56551 = EDGE_LOOP ( 'NONE', ( #84177, #55120, #37269, #82245, #88918, #24230 ) ) ;
#56552 = CARTESIAN_POINT ( 'NONE',  ( -6.287528586677907235E-14, 28.20649408426966431, -38.24999999999931077 ) ) ;
#56553 = DIRECTION ( 'NONE',  ( -0.000000000000000000, -1.000000000000000000, -0.000000000000000000 ) ) ;
#56554 = AXIS2_PLACEMENT_3D ( 'NONE', #87578, #72440, #37997 ) ;
#56555 = FACE_OUTER_BOUND ( 'NONE', #84704, .T. ) ;
#56557 = CARTESIAN_POINT ( 'NONE',  ( -17.81928184698856654, 45.39461501854592740, 4.975624619099529689 ) ) ;
#56556 = PRESENTATION_STYLE_ASSIGNMENT (( #90538 ) ) ;
#56558 = CARTESIAN_POINT ( 'NONE',  ( -83.89053484538156624, -25.60343038821535799, 156.2415415813698871 ) ) ;
#56559 = ORIENTED_EDGE ( 'NONE', *, *, #82149, .F. ) ;
#56560 = ORIENTED_EDGE ( 'NONE', *, *, #87664, .F. ) ;
#56561 = ORIENTED_EDGE ( 'NONE', *, *, #40757, .F. ) ;
#56562 = CARTESIAN_POINT ( 'NONE',  ( 7.157960986247998925, -5.000000000000000000, -14.69147069243657100 ) ) ;
#56563 = CARTESIAN_POINT ( 'NONE',  ( -5.000000000000000000, -14.90207541443127148, 12.47233211438449629 ) ) ;
#56564 = DIRECTION ( 'NONE',  ( -0.000000000000000000, 1.000000000000000000, -0.000000000000000000 ) ) ;
#56565 = ORIENTED_EDGE ( 'NONE', *, *, #93956, .F. ) ;
#56566 = ADVANCED_FACE ( 'NONE', ( #2584 ), #31973, .T. ) ;
#56567 = CARTESIAN_POINT ( 'NONE',  ( -42.99999999999998579, 487.9285348210859752, 8.903916466042446132 ) ) ;
#56568 = CARTESIAN_POINT ( 'NONE',  ( -3.068228200247433018E-15, 53.37899725327129374, 25.05398456423234066 ) ) ;
#56569 = AXIS2_PLACEMENT_3D ( 'NONE', #64789, #90126, #73387 ) ;
#56570 = CARTESIAN_POINT ( 'NONE',  ( -10.00000000000000000, 15.00000000000000000, -4.397168787612341312 ) ) ;
#56571 = CARTESIAN_POINT ( 'NONE',  ( -100.8911947370258844, -57.62911827813870502, 203.6698938757279223 ) ) ;
#56572 = CARTESIAN_POINT ( 'NONE',  ( -5.858881034796412202, -68.78586324002981200, 1.317748741875970797 ) ) ;
#56573 = DIRECTION ( 'NONE',  ( 0.000000000000000000, 1.000000000000000000, 0.000000000000000000 ) ) ;
#56574 = CIRCLE ( 'NONE', #72147, 3.309500000000001663 ) ;
#56575 = CARTESIAN_POINT ( 'NONE',  ( -20.24579557674108088, 304.8297271373347144, -10.00469232190996749 ) ) ;
#56576 = FACE_BOUND ( 'NONE', #39984, .T. ) ;
#56577 = CARTESIAN_POINT ( 'NONE',  ( 40.74889026577078965, -14.21045842199439591, -34.22240887780809260 ) ) ;
#56578 = EDGE_CURVE ( 'NONE', #60134, #44183, #74199, .T. ) ;
#56579 = CARTESIAN_POINT ( 'NONE',  ( -16.61716630718971643, -29.99999999999995026, 37.21284229651715947 ) ) ;
#56580 = CARTESIAN_POINT ( 'NONE',  ( -54.05184654259630150, -22.16297058472909498, 51.66483102732016874 ) ) ;
#56581 = CIRCLE ( 'NONE', #61870, 4.000000000000001776 ) ;
#56582 = DIRECTION ( 'NONE',  ( -0.000000000000000000, -0.000000000000000000, 1.000000000000000000 ) ) ;
#56583 = ORIENTED_EDGE ( 'NONE', *, *, #77116, .T. ) ;
#56584 = CARTESIAN_POINT ( 'NONE',  ( -97.42952934929957109, -60.35587105709884526, 196.6991795949842299 ) ) ;
#56585 = CARTESIAN_POINT ( 'NONE',  ( -1.488823952716137988, 295.3362597640263516, -10.00085782936719880 ) ) ;
#56586 = STYLED_ITEM ( 'NONE', ( #41376 ), #31006 ) ;
#56587 = ORIENTED_EDGE ( 'NONE', *, *, #31341, .F. ) ;
#56588 = CARTESIAN_POINT ( 'NONE',  ( -16.80185364056168140, 43.70017998952184968, 4.157797401561232675 ) ) ;
#56589 = ADVANCED_FACE ( 'NONE', ( #92667 ), #92212, .T. ) ;
#56590 = CARTESIAN_POINT ( 'NONE',  ( 92.11181465698672355, -38.35455481329138649, 36.38192987799886424 ) ) ;
#56591 = DIRECTION ( 'NONE',  ( 0.000000000000000000, 0.000000000000000000, 1.000000000000000000 ) ) ;
#56592 = CARTESIAN_POINT ( 'NONE',  ( -7.188101187500001821, -11.37500000204838813, -2.977408999572651371 ) ) ;
#56593 = CARTESIAN_POINT ( 'NONE',  ( -15.86549515342121452, 294.5609651447646229, 9.875179695847329242 ) ) ;
#56594 = CARTESIAN_POINT ( 'NONE',  ( -18.00000000000000355, 12.99999999999999289, -7.500000000000000000 ) ) ;
#56595 = CARTESIAN_POINT ( 'NONE',  ( 82.48055652934633031, -30.00000000000000711, 149.2060676150218796 ) ) ;
#56596 = CARTESIAN_POINT ( 'NONE',  ( 5.299999999999999822, 0.000000000000000000, 0.000000000000000000 ) ) ;
#56597 = DIRECTION ( 'NONE',  ( -1.000000000000000000, -1.224606353822377258E-16, -0.000000000000000000 ) ) ;
#56598 = CARTESIAN_POINT ( 'NONE',  ( -28.52985215182788892, 11.34625443571976078, 41.35275482200152197 ) ) ;
#56599 = CARTESIAN_POINT ( 'NONE',  ( -6.831985876597696183, 3.295913427296334408, -6.443925148804114045 ) ) ;
#56600 = STYLED_ITEM ( 'NONE', ( #75254 ), #76497 ) ;
#56601 = EDGE_LOOP ( 'NONE', ( #74328, #94385, #298, #11778, #57324 ) ) ;
#56602 = ORIENTED_EDGE ( 'NONE', *, *, #64455, .F. ) ;
#56603 = CARTESIAN_POINT ( 'NONE',  ( 50.33955204055388322, -56.83121431495037967, 57.28224304148754698 ) ) ;
#56604 = CARTESIAN_POINT ( 'NONE',  ( 5.415856237588537958, 41.85405046271414875, -58.97635192936115800 ) ) ;
#56606 = CLOSED_SHELL ( 'NONE', ( #15243, #31515, #74678, #34271, #54999, #27981, #103525, #26328, #24546, #33614, #18657, #4449, #32241, #68817 ) ) ;
#56605 = FACE_OUTER_BOUND ( 'NONE', #37224, .T. ) ;
#56607 = ORIENTED_EDGE ( 'NONE', *, *, #99623, .T. ) ;
#56608 = CARTESIAN_POINT ( 'NONE',  ( -108.4759618192267538, -38.35621021443558476, 141.3483429577475761 ) ) ;
#56609 = ORIENTED_EDGE ( 'NONE', *, *, #35977, .T. ) ;
#56610 = CARTESIAN_POINT ( 'NONE',  ( 54.52222222222221859, -3.309500000000000774, 4.475777889183797681E-16 ) ) ;
#56611 = CARTESIAN_POINT ( 'NONE',  ( 92.05394513303022563, -38.35408998850439133, 35.25469512580827569 ) ) ;
#56612 = CARTESIAN_POINT ( 'NONE',  ( 10.24044431011775025, 16.34647364769404732, -10.08608596195729135 ) ) ;
#56613 = CARTESIAN_POINT ( 'NONE',  ( -42.71735565817839131, 428.6843791680139475, 18.96713788493819663 ) ) ;
#56614 = CARTESIAN_POINT ( 'NONE',  ( 104.6332049901833301, -52.71708914408988278, 158.7351461483158062 ) ) ;
#56615 = DIRECTION ( 'NONE',  ( -1.000000000000000000, -0.000000000000000000, -0.000000000000000000 ) ) ;
#56616 = FACE_OUTER_BOUND ( 'NONE', #24530, .T. ) ;
#56617 = CARTESIAN_POINT ( 'NONE',  ( -30.72240112801715384, 310.9384333019646078, -8.350412465344515311 ) ) ;
#56618 =( NAMED_UNIT ( * ) SI_UNIT ( $, .STERADIAN. ) SOLID_ANGLE_UNIT ( ) );
#56619 = CARTESIAN_POINT ( 'NONE',  ( 85.18286175503386914, -59.99999999999999289, 200.1974052157080735 ) ) ;
#56620 = AXIS2_PLACEMENT_3D ( 'NONE', #87082, #47124, #14749 ) ;
#56621 = CARTESIAN_POINT ( 'NONE',  ( -43.71217423904473520, 435.6632154632215475, 9.092528312227507570 ) ) ;
#56622 = ORIENTED_EDGE ( 'NONE', *, *, #56843, .F. ) ;
#56623 = CARTESIAN_POINT ( 'NONE',  ( 56.02781999547231351, -32.55576276548075043, 59.68983337992042948 ) ) ;
#56624 = CARTESIAN_POINT ( 'NONE',  ( -34.42777433040655666, 300.8302020014492655, -8.658268271844590913 ) ) ;
#56625 = CARTESIAN_POINT ( 'NONE',  ( 9.521849859704259345, -51.55475818109406561, 23.94093251888962470 ) ) ;
#56626 = ADVANCED_FACE ( 'NONE', ( #75952 ), #18825, .F. ) ;
#56627 = CARTESIAN_POINT ( 'NONE',  ( -6.390922558478501436, -4.999999999999999112, -15.34850256275529112 ) ) ;
#56628 = EDGE_LOOP ( 'NONE', ( #77349, #81935, #101857, #3441 ) ) ;
#56630 = CARTESIAN_POINT ( 'NONE',  ( -14.87651757722494139, 23.07725274647275526, -1.016940421418421892 ) ) ;
#56629 = CARTESIAN_POINT ( 'NONE',  ( -90.41875325581872858, -38.40214660397878532, -14.85380760910452125 ) ) ;
#56631 = CARTESIAN_POINT ( 'NONE',  ( -42.55893460000644524, 435.1566242046031334, 18.92048169488384346 ) ) ;
#56632 = CARTESIAN_POINT ( 'NONE',  ( 20.45590100891671526, 304.8998341874647622, 8.947178418926538868 ) ) ;
#56633 = LINE ( 'NONE', #23786, #76480 ) ;
#56634 = CARTESIAN_POINT ( 'NONE',  ( -3.594029362035469966, -9.531975552779805128, 6.225090491435913975 ) ) ;
#56635 = CARTESIAN_POINT ( 'NONE',  ( 0.000000000000000000, 45.89575828009193259, 0.000000000000000000 ) ) ;
#56636 = AXIS2_PLACEMENT_3D ( 'NONE', #73749, #98032, #40327 ) ;
#56637 = EDGE_CURVE ( 'NONE', #55094, #52776, #50868, .T. ) ;
#56638 = VECTOR ( 'NONE', #101272, 1000.000000000000000 ) ;
#56639 = CARTESIAN_POINT ( 'NONE',  ( -33.00496812084397646, 465.6658704666172639, 15.15901827095664522 ) ) ;
#56640 = VERTEX_POINT ( 'NONE', #59254 ) ;
#56641 = CARTESIAN_POINT ( 'NONE',  ( 84.47475691905646045, -32.43330153130234095, 172.8622483833046033 ) ) ;
#56642 = CARTESIAN_POINT ( 'NONE',  ( 4.247384345738219658, -12.84326104839635896, -9.569854795092682664 ) ) ;
#56643 = CARTESIAN_POINT ( 'NONE',  ( -35.73338497923415957, 439.1098013319271445, 24.04626675101893696 ) ) ;
#56644 = VERTEX_POINT ( 'NONE', #25309 ) ;
#56645 = CARTESIAN_POINT ( 'NONE',  ( -31.03678703374875880, 438.6650838204938054, 21.86890379898545334 ) ) ;
#56646 = EDGE_CURVE ( 'NONE', #478, #18278, #92128, .T. ) ;
#56647 = CARTESIAN_POINT ( 'NONE',  ( 40.38558041326821524, 460.4656361498749675, 1.744807035484959634 ) ) ;
#56648 = CARTESIAN_POINT ( 'NONE',  ( 14.37299415487856713, 2.005565780252362540, 4.271091604485595106 ) ) ;
#56649 = CARTESIAN_POINT ( 'NONE',  ( -39.01859936591235112, 42.04209281348008176, -56.85829446836521583 ) ) ;
#56650 = CARTESIAN_POINT ( 'NONE',  ( -28.71655383515105697, 10.49725697686257675, -41.65669210871969597 ) ) ;
#56651 = ORIENTED_EDGE ( 'NONE', *, *, #2698, .T. ) ;
#56652 = B_SPLINE_CURVE_WITH_KNOTS ( 'NONE', 3,
 ( #74841, #98069, #24218, #33906, #31766, #56532, #58690, #91591, #83478, #39852, #72724, #105626, #64648, #97522, #23684, #57068, #52172, #85630, #27424, #76986, #92635, #19867, #43033, #101274, #75922, #59225, #60302, #92100, #84559, #10123, #59759, #3100, #10642, #69443, #18793, #76444, #36045, #68380, #53253, #93175, #34971, #2023, #101791, #51100, #93713, #42488, #84017, #1482, #68917, #67834, #26885, #100723, #19343, #28475, #34447, #85086, #102325, #51640, #27959, #43559, #11704, #3640, #36576, #60822, #61353, #52702, #2554, #94248, #35500, #11171, #44639, #44097, #67316, #77526, #20408, #9577, #75383, #100198, #26363, #18242, #20933, #21436, #61894, #86699, #37100, #104436, #38158, #94790, #46221, #80160, #64014, #96892, #71017, #104985, #95306 ),
 .UNSPECIFIED., .F., .F.,
 ( 4, 2, 2, 1, 1, 1, 2, 2, 2, 1, 1, 1, 1, 2, 2, 2, 2, 1, 1, 1, 2, 2, 1, 2, 2, 1, 1, 1, 2, 2, 1, 2, 2, 1, 1, 1, 1, 2, 2, 1, 2, 2, 2, 1, 1, 2, 2, 1, 2, 2, 2, 1, 1, 2, 2, 2, 2, 2, 2, 4 ),
 ( 0.000000000000000000, 0.01569797913311701126, 0.02354696869967563139, 0.02747146348295482002, 0.02943371087459440219, 0.03041483457041407878, 0.03090539641832402984, 0.03139595826623398089, 0.04709393739935408690, 0.05494292696591414338, 0.05886742174919416121, 0.06082966914083415971, 0.06181079283665415897, 0.06230135468456415859, 0.06279191653247415128, 0.09418787479871693069, 0.1098858539318383204, 0.1177348434983990361, 0.1216593382816793245, 0.1236215856733193647, 0.1246027093691394749, 0.1250932712170494676, 0.1255838330649594325, 0.1569797913311997695, 0.1726777704643198963, 0.1805267600308799736, 0.1844512548141599984, 0.1864135022058000801, 0.1873946259016200655, 0.1878851877495300027, 0.1883757495974398843, 0.2197717078636771959, 0.2354696869967959350, 0.2433186765633552073, 0.2472431713466348435, 0.2492054187382747588, 0.2496959805861847237, 0.2499412615101397617, 0.2501865424340947719, 0.2511676661299149793, 0.3139595826624118069, 0.3453555409286603317, 0.3610535200617845941, 0.3689025096283466421, 0.3728270044116277493, 0.3747892518032683307, 0.3757703754990885936, 0.3767514991949088565, 0.4081474574611569928, 0.4238454365942810331, 0.4316944261608430811, 0.4356189209441241328, 0.4366000446399443957, 0.4370906064878545272, 0.4375811683357646587, 0.4395434157274052400, 0.4709393739936550416, 0.4866373531267799146, 0.4944863426933423511, 0.5023353322599047877 ),
 .UNSPECIFIED. ) ;
#56653 = CARTESIAN_POINT ( 'NONE',  ( 7.344133061198929724, 107.4449439268058057, 3.176267128233876136 ) ) ;
#56654 = DIRECTION ( 'NONE',  ( 0.000000000000000000, 0.000000000000000000, -1.000000000000000000 ) ) ;
#56657 = STYLED_ITEM ( 'NONE', ( #96697 ), #33066 ) ;
#56656 = CARTESIAN_POINT ( 'NONE',  ( -10.51652355666575467, 10.28136275940053856, -10.32830338406821902 ) ) ;
#56655 = CARTESIAN_POINT ( 'NONE',  ( -22.17399802466769287, -27.13132360212460981, 37.38406957163105915 ) ) ;
#56658 = CARTESIAN_POINT ( 'NONE',  ( -1.320432766682874540E-15, -13.53125000204838457, 7.188101187500000044 ) ) ;
#56659 = CARTESIAN_POINT ( 'NONE',  ( -43.69716417776824358, 40.83906611472755088, 48.48761666261796677 ) ) ;
#56660 = SURFACE_SIDE_STYLE ('',( #14603 ) ) ;
#56661 = AXIS2_PLACEMENT_3D ( 'NONE', #68279, #100632, #67224 ) ;
#56662 = VERTEX_POINT ( 'NONE', #18276 ) ;
#56663 = DIRECTION ( 'NONE',  ( 0.000000000000000000, -1.000000000000000000, 0.000000000000000000 ) ) ;
#56664 = CARTESIAN_POINT ( 'NONE',  ( -30.00000000000000000, 0.000000000000000000, 0.000000000000000000 ) ) ;
#56665 = CARTESIAN_POINT ( 'NONE',  ( 82.70911704725124025, 5.000000000000023093, 6.123233995736781074E-16 ) ) ;
#56666 = CARTESIAN_POINT ( 'NONE',  ( -6.931554132395168821, -5.000000000000945022, -71.13906995425499247 ) ) ;
#56667 = DIRECTION ( 'NONE',  ( -0.000000000000000000, -0.000000000000000000, 1.000000000000000000 ) ) ;
#56668 = EDGE_CURVE ( 'NONE', #29831, #2324, #76692, .T. ) ;
#56669 = ORIENTED_EDGE ( 'NONE', *, *, #72727, .T. ) ;
#56670 = VECTOR ( 'NONE', #24589, 1000.000000000000000 ) ;
#56671 = CARTESIAN_POINT ( 'NONE',  ( -4.905194654929173836, -87.02394395019842932, 3.459476078998853676 ) ) ;
#56672 = CARTESIAN_POINT ( 'NONE',  ( 9.833493305133801599, 4.000000000000002665, 0.000000000000000000 ) ) ;
#56673 = ORIENTED_EDGE ( 'NONE', *, *, #54948, .T. ) ;
#56674 = CLOSED_SHELL ( 'NONE', ( #49527, #18983, #95029, #87857, #75704, #25199, #5412, #29970, #18198, #70987, #50146 ) ) ;
#56675 = EDGE_CURVE ( 'NONE', #3039, #36200, #59527, .T. ) ;
#56676 = FILL_AREA_STYLE_COLOUR ( '', #97146 ) ;
#56677 =( LENGTH_UNIT ( ) NAMED_UNIT ( * ) SI_UNIT ( .MILLI., .METRE. ) );
#56678 = CARTESIAN_POINT ( 'NONE',  ( -23.97670849968361395, 41.62117736604113816, -74.33761154807883997 ) ) ;
#56679 = UNCERTAINTY_MEASURE_WITH_UNIT (LENGTH_MEASURE( 1.000000000000000082E-05 ), #58996, 'distance_accuracy_value', 'NONE');
#56680 = CARTESIAN_POINT ( 'NONE',  ( -112.0851447084041439, -60.00000000000000000, 178.2367466408115888 ) ) ;
#56681 = CARTESIAN_POINT ( 'NONE',  ( 28.49074715056170959, 18.29855530143743181, -40.46824935483557795 ) ) ;
#56682 = FACE_OUTER_BOUND ( 'NONE', #81813, .T. ) ;
#56683 = CARTESIAN_POINT ( 'NONE',  ( 4.582575694955842494, 16.00000000000000000, -9.999999999999998224 ) ) ;
#56684 = CARTESIAN_POINT ( 'NONE',  ( -9.680134077953582050, 2.794975873512704378, 14.73912665704113500 ) ) ;
#56686 = CARTESIAN_POINT ( 'NONE',  ( 32.00044432194599153, 486.9480297505133990, 7.098288108114727990 ) ) ;
#56685 = CARTESIAN_POINT ( 'NONE',  ( 9.596002107491598210, -5.000000000000002665, -92.37456064098007857 ) ) ;
#56687 = MECHANICAL_DESIGN_GEOMETRIC_PRESENTATION_REPRESENTATION (  '', ( #103226 ), #5059 ) ;
#56688 = CARTESIAN_POINT ( 'NONE',  ( -85.50314036829099962, -25.31086881602239913, 172.5804574615907541 ) ) ;
#56689 = ORIENTED_EDGE ( 'NONE', *, *, #99839, .T. ) ;
#56690 = ORIENTED_EDGE ( 'NONE', *, *, #104668, .T. ) ;
#56691 = VERTEX_POINT ( 'NONE', #21467 ) ;
#56692 = CARTESIAN_POINT ( 'NONE',  ( -13.00000000000003730, -65.00000000000000000, 0.000000000000000000 ) ) ;
#56693 = FACE_OUTER_BOUND ( 'NONE', #70049, .T. ) ;
#56694 = EDGE_CURVE ( 'NONE', #59320, #81173, #70354, .T. ) ;
#56695 = LINE ( 'NONE', #89086, #1179 ) ;
#56696 = CARTESIAN_POINT ( 'NONE',  ( -6.944031699373468314, -64.46539345443871127, 3.972913591453824278 ) ) ;
#56697 = CARTESIAN_POINT ( 'NONE',  ( 4.250000000000000000, 0.000000000000000000, -10.00000000000000000 ) ) ;
#56698 = CARTESIAN_POINT ( 'NONE',  ( -12.12948968253070881, -5.000000000000000000, -89.82632555826474174 ) ) ;
#56699 = CARTESIAN_POINT ( 'NONE',  ( -43.18057774162383566, 485.1460640375049707, 5.477159825600939946 ) ) ;
#56700 = CARTESIAN_POINT ( 'NONE',  ( 114.5100518737696689, -60.00000000000002132, 177.0882855716755557 ) ) ;
#56701 = CARTESIAN_POINT ( 'NONE',  ( -108.0662369917864680, -29.99999999999997513, 149.4678941581608740 ) ) ;
#56702 = CARTESIAN_POINT ( 'NONE',  ( -61.92732175817126716, -56.86970651190488724, 86.14273502844355335 ) ) ;
#56703 = ORIENTED_EDGE ( 'NONE', *, *, #84430, .F. ) ;
#56704 = CARTESIAN_POINT ( 'NONE',  ( -14.49391709338271816, 38.95396881702665581, 62.06433840696379178 ) ) ;
#56705 = CARTESIAN_POINT ( 'NONE',  ( 103.1163125918749870, -59.99999999997518785, 203.2865156566705025 ) ) ;
#56706 =( GEOMETRIC_REPRESENTATION_CONTEXT ( 3 ) GLOBAL_UNCERTAINTY_ASSIGNED_CONTEXT ( ( #83983 ) ) GLOBAL_UNIT_ASSIGNED_CONTEXT ( ( #9844, #34706, #25009 ) ) REPRESENTATION_CONTEXT ( 'NONE', 'WORKASPACE' ) );
#56707 = ORIENTED_EDGE ( 'NONE', *, *, #88264, .F. ) ;
#56708 = CARTESIAN_POINT ( 'NONE',  ( 13.56235479181388115, -55.77948487150412404, 23.52533112101723844 ) ) ;
#56709 = CARTESIAN_POINT ( 'NONE',  ( -7.188101187500002709, -12.68750000204838635, 2.977408999572647819 ) ) ;
#56710 = ADVANCED_FACE ( 'NONE', ( #102354 ), #11289, .T. ) ;
#56711 = CARTESIAN_POINT ( 'NONE',  ( -5.290067270632216712, 52.08006895350504095, 6.031152949374556371 ) ) ;
#56712 = ORIENTED_EDGE ( 'NONE', *, *, #46430, .T. ) ;
#56713 = CARTESIAN_POINT ( 'NONE',  ( 35.59152797293441495, 464.2026968846542445, 19.31774162833587383 ) ) ;
#56714 = ORIENTED_EDGE ( 'NONE', *, *, #55868, .T. ) ;
#56715 = CARTESIAN_POINT ( 'NONE',  ( -43.32918576489194606, 484.9664181796746902, 4.870614540792155722 ) ) ;
#56716 = LINE ( 'NONE', #15204, #42021 ) ;
#56717 = CARTESIAN_POINT ( 'NONE',  ( -101.6271150938965633, -59.99999999999997868, 201.3150328502970581 ) ) ;
#56718 = CARTESIAN_POINT ( 'NONE',  ( 9.934548988108780065, -57.86759105402752823, 28.17116772486389564 ) ) ;
#56719 = CARTESIAN_POINT ( 'NONE',  ( 2.977408999572651815, -28.81250000204838457, 7.188101187500000933 ) ) ;
#56720 = CARTESIAN_POINT ( 'NONE',  ( 46.00000000000000000, 461.2902899409244242, 8.859728897585586793 ) ) ;
#56721 = CARTESIAN_POINT ( 'NONE',  ( -6.075342555560988345, 53.39437066006075838, -8.268384239318029572 ) ) ;
#56722 = CARTESIAN_POINT ( 'NONE',  ( -10.59260543037239799, -5.000000000000000000, -12.53864087336843447 ) ) ;
#56723 = CARTESIAN_POINT ( 'NONE',  ( 22.33349330513380337, -7.703719777548943412E-31, 4.000000000000001776 ) ) ;
#56724 = CARTESIAN_POINT ( 'NONE',  ( 26.69900261086841198, -5.000000000000000888, 6.123233995736769241E-16 ) ) ;
#56725 = DIRECTION ( 'NONE',  ( -0.5735764363510497121, 0.8191520442889892450, 1.003171929053521665E-16 ) ) ;
#56726 = CARTESIAN_POINT ( 'NONE',  ( 90.21675587111627692, -60.00000000000002132, 56.33244548193629697 ) ) ;
#56727 = CARTESIAN_POINT ( 'NONE',  ( -31.50654607522282546, -25.60952003222888251, 31.14771393841350644 ) ) ;
#56728 = VECTOR ( 'NONE', #78473, 999.9999999999998863 ) ;
#56729 = CARTESIAN_POINT ( 'NONE',  ( -1.545654944153988408, -49.97154544717239588, 101.5781950003720482 ) ) ;
#56730 = CIRCLE ( 'NONE', #70536, 0.6186547224754559426 ) ;
#56731 = CARTESIAN_POINT ( 'NONE',  ( 39.66000813785471735, -49.88695016216475864, 40.68345913021443039 ) ) ;
#56732 =( NAMED_UNIT ( * ) PLANE_ANGLE_UNIT ( ) SI_UNIT ( $, .RADIAN. ) );
#56733 = ORIENTED_EDGE ( 'NONE', *, *, #70664, .F. ) ;
#56734 =( GEOMETRIC_REPRESENTATION_CONTEXT ( 3 ) GLOBAL_UNCERTAINTY_ASSIGNED_CONTEXT ( ( #78496 ) ) GLOBAL_UNIT_ASSIGNED_CONTEXT ( ( #97084, #16704, #84631 ) ) REPRESENTATION_CONTEXT ( 'NONE', 'WORKASPACE' ) );
#56735 = CARTESIAN_POINT ( 'NONE',  ( -73.92149184568339138, -38.32661406644628244, 159.6910106498240225 ) ) ;
#56736 = ORIENTED_EDGE ( 'NONE', *, *, #82743, .F. ) ;
#56738 = CARTESIAN_POINT ( 'NONE',  ( 44.66387834505498944, 341.6072687625629101, 1.189588019127773677 ) ) ;
#56737 = CARTESIAN_POINT ( 'NONE',  ( 2.499999999999999556, -8.980730705452300455, 18.56355459479395620 ) ) ;
#56739 = CARTESIAN_POINT ( 'NONE',  ( -52.56491209535032993, 39.42572890908718364, -38.23519342730719472 ) ) ;
#56740 = CARTESIAN_POINT ( 'NONE',  ( -7.054523059426879961, 41.71556238290650498, -59.55896278357374030 ) ) ;
#56741 = CARTESIAN_POINT ( 'NONE',  ( 0.6416334532436100968, 44.01761382017788549, -16.42407442096259729 ) ) ;
#56742 = CARTESIAN_POINT ( 'NONE',  ( -38.78071457445877712, 25.16813833650925503, 12.51568302197794047 ) ) ;
#56743 = CARTESIAN_POINT ( 'NONE',  ( -28.74870929803160635, 319.1494203397336378, 12.45838930289386504 ) ) ;
#56744 = CARTESIAN_POINT ( 'NONE',  ( 100.6605546286570529, -60.00000000000000711, 84.90741128258979131 ) ) ;
#56745 = CARTESIAN_POINT ( 'NONE',  ( -42.18756898894582719, 484.4522853017719513, -2.425645685620470449 ) ) ;
#56746 = FACE_OUTER_BOUND ( 'NONE', #103320, .T. ) ;
#56747 = CARTESIAN_POINT ( 'NONE',  ( -2.499999999999999556, -11.82939293535852343, 20.68570066208713243 ) ) ;
#56748 = VERTEX_POINT ( 'NONE', #53280 ) ;
#56749 = EDGE_CURVE ( 'NONE', #54573, #15029, #45736, .T. ) ;
#56750 = CARTESIAN_POINT ( 'NONE',  ( -99.54366155252257897, -30.00000000000000711, 187.3415679194916947 ) ) ;
#56751 = ORIENTED_EDGE ( 'NONE', *, *, #36439, .F. ) ;
#56752 = CIRCLE ( 'NONE', #60275, 1.000000000000000888 ) ;
#56753 = CARTESIAN_POINT ( 'NONE',  ( -9.933368185767806224, -57.79351752493647609, 25.82212275612567964 ) ) ;
#56754 = CARTESIAN_POINT ( 'NONE',  ( -15.86692673747445603, 3.934633648119529425, -3.950574283722150248 ) ) ;
#56755 = CARTESIAN_POINT ( 'NONE',  ( 9.609486011791082305, 8.908497650349785246, 0.000000000000000000 ) ) ;
#56756 = CARTESIAN_POINT ( 'NONE',  ( 102.0666666666666629, 4.172000000000019249, 5.109226446042768454E-16 ) ) ;
#56757 = CARTESIAN_POINT ( 'NONE',  ( -23.21751746555280249, 28.11705169068991239, -30.70617127781034839 ) ) ;
#56758 = CARTESIAN_POINT ( 'NONE',  ( -7.188101187500002709, -27.68750000204838813, 2.977408999572648707 ) ) ;
#56759 = DIRECTION ( 'NONE',  ( -1.000000000000000000, -1.224606353822377258E-16, -0.000000000000000000 ) ) ;
#56760 = CARTESIAN_POINT ( 'NONE',  ( 7.071721972134253242, 41.30029428951767301, -70.42654619687203876 ) ) ;
#56761 = EDGE_CURVE ( 'NONE', #92197, #70305, #104310, .T. ) ;
#56762 = EDGE_LOOP ( 'NONE', ( #68141, #71185, #41579, #84640 ) ) ;
#56763 = EDGE_CURVE ( 'NONE', #78737, #37873, #22809, .T. ) ;
#56764 = STYLED_ITEM ( 'NONE', ( #10554 ), #70987 ) ;
#56766 = VERTEX_POINT ( 'NONE', #4196 ) ;
#56765 = CARTESIAN_POINT ( 'NONE',  ( -10.00000000000000355, 85.00000000000000000, 4.000000000000000000 ) ) ;
#56767 = CARTESIAN_POINT ( 'NONE',  ( 80.89341655852713586, -39.49760101440538307, 151.8480467892282775 ) ) ;
#56768 = VECTOR ( 'NONE', #51116, 1000.000000000000000 ) ;
#56769 = CARTESIAN_POINT ( 'NONE',  ( -5.787521267941007963, 41.99999999999999289, -59.87256577776128097 ) ) ;
#56770 = DIRECTION ( 'NONE',  ( -1.000000000000000000, -0.000000000000000000, -0.000000000000000000 ) ) ;
#56771 = ORIENTED_EDGE ( 'NONE', *, *, #33542, .F. ) ;
#56772 = CARTESIAN_POINT ( 'NONE',  ( 15.11650669486618881, 1.474610560812782335E-15, 0.000000000000000000 ) ) ;
#56773 = EDGE_CURVE ( 'NONE', #52640, #5765, #56088, .T. ) ;
#56774 = DIRECTION ( 'NONE',  ( 1.000000000000000000, -0.000000000000000000, -0.000000000000000000 ) ) ;
#56775 = CARTESIAN_POINT ( 'NONE',  ( -5.082755093536326818, -15.21875000204838457, 5.082755093536325042 ) ) ;
#56776 = CARTESIAN_POINT ( 'NONE',  ( 7.414346147792000075, 27.35410842337735815, -3.010818766110528344 ) ) ;
#56777 =( BOUNDED_CURVE ( )  B_SPLINE_CURVE ( 2, ( #101227, #78009, #4126, #35457, #36534, #3054, #102281, #37594, #44595 ),
 .UNSPECIFIED., .F., .F. ) 
 B_SPLINE_CURVE_WITH_KNOTS ( ( 3, 2, 2, 2, 3 ),
 ( 0.8676470588235293269, 0.8749999999999998890, 0.8823529411764705621, 0.8897058823529411242, 0.8970588235294117974 ),
 .UNSPECIFIED. ) 
 CURVE ( )  GEOMETRIC_REPRESENTATION_ITEM ( )  RATIONAL_B_SPLINE_CURVE ( ( 1.000000000000001110, 0.9238795325112856283, 1.000000000000000000, 0.9238795325112867385, 1.000000000000000000, 0.9238795325112867385, 1.000000000000000000, 0.9238795325112867385, 1.000000000000000000 ) ) 
 REPRESENTATION_ITEM ( '' )  );
#56778 = CARTESIAN_POINT ( 'NONE',  ( -21.50832034731008591, -57.67247026516260178, 42.43288772392129715 ) ) ;
#56779 = CARTESIAN_POINT ( 'NONE',  ( 20.97754405179124504, 294.8763868968453608, 9.942224931492244622 ) ) ;
#56780 = EDGE_LOOP ( 'NONE', ( #15392, #72636, #38489, #35815, #54741, #103393 ) ) ;
#56781 = B_SPLINE_CURVE_WITH_KNOTS ( 'NONE', 3,
 ( #21902, #87678, #13230, #38091, #44567 ),
 .UNSPECIFIED., .F., .F.,
 ( 4, 1, 4 ),
 ( 0.000000000000000000, 0.003752776749732567897, 0.007505553499465135794 ),
 .UNSPECIFIED. ) ;
#56782 = FACE_OUTER_BOUND ( 'NONE', #103559, .T. ) ;
#56783 = CIRCLE ( 'NONE', #10284, 2.000000000000001776 ) ;
#56784 = CARTESIAN_POINT ( 'NONE',  ( 34.12287332558704378, 18.64284798592593262, -17.67912453243325999 ) ) ;
#56785 = SURFACE_STYLE_FILL_AREA ( #22348 ) ;
#56786 = ORIENTED_EDGE ( 'NONE', *, *, #12563, .T. ) ;
#56787 = CARTESIAN_POINT ( 'NONE',  ( 7.188101187500001821, -29.56250000204838813, -2.977408999572650483 ) ) ;
#56788 = CARTESIAN_POINT ( 'NONE',  ( -10.93314270704077629, -14.00130306865723817, 31.84631742024726009 ) ) ;
#56789 = CARTESIAN_POINT ( 'NONE',  ( -37.62595466100675168, 491.2446780561949140, 12.18850516984412735 ) ) ;
#56790 = CARTESIAN_POINT ( 'NONE',  ( 0.000000000000000000, 0.000000000000000000, 0.000000000000000000 ) ) ;
#56791 = CARTESIAN_POINT ( 'NONE',  ( -9.843039827103245543, 88.59083502508335073, -1.781495459429540684 ) ) ;
#56792 = B_SPLINE_CURVE_WITH_KNOTS ( 'NONE', 3,
 ( #76647, #77192, #2758, #61561 ),
 .UNSPECIFIED., .F., .F.,
 ( 4, 4 ),
 ( 0.000000000000000000, 1.000000000000000000 ),
 .UNSPECIFIED. ) ;
#56793 = DIRECTION ( 'NONE',  ( -1.000000000000000000, -0.000000000000000000, -0.000000000000000000 ) ) ;
#56794 = PRODUCT_CONTEXT ( 'NONE', #71366, 'mechanical' ) ;
#56795 = CARTESIAN_POINT ( 'NONE',  ( -9.165151389911679658, 30.26319506294883510, 3.999999999999999112 ) ) ;
#56796 = EDGE_LOOP ( 'NONE', ( #53795, #24894 ) ) ;
#56797 = DIRECTION ( 'NONE',  ( -1.000000000000000000, -1.224606353822377258E-16, -0.000000000000000000 ) ) ;
#56798 = DIRECTION ( 'NONE',  ( -1.000000000000000000, -0.000000000000000000, -0.000000000000000000 ) ) ;
#56799 = FACE_OUTER_BOUND ( 'NONE', #15274, .T. ) ;
#56800 = CARTESIAN_POINT ( 'NONE',  ( 43.65977048856617415, -34.03584407960176605, -37.07728933806833993 ) ) ;
#56801 = DIRECTION ( 'NONE',  ( -1.000000000000000000, -1.224606353822377258E-16, -0.000000000000000000 ) ) ;
#56802 =( BOUNDED_SURFACE ( )  B_SPLINE_SURFACE ( 3, 2, ( 
 ( #19865, #37634, #19341 ),
 ( #52170, #3098, #64011 ),
 ( #104433, #31642, #22504 ),
 ( #89330, #7321, #6259 ),
 ( #47257, #79629, #96888 ),
 ( #23553, #23023, #30582 ),
 ( #46219, #13827, #15423 ),
 ( #79107, #62410, #13291 ),
 ( #38156, #14884, #31127 ),
 ( #56393, #5229, #46739 ) ),
 .UNSPECIFIED., .F., .F., .T. ) 
 B_SPLINE_SURFACE_WITH_KNOTS ( ( 4, 2, 2, 2, 4 ),
 ( 3, 3 ),
 ( 0.002450517525418897339, 0.003060732775749461232, 0.003670948026080025559, 0.004891378526741153344, 0.007332239528063409784 ),
 ( 0.000000000000000000, 1.000000000000000000 ),
 .UNSPECIFIED. ) 
 GEOMETRIC_REPRESENTATION_ITEM ( )  RATIONAL_B_SPLINE_SURFACE ( (
 ( 1.000000000000000000, 0.7071067811865481278, 1.000000000000000000),
 ( 1.000000000000000000, 0.7344063550101943560, 1.000000000000000000),
 ( 1.000000000000000000, 0.7590375248711014322, 1.000000000000000000),
 ( 1.000000000000000000, 0.8038331608704090137, 1.000000000000000000),
 ( 1.000000000000000000, 0.8240352460866353645, 1.000000000000000000),
 ( 1.000000000000000000, 0.8791017378332339760, 1.000000000000000000),
 ( 1.000000000000000000, 0.9085032776980893621, 1.000000000000000000),
 ( 1.000000000000000000, 0.9784170511696805850, 1.000000000000000000),
 ( 1.000000000000000000, 0.9996598051696602427, 1.000000000000000000),
 ( 1.000000000000000000, 1.000000000000000000, 1.000000000000000000) ) ) 
 REPRESENTATION_ITEM ( '' )  SURFACE ( )  );
#56803 =( NAMED_UNIT ( * ) SI_UNIT ( $, .STERADIAN. ) SOLID_ANGLE_UNIT ( ) );
#56804 = STYLED_ITEM ( 'NONE', ( #92681 ), #46117 ) ;
#56805 = ORIENTED_EDGE ( 'NONE', *, *, #69466, .F. ) ;
#56806 = AXIS2_PLACEMENT_3D ( 'NONE', #34826, #19714, #101114 ) ;
#56807 = DIRECTION ( 'NONE',  ( -1.000000000000000000, -1.224606353822377258E-16, -0.000000000000000000 ) ) ;
#56808 = CARTESIAN_POINT ( 'NONE',  ( 106.5779991752715148, -57.65217259572543895, 200.4557265301127984 ) ) ;
#56809 = ADVANCED_FACE ( 'NONE', ( #94818 ), #94004, .T. ) ;
#56810 = SURFACE_STYLE_FILL_AREA ( #7727 ) ;
#56811 = CARTESIAN_POINT ( 'NONE',  ( 3.586311574072714503, 16.06230210627474264, 6.012682668914248296 ) ) ;
#56812 =( NAMED_UNIT ( * ) PLANE_ANGLE_UNIT ( ) SI_UNIT ( $, .RADIAN. ) );
#56813 = CARTESIAN_POINT ( 'NONE',  ( 33.84761347220318584, 488.7471039746334895, 11.01988148152525504 ) ) ;
#56814 = CARTESIAN_POINT ( 'NONE',  ( -75.32987886060202243, -60.00000000000000711, 183.4819721636450254 ) ) ;
#56815 = CARTESIAN_POINT ( 'NONE',  ( -40.75641113481592726, 360.0948485545300741, 24.37153223514695100 ) ) ;
#56816 = DIRECTION ( 'NONE',  ( 0.000000000000000000, -1.000000000000000000, 0.000000000000000000 ) ) ;
#56817 =( GEOMETRIC_REPRESENTATION_CONTEXT ( 3 ) GLOBAL_UNCERTAINTY_ASSIGNED_CONTEXT ( ( #28948 ) ) GLOBAL_UNIT_ASSIGNED_CONTEXT ( ( #80219, #87807, #79696 ) ) REPRESENTATION_CONTEXT ( 'NONE', 'WORKASPACE' ) );
#56818 = CARTESIAN_POINT ( 'NONE',  ( -45.50145573691759182, 405.2496736015978627, 8.430338687477670234 ) ) ;
#56819 = B_SPLINE_CURVE_WITH_KNOTS ( 'NONE', 3,
 ( #20867, #68301, #3022, #35972, #3566, #93101, #101720, #35429, #36503, #102790, #11633, #44565, #44019, #101195, #52100, #94718, #27354, #53700, #61275, #86632, #60232, #100650, #85010, #51568, #76368, #11094, #53181, #86098, #69369, #68843, #60754, #12696, #12169, #102251 ),
 .UNSPECIFIED., .F., .F.,
 ( 4, 2, 2, 2, 2, 2, 2, 2, 2, 2, 2, 2, 2, 2, 2, 2, 4 ),
 ( 0.000000000000000000, 0.0007857361314144349846, 0.001571472262828869969, 0.002357208394243305062, 0.003142944525657739938, 0.003928680657072174814, 0.004714416788486610124, 0.005500152919901044567, 0.006285889051315479877, 0.007071625182729915186, 0.007857361314144349629, 0.008643097445558784939, 0.009428833576973220248, 0.01021456970838765556, 0.01100030583980208913, 0.01178604197121652444, 0.01257177810263095975 ),
 .UNSPECIFIED. ) ;
#56820 = CARTESIAN_POINT ( 'NONE',  ( -86.31808703902099467, -21.06115829967098918, 180.2389313303544895 ) ) ;
#56821 = ORIENTED_EDGE ( 'NONE', *, *, #8268, .F. ) ;
#56822 = CARTESIAN_POINT ( 'NONE',  ( 21.87703882378025710, 304.0646303204994751, -9.954777887710193340 ) ) ;
#56823 = MECHANICAL_DESIGN_GEOMETRIC_PRESENTATION_REPRESENTATION (  '', ( #93032 ), #98182 ) ;
#56824 = ORIENTED_EDGE ( 'NONE', *, *, #7044, .F. ) ;
#56826 = EDGE_CURVE ( 'NONE', #102396, #12309, #95704, .T. ) ;
#56825 = CARTESIAN_POINT ( 'NONE',  ( 16.05785784214673129, 4.775831776474256607, -3.710403933782447261 ) ) ;
#56827 = CARTESIAN_POINT ( 'NONE',  ( -6.457005523775564804, 41.52802923939503899, -70.63630686657118929 ) ) ;
#56828 = CARTESIAN_POINT ( 'NONE',  ( -83.13229060262131043, -37.80927313738316542, -3.002860636706784270 ) ) ;
#56829 = DIRECTION ( 'NONE',  ( -1.000000000000000000, -1.224606353822377258E-16, -0.000000000000000000 ) ) ;
#56830 = ORIENTED_EDGE ( 'NONE', *, *, #31632, .T. ) ;
#56831 = CARTESIAN_POINT ( 'NONE',  ( 27.85367641560119978, 36.60113970943790918, -7.793258884886260951 ) ) ;
#56832 = CARTESIAN_POINT ( 'NONE',  ( 12.50584327394879303, 22.74509139218984544, -5.893325311387099141 ) ) ;
#56833 = CARTESIAN_POINT ( 'NONE',  ( -4.453875240773214728, -1.734723475976807094E-15, -16.57301948837565675 ) ) ;
#56834 = CARTESIAN_POINT ( 'NONE',  ( -35.47684105139835253, 436.4843629120474588, 5.043999258399300523 ) ) ;
#56835 = AXIS2_PLACEMENT_3D ( 'NONE', #70428, #80087, #5160 ) ;
#56836 = CARTESIAN_POINT ( 'NONE',  ( -68.53940498225642841, -14.21045842199433729, -27.47940008941059276 ) ) ;
#56837 = CARTESIAN_POINT ( 'NONE',  ( -80.17676966763509938, -18.67864944542718675, 127.0877505495672466 ) ) ;
#56838 = EDGE_LOOP ( 'NONE', ( #47317, #105443, #41394, #72623, #2582, #40058 ) ) ;
#56839 = CARTESIAN_POINT ( 'NONE',  ( 7.151597709147950788, 86.78929265052215669, 3.587174531012138790 ) ) ;
#56840 = CARTESIAN_POINT ( 'NONE',  ( 90.12561416859028895, -57.66693923673333444, -22.18623277742999989 ) ) ;
#56841 = CARTESIAN_POINT ( 'NONE',  ( 27.26539850557486844, 34.42266064818549864, 10.05698433968570704 ) ) ;
#56842 = ADVANCED_FACE ( 'NONE', ( #86727 ), #46772, .F. ) ;
#56843 = EDGE_CURVE ( 'NONE', #26677, #79305, #49179, .T. ) ;
#56844 = AXIS2_PLACEMENT_3D ( 'NONE', #100611, #52588, #2443 ) ;
#56845 = DIRECTION ( 'NONE',  ( 0.5735764363510466035, -0.8191520442889914655, 1.003171929053524500E-16 ) ) ;
#56846 = VERTEX_POINT ( 'NONE', #5262 ) ;
#56847 = CARTESIAN_POINT ( 'NONE',  ( 0.000000000000000000, 0.000000000000000000, 0.000000000000000000 ) ) ;
#56848 = DIRECTION ( 'NONE',  ( 1.000000000000000000, 0.000000000000000000, 0.000000000000000000 ) ) ;
#56849 = CARTESIAN_POINT ( 'NONE',  ( 16.48304798889096290, 43.52978450323011117, 6.657797401561433404 ) ) ;
#56850 = CARTESIAN_POINT ( 'NONE',  ( 7.188101187499999156, -17.75000000204838457, 2.977408999572654924 ) ) ;
#56851 = CARTESIAN_POINT ( 'NONE',  ( 5.112021521199307195, -5.708827036476817440, -7.069802615102037890 ) ) ;
#56852 = CARTESIAN_POINT ( 'NONE',  ( 9.989285784994814676, 81.02657572554299747, 0.5301777604595927507 ) ) ;
#56853 = VERTEX_POINT ( 'NONE', #5779 ) ;
#56854 = CARTESIAN_POINT ( 'NONE',  ( 54.52222222222221859, 6.915964383211875250E-15, 0.000000000000000000 ) ) ;
#56855 = CARTESIAN_POINT ( 'NONE',  ( -8.000000000000001776, -13.34375000409676737, 3.313708498984759387 ) ) ;
#56856 = ORIENTED_EDGE ( 'NONE', *, *, #82338, .F. ) ;
#56857 = DIRECTION ( 'NONE',  ( 0.000000000000000000, 0.000000000000000000, -1.000000000000000000 ) ) ;
#56859 = CARTESIAN_POINT ( 'NONE',  ( 27.61403203557017250, -18.62762456134801070, 28.73031301232119716 ) ) ;
#56858 = CARTESIAN_POINT ( 'NONE',  ( -8.310099524471651122, -29.99999999999994316, 36.98670313214555705 ) ) ;
#56860 = DIRECTION ( 'NONE',  ( 0.000000000000000000, -1.000000000000000000, 0.000000000000000000 ) ) ;
#56861 = ORIENTED_EDGE ( 'NONE', *, *, #24359, .T. ) ;
#56862 = VERTEX_POINT ( 'NONE', #103940 ) ;
#56864 = CARTESIAN_POINT ( 'NONE',  ( 36.23800438212097674, 462.2863016840603336, 3.479460024273059560 ) ) ;
#56863 = DIRECTION ( 'NONE',  ( 0.000000000000000000, 1.000000000000000000, 0.000000000000000000 ) ) ;
#56865 = DIRECTION ( 'NONE',  ( 1.000000000000000000, 0.000000000000000000, -0.000000000000000000 ) ) ;
#56866 = LINE ( 'NONE', #1271, #41381 ) ;
#56867 = LINE ( 'NONE', #48771, #56949 ) ;
#56868 = DIRECTION ( 'NONE',  ( -0.000000000000000000, -0.000000000000000000, 1.000000000000000000 ) ) ;
#56869 = CYLINDRICAL_SURFACE ( 'NONE', #12479, 7.000000000000000000 ) ;
#56870 = ORIENTED_EDGE ( 'NONE', *, *, #3671, .F. ) ;
#56871 = CARTESIAN_POINT ( 'NONE',  ( 65.88819888065104635, -59.99999999999998579, -33.92666894943724287 ) ) ;
#56872 = CARTESIAN_POINT ( 'NONE',  ( -9.443129677144035838, 46.21199370134087303, 13.23108103747117070 ) ) ;
#56873 = CARTESIAN_POINT ( 'NONE',  ( 30.00000000000000000, 464.2362426119078691, 15.22860355415621925 ) ) ;
#56874 = CARTESIAN_POINT ( 'NONE',  ( 76.76915258873057724, -30.00000000000000711, -16.81647129862127699 ) ) ;
#56875 = CARTESIAN_POINT ( 'NONE',  ( 18.71538461538461462, -4.171999999999999709, 5.616230220889763424E-16 ) ) ;
#56876 = ORIENTED_EDGE ( 'NONE', *, *, #41468, .T. ) ;
#56877 = STYLED_ITEM ( 'NONE', ( #43224 ), #46730 ) ;
#56878 = VERTEX_POINT ( 'NONE', #103421 ) ;
#56879 = EDGE_LOOP ( 'NONE', ( #32881, #57262, #47753, #1924 ) ) ;
#56880 = DIRECTION ( 'NONE',  ( -0.4804656623126268844, -0.6318279369468200457, -0.6082320325599548383 ) ) ;
#56881 = CARTESIAN_POINT ( 'NONE',  ( 44.19369980509995344, 485.2130927455154961, 1.003348617673237131 ) ) ;
#56882 =( NAMED_UNIT ( * ) PLANE_ANGLE_UNIT ( ) SI_UNIT ( $, .RADIAN. ) );
#56883 = CARTESIAN_POINT ( 'NONE',  ( 33.15568924549393870, 409.3318216629285757, 25.92143113850746872 ) ) ;
#56884 = CARTESIAN_POINT ( 'NONE',  ( -34.91408493170087013, 321.8851433098943744, -5.358867272492853218 ) ) ;
#56885 = CARTESIAN_POINT ( 'NONE',  ( -3.693992608460733074, -68.08033126016331948, 13.10824594383253050 ) ) ;
#56886 = CARTESIAN_POINT ( 'NONE',  ( -46.00000000000003553, 486.3928777044199592, 3.761659546714874125 ) ) ;
#56887 =( NAMED_UNIT ( * ) PLANE_ANGLE_UNIT ( ) SI_UNIT ( $, .RADIAN. ) );
#56889 = ORIENTED_EDGE ( 'NONE', *, *, #2572, .T. ) ;
#56888 = AXIS2_PLACEMENT_3D ( 'NONE', #88269, #79101, #5225 ) ;
#56890 = CARTESIAN_POINT ( 'NONE',  ( 29.68315524077034340, 13.12249633091093415, 39.60535821593451544 ) ) ;
#56891 = ORIENTED_EDGE ( 'NONE', *, *, #52910, .F. ) ;
#56892 = DIRECTION ( 'NONE',  ( 0.000000000000000000, -1.000000000000000000, 0.000000000000000000 ) ) ;
#56893 = FACE_OUTER_BOUND ( 'NONE', #11181, .T. ) ;
#56894 = CARTESIAN_POINT ( 'NONE',  ( -71.97080448170594025, -59.99999999999997158, 122.5097884546718490 ) ) ;
#56895 = CARTESIAN_POINT ( 'NONE',  ( 67.15832716194654495, -22.10445124349199020, 83.33801890902627463 ) ) ;
#56896 = EDGE_LOOP ( 'NONE', ( #66497, #12941, #77117, #75542 ) ) ;
#56897 = AXIS2_PLACEMENT_3D ( 'NONE', #82770, #27238, #101620 ) ;
#56898 = CARTESIAN_POINT ( 'NONE',  ( 39.12903940704961769, 38.95383793072134182, 50.91589357078481726 ) ) ;
#56899 = ADVANCED_FACE ( 'NONE', ( #71048 ), #19987, .T. ) ;
#56900 = CARTESIAN_POINT ( 'NONE',  ( 0.5805565836007701153, -7.505553499465148271, -1.383738442504732931E-16 ) ) ;
#56901 = AXIS2_PLACEMENT_3D ( 'NONE', #9919, #34773, #20199 ) ;
#56902 = ADVANCED_FACE ( 'NONE', ( #73692, #80189, #72634 ), #16000, .T. ) ;
#56903 = CARTESIAN_POINT ( 'NONE',  ( -2.836400373815510800, -57.67120205560058110, -44.61166178099613688 ) ) ;
#56904 = B_SPLINE_CURVE_WITH_KNOTS ( 'NONE', 3,
 ( #73871, #16167, #65257, #72800, #49053, #66316, #81949, #32386, #1004, #82504 ),
 .UNSPECIFIED., .F., .F.,
 ( 4, 2, 2, 2, 4 ),
 ( 0.000000000000000000, 0.001993803085173304328, 0.003987606170346608657, 0.005981409255519914286, 0.007975212340693219049 ),
 .UNSPECIFIED. ) ;
#56905 = ORIENTED_EDGE ( 'NONE', *, *, #47791, .F. ) ;
#56906 = CIRCLE ( 'NONE', #105120, 4.000000000000001776 ) ;
#56907 = CARTESIAN_POINT ( 'NONE',  ( 37.38561277374697056, 1.340359594676612611E-15, 0.000000000000000000 ) ) ;
#56908 = CARTESIAN_POINT ( 'NONE',  ( 17.33349330513380693, 4.000000000000002665, 0.000000000000000000 ) ) ;
#56909 = AXIS2_PLACEMENT_3D ( 'NONE', #46545, #54606, #30385 ) ;
#56910 = CARTESIAN_POINT ( 'NONE',  ( -5.656854249492381470, -29.75000000409677270, 5.656854249492379694 ) ) ;
#56911 = CARTESIAN_POINT ( 'NONE',  ( 7.137815226410046066, -3.000000000000000000, 4.175893272574714210 ) ) ;
#56912 = DIRECTION ( 'NONE',  ( 1.096832036894112098E-16, -0.000000000000000000, 1.000000000000000000 ) ) ;
#56913 = FILL_AREA_STYLE_COLOUR ( '', #11978 ) ;
#56914 = CARTESIAN_POINT ( 'NONE',  ( -6.067394940365958611, 4.399108099114772408, 5.000000000000000888 ) ) ;
#56915 = FACE_OUTER_BOUND ( 'NONE', #30806, .T. ) ;
#56916 =( LENGTH_UNIT ( ) NAMED_UNIT ( * ) SI_UNIT ( .MILLI., .METRE. ) );
#56917 = FILL_AREA_STYLE ('',( #90365 ) ) ;
#56918 = ORIENTED_EDGE ( 'NONE', *, *, #64914, .F. ) ;
#56919 = DIRECTION ( 'NONE',  ( -0.7071067811865555663, 0.000000000000000000, 0.7071067811865393571 ) ) ;
#56920 = CARTESIAN_POINT ( 'NONE',  ( 2.377971153322278042E-07, -60.00000000000000000, 39.63907915656436387 ) ) ;
#56921 = CARTESIAN_POINT ( 'NONE',  ( -98.87062525871608898, -29.99999999999999289, 189.1229995020886179 ) ) ;
#56922 = CARTESIAN_POINT ( 'NONE',  ( -39.67558661318489044, 485.2175335192594048, -4.383050085588370059 ) ) ;
#56923 = CARTESIAN_POINT ( 'NONE',  ( 45.36739251505076709, -57.68277139381120122, 65.96562024646243572 ) ) ;
#56924 = VECTOR ( 'NONE', #9167, 999.9999999999998863 ) ;
#56926 = CARTESIAN_POINT ( 'NONE',  ( -9.170934695443028417, 53.73492620751849813, 1.679349929019868570 ) ) ;
#56925 = CARTESIAN_POINT ( 'NONE',  ( 3.313708498984761608, -15.40625000409677092, -8.000000000000000000 ) ) ;
#56927 = EDGE_CURVE ( 'NONE', #77149, #19064, #946, .T. ) ;
#56928 = CARTESIAN_POINT ( 'NONE',  ( -38.83413156602095739, 459.9242647137451740, 1.954013010003036621 ) ) ;
#56929 = VECTOR ( 'NONE', #63013, 1000.000000000000000 ) ;
#56930 =( LENGTH_UNIT ( ) NAMED_UNIT ( * ) SI_UNIT ( .MILLI., .METRE. ) );
#56931 = UNCERTAINTY_MEASURE_WITH_UNIT (LENGTH_MEASURE( 1.000000000000000082E-05 ), #49252, 'distance_accuracy_value', 'NONE');
#56932 = CARTESIAN_POINT ( 'NONE',  ( 26.69900261086841198, 3.851859888774471706E-31, 5.000000000000001776 ) ) ;
#56933 = CARTESIAN_POINT ( 'NONE',  ( -8.458412064297640143, -60.00000000000000000, 39.63599595626720884 ) ) ;
#56934 = CARTESIAN_POINT ( 'NONE',  ( 12.43927466310973173, 9.603553788038196259, 9.411862679792397657 ) ) ;
#56935 = CARTESIAN_POINT ( 'NONE',  ( 5.622453258321459479, 53.42013071948692016, 8.498021148331359242 ) ) ;
#56936 = CARTESIAN_POINT ( 'NONE',  ( -87.09125453590827703, -35.39906969241756229, 188.3565598345231251 ) ) ;
#56937 = ORIENTED_EDGE ( 'NONE', *, *, #14823, .T. ) ;
#56938 = CARTESIAN_POINT ( 'NONE',  ( 17.50000000000007105, 48.00000000000682832, 64.09945636502658317 ) ) ;
#56939 = CARTESIAN_POINT ( 'NONE',  ( 8.091997990208083635, -14.49474307880116086, 15.56218444166430892 ) ) ;
#56940 = CARTESIAN_POINT ( 'NONE',  ( -5.993894117748983952, -22.06774329507786447, 27.55811915394870226 ) ) ;
#56941 = CARTESIAN_POINT ( 'NONE',  ( 0.05533025579362507718, -4.993776679985868050, -4.350525068611865720 ) ) ;
#56944 = ADVANCED_FACE ( 'NONE', ( #39234 ), #83778, .T. ) ;
#56943 = CARTESIAN_POINT ( 'NONE',  ( 4.999999999999524825, -61.74609737454713354, 12.75775085714972690 ) ) ;
#56942 = SPHERICAL_SURFACE ( 'NONE', #91343, 1.000000000000000000 ) ;
#56945 = EDGE_CURVE ( 'NONE', #84380, #38837, #61312, .T. ) ;
#56946 = ORIENTED_EDGE ( 'NONE', *, *, #40476, .T. ) ;
#56947 = CONICAL_SURFACE ( 'NONE', #53590, 4.172000000000001485, 0.9599310885968750373 ) ;
#56948 = PLANE ( 'NONE',  #52501 ) ;
#56949 = VECTOR ( 'NONE', #7786, 999.9999999999998863 ) ;
#56950 = CARTESIAN_POINT ( 'NONE',  ( -6.618366600633001084, -4.380080200176828420, -16.79229307443615582 ) ) ;
#56951 = CARTESIAN_POINT ( 'NONE',  ( 15.73414724454982583, 35.06317813786103699, 22.31186484002455472 ) ) ;
#56952 = CARTESIAN_POINT ( 'NONE',  ( 28.99461337544303774, 306.6923402040300175, -9.137068254448493576 ) ) ;
#56953 = FACE_BOUND ( 'NONE', #9216, .T. ) ;
#56954 =( NAMED_UNIT ( * ) PLANE_ANGLE_UNIT ( ) SI_UNIT ( $, .RADIAN. ) );
#56955 = CARTESIAN_POINT ( 'NONE',  ( 72.91237123256428276, -60.00000000000000000, 161.6570857422749157 ) ) ;
#56956 = DIRECTION ( 'NONE',  ( -1.000000000000000000, -0.000000000000000000, -0.000000000000000000 ) ) ;
#56957 = EDGE_LOOP ( 'NONE', ( #5729, #64221, #80229, #15265, #97695, #86184 ) ) ;
#56958 = CARTESIAN_POINT ( 'NONE',  ( -4.681884270554226291, -29.99999999999996803, 5.894723978655478369 ) ) ;
#56959 = CARTESIAN_POINT ( 'NONE',  ( -9.918512371096326774, 253.7928299227055220, -1.297150762882672614 ) ) ;
#56960 = DIRECTION ( 'NONE',  ( 0.000000000000000000, 1.000000000000000000, -0.000000000000000000 ) ) ;
#56961 = DIRECTION ( 'NONE',  ( -1.000000000000000000, -1.224606353822377258E-16, -0.000000000000000000 ) ) ;
#56962 =( BOUNDED_SURFACE ( )  B_SPLINE_SURFACE ( 3, 2, ( 
 ( #77484, #20897, #28429 ),
 ( #20368, #55306, #97360 ),
 ( #79070, #62377, #15387 ),
 ( #22462, #96334, #23514 ),
 ( #56357, #21397, #88233 ),
 ( #14313, #47217, #38631 ),
 ( #80118, #39158, #103864 ),
 ( #54235, #62900, #105466 ),
 ( #40192, #95267, #89293 ),
 ( #39687, #87175, #73069 ),
 ( #5705, #6221, #30014 ),
 ( #63968, #31606, #72039 ),
 ( #5190, #55818, #46178 ),
 ( #104947, #13256, #31089 ) ),
 .UNSPECIFIED., .F., .F., .T. ) 
 B_SPLINE_SURFACE_WITH_KNOTS ( ( 4, 2, 2, 2, 2, 2, 4 ),
 ( 3, 3 ),
 ( -1.455432996344541152E-15, 0.001037790322795861028, 0.001556685484194519258, 0.002075580645593177488, 0.002594475806991835935, 0.003113370968390493949, 0.004151161291187810409 ),
 ( 0.000000000000000000, 1.000000000000000000 ),
 .UNSPECIFIED. ) 
 GEOMETRIC_REPRESENTATION_ITEM ( )  RATIONAL_B_SPLINE_SURFACE ( (
 ( 1.000000000000000000, 0.8266506655094397749, 1.000000000000000000),
 ( 1.000000000000000000, 0.8403402121237507627, 1.000000000000000000),
 ( 1.000000000000000000, 0.8527375874848021065, 1.000000000000000000),
 ( 1.000000000000000000, 0.8685816477878300912, 1.000000000000000000),
 ( 1.000000000000000000, 0.8733924426121236761, 1.000000000000000000),
 ( 1.000000000000000000, 0.8815965360754977054, 1.000000000000000000),
 ( 1.000000000000000000, 0.8850417602709202969, 1.000000000000000000),
 ( 1.000000000000000000, 0.8904811663259585286, 1.000000000000000000),
 ( 1.000000000000000000, 0.8924856662908452476, 1.000000000000000000),
 ( 1.000000000000000000, 0.8947492012711196763, 1.000000000000000000),
 ( 1.000000000000000000, 0.8950270886643441060, 1.000000000000000000),
 ( 1.000000000000000000, 0.8933353874821594598, 1.000000000000000000),
 ( 1.000000000000000000, 0.8887179207565071293, 1.000000000000000000),
 ( 1.000000000000000000, 0.8812198548863955372, 1.000000000000000000) ) ) 
 REPRESENTATION_ITEM ( '' )  SURFACE ( )  );
#56963 = CARTESIAN_POINT ( 'NONE',  ( 0.000000000000000000, 45.00000000000000711, 65.00000000000000000 ) ) ;
#56964 = EDGE_CURVE ( 'NONE', #62284, #11843, #68133, .T. ) ;
#56965 = ORIENTED_EDGE ( 'NONE', *, *, #94152, .T. ) ;
#56966 = UNCERTAINTY_MEASURE_WITH_UNIT (LENGTH_MEASURE( 1.000000000000000082E-05 ), #69042, 'distance_accuracy_value', 'NONE');
#56967 = VECTOR ( 'NONE', #49244, 1000.000000000000341 ) ;
#56968 = CONICAL_SURFACE ( 'NONE', #13934, 4.000000000000001776, 0.9599310885968808105 ) ;
#56969 = CARTESIAN_POINT ( 'NONE',  ( -23.33774967493778263, 304.7266520059388881, 10.12724404418439939 ) ) ;
#56970 = VERTEX_POINT ( 'NONE', #106050 ) ;
#56971 = CARTESIAN_POINT ( 'NONE',  ( 38.08399829462226904, 485.5430321159580558, -4.039315524879443231 ) ) ;
#56973 = EDGE_CURVE ( 'NONE', #22823, #37408, #88849, .T. ) ;
#56972 = SURFACE_SIDE_STYLE ('',( #99021 ) ) ;
#56974 = DIRECTION ( 'NONE',  ( -0.7611201562154610301, 0.000000000000000000, -0.6486109063240860229 ) ) ;
#56975 = CYLINDRICAL_SURFACE ( 'NONE', #105269, 4.000000000000000000 ) ;
#56976 = ORIENTED_EDGE ( 'NONE', *, *, #97659, .F. ) ;
#56977 = CARTESIAN_POINT ( 'NONE',  ( 55.22048556082879145, 50.00000000002004441, 34.80214219306057544 ) ) ;
#56978 = CARTESIAN_POINT ( 'NONE',  ( -57.54921171551777093, -59.99999999998048139, 100.4542084673178408 ) ) ;
#56979 = CIRCLE ( 'NONE', #29484, 5.000000000000001776 ) ;
#56980 = CARTESIAN_POINT ( 'NONE',  ( 45.99999999999995026, 436.1515134926989390, 9.232507626554589564 ) ) ;
#56981 = CARTESIAN_POINT ( 'NONE',  ( 78.09062726087394424, -59.99999999999997158, 193.0367330576344784 ) ) ;
#56983 = CARTESIAN_POINT ( 'NONE',  ( 15.83979721888547409, -49.91555666069991304, 32.40126087659623977 ) ) ;
#56982 = CARTESIAN_POINT ( 'NONE',  ( -114.0148073962512854, -59.99999999999994316, 183.4850465800912218 ) ) ;
#56984 = CARTESIAN_POINT ( 'NONE',  ( 101.2009270926939450, -38.00000000000001421, 187.7194746866334185 ) ) ;
#56985 = CARTESIAN_POINT ( 'NONE',  ( 0.5686146804203622285, 53.44061092886668973, -10.11633179230661206 ) ) ;
#56986 = CARTESIAN_POINT ( 'NONE',  ( -46.21137058018805277, -25.69989330234890801, 41.24333236953626169 ) ) ;
#56987 = AXIS2_PLACEMENT_3D ( 'NONE', #83179, #26586, #42725 ) ;
#56988 = DIRECTION ( 'NONE',  ( 0.000000000000000000, -1.000000000000000000, 0.000000000000000000 ) ) ;
#56989 = ORIENTED_EDGE ( 'NONE', *, *, #7455, .F. ) ;
#56990 = EDGE_CURVE ( 'NONE', #94292, #41603, #89369, .T. ) ;
#56991 =( NAMED_UNIT ( * ) SI_UNIT ( $, .STERADIAN. ) SOLID_ANGLE_UNIT ( ) );
#56992 = CARTESIAN_POINT ( 'NONE',  ( 16.10155864910916534, 21.86284619731734935, 0.4346306502230241620 ) ) ;
#56993 = CARTESIAN_POINT ( 'NONE',  ( 40.85254446136673323, 441.7500193615117610, 25.53625856138344474 ) ) ;
#56994 = DIRECTION ( 'NONE',  ( 0.000000000000000000, 0.000000000000000000, 1.000000000000000000 ) ) ;
#56995 = CYLINDRICAL_SURFACE ( 'NONE', #82639, 5.000000000000002665 ) ;
#56996 = CARTESIAN_POINT ( 'NONE',  ( 31.03867016165222026, 468.3124986733989772, 18.90871194958903345 ) ) ;
#56997 = ORIENTED_EDGE ( 'NONE', *, *, #37721, .F. ) ;
#56998 = EDGE_CURVE ( 'NONE', #87270, #58778, #99139, .T. ) ;
#56999 = B_SPLINE_CURVE_WITH_KNOTS ( 'NONE', 3,
 ( #6069, #22299, #95110, #88598, #97204, #29339 ),
 .UNSPECIFIED., .F., .F.,
 ( 4, 2, 4 ),
 ( 0.000000000000000000, 0.0003352299596267559732, 0.0006704599192535119464 ),
 .UNSPECIFIED. ) ;
#57000 = ORIENTED_EDGE ( 'NONE', *, *, #15030, .F. ) ;
#57001 = CARTESIAN_POINT ( 'NONE',  ( 106.8088085084784780, -30.00000000000934719, 192.1296079279642584 ) ) ;
#57002 = CARTESIAN_POINT ( 'NONE',  ( 47.14858110737401375, 13.36679009520640093, 14.71571165017371463 ) ) ;
#57003 = EDGE_CURVE ( 'NONE', #6290, #28486, #55892, .T. ) ;
#57004 = DIRECTION ( 'NONE',  ( 0.000000000000000000, 0.000000000000000000, -1.000000000000000000 ) ) ;
#57005 = SURFACE_STYLE_FILL_AREA ( #30649 ) ;
#57006 = CARTESIAN_POINT ( 'NONE',  ( 97.88916531341952521, -30.00000000000000000, 136.7528328087380203 ) ) ;
#57007 = CARTESIAN_POINT ( 'NONE',  ( 7.150053860865848598, 103.2173454608602299, 3.590189269391292015 ) ) ;
#57008 = VERTEX_POINT ( 'NONE', #6835 ) ;
#57009 = VECTOR ( 'NONE', #54553, 1000.000000000000000 ) ;
#57010 = ORIENTED_EDGE ( 'NONE', *, *, #49451, .T. ) ;
#57011 = ORIENTED_EDGE ( 'NONE', *, *, #2264, .F. ) ;
#57012 = DIRECTION ( 'NONE',  ( 0.000000000000000000, 0.000000000000000000, 1.000000000000000000 ) ) ;
#57013 = LINE ( 'NONE', #23627, #26666 ) ;
#57014 = AXIS2_PLACEMENT_3D ( 'NONE', #14265, #39107, #47694 ) ;
#57015 = DIRECTION ( 'NONE',  ( 0.000000000000000000, 0.000000000000000000, 1.000000000000000000 ) ) ;
#57016 = EDGE_LOOP ( 'NONE', ( #45518, #33070, #10054, #35435 ) ) ;
#57017 = CARTESIAN_POINT ( 'NONE',  ( 56.96666666666666856, -3.309500000000000774, 4.475777889183797681E-16 ) ) ;
#57018 = ORIENTED_EDGE ( 'NONE', *, *, #37366, .T. ) ;
#57019 = CARTESIAN_POINT ( 'NONE',  ( 0.000000000000000000, 0.000000000000000000, 0.000000000000000000 ) ) ;
#57020 = CARTESIAN_POINT ( 'NONE',  ( 81.85842773695857488, -38.84088539656383432, 195.7169493522233950 ) ) ;
#57021 = CARTESIAN_POINT ( 'NONE',  ( 11.99918652032940436, 8.156082305580584446, 8.762798087422753568 ) ) ;
#57022 = CARTESIAN_POINT ( 'NONE',  ( 36.73804107120987794, 310.3495191438393022, 13.65122708957765241 ) ) ;
#57023 = FILL_AREA_STYLE_COLOUR ( '', #35009 ) ;
#57024 = CARTESIAN_POINT ( 'NONE',  ( 0.5805565836007650082, -3.752776749732574135, -6.500000000000001776 ) ) ;
#57025 = CARTESIAN_POINT ( 'NONE',  ( -27.26426147078658602, 34.70249704477448205, -7.556984339685874019 ) ) ;
#57026 = CARTESIAN_POINT ( 'NONE',  ( -4.902312018371808300, -46.91782384206801737, 103.3400275729950550 ) ) ;
#57027 = EDGE_CURVE ( 'NONE', #96238, #30181, #105536, .T. ) ;
#57028 = CARTESIAN_POINT ( 'NONE',  ( 32.68253575351396023, 486.6530702916748510, 8.413834116604476776 ) ) ;
#57029 =( GEOMETRIC_REPRESENTATION_CONTEXT ( 3 ) GLOBAL_UNCERTAINTY_ASSIGNED_CONTEXT ( ( #43003 ) ) GLOBAL_UNIT_ASSIGNED_CONTEXT ( ( #26301, #42429, #11647 ) ) REPRESENTATION_CONTEXT ( 'NONE', 'WORKASPACE' ) );
#57030 = CARTESIAN_POINT ( 'NONE',  ( -4.484401894551007572, 9.375573132718574954, 5.000000000000000888 ) ) ;
#57031 = ORIENTED_EDGE ( 'NONE', *, *, #45167, .T. ) ;
#57032 = CARTESIAN_POINT ( 'NONE',  ( 1.461497756933666903, -49.97255764215042717, 101.6363431123547798 ) ) ;
#57034 = CARTESIAN_POINT ( 'NONE',  ( -19.96162532426522773, 302.8116070918645164, 9.928455558879878851 ) ) ;
#57033 = DIRECTION ( 'NONE',  ( 0.000000000000000000, 0.000000000000000000, 1.000000000000000000 ) ) ;
#57035 = SURFACE_SIDE_STYLE ('',( #18214 ) ) ;
#57036 = UNCERTAINTY_MEASURE_WITH_UNIT (LENGTH_MEASURE( 1.000000000000000082E-05 ), #22561, 'distance_accuracy_value', 'NONE');
#57037 = CARTESIAN_POINT ( 'NONE',  ( -8.000000000000000000, -14.74999999999999289, -9.797174393178825657E-16 ) ) ;
#57038 = CARTESIAN_POINT ( 'NONE',  ( 32.89005191666632300, -34.30586786915193187, 42.46426960025681296 ) ) ;
#57039 = ADVANCED_FACE ( 'NONE', ( #15459 ), #1030, .T. ) ;
#57040 = CARTESIAN_POINT ( 'NONE',  ( 6.962581867957212012, 296.7069905224671515, 7.199939672562493342 ) ) ;
#57041 = ORIENTED_EDGE ( 'NONE', *, *, #103892, .F. ) ;
#57042 = CARTESIAN_POINT ( 'NONE',  ( 83.81614971311275042, -53.76474988997830451, 188.4634654509657707 ) ) ;
#57043 = CARTESIAN_POINT ( 'NONE',  ( 0.07794078601782293558, 18.87382441218279538, 49.24999999999998579 ) ) ;
#57044 = CARTESIAN_POINT ( 'NONE',  ( -9.433863490721467571, 141.8798491995649442, -6.333282113655117596E-13 ) ) ;
#57045 = ORIENTED_EDGE ( 'NONE', *, *, #95812, .T. ) ;
#57046 = CARTESIAN_POINT ( 'NONE',  ( 90.98197251250333295, -57.66404948542993480, -20.95280514685850193 ) ) ;
#57047 = CIRCLE ( 'NONE', #65691, 5.000000000000002665 ) ;
#57048 = CARTESIAN_POINT ( 'NONE',  ( 34.88259098417261583, 437.7046102974892960, 4.606877878020303463 ) ) ;
#57049 = PRESENTATION_STYLE_ASSIGNMENT (( #106128 ) ) ;
#57050 = CARTESIAN_POINT ( 'NONE',  ( 28.77610217197986486, 13.65956388957901524, 39.99200581488069872 ) ) ;
#57051 = AXIS2_PLACEMENT_3D ( 'NONE', #25515, #24454, #8221 ) ;
#57052 = CARTESIAN_POINT ( 'NONE',  ( -81.36109053512349476, -30.00000000000000711, -1.390147020584881155 ) ) ;
#57053 = EDGE_CURVE ( 'NONE', #13222, #88217, #24128, .T. ) ;
#57054 = CIRCLE ( 'NONE', #74230, 5.000000000000002665 ) ;
#57055 = CARTESIAN_POINT ( 'NONE',  ( 28.45500467043821047, 17.07616014098844559, 41.11859397474279376 ) ) ;
#57056 = AXIS2_PLACEMENT_3D ( 'NONE', #52202, #28502, #19371 ) ;
#57057 = CARTESIAN_POINT ( 'NONE',  ( -7.137815226412437930, -4.999999999998865796, -4.175893272574592530 ) ) ;
#57058 = CARTESIAN_POINT ( 'NONE',  ( 20.00100000000000477, 12.99999999999999289, 10.00000000000000178 ) ) ;
#57060 = CARTESIAN_POINT ( 'NONE',  ( -7.500000000000000000, 4.330127018922188320, -7.422398894150033399 ) ) ;
#57059 = DIRECTION ( 'NONE',  ( 0.000000000000000000, 0.000000000000000000, 1.000000000000000000 ) ) ;
#57061 = MECHANICAL_DESIGN_GEOMETRIC_PRESENTATION_REPRESENTATION (  '', ( #58792 ), #67414 ) ;
#57062 = ADVANCED_FACE ( 'NONE', ( #85945 ), #42800, .T. ) ;
#57063 = FACE_OUTER_BOUND ( 'NONE', #64474, .T. ) ;
#57064 = CARTESIAN_POINT ( 'NONE',  ( -12.50000000000000178, -3.000000000000000000, -34.12705337366766400 ) ) ;
#57065 = CARTESIAN_POINT ( 'NONE',  ( 11.99986829839165203, -5.000000000000000000, -83.40936345626406023 ) ) ;
#57066 = CARTESIAN_POINT ( 'NONE',  ( -10.58321096220334034, -23.34997317828527841, -30.52089866259334272 ) ) ;
#57067 =( LENGTH_UNIT ( ) NAMED_UNIT ( * ) SI_UNIT ( .MILLI., .METRE. ) );
#57068 = CARTESIAN_POINT ( 'NONE',  ( 65.16637633022084231, -29.76141079654699695, -22.99752254794697137 ) ) ;
#57069 = ORIENTED_EDGE ( 'NONE', *, *, #51719, .T. ) ;
#57070 = CARTESIAN_POINT ( 'NONE',  ( -6.419907845689960091, -0.01065582494818990457, 18.86296154573671657 ) ) ;
#57071 = CARTESIAN_POINT ( 'NONE',  ( 32.33349330513379982, 1.593028355512270567E-15, 0.000000000000000000 ) ) ;
#57072 = CARTESIAN_POINT ( 'NONE',  ( -7.551560007654695816, 81.99089648193009339, -2.648022159607839043 ) ) ;
#57073 = CARTESIAN_POINT ( 'NONE',  ( -35.05577973701957717, -23.33692852230415582, -31.27659717426585573 ) ) ;
#57076 = EDGE_CURVE ( 'NONE', #86829, #45464, #37217, .T. ) ;
#57075 = CARTESIAN_POINT ( 'NONE',  ( -25.26744833228682197, -34.58977355993737746, -31.36978027168452954 ) ) ;
#57074 = CARTESIAN_POINT ( 'NONE',  ( 5.290067270632397012, 54.20842449845690680, 6.031152949374294359 ) ) ;
#57077 = VERTEX_POINT ( 'NONE', #59535 ) ;
#57078 = AXIS2_PLACEMENT_3D ( 'NONE', #69588, #102478, #28624 ) ;
#57079 = ORIENTED_EDGE ( 'NONE', *, *, #39815, .F. ) ;
#57080 = LINE ( 'NONE', #106697, #20805 ) ;
#57081 = VECTOR ( 'NONE', #31303, 1000.000000000000000 ) ;
#57082 = CARTESIAN_POINT ( 'NONE',  ( 13.37207953394533355, 1.482358050883964840E-15, 0.000000000000000000 ) ) ;
#57083 = CIRCLE ( 'NONE', #39863, 4.250000000000000000 ) ;
#57084 = CARTESIAN_POINT ( 'NONE',  ( -85.63645619683279619, -59.99999999999998579, -24.02817151352510194 ) ) ;
#57085 = ORIENTED_EDGE ( 'NONE', *, *, #77436, .T. ) ;
#57086 = FACE_OUTER_BOUND ( 'NONE', #97487, .T. ) ;
#57087 = CARTESIAN_POINT ( 'NONE',  ( 11.31153846153846132, 4.172000000000003261, 0.000000000000000000 ) ) ;
#57088 = CARTESIAN_POINT ( 'NONE',  ( 99.94366276826657725, -60.30227360360919420, 195.8446303873824945 ) ) ;
#57090 = LINE ( 'NONE', #58714, #104616 ) ;
#57089 = DIRECTION ( 'NONE',  ( -1.000000000000000000, 0.000000000000000000, 0.000000000000000000 ) ) ;
#57091 = EDGE_LOOP ( 'NONE', ( #40091, #60390, #55886, #104061, #19365 ) ) ;
#57092 = EDGE_LOOP ( 'NONE', ( #78170, #29251, #55513, #2349, #17537, #73550 ) ) ;
#57093 = ORIENTED_EDGE ( 'NONE', *, *, #88027, .F. ) ;
#57095 =( BOUNDED_CURVE ( )  B_SPLINE_CURVE ( 2, ( #60057, #27704, #20689, #12517, #92913, #2838, #19080, #51917, #75665 ),
 .UNSPECIFIED., .F., .T. ) 
 B_SPLINE_CURVE_WITH_KNOTS ( ( 3, 2, 2, 2, 3 ),
 ( 0.3382352941176470229, 0.3455882352941175850, 0.3529411764705882026, 0.3602941176470588203, 0.3676470588235294379 ),
 .UNSPECIFIED. ) 
 CURVE ( )  GEOMETRIC_REPRESENTATION_ITEM ( )  RATIONAL_B_SPLINE_CURVE ( ( 1.000000000000000666, 0.9238795325112861834, 1.000000000000000000, 0.9238795325112867385, 1.000000000000000000, 0.9238795325112867385, 1.000000000000000000, 0.9238795325112867385, 1.000000000000000000 ) ) 
 REPRESENTATION_ITEM ( '' )  );
#57094 = CARTESIAN_POINT ( 'NONE',  ( 30.15836800272330365, 323.6799505684332985, 14.82125230496755641 ) ) ;
#57096 = EDGE_CURVE ( 'NONE', #82432, #75817, #3942, .T. ) ;
#57097 = CARTESIAN_POINT ( 'NONE',  ( -6.249254171365509869, -12.00724809824330386, 11.39149369527972766 ) ) ;
#57098 = CARTESIAN_POINT ( 'NONE',  ( 25.11650669486618881, 1.474610560812782335E-15, 0.000000000000000000 ) ) ;
#57099 = ORIENTED_EDGE ( 'NONE', *, *, #52609, .F. ) ;
#57100 = FACE_OUTER_BOUND ( 'NONE', #85535, .T. ) ;
#57101 = CARTESIAN_POINT ( 'NONE',  ( 0.000000000000000000, -30.00000000000000000, 0.000000000000000000 ) ) ;
#57102 = CARTESIAN_POINT ( 'NONE',  ( 9.090909090909088164, 16.00000000000000000, 4.165977904505314910 ) ) ;
#57103 = CARTESIAN_POINT ( 'NONE',  ( -21.50832034731008591, -57.67247026516260178, 42.43288772392129715 ) ) ;
#57104 = CARTESIAN_POINT ( 'NONE',  ( -5.082755093536325042, -30.59375000204838813, -5.082755093536325930 ) ) ;
#57105 = CARTESIAN_POINT ( 'NONE',  ( -30.42537733501908548, 12.90981014178662001, 41.86413436173241820 ) ) ;
#57106 = LINE ( 'NONE', #47425, #95939 ) ;
#57107 = DIRECTION ( 'NONE',  ( -1.000000000000000000, -1.224606353822377258E-16, -0.000000000000000000 ) ) ;
#57108 = CARTESIAN_POINT ( 'NONE',  ( -79.45587154498480231, -59.99999999999991473, -31.00068500363164858 ) ) ;
#57109 = ADVANCED_FACE ( 'NONE', ( #53022 ), #9675, .F. ) ;
#57110 = DIRECTION ( 'NONE',  ( -1.000000000000000000, -1.224606353822377258E-16, -0.000000000000000000 ) ) ;
#57111 = CARTESIAN_POINT ( 'NONE',  ( -51.66175631953248626, -46.44323033348981511, 56.12883151261869585 ) ) ;
#57112 = CARTESIAN_POINT ( 'NONE',  ( -19.99999999999999289, -4.000000000000000000, -1.500000000000001332 ) ) ;
#57113 = VERTEX_POINT ( 'NONE', #51414 ) ;
#57114 = CARTESIAN_POINT ( 'NONE',  ( -100.9488071816703325, -60.26389219641809092, 195.1823302269569638 ) ) ;
#57115 = CARTESIAN_POINT ( 'NONE',  ( -0.08513827788200560576, 51.26930509877139031, 10.24999999999999822 ) ) ;
#57116 = ORIENTED_EDGE ( 'NONE', *, *, #90306, .F. ) ;
#57117 = CARTESIAN_POINT ( 'NONE',  ( -17.81989518783386828, 43.26589036823222045, 4.977204039784022704 ) ) ;
#57119 = STYLED_ITEM ( 'NONE', ( #33495 ), #8082 ) ;
#57118 = CARTESIAN_POINT ( 'NONE',  ( 101.4909721992553386, -38.35592705684496195, 96.87947274763887151 ) ) ;
#57120 = DIRECTION ( 'NONE',  ( -1.000000000000000000, -1.224606353822377258E-16, -0.000000000000000000 ) ) ;
#57121 = CARTESIAN_POINT ( 'NONE',  ( -6.738100187484505454, 41.71798639774085160, -59.05424569925489209 ) ) ;
#57123 = ADVANCED_FACE ( 'NONE', ( #44949 ), #23518, .F. ) ;
#57122 = AXIS2_PLACEMENT_3D ( 'NONE', #29255, #94493, #52404 ) ;
#57124 = CARTESIAN_POINT ( 'NONE',  ( 0.000000000000000000, -0.5000000000000000000, 0.000000000000000000 ) ) ;
#57125 = FACE_OUTER_BOUND ( 'NONE', #9932, .T. ) ;
#57127 = CARTESIAN_POINT ( 'NONE',  ( 82.59143751758651320, -29.99999999999999289, 149.9729633368418149 ) ) ;
#57126 = UNCERTAINTY_MEASURE_WITH_UNIT (LENGTH_MEASURE( 1.000000000000000082E-05 ), #84072, 'distance_accuracy_value', 'NONE');
#57128 = MECHANICAL_DESIGN_GEOMETRIC_PRESENTATION_REPRESENTATION (  '', ( #93335 ), #91577 ) ;
#57129 = CARTESIAN_POINT ( 'NONE',  ( -10.45127858233877127, 43.22611363095290216, -15.39966633374197258 ) ) ;
#57130 = CARTESIAN_POINT ( 'NONE',  ( -28.79545026039450661, 10.21913446882438059, 41.74404769594809039 ) ) ;
#57131 = FACE_OUTER_BOUND ( 'NONE', #79464, .T. ) ;
#57132 = EDGE_LOOP ( 'NONE', ( #51622, #326, #65074, #102457, #16287 ) ) ;
#57133 = ORIENTED_EDGE ( 'NONE', *, *, #49663, .T. ) ;
#57134 = CARTESIAN_POINT ( 'NONE',  ( 50.59493527809745927, -22.19395423099893350, 45.92767238662714391 ) ) ;
#57135 = CARTESIAN_POINT ( 'NONE',  ( -34.16642289233710983, 463.8422268500497125, 18.98106911353875148 ) ) ;
#57136 = CARTESIAN_POINT ( 'NONE',  ( 36.62653249502783126, 28.16896743844737472, -11.37818750331463669 ) ) ;
#57137 = AXIS2_PLACEMENT_3D ( 'NONE', #4680, #62391, #36022 ) ;
#57138 = ORIENTED_EDGE ( 'NONE', *, *, #99693, .T. ) ;
#57139 = CARTESIAN_POINT ( 'NONE',  ( -108.0453605404376418, -38.35628879702573357, 138.1634217362548895 ) ) ;
#57140 = ORIENTED_EDGE ( 'NONE', *, *, #106081, .F. ) ;
#57141 = CARTESIAN_POINT ( 'NONE',  ( 28.17375089705461377, 34.32482771417988232, -8.153477830591306486 ) ) ;
#57142 = CARTESIAN_POINT ( 'NONE',  ( 90.86190182423041506, -38.35175838285157113, 20.64935856576204642 ) ) ;
#57143 = CARTESIAN_POINT ( 'NONE',  ( 10.82137645999426034, 16.06255650797403334, -9.525625210853387870 ) ) ;
#57144 = CARTESIAN_POINT ( 'NONE',  ( -36.34588046138484430, 26.08150859950978528, -11.88946398838879936 ) ) ;
#57145 = CARTESIAN_POINT ( 'NONE',  ( 97.60711786217987651, -45.28277154639692270, 115.8989380571673138 ) ) ;
#57146 = CARTESIAN_POINT ( 'NONE',  ( -31.66959486501912124, 439.0151181633245301, 23.43702844066392998 ) ) ;
#57147 =( NAMED_UNIT ( * ) SI_UNIT ( $, .STERADIAN. ) SOLID_ANGLE_UNIT ( ) );
#57148 = CARTESIAN_POINT ( 'NONE',  ( -30.37040671822360238, 310.2650604196215909, -8.515671380529434842 ) ) ;
#57149 = CARTESIAN_POINT ( 'NONE',  ( 2.727075792294463508, -69.18208090123930276, 12.97754602523916212 ) ) ;
#57150 = CARTESIAN_POINT ( 'NONE',  ( 76.44766553792378261, -60.00000000000000711, 188.7013745601435915 ) ) ;
#57151 = B_SPLINE_CURVE_WITH_KNOTS ( 'NONE', 3,
 ( #24287, #50626, #16694, #105693, #41495, #8593, #90585, #40971, #15622, #42026, #74383, #73859, #81405, #24810, #98136, #66305, #57136, #7516, #9117, #106754, #74909, #106210 ),
 .UNSPECIFIED., .F., .F.,
 ( 4, 2, 2, 2, 2, 2, 2, 2, 2, 2, 4 ),
 ( 0.007135418818287256673, 0.007639688340070102668, 0.008143957861852950397, 0.008396092622744374262, 0.008648227383635799861, 0.009152496905418661469, 0.009656766427201524811, 0.009908901188092952145, 0.01016103594898437948, 0.01066530547076722027, 0.01116957499255006279 ),
 .UNSPECIFIED. ) ;
#57152 = CARTESIAN_POINT ( 'NONE',  ( 18.01087898364460216, 44.99999999999999289, 62.56010773621230214 ) ) ;
#57153 = ORIENTED_EDGE ( 'NONE', *, *, #83019, .F. ) ;
#57154 = CARTESIAN_POINT ( 'NONE',  ( 55.70686534075314000, -39.49626118740381031, 61.84722421453820829 ) ) ;
#57155 = CARTESIAN_POINT ( 'NONE',  ( -21.29975379448944750, 294.8969325209484396, -1.990407376643355430 ) ) ;
#57156 = EDGE_CURVE ( 'NONE', #18822, #16756, #4460, .T. ) ;
#57157 = DIRECTION ( 'NONE',  ( -1.000000000000000000, -1.224606353822377258E-16, -0.000000000000000000 ) ) ;
#57158 = CIRCLE ( 'NONE', #21041, 8.000000000000014211 ) ;
#57159 = DIRECTION ( 'NONE',  ( -1.000000000000000000, 0.000000000000000000, 0.000000000000000000 ) ) ;
#57161 = DIRECTION ( 'NONE',  ( 0.000000000000000000, 0.000000000000000000, -1.000000000000000000 ) ) ;
#57160 = CARTESIAN_POINT ( 'NONE',  ( -89.39007834610079328, -38.38716907517502364, -17.33792631335736800 ) ) ;
#57162 = CARTESIAN_POINT ( 'NONE',  ( -42.35645304355714558, 435.3801053262068308, 19.45913382674001113 ) ) ;
#57163 = CARTESIAN_POINT ( 'NONE',  ( 31.43654395834863280, 409.1920974130434843, 24.49082746238584107 ) ) ;
#57164 = CARTESIAN_POINT ( 'NONE',  ( -38.45248457205872938, 463.5270362811817222, 19.68931241193499915 ) ) ;
#57165 = CARTESIAN_POINT ( 'NONE',  ( -8.000000000000000000, -34.34375000000000000, -3.313708498984762496 ) ) ;
#57166 = AXIS2_PLACEMENT_3D ( 'NONE', #16966, #49842, #15889 ) ;
#57167 =( LENGTH_UNIT ( ) NAMED_UNIT ( * ) SI_UNIT ( .MILLI., .METRE. ) );
#57168 = EDGE_CURVE ( 'NONE', #7878, #37991, #11376, .T. ) ;
#57169 = DIRECTION ( 'NONE',  ( 0.000000000000000000, 0.2755684261024844983, -0.9612814585413576030 ) ) ;
#57170 = EDGE_CURVE ( 'NONE', #34186, #29730, #14851, .T. ) ;
#57171 = ORIENTED_EDGE ( 'NONE', *, *, #60362, .F. ) ;
#57172 = CARTESIAN_POINT ( 'NONE',  ( 84.93122466964305772, -28.90423046881255686, 171.9484601080571338 ) ) ;
#57173 = DIRECTION ( 'NONE',  ( -1.000000000000000000, -1.224606353822377258E-16, -0.000000000000000000 ) ) ;
#57174 = VERTEX_POINT ( 'NONE', #68694 ) ;
#57175 = CARTESIAN_POINT ( 'NONE',  ( 6.289692432696780244, -0.6618655008720318866, 6.828989928337167115 ) ) ;
#57176 = CARTESIAN_POINT ( 'NONE',  ( 5.686850908482750988, -4.337623088852442521, -16.91150612930258035 ) ) ;
#57177 = CARTESIAN_POINT ( 'NONE',  ( 31.08349330513380337, -4.000000000000000888, 4.898587196589416773E-16 ) ) ;
#57178 = CARTESIAN_POINT ( 'NONE',  ( -6.061707334783565493, 50.00000000000000000, -95.47772246151531306 ) ) ;
#57179 = CARTESIAN_POINT ( 'NONE',  ( 97.73333333333333428, -4.171999999999998820, 5.616230220889773285E-16 ) ) ;
#57180 = DIRECTION ( 'NONE',  ( -1.000000000000000000, -0.000000000000000000, -0.000000000000000000 ) ) ;
#57181 = EDGE_CURVE ( 'NONE', #103416, #37313, #95997, .T. ) ;
#57182 = CARTESIAN_POINT ( 'NONE',  ( 38.64309545302648274, 25.32034139323217303, 11.54985948942248442 ) ) ;
#57183 = CARTESIAN_POINT ( 'NONE',  ( -4.571008445750556426, -47.80671748343184646, 102.5889671997070991 ) ) ;
#57185 = CARTESIAN_POINT ( 'NONE',  ( -11.44715097168767493, 7.561630284056658269, -9.465016000907271021 ) ) ;
#57184 = CARTESIAN_POINT ( 'NONE',  ( -4.959378720893033332, -18.58292471749708952, 35.08865701613389376 ) ) ;
#57186 = CARTESIAN_POINT ( 'NONE',  ( 5.082755093536324154, -16.34375000204838813, 5.082755093536326818 ) ) ;
#57187 = CARTESIAN_POINT ( 'NONE',  ( -39.04923757955551622, 40.83906611472718140, 52.30342408729326564 ) ) ;
#57188 = CARTESIAN_POINT ( 'NONE',  ( 4.392764327028893412, -1.139124805377877303, 104.3925874334283037 ) ) ;
#57189 = VERTEX_POINT ( 'NONE', #36354 ) ;
#57190 = AXIS2_PLACEMENT_3D ( 'NONE', #88387, #6375, #105096 ) ;
#57191 = CARTESIAN_POINT ( 'NONE',  ( -17.49999999999978684, 49.99999999999968026, 59.86364615470553474 ) ) ;
#57192 = CARTESIAN_POINT ( 'NONE',  ( 23.21751746555303342, 25.25267828308493989, 33.20617127781017075 ) ) ;
#57193 = STYLED_ITEM ( 'NONE', ( #52407 ), #51679 ) ;
#57194 = CARTESIAN_POINT ( 'NONE',  ( -3.981297741196698770, 136.6372954359305254, -5.000000000000002665 ) ) ;
#57195 = DIRECTION ( 'NONE',  ( 0.000000000000000000, 0.000000000000000000, -1.000000000000000000 ) ) ;
#57196 = CARTESIAN_POINT ( 'NONE',  ( 4.660622226121999390, 53.64064877316351954, 8.373216872651239484 ) ) ;
#57197 = ORIENTED_EDGE ( 'NONE', *, *, #14245, .T. ) ;
#57198 = CARTESIAN_POINT ( 'NONE',  ( 12.01340667464404710, 17.09192326160534492, -9.133615181541646422 ) ) ;
#57199 = CARTESIAN_POINT ( 'NONE',  ( 0.000000000000000000, 0.000000000000000000, 0.000000000000000000 ) ) ;
#57201 = ORIENTED_EDGE ( 'NONE', *, *, #70494, .T. ) ;
#57200 = STYLED_ITEM ( 'NONE', ( #85975 ), #20774 ) ;
#57203 = SURFACE_STYLE_FILL_AREA ( #56126 ) ;
#57202 = VECTOR ( 'NONE', #71526, 1000.000000000000000 ) ;
#57204 = CARTESIAN_POINT ( 'NONE',  ( -1.469576158976823947E-15, -16.06250000409677270, 8.000000000000000000 ) ) ;
#57205 = CARTESIAN_POINT ( 'NONE',  ( -24.08450779687392895, 41.61345875976761732, -74.19243768968262032 ) ) ;
#57206 = CARTESIAN_POINT ( 'NONE',  ( -100.9029158711696255, -59.99999999999999289, 86.33068100717986226 ) ) ;
#57207 = FACE_BOUND ( 'NONE', #8434, .T. ) ;
#57208 = CARTESIAN_POINT ( 'NONE',  ( 0.000000000000000000, 294.8518027762758038, -10.00000000000000355 ) ) ;
#57209 = CARTESIAN_POINT ( 'NONE',  ( 26.54817876223620488, 310.6276912632132507, 11.31208242866018132 ) ) ;
#57210 = CARTESIAN_POINT ( 'NONE',  ( -8.833736740224848560, 2.942687158940284764, 14.70881556658443756 ) ) ;
#57212 = CARTESIAN_POINT ( 'NONE',  ( 32.18423816190075115, 486.1452344075074734, 5.458209535234520793 ) ) ;
#57211 = CARTESIAN_POINT ( 'NONE',  ( 6.043427762770655853, -5.000000000000002665, -95.48543666094731464 ) ) ;
#57213 = CARTESIAN_POINT ( 'NONE',  ( -86.13910310123007719, -18.34493521033569863, 167.7294979905272498 ) ) ;
#57214 = VERTEX_POINT ( 'NONE', #69223 ) ;
#57215 = ORIENTED_EDGE ( 'NONE', *, *, #16038, .T. ) ;
#57216 = EDGE_LOOP ( 'NONE', ( #101744, #15430, #71026, #92650, #42344 ) ) ;
#57217 = DIRECTION ( 'NONE',  ( 0.000000000000000000, 1.000000000000000000, 0.000000000000000000 ) ) ;
#57218 = ADVANCED_FACE ( 'NONE', ( #102091 ), #59606, .T. ) ;
#57219 = ORIENTED_EDGE ( 'NONE', *, *, #91953, .F. ) ;
#57220 =( GEOMETRIC_REPRESENTATION_CONTEXT ( 3 ) GLOBAL_UNCERTAINTY_ASSIGNED_CONTEXT ( ( #75515 ) ) GLOBAL_UNIT_ASSIGNED_CONTEXT ( ( #72696, #6898, #99084 ) ) REPRESENTATION_CONTEXT ( 'NONE', 'WORKASPACE' ) );
#57221 = DIRECTION ( 'NONE',  ( -0.000000000000000000, -1.000000000000000000, -0.000000000000000000 ) ) ;
#57222 = EDGE_CURVE ( 'NONE', #57919, #97345, #53387, .T. ) ;
#57223 = CARTESIAN_POINT ( 'NONE',  ( 0.000000000000000000, 0.000000000000000000, 0.000000000000000000 ) ) ;
#57224 = AXIS2_PLACEMENT_3D ( 'NONE', #34114, #65382, #49173 ) ;
#57225 = CARTESIAN_POINT ( 'NONE',  ( 9.300689190521341132, 11.36225021108674405, -3.068995344595356157E-13 ) ) ;
#57226 = DIRECTION ( 'NONE',  ( -1.000000000000000000, -1.224606353822377258E-16, -0.000000000000000000 ) ) ;
#57227 = DIRECTION ( 'NONE',  ( 0.000000000000000000, -0.9253863139535718485, 0.3790252893243686305 ) ) ;
#57228 = CARTESIAN_POINT ( 'NONE',  ( 106.6793784964389289, -14.21045842199433729, 163.7934217252150972 ) ) ;
#57229 = EDGE_CURVE ( 'NONE', #24908, #35576, #20000, .T. ) ;
#57230 = CARTESIAN_POINT ( 'NONE',  ( -113.0839934364197887, -60.00000000000005684, 149.3435297534686299 ) ) ;
#57231 = CARTESIAN_POINT ( 'NONE',  ( -60.41731799762936816, -53.39197530348098297, 80.04476055597704942 ) ) ;
#57232 = VERTEX_POINT ( 'NONE', #30898 ) ;
#57233 = CARTESIAN_POINT ( 'NONE',  ( -48.74182829061921041, 38.95314221987509029, 41.06628751931371113 ) ) ;
#57234 = CARTESIAN_POINT ( 'NONE',  ( 94.21046238432340658, -60.00000000000971312, 11.80878925958715087 ) ) ;
#57235 = VERTEX_POINT ( 'NONE', #103691 ) ;
#57236 = CARTESIAN_POINT ( 'NONE',  ( 2.053817364943875123, -60.35891754953962618, 33.94675380999842673 ) ) ;
#57237 = CARTESIAN_POINT ( 'NONE',  ( -2.977408999572654480, -11.00000000204838635, 7.188101187499999156 ) ) ;
#57238 = VERTEX_POINT ( 'NONE', #13068 ) ;
#57239 = CARTESIAN_POINT ( 'NONE',  ( -1.469576158976823947E-15, -29.37499999999999645, 8.000000000000000000 ) ) ;
#57240 = ORIENTED_EDGE ( 'NONE', *, *, #1332, .T. ) ;
#57241 = CARTESIAN_POINT ( 'NONE',  ( 24.34999999999999787, -3.309499999999999886, 4.475777889183790779E-16 ) ) ;
#57242 = CARTESIAN_POINT ( 'NONE',  ( -7.914984360234579519, 3.818534719232086871, -7.907701344400643428 ) ) ;
#57243 = CARTESIAN_POINT ( 'NONE',  ( -112.1314382224425401, -60.00000000000002842, 166.9117109934064160 ) ) ;
#57244 = CARTESIAN_POINT ( 'NONE',  ( 9.771873710511815858, -57.46329652640150698, 29.13520411490522122 ) ) ;
#57245 = CARTESIAN_POINT ( 'NONE',  ( 5.082755093536324154, -25.71875000204838813, 5.082755093536326818 ) ) ;
#57246 = ADVANCED_FACE ( 'NONE', ( #78877 ), #75115, .T. ) ;
#57247 = DIRECTION ( 'NONE',  ( 0.000000000000000000, 0.000000000000000000, 1.000000000000000000 ) ) ;
#57248 = CARTESIAN_POINT ( 'NONE',  ( 17.89152967391262905, 43.20852219665771088, -5.298485905622539072 ) ) ;
#57249 = CARTESIAN_POINT ( 'NONE',  ( -11.62298468832406328, 15.73209527160812904, 9.621853404307836755 ) ) ;
#57250 = CARTESIAN_POINT ( 'NONE',  ( 1.000000000000000000, -4.607437535715904531, -14.28092741399824384 ) ) ;
#57251 = DIRECTION ( 'NONE',  ( -1.000000000000000000, -0.000000000000000000, -0.000000000000000000 ) ) ;
#57252 = CARTESIAN_POINT ( 'NONE',  ( 13.71723496859481983, -8.874210861067291845, 12.10439619743532624 ) ) ;
#57253 = CARTESIAN_POINT ( 'NONE',  ( -34.23737646655726508, 301.4688704001253541, -0.5023635973111234554 ) ) ;
#57254 = CARTESIAN_POINT ( 'NONE',  ( 93.00819039107329900, -59.99999999999998579, 74.24814202458328793 ) ) ;
#57255 = CARTESIAN_POINT ( 'NONE',  ( -32.62005641966797498, -46.43469510831215530, 35.44769554474900275 ) ) ;
#57256 = LINE ( 'NONE', #42688, #81735 ) ;
#57257 = CARTESIAN_POINT ( 'NONE',  ( 40.90383831102949586, -56.79723033808241439, 43.40186584424645133 ) ) ;
#57258 = DIRECTION ( 'NONE',  ( 0.000000000000000000, 0.000000000000000000, 1.000000000000000000 ) ) ;
#57259 = VERTEX_POINT ( 'NONE', #47563 ) ;
#57260 = CARTESIAN_POINT ( 'NONE',  ( 43.78231969043036997, 434.3019752265855118, 13.50801524699893186 ) ) ;
#57261 = CARTESIAN_POINT ( 'NONE',  ( -83.78472431295821821, -38.77414610831009867, 197.6093069242124614 ) ) ;
#57262 = ORIENTED_EDGE ( 'NONE', *, *, #64968, .F. ) ;
#57264 = CARTESIAN_POINT ( 'NONE',  ( 45.48003679188781234, 379.8448106960472614, 7.220331889307936457 ) ) ;
#57263 = FACE_OUTER_BOUND ( 'NONE', #6896, .T. ) ;
#57265 = CARTESIAN_POINT ( 'NONE',  ( -11.07540909475009450, 19.47767444011234161, 8.771819969050072885 ) ) ;
#57266 = CARTESIAN_POINT ( 'NONE',  ( -49.13582233779567332, 7.783546568855187253, -16.18978396958260646 ) ) ;
#57267 = CARTESIAN_POINT ( 'NONE',  ( -6.866539648855182421, 41.67963793714291398, -59.06571870949380809 ) ) ;
#57268 = CARTESIAN_POINT ( 'NONE',  ( 6.563035550597770218, 3.302680408004402768, -6.845819698387222374 ) ) ;
#57269 = CARTESIAN_POINT ( 'NONE',  ( -37.71459991402550571, 437.7716825518407973, 4.505118785440077822 ) ) ;
#57271 = CARTESIAN_POINT ( 'NONE',  ( 5.725989721596477899, -88.57677111256464286, 1.809923354557187336 ) ) ;
#57270 = CIRCLE ( 'NONE', #78157, 4.000000000000007105 ) ;
#57272 =( NAMED_UNIT ( * ) PLANE_ANGLE_UNIT ( ) SI_UNIT ( $, .RADIAN. ) );
#57273 = CARTESIAN_POINT ( 'NONE',  ( 102.9377691848878840, -60.00000000000000000, 98.21790666211499854 ) ) ;
#57274 = CARTESIAN_POINT ( 'NONE',  ( -1.955013656259688704, -53.86110022085453863, 40.86468968543578484 ) ) ;
#57275 = CYLINDRICAL_SURFACE ( 'NONE', #14667, 1.250000000000000222 ) ;
#57276 = ORIENTED_EDGE ( 'NONE', *, *, #89865, .F. ) ;
#57277 = B_SPLINE_CURVE_WITH_KNOTS ( 'NONE', 3,
 ( #101772, #50541, #34423, #1461, #19845, #101254, #10624, #67295, #41935, #76961, #52680, #99640, #9026, #52151, #17678, #27408, #19323, #58669, #59735, #100173, #51618, #43012, #83456, #85066 ),
 .UNSPECIFIED., .F., .F.,
 ( 4, 2, 2, 2, 2, 2, 2, 2, 2, 2, 2, 4 ),
 ( 0.004982501964703167467, 0.005234564667989247827, 0.005486627371275329054, 0.005990752777847501917, 0.006494878184419674780, 0.006999003590991847643, 0.007251066294277925400, 0.007503128997564004893, 0.008007254404136165613, 0.008511379810708326332, 0.008763442513994402355, 0.009015505217280478378 ),
 .UNSPECIFIED. ) ;
#57278 = ADVANCED_FACE ( 'NONE', ( #104210 ), #47032, .T. ) ;
#57279 = CARTESIAN_POINT ( 'NONE',  ( -96.99816414976265833, -29.99999999999981171, 191.0865392925242077 ) ) ;
#57280 = ORIENTED_EDGE ( 'NONE', *, *, #90337, .T. ) ;
#57281 = CARTESIAN_POINT ( 'NONE',  ( -9.981919929974880645, -57.97247446290226947, 27.65434374221348435 ) ) ;
#57282 = CARTESIAN_POINT ( 'NONE',  ( -16.02335565827205954, 4.077236164004103713, -2.242500883993121530 ) ) ;
#57283 = CARTESIAN_POINT ( 'NONE',  ( 8.361452242971266102, 30.82456655884568519, 0.000000000000000000 ) ) ;
#57284 = CARTESIAN_POINT ( 'NONE',  ( -2.499999999999996447, -30.00000000000000000, -14.79019945774903988 ) ) ;
#57285 = CARTESIAN_POINT ( 'NONE',  ( 9.165151389911677882, 29.73264844392884143, -4.000000000000000000 ) ) ;
#57286 = VECTOR ( 'NONE', #64854, 1000.000000000000000 ) ;
#57287 = CARTESIAN_POINT ( 'NONE',  ( 2.977408999572650927, -23.75000000204839168, -7.188101187500001821 ) ) ;
#57288 =( LENGTH_UNIT ( ) NAMED_UNIT ( * ) SI_UNIT ( .MILLI., .METRE. ) );
#57290 = EDGE_CURVE ( 'NONE', #36676, #97864, #33823, .T. ) ;
#57289 = DIRECTION ( 'NONE',  ( -0.000000000000000000, -0.000000000000000000, 1.000000000000000000 ) ) ;
#57291 = EDGE_CURVE ( 'NONE', #87062, #87964, #26905, .T. ) ;
#57292 = VERTEX_POINT ( 'NONE', #64306 ) ;
#57294 = ORIENTED_EDGE ( 'NONE', *, *, #7452, .F. ) ;
#57293 = CARTESIAN_POINT ( 'NONE',  ( 4.999999999999996447, -3.723962137281043638, 102.2532056551910529 ) ) ;
#57295 = CARTESIAN_POINT ( 'NONE',  ( 80.21638703355559130, -49.90724840867629553, 160.3600109673918155 ) ) ;
#57296 = CARTESIAN_POINT ( 'NONE',  ( 0.000000000000000000, 0.000000000000000000, -7.657127082228716297 ) ) ;
#57297 = CARTESIAN_POINT ( 'NONE',  ( 9.646032546913144046, 88.01280328474365433, 2.644051433538241902 ) ) ;
#57298 = ORIENTED_EDGE ( 'NONE', *, *, #22285, .T. ) ;
#57299 = CARTESIAN_POINT ( 'NONE',  ( -24.21469879905009392, 50.00000000000000000, 58.37456082337698149 ) ) ;
#57300 = CARTESIAN_POINT ( 'NONE',  ( 7.046357527897573192, -86.30615650601002642, -3.789683693877209159 ) ) ;
#57301 = CARTESIAN_POINT ( 'NONE',  ( 7.188101187499999156, -11.75000000204838813, 2.977408999572654924 ) ) ;
#57302 = FACE_OUTER_BOUND ( 'NONE', #63819, .T. ) ;
#57303 = FACE_OUTER_BOUND ( 'NONE', #31814, .T. ) ;
#57305 = CARTESIAN_POINT ( 'NONE',  ( -21.79395256997316110, 303.1333420030371713, 9.997488266507673416 ) ) ;
#57304 = CIRCLE ( 'NONE', #24624, 5.000000000000011546 ) ;
#57306 = CARTESIAN_POINT ( 'NONE',  ( -31.35596682365705945, 438.0939828603719093, 22.55458131664414267 ) ) ;
#57307 = ADVANCED_FACE ( 'NONE', ( #70271 ), #47557, .T. ) ;
#57308 = ORIENTED_EDGE ( 'NONE', *, *, #68350, .F. ) ;
#57309 = B_SPLINE_CURVE_WITH_KNOTS ( 'NONE', 3,
 ( #766, #17011, #25667, #66610, #10490, #91434 ),
 .UNSPECIFIED., .F., .F.,
 ( 4, 2, 4 ),
 ( -4.698498718846532140E-06, 0.0003457374136903327362, 0.0006961733260995119944 ),
 .UNSPECIFIED. ) ;
#57310 = CIRCLE ( 'NONE', #26352, 61.50000000000000000 ) ;
#57311 = CARTESIAN_POINT ( 'NONE',  ( 4.561148568382666468, 143.2220574413671557, 5.000000000000000888 ) ) ;
#57312 = CARTESIAN_POINT ( 'NONE',  ( 7.484880573657958003, 40.61738193562707977, -59.44022980582506221 ) ) ;
#57313 = EDGE_CURVE ( 'NONE', #99443, #4316, #85470, .T. ) ;
#57314 = CARTESIAN_POINT ( 'NONE',  ( 1.250068677369559955, 34.55937372842163313, -28.65813469251532908 ) ) ;
#57315 = VERTEX_POINT ( 'NONE', #71315 ) ;
#57316 = CARTESIAN_POINT ( 'NONE',  ( -1.320432766682874540E-15, -33.03125000204838813, 7.188101187500000044 ) ) ;
#57317 = CARTESIAN_POINT ( 'NONE',  ( 29.52976757919392270, -32.13639089429810980, 40.30885829581517044 ) ) ;
#57318 = CARTESIAN_POINT ( 'NONE',  ( 0.000000000000000000, 0.000000000000000000, 0.000000000000000000 ) ) ;
#57319 = CYLINDRICAL_SURFACE ( 'NONE', #92992, 4.000000000000000888 ) ;
#57320 = EDGE_CURVE ( 'NONE', #50509, #85798, #75345, .T. ) ;
#57321 = CARTESIAN_POINT ( 'NONE',  ( 38.13886201901005535, 438.4571414526099034, 23.48832422888811067 ) ) ;
#57322 = APPLICATION_PROTOCOL_DEFINITION ( 'draft international standard', 'automotive_design', 1998, #83806 ) ;
#57323 = CARTESIAN_POINT ( 'NONE',  ( 49.07509721567211614, 8.836758769845308947, 14.91787708872405993 ) ) ;
#57324 = ORIENTED_EDGE ( 'NONE', *, *, #34162, .T. ) ;
#57325 = CARTESIAN_POINT ( 'NONE',  ( 1.220516205144134947, 43.50113954421431117, 17.81384183994350678 ) ) ;
#57326 = CARTESIAN_POINT ( 'NONE',  ( 9.090909090909089940, 16.00000000000000000, -4.165977904505312246 ) ) ;
#57327 = DIRECTION ( 'NONE',  ( 0.000000000000000000, -1.000000000000000000, 0.000000000000000000 ) ) ;
#57328 = CARTESIAN_POINT ( 'NONE',  ( 12.13034742782337538, 42.00000149833409324, -93.82352941176404215 ) ) ;
#57329 = ORIENTED_EDGE ( 'NONE', *, *, #36957, .F. ) ;
#57330 = CARTESIAN_POINT ( 'NONE',  ( 0.000000000000000000, -1.200000000000000030E-05, -9.000000000000000000 ) ) ;
#57331 = CARTESIAN_POINT ( 'NONE',  ( 108.1233463498552680, -57.67127209427924583, 117.1904254369292318 ) ) ;
#57332 = CARTESIAN_POINT ( 'NONE',  ( 37.31409640255603932, 464.0485063763027824, 19.52659819501504046 ) ) ;
#57333 = PLANE ( 'NONE',  #74218 ) ;
#57334 = CARTESIAN_POINT ( 'NONE',  ( -4.205882352941162416, -5.000000000000000000, -72.69916451482997388 ) ) ;
#57335 = CARTESIAN_POINT ( 'NONE',  ( 11.91432047162523311, 40.83906611472392001, 64.17585289265115023 ) ) ;
#57336 = CARTESIAN_POINT ( 'NONE',  ( -74.55215148334558251, -59.99999999999999289, 177.5930982106680744 ) ) ;
#57337 = STYLED_ITEM ( 'NONE', ( #29710 ), #53583 ) ;
#57338 = CARTESIAN_POINT ( 'NONE',  ( -34.95237279327285762, 304.8277712208536627, 12.26231981495593537 ) ) ;
#57339 = CYLINDRICAL_SURFACE ( 'NONE', #18431, 4.000000000000000000 ) ;
#57340 = CARTESIAN_POINT ( 'NONE',  ( -40.61216075948964033, 351.1469683695276558, 22.89433108575548914 ) ) ;
#57341 = CARTESIAN_POINT ( 'NONE',  ( -85.09751082350868501, -42.94669665112929380, 186.0240982620516093 ) ) ;
#57342 = VECTOR ( 'NONE', #100867, 1000.000000000000114 ) ;
#57343 = VERTEX_POINT ( 'NONE', #57239 ) ;
#57344 = CARTESIAN_POINT ( 'NONE',  ( 25.01177788099232657, 306.1649447482250821, -9.713921147030010417 ) ) ;
#57345 = AXIS2_PLACEMENT_3D ( 'NONE', #88803, #70506, #95311 ) ;
#57346 = ORIENTED_EDGE ( 'NONE', *, *, #37020, .F. ) ;
#57347 = CARTESIAN_POINT ( 'NONE',  ( 16.01731089354320048, 3.899811580360073471, 1.614417983590256123 ) ) ;
#57348 = EDGE_CURVE ( 'NONE', #67879, #54018, #97704, .T. ) ;
#57349 = FILL_AREA_STYLE_COLOUR ( '', #81731 ) ;
#57350 = CARTESIAN_POINT ( 'NONE',  ( -85.70554460909363570, -52.72876096884451869, -4.541171915920864777 ) ) ;
#57351 = CARTESIAN_POINT ( 'NONE',  ( 16.08349330513380337, 4.898587196589405926E-16, -4.000000000000001776 ) ) ;
#57352 = FILL_AREA_STYLE ('',( #65471 ) ) ;
#57353 = ORIENTED_EDGE ( 'NONE', *, *, #20430, .F. ) ;
#57354 = VECTOR ( 'NONE', #101085, 1000.000000000000000 ) ;
#57355 = DIRECTION ( 'NONE',  ( 0.000000000000000000, -1.000000000000000000, 0.000000000000000000 ) ) ;
#57356 = CARTESIAN_POINT ( 'NONE',  ( 13.24339100265629376, 3.909282924590824937, -6.957567076447526588 ) ) ;
#57357 = EDGE_CURVE ( 'NONE', #34141, #47279, #31633, .T. ) ;
#57358 = CARTESIAN_POINT ( 'NONE',  ( 10.45706415777664411, -1.734723475976807094E-15, 13.60704923275374156 ) ) ;
#57359 = CARTESIAN_POINT ( 'NONE',  ( 0.000000000000000000, 0.000000000000000000, 4.000000000000000888 ) ) ;
#57360 = EDGE_CURVE ( 'NONE', #75872, #57426, #76828, .T. ) ;
#57361 = CARTESIAN_POINT ( 'NONE',  ( -25.62895382379538489, -60.00000000000000711, -43.76007060795225101 ) ) ;
#57362 = CARTESIAN_POINT ( 'NONE',  ( -78.10409042525387235, -36.02680010123066268, 131.9807425273284025 ) ) ;
#57363 = EDGE_LOOP ( 'NONE', ( #27212, #62225, #19697 ) ) ;
#57364 = CARTESIAN_POINT ( 'NONE',  ( 29.53284356080077444, -60.00000000000004974, 45.26708560465603171 ) ) ;
#57365 = CARTESIAN_POINT ( 'NONE',  ( 6.928203230275508773, 85.26883324508999351, -4.000000000000001776 ) ) ;
#57366 = CARTESIAN_POINT ( 'NONE',  ( 93.92944981285859285, -57.67333411593723014, 17.34817390334868392 ) ) ;
#57367 = ORIENTED_EDGE ( 'NONE', *, *, #11082, .T. ) ;
#57368 = DIRECTION ( 'NONE',  ( 0.000000000000000000, 1.000000000000000000, 0.000000000000000000 ) ) ;
#57369 = EDGE_CURVE ( 'NONE', #20513, #102378, #42413, .T. ) ;
#57370 = DIRECTION ( 'NONE',  ( 0.000000000000000000, 0.000000000000000000, -1.000000000000000000 ) ) ;
#57371 = ORIENTED_EDGE ( 'NONE', *, *, #5071, .F. ) ;
#57372 = CARTESIAN_POINT ( 'NONE',  ( 24.34999999999999787, -3.309499999999999886, 0.000000000000000000 ) ) ;
#57373 = CIRCLE ( 'NONE', #19571, 5.000000000000002665 ) ;
#57374 = FILL_AREA_STYLE_COLOUR ( '', #96159 ) ;
#57375 = CARTESIAN_POINT ( 'NONE',  ( 5.799999999999999822, 9.237604307034018802, 0.000000000000000000 ) ) ;
#57376 = CARTESIAN_POINT ( 'NONE',  ( -5.082755093536326818, -19.71875000204838457, 5.082755093536325042 ) ) ;
#57377 = EDGE_CURVE ( 'NONE', #70831, #3869, #40640, .T. ) ;
#57378 = EDGE_CURVE ( 'NONE', #46114, #8430, #100932, .T. ) ;
#57379 = CARTESIAN_POINT ( 'NONE',  ( 1.015826369459132961, -8.073766409984528991, -7.642786413616108554 ) ) ;
#57380 = CIRCLE ( 'NONE', #46990, 1.000000000000000444 ) ;
#57381 = CARTESIAN_POINT ( 'NONE',  ( 9.482856158761270748, 82.55692884145280175, 3.177891129109650770 ) ) ;
#57382 = CARTESIAN_POINT ( 'NONE',  ( 7.322849800245819551, 11.36060796471277712, -13.00000000000000711 ) ) ;
#57383 = CARTESIAN_POINT ( 'NONE',  ( -16.80328583523074570, 45.82802980027265960, -4.157797401561525774 ) ) ;
#57384 = CARTESIAN_POINT ( 'NONE',  ( -2.354743324221993728, 47.99999999999999289, -99.86073547176457055 ) ) ;
#57385 =( GEOMETRIC_REPRESENTATION_CONTEXT ( 3 ) GLOBAL_UNCERTAINTY_ASSIGNED_CONTEXT ( ( #51351 ) ) GLOBAL_UNIT_ASSIGNED_CONTEXT ( ( #53090, #69289, #11545 ) ) REPRESENTATION_CONTEXT ( 'NONE', 'WORKASPACE' ) );
#57386 = B_SPLINE_CURVE_WITH_KNOTS ( 'NONE', 3,
 ( #65991, #24512, #73534, #91348, #64934, #83233, #33122, #81616, #15314, #25579 ),
 .UNSPECIFIED., .F., .F.,
 ( 4, 2, 2, 2, 4 ),
 ( 1.748223473168675632E-18, 0.0008022363492415249221, 0.001604472698483048109, 0.002406709047724571188, 0.003208945396966094484 ),
 .UNSPECIFIED. ) ;
#57387 = EDGE_LOOP ( 'NONE', ( #51001, #64951, #79576, #20086 ) ) ;
#57388 = CARTESIAN_POINT ( 'NONE',  ( -7.150000000000003908, 41.64999999999997726, -68.91429205801804869 ) ) ;
#57389 = CONICAL_SURFACE ( 'NONE', #84973, 4.000000000000001776, 0.9599310885968774798 ) ;
#57391 = CARTESIAN_POINT ( 'NONE',  ( 31.19770315994506404, -42.95952005011717034, 34.19569303745028321 ) ) ;
#57390 = CARTESIAN_POINT ( 'NONE',  ( -1.309564884278361513E-05, -14.21045842199434972, 34.36840973699906243 ) ) ;
#57392 = CARTESIAN_POINT ( 'NONE',  ( -32.71902930631085837, 485.4797908183046502, 6.287473911063091059 ) ) ;
#57393 = EDGE_LOOP ( 'NONE', ( #76312, #87766, #15581, #61947 ) ) ;
#57394 = VERTEX_POINT ( 'NONE', #98247 ) ;
#57396 = CARTESIAN_POINT ( 'NONE',  ( 37.85390227844803945, 460.2287157790690344, 2.227471321855208242 ) ) ;
#57395 = FILL_AREA_STYLE_COLOUR ( '', #10736 ) ;
#57397 = CARTESIAN_POINT ( 'NONE',  ( 36.48461538461538822, 4.172000000000003261, 0.000000000000000000 ) ) ;
#57398 = CARTESIAN_POINT ( 'NONE',  ( 80.00000000000000000, -38.00000000001091394, -21.09707704303352926 ) ) ;
#57399 = CARTESIAN_POINT ( 'NONE',  ( 1.009888436704913683, 46.02255095878446411, 16.74547954875638567 ) ) ;
#57400 = CARTESIAN_POINT ( 'NONE',  ( -37.72498816019726320, 463.3860965757806412, 19.97126500436749907 ) ) ;
#57401 = ORIENTED_EDGE ( 'NONE', *, *, #105061, .T. ) ;
#57402 = CARTESIAN_POINT ( 'NONE',  ( 8.180595432802771683, -59.99999999999999289, -42.48548993661778184 ) ) ;
#57403 = CARTESIAN_POINT ( 'NONE',  ( -11.29905645152040350, 45.32368457861270628, -14.89516444794125860 ) ) ;
#57404 = CARTESIAN_POINT ( 'NONE',  ( 30.00000000000000355, 461.8887775513395013, 11.55279652843918825 ) ) ;
#57405 = CARTESIAN_POINT ( 'NONE',  ( 46.00000000000000000, 461.6622277975422435, 10.18145404766785589 ) ) ;
#57406 = CARTESIAN_POINT ( 'NONE',  ( 46.78648606410028066, 13.65508681559503223, -15.44775621776510732 ) ) ;
#57407 = ORIENTED_EDGE ( 'NONE', *, *, #72017, .T. ) ;
#57408 = CARTESIAN_POINT ( 'NONE',  ( -37.56673239365849781, 27.60449318992554169, 13.45617127781067168 ) ) ;
#57409 = EDGE_LOOP ( 'NONE', ( #13250, #25151, #15659, #75211 ) ) ;
#57410 = VERTEX_POINT ( 'NONE', #7106 ) ;
#57411 = DIRECTION ( 'NONE',  ( -0.1270361284032274773, 0.9918980905719693153, 0.000000000000000000 ) ) ;
#57412 = CARTESIAN_POINT ( 'NONE',  ( -32.45623693502356133, 464.7023894946334508, 16.04003527244881866 ) ) ;
#57413 = DIRECTION ( 'NONE',  ( 0.000000000000000000, 0.000000000000000000, 1.000000000000000000 ) ) ;
#57414 = CARTESIAN_POINT ( 'NONE',  ( -45.43249564040426947, 375.4183832217576082, 6.657994069051931696 ) ) ;
#57415 = CARTESIAN_POINT ( 'NONE',  ( 32.64147241561500579, 439.6779429780671649, 24.07034118911087006 ) ) ;
#57416 = ORIENTED_EDGE ( 'NONE', *, *, #90251, .T. ) ;
#57418 = EDGE_CURVE ( 'NONE', #98139, #56878, #40542, .T. ) ;
#57417 = CARTESIAN_POINT ( 'NONE',  ( -9.657190910579735998, 43.43017001567654489, 15.25012657391256354 ) ) ;
#57419 = ORIENTED_EDGE ( 'NONE', *, *, #12175, .T. ) ;
#57420 = CARTESIAN_POINT ( 'NONE',  ( 9.215420734788356327, -54.00000000000000000, 23.11721482942554928 ) ) ;
#57421 = CARTESIAN_POINT ( 'NONE',  ( 6.763850406535977022, 294.7356673863635592, 9.912314076180619438 ) ) ;
#57422 = STYLED_ITEM ( 'NONE', ( #36571 ), #54693 ) ;
#57423 = DIRECTION ( 'NONE',  ( 1.000000000000000000, 1.224606353822377258E-16, 0.000000000000000000 ) ) ;
#57424 = CARTESIAN_POINT ( 'NONE',  ( 69.94764612343819010, -18.63634428197197579, 89.84345188368395441 ) ) ;
#57425 = AXIS2_PLACEMENT_3D ( 'NONE', #37639, #96893, #71536 ) ;
#57426 = VERTEX_POINT ( 'NONE', #82053 ) ;
#57427 = MECHANICAL_DESIGN_GEOMETRIC_PRESENTATION_REPRESENTATION (  '', ( #43665 ), #24823 ) ;
#57428 = CARTESIAN_POINT ( 'NONE',  ( -33.00000000000000000, 463.5362553048592531, 6.739467187734380360 ) ) ;
#57429 = FILL_AREA_STYLE_COLOUR ( '', #15379 ) ;
#57430 = ORIENTED_EDGE ( 'NONE', *, *, #25787, .T. ) ;
#57431 =( NAMED_UNIT ( * ) SI_UNIT ( $, .STERADIAN. ) SOLID_ANGLE_UNIT ( ) );
#57432 = B_SPLINE_CURVE_WITH_KNOTS ( 'NONE', 3,
 ( #40917, #31269, #64153, #72738 ),
 .UNSPECIFIED., .F., .F.,
 ( 4, 4 ),
 ( 0.4999999999999996114, 1.000000000000000000 ),
 .UNSPECIFIED. ) ;
#57433 = AXIS2_PLACEMENT_3D ( 'NONE', #60130, #92994, #20224 ) ;
#57434 = CARTESIAN_POINT ( 'NONE',  ( 5.615901427346222441, 51.99194348808828181, -6.063755289240993385 ) ) ;
#57435 = EDGE_CURVE ( 'NONE', #84910, #84383, #1115, .T. ) ;
#57436 = DIRECTION ( 'NONE',  ( 1.000000000000000000, 0.000000000000000000, 0.000000000000000000 ) ) ;
#57437 = CARTESIAN_POINT ( 'NONE',  ( -8.000000000000000000, -25.53125000409676915, -3.313708498984762496 ) ) ;
#57438 = CARTESIAN_POINT ( 'NONE',  ( -19.99999999999999289, 4.000000000000000888, 25.00000000000000000 ) ) ;
#57439 = CARTESIAN_POINT ( 'NONE',  ( 9.646032546913160033, 246.9871967152563457, 2.644051433538255669 ) ) ;
#57440 = DIRECTION ( 'NONE',  ( -1.000000000000000000, -1.224606353822377258E-16, -0.000000000000000000 ) ) ;
#57441 = EDGE_CURVE ( 'NONE', #6068, #43310, #35524, .T. ) ;
#57442 = CARTESIAN_POINT ( 'NONE',  ( -6.425022312393147139, 3.888363280597711302, 5.000000000000000888 ) ) ;
#57443 = CARTESIAN_POINT ( 'NONE',  ( 7.550180524134850302, -6.994407527868143681, 2.651855549982494509 ) ) ;
#57445 = AXIS2_PLACEMENT_3D ( 'NONE', #16197, #81980, #27531 ) ;
#57444 =( NAMED_UNIT ( * ) SI_UNIT ( $, .STERADIAN. ) SOLID_ANGLE_UNIT ( ) );
#57446 = CARTESIAN_POINT ( 'NONE',  ( -2.918503601031048333, 15.30040232763797192, -9.571198553003716469 ) ) ;
#57447 = ORIENTED_EDGE ( 'NONE', *, *, #27938, .T. ) ;
#57448 =( NAMED_UNIT ( * ) PLANE_ANGLE_UNIT ( ) SI_UNIT ( $, .RADIAN. ) );
#57449 = CARTESIAN_POINT ( 'NONE',  ( 95.42421628608209971, 6.123233995736568081E-16, -5.000000000000011546 ) ) ;
#57450 = CARTESIAN_POINT ( 'NONE',  ( 8.700108653991776464, -60.00000000000000000, 39.63767202453095706 ) ) ;
#57451 = CONICAL_SURFACE ( 'NONE', #10947, 3.309500000000001663, 0.9599310885968770357 ) ;
#57452 = CARTESIAN_POINT ( 'NONE',  ( -98.22775549665112749, -30.00000000000000000, 190.2606745111846180 ) ) ;
#57453 = AXIS2_PLACEMENT_3D ( 'NONE', #33751, #18091, #41810 ) ;
#57454 = MECHANICAL_DESIGN_GEOMETRIC_PRESENTATION_REPRESENTATION (  '', ( #14421 ), #10958 ) ;
#57455 = FACE_OUTER_BOUND ( 'NONE', #59640, .T. ) ;
#57456 = CARTESIAN_POINT ( 'NONE',  ( 73.84627813901309423, -57.61934647735279924, 186.2875162611425992 ) ) ;
#57458 = LINE ( 'NONE', #18105, #80977 ) ;
#57457 = CARTESIAN_POINT ( 'NONE',  ( -1.010512028542145835, 25.89279316576818601, -38.74621732557902476 ) ) ;
#57459 = CARTESIAN_POINT ( 'NONE',  ( 14.75721006082208575, -24.00293099030797705, -38.53146564288101672 ) ) ;
#57460 = DIRECTION ( 'NONE',  ( 0.000000000000000000, 0.000000000000000000, 1.000000000000000000 ) ) ;
#57461 = PRODUCT_RELATED_PRODUCT_CATEGORY ( 'part', '', ( #38205 ) ) ;
#57462 = FACE_OUTER_BOUND ( 'NONE', #79616, .T. ) ;
#57463 = CARTESIAN_POINT ( 'NONE',  ( -8.401912187080752048, -60.00000000000000711, 39.63564103648013059 ) ) ;
#57464 = CARTESIAN_POINT ( 'NONE',  ( 13.11993966223870522, 19.43011205168758693, 7.666318333318653089 ) ) ;
#57465 = CARTESIAN_POINT ( 'NONE',  ( 1.220421971816566309, 45.62918557654543861, -17.81470306399649672 ) ) ;
#57466 = CARTESIAN_POINT ( 'NONE',  ( -86.53945512387777228, -17.00671387159180625, 184.4939234780275967 ) ) ;
#57467 = B_SPLINE_CURVE_WITH_KNOTS ( 'NONE', 3,
 ( #36778, #69643, #71218, #55019, #87950, #48524, #30798, #73324, #40444, #15631, #72798, #47464, #73869, #106222, #105703, #6473, #23768, #23227, #98146, #89008, #39405, #31846, #106764, #81415, #7526, #56066 ),
 .UNSPECIFIED., .F., .F.,
 ( 4, 2, 2, 2, 2, 2, 2, 2, 2, 2, 2, 2, 4 ),
 ( 0.003090214743966921036, 0.003342416748342327739, 0.003594618752717734442, 0.003846820757093141578, 0.004099022761468547847, 0.004603426770219354314, 0.004855628774594765787, 0.005107830778970177260, 0.006116638796471883868, 0.006368840800847312689, 0.006621042805222741509, 0.006873244809598170330, 0.007125446813973600017 ),
 .UNSPECIFIED. ) ;
#57468 = ORIENTED_EDGE ( 'NONE', *, *, #94659, .T. ) ;
#57469 = CARTESIAN_POINT ( 'NONE',  ( 17.50000000000261124, 50.02580020274679384, 60.61389435659040004 ) ) ;
#57470 = CARTESIAN_POINT ( 'NONE',  ( 28.50099738913158376, 0.000000000000000000, 5.000000000000002665 ) ) ;
#57471 = CARTESIAN_POINT ( 'NONE',  ( -10.41106923231795101, -53.40263473211271616, 32.80381487082638614 ) ) ;
#57472 = DIRECTION ( 'NONE',  ( 0.000000000000000000, 1.000000000000000000, 0.000000000000000000 ) ) ;
#57474 = CARTESIAN_POINT ( 'NONE',  ( 4.962386525749626465, -62.75672373854419561, 12.88232180906529223 ) ) ;
#57473 = CARTESIAN_POINT ( 'NONE',  ( -103.5376772722346459, -60.00000000000000711, 191.8212684384977536 ) ) ;
#57475 = ORIENTED_EDGE ( 'NONE', *, *, #81699, .T. ) ;
#57476 = MECHANICAL_DESIGN_GEOMETRIC_PRESENTATION_REPRESENTATION (  '', ( #9289 ), #45430 ) ;
#57477 = CARTESIAN_POINT ( 'NONE',  ( -6.735051087780404622, -4.346205982504359078, -16.86563398496736710 ) ) ;
#57478 = CARTESIAN_POINT ( 'NONE',  ( 17.50000000000000711, 2.500000000000000444, 0.000000000000000000 ) ) ;
#57479 = CARTESIAN_POINT ( 'NONE',  ( 31.94399449188606965, 299.1674248799971565, -1.040763782016456362 ) ) ;
#57480 = CARTESIAN_POINT ( 'NONE',  ( 4.861072549008417454, -47.07915654916947545, 102.3606070684416807 ) ) ;
#57481 = EDGE_CURVE ( 'NONE', #97430, #5281, #102706, .T. ) ;
#57482 = CARTESIAN_POINT ( 'NONE',  ( -7.999885325681428405, -81.00022934870062841, 0.2682325777720067084 ) ) ;
#57483 = LINE ( 'NONE', #75814, #34194 ) ;
#57484 = CARTESIAN_POINT ( 'NONE',  ( 106.9110190588319540, -14.21045842199441367, 176.0591306608180844 ) ) ;
#57485 = CARTESIAN_POINT ( 'NONE',  ( -34.94338628507543376, 342.5355909536760350, -0.9693026116538068226 ) ) ;
#57486 = ORIENTED_EDGE ( 'NONE', *, *, #103889, .F. ) ;
#57487 = CARTESIAN_POINT ( 'NONE',  ( 21.08349330513380337, -7.703719777548943412E-31, 4.000000000000001776 ) ) ;
#57488 = CARTESIAN_POINT ( 'NONE',  ( 0.1306530452038046075, -5.952467836904144605, 5.690023276062396107 ) ) ;
#57489 = VECTOR ( 'NONE', #10900, 1000.000000000000000 ) ;
#57490 = CARTESIAN_POINT ( 'NONE',  ( -33.24561022503097263, 485.0000549217730281, 0.3114934373726880867 ) ) ;
#57491 = CARTESIAN_POINT ( 'NONE',  ( 37.63786767139364287, 432.3659482643442402, 5.163126625230292532 ) ) ;
#57492 = CARTESIAN_POINT ( 'NONE',  ( 44.27172743695263790, 463.5980762766301950, 7.352902973909428930 ) ) ;
#57493 = EDGE_LOOP ( 'NONE', ( #39078, #72559, #23753, #31299 ) ) ;
#57494 = MECHANICAL_DESIGN_GEOMETRIC_PRESENTATION_REPRESENTATION (  '', ( #19615 ), #38526 ) ;
#57495 = CARTESIAN_POINT ( 'NONE',  ( -8.000000000000000000, -22.34374999999999645, -3.313708498984762496 ) ) ;
#57496 = EDGE_CURVE ( 'NONE', #93532, #88504, #56156, .T. ) ;
#57497 = VECTOR ( 'NONE', #87394, 1000.000000000000000 ) ;
#57498 = ORIENTED_EDGE ( 'NONE', *, *, #92875, .F. ) ;
#57499 = CARTESIAN_POINT ( 'NONE',  ( 36.04707687143260841, 485.1891289572317874, -2.470783067951639378 ) ) ;
#57500 = EDGE_CURVE ( 'NONE', #68507, #62602, #84340, .T. ) ;
#57501 = CARTESIAN_POINT ( 'NONE',  ( 30.98778555464372886, 438.9951436325601435, 22.21946372908199407 ) ) ;
#57502 = DIRECTION ( 'NONE',  ( 0.000000000000000000, 1.000000000000000000, 0.000000000000000000 ) ) ;
#57503 = CARTESIAN_POINT ( 'NONE',  ( 9.182151393623465552, 45.78138532639618319, 14.82507784383104621 ) ) ;
#57504 = ORIENTED_EDGE ( 'NONE', *, *, #14563, .T. ) ;
#57505 = CARTESIAN_POINT ( 'NONE',  ( 5.000000000000000000, -13.83542193917754126, 11.07282995724436780 ) ) ;
#57506 = CARTESIAN_POINT ( 'NONE',  ( -71.71355155960320360, -60.00000000004398970, 173.0691681726769957 ) ) ;
#57507 = CARTESIAN_POINT ( 'NONE',  ( 46.00000000000000000, 437.8943772434384414, 13.39121328441395953 ) ) ;
#57508 = VERTEX_POINT ( 'NONE', #59406 ) ;
#57509 = CARTESIAN_POINT ( 'NONE',  ( 91.91289437223223047, -60.00000000000001421, 16.01571062708334381 ) ) ;
#57511 = CARTESIAN_POINT ( 'NONE',  ( 14.77419618374876897, -53.39659763945549997, 32.92159578500137940 ) ) ;
#57510 = CARTESIAN_POINT ( 'NONE',  ( -104.0091953780157752, -14.21045842199432663, 192.0632730704776066 ) ) ;
#57513 = CARTESIAN_POINT ( 'NONE',  ( 1.998715226652062816E-15, 61.49999999999999289, -8.160374191332742555 ) ) ;
#57512 = UNCERTAINTY_MEASURE_WITH_UNIT (LENGTH_MEASURE( 1.000000000000000082E-05 ), #104150, 'distance_accuracy_value', 'NONE');
#57514 = CARTESIAN_POINT ( 'NONE',  ( 0.000000000000000000, 43.34115912517999902, 0.000000000000000000 ) ) ;
#57515 = CARTESIAN_POINT ( 'NONE',  ( -39.39627231840285759, -22.22833841577496727, 34.41038875012783649 ) ) ;
#57516 = CARTESIAN_POINT ( 'NONE',  ( 0.000000000000000000, 6.123233995736770227E-16, -5.000000000000002665 ) ) ;
#57517 = ORIENTED_EDGE ( 'NONE', *, *, #89354, .F. ) ;
#57518 = CARTESIAN_POINT ( 'NONE',  ( 79.82022815836235452, -5.000000000000000000, 0.000000000000000000 ) ) ;
#57519 = CARTESIAN_POINT ( 'NONE',  ( 14.29190075645216851, 12.99999999999999289, 7.999999999999998224 ) ) ;
#57520 = CARTESIAN_POINT ( 'NONE',  ( 40.73878142687892279, 503.7113041876743864, 10.19672445236252045 ) ) ;
#57521 = CARTESIAN_POINT ( 'NONE',  ( -46.00000000000000000, 500.0000000000002274, 0.000000000000000000 ) ) ;
#57522 = DIRECTION ( 'NONE',  ( 0.000000000000000000, -1.000000000000000000, 0.000000000000000000 ) ) ;
#57523 = CARTESIAN_POINT ( 'NONE',  ( -32.32362562572921405, 488.2653032247410465, 9.218764297502717753 ) ) ;
#57524 = EDGE_LOOP ( 'NONE', ( #100474, #101325, #60966, #44767, #10184 ) ) ;
#57525 = CARTESIAN_POINT ( 'NONE',  ( 4.869065774733604357, -47.04879514974216903, 102.3543991519893979 ) ) ;
#57526 = ORIENTED_EDGE ( 'NONE', *, *, #27868, .F. ) ;
#57527 = CARTESIAN_POINT ( 'NONE',  ( 75.98997121514811681, -30.00000000000000711, -17.37669743398828359 ) ) ;
#57528 = CARTESIAN_POINT ( 'NONE',  ( 23.96490998088334479, 41.62201801232857434, -74.35350452741216998 ) ) ;
#57529 = CARTESIAN_POINT ( 'NONE',  ( 61.11682663846713837, 6.975173280561618775E-15, 0.000000000000000000 ) ) ;
#57530 = DIRECTION ( 'NONE',  ( 0.000000000000000000, 0.000000000000000000, 1.000000000000000000 ) ) ;
#57531 = CARTESIAN_POINT ( 'NONE',  ( 94.94366555557748200, -30.00000000000000711, 117.6622010833369245 ) ) ;
#57532 = DIRECTION ( 'NONE',  ( 0.000000000000000000, -1.000000000000000000, 0.000000000000000000 ) ) ;
#57533 = VERTEX_POINT ( 'NONE', #92269 ) ;
#57534 = PRESENTATION_LAYER_ASSIGNMENT (  '', '', ( #104041 ) ) ;
#57535 = ORIENTED_EDGE ( 'NONE', *, *, #87735, .F. ) ;
#57536 = EDGE_LOOP ( 'NONE', ( #67867, #13261, #86012, #96785 ) ) ;
#57537 = CARTESIAN_POINT ( 'NONE',  ( 0.08285530294364991388, 1.570896314703519092, -8.000000000000000000 ) ) ;
#57538 = CARTESIAN_POINT ( 'NONE',  ( 42.69811214730273718, 434.9611672192513652, 18.34625614733210242 ) ) ;
#57539 = DIRECTION ( 'NONE',  ( -1.000000000000000000, -0.000000000000000000, -0.000000000000000000 ) ) ;
#57540 = ORIENTED_EDGE ( 'NONE', *, *, #5146, .F. ) ;
#57542 = ADVANCED_FACE ( 'NONE', ( #77171 ), #31007, .T. ) ;
#57541 = CARTESIAN_POINT ( 'NONE',  ( 9.177080501238306098, 105.5334694285426878, -3.972956046786646489 ) ) ;
#57543 = B_SPLINE_CURVE_WITH_KNOTS ( 'NONE', 3,
 ( #59867, #11270, #28053, #100821, #44204, #60403, #70065, #77090, #93811, #93283, #69019, #67938, #18897, #78149, #102967, #3209, #36149, #52814, #84658, #77628 ),
 .UNSPECIFIED., .F., .F.,
 ( 4, 2, 2, 2, 2, 2, 2, 2, 2, 4 ),
 ( 0.001107850312301168066, 0.001612907343245352943, 0.002117964374189537820, 0.002623021405133722696, 0.003128078436077907573, 0.003380606951549999795, 0.003633135467022092450, 0.004138192497966277326, 0.004643249528910462637, 0.005148306559854647080 ),
 .UNSPECIFIED. ) ;
#57544 = EDGE_LOOP ( 'NONE', ( #58049, #33918, #102739, #72803, #27659 ) ) ;
#57545 = CARTESIAN_POINT ( 'NONE',  ( 33.11888822396143439, 438.9412710830782203, 23.90522241289666994 ) ) ;
#57546 = CARTESIAN_POINT ( 'NONE',  ( 79.86200412043599783, -38.77158211078923955, 192.7350020035291038 ) ) ;
#57547 = CARTESIAN_POINT ( 'NONE',  ( 32.82876496518922949, 434.9825001184026974, 12.61068621696671244 ) ) ;
#57548 = CARTESIAN_POINT ( 'NONE',  ( 35.70121033104481256, 304.3670428735860582, 4.138962953855986449 ) ) ;
#57549 = DIRECTION ( 'NONE',  ( 0.000000000000000000, 0.000000000000000000, 1.000000000000000000 ) ) ;
#57550 = CARTESIAN_POINT ( 'NONE',  ( 17.33349330513380337, 1.593028355512270567E-15, 0.000000000000000000 ) ) ;
#57551 = DIRECTION ( 'NONE',  ( 0.000000000000000000, 0.000000000000000000, -1.000000000000000000 ) ) ;
#57552 = ADVANCED_FACE ( 'NONE', ( #26011 ), #61455, .T. ) ;
#57553 = CIRCLE ( 'NONE', #50688, 3.309500000000001663 ) ;
#57554 = CARTESIAN_POINT ( 'NONE',  ( -5.566314792736418937, 5.173014757752155468, 5.000000000000000000 ) ) ;
#57555 = ORIENTED_EDGE ( 'NONE', *, *, #94585, .F. ) ;
#57556 = CARTESIAN_POINT ( 'NONE',  ( 6.575925811255157072, 7.701774614579013800, -1.127145213565506199E-15 ) ) ;
#57557 = CARTESIAN_POINT ( 'NONE',  ( -22.10619625089826101, 303.2187564606320507, 10.01583238429591383 ) ) ;
#57558 = CARTESIAN_POINT ( 'NONE',  ( 7.941476738584017703, 54.17312961474247857, -1.691542695135636043 ) ) ;
#57559 = FILL_AREA_STYLE_COLOUR ( '', #80021 ) ;
#57560 = CARTESIAN_POINT ( 'NONE',  ( 3.313708498984762052, -10.71874999999999289, -8.000000000000000000 ) ) ;
#57561 = DIRECTION ( 'NONE',  ( 0.000000000000000000, 0.000000000000000000, 1.000000000000000000 ) ) ;
#57562 = LINE ( 'NONE', #24194, #96066 ) ;
#57563 = STYLED_ITEM ( 'NONE', ( #44458 ), #87330 ) ;
#57564 = CARTESIAN_POINT ( 'NONE',  ( 11.57593719571816848, 303.6016380201557467, 9.883826392888126477 ) ) ;
#57565 = AXIS2_PLACEMENT_3D ( 'NONE', #88808, #64540, #63488 ) ;
#57566 = VERTEX_POINT ( 'NONE', #17885 ) ;
#57567 = CARTESIAN_POINT ( 'NONE',  ( 84.00255077718880159, -61.04110459592344995, 192.3126038394468367 ) ) ;
#57568 = FACE_OUTER_BOUND ( 'NONE', #89711, .T. ) ;
#57569 = EDGE_CURVE ( 'NONE', #12793, #8878, #40724, .T. ) ;
#57570 = CARTESIAN_POINT ( 'NONE',  ( -9.514607632263416548, 142.5277189159678244, 4.999999999993908872 ) ) ;
#57571 = ORIENTED_EDGE ( 'NONE', *, *, #98343, .F. ) ;
#57572 = AXIS2_PLACEMENT_3D ( 'NONE', #71555, #97417, #80179 ) ;
#57573 = CARTESIAN_POINT ( 'NONE',  ( 93.24448322355969765, -57.65503295969547537, -16.59265381772082648 ) ) ;
#57574 = DIRECTION ( 'NONE',  ( -1.000000000000000000, -1.224606353822377258E-16, -0.000000000000000000 ) ) ;
#57575 = CARTESIAN_POINT ( 'NONE',  ( -3.979266480701241449, -30.00000000000000000, -6.940132439339150139 ) ) ;
#57576 = CARTESIAN_POINT ( 'NONE',  ( 28.43345358725029115, 12.59863739772601399, 40.78014218160711124 ) ) ;
#57577 = EDGE_CURVE ( 'NONE', #94251, #92669, #97520, .T. ) ;
#57578 = CARTESIAN_POINT ( 'NONE',  ( -80.76340928301335964, -29.99999999999999645, 14.59015454481636631 ) ) ;
#57579 = CARTESIAN_POINT ( 'NONE',  ( -73.67282519167521571, -37.99999999999996447, 114.1319439230774293 ) ) ;
#57580 = CARTESIAN_POINT ( 'NONE',  ( -1.469576158976823947E-15, -29.56250000409677270, 8.000000000000000000 ) ) ;
#57582 = CARTESIAN_POINT ( 'NONE',  ( -32.94021323899823983, 485.0599191339510980, 5.361609822537303671 ) ) ;
#57581 = CARTESIAN_POINT ( 'NONE',  ( 3.668277386370350612, -48.89637005407674053, 104.6014336420241051 ) ) ;
#57583 = CARTESIAN_POINT ( 'NONE',  ( -17.49999999999997158, 48.39190472549704936, 64.09945637329882118 ) ) ;
#57584 = CARTESIAN_POINT ( 'NONE',  ( -10.28624191511816832, 43.25714326066847804, -15.40779740156204980 ) ) ;
#57585 = CARTESIAN_POINT ( 'NONE',  ( -12.50000000000000533, -3.000000000000000000, -55.73109925765190553 ) ) ;
#57586 = CARTESIAN_POINT ( 'NONE',  ( 6.000469943554648466, -80.99929508329502426, 0.2622423038614462021 ) ) ;
#57587 = CARTESIAN_POINT ( 'NONE',  ( -7.000000000000000000, 8.572527594031471218E-16, -10.42450674750459072 ) ) ;
#57588 = DIRECTION ( 'NONE',  ( -0.5735764363510497121, 0.8191520442889892450, 1.003171929053521665E-16 ) ) ;
#57590 = EDGE_CURVE ( 'NONE', #26910, #16434, #30433, .T. ) ;
#57589 = AXIS2_PLACEMENT_3D ( 'NONE', #28461, #63999, #48823 ) ;
#57591 = ORIENTED_EDGE ( 'NONE', *, *, #69650, .F. ) ;
#57592 = CARTESIAN_POINT ( 'NONE',  ( 6.333820801330004358, -4.275724398228958556, -5.594228103109302630 ) ) ;
#57593 = CYLINDRICAL_SURFACE ( 'NONE', #71078, 3.400000000000000355 ) ;
#57594 = CARTESIAN_POINT ( 'NONE',  ( -7.999885325681426629, 81.00022934870064262, 0.2682325777720090954 ) ) ;
#57595 = CARTESIAN_POINT ( 'NONE',  ( -70.63365275292957790, -30.00000000000000355, -20.40377125985679285 ) ) ;
#57596 = AXIS2_PLACEMENT_3D ( 'NONE', #2251, #59467, #68072 ) ;
#57598 = CARTESIAN_POINT ( 'NONE',  ( -69.96807924604867424, -47.40884888655846652, -24.11331608286603867 ) ) ;
#57597 = CYLINDRICAL_SURFACE ( 'NONE', #96647, 11.27631144943088515 ) ;
#57599 = AXIS2_PLACEMENT_3D ( 'NONE', #33749, #83863, #60681 ) ;
#57600 = ORIENTED_EDGE ( 'NONE', *, *, #26804, .F. ) ;
#57601 = AXIS2_PLACEMENT_3D ( 'NONE', #100813, #19433, #26974 ) ;
#57602 =( LENGTH_UNIT ( ) NAMED_UNIT ( * ) SI_UNIT ( .MILLI., .METRE. ) );
#57603 = VERTEX_POINT ( 'NONE', #32295 ) ;
#57604 = CARTESIAN_POINT ( 'NONE',  ( 42.16858620283969827, 461.4629983908274085, 3.513115262088578383 ) ) ;
#57605 = SURFACE_STYLE_FILL_AREA ( #24757 ) ;
#57606 = CARTESIAN_POINT ( 'NONE',  ( -33.51294852578469374, -60.00000000000000711, -40.49430134959939664 ) ) ;
#57607 = EDGE_LOOP ( 'NONE', ( #21998, #42987, #79402, #4942 ) ) ;
#57608 = PLANE ( 'NONE',  #25774 ) ;
#57609 = CARTESIAN_POINT ( 'NONE',  ( -8.392066182232479576, 294.6889698295346989, -5.445651201154610987 ) ) ;
#57610 = CARTESIAN_POINT ( 'NONE',  ( 96.24277997628448134, -45.27105860737465548, 194.1195206907109707 ) ) ;
#57612 = CARTESIAN_POINT ( 'NONE',  ( -17.40646473312639841, 45.37698912868007284, 6.411815653116708091 ) ) ;
#57611 = SURFACE_SIDE_STYLE ('',( #40920 ) ) ;
#57613 = ORIENTED_EDGE ( 'NONE', *, *, #60962, .T. ) ;
#57614 = EDGE_LOOP ( 'NONE', ( #1199, #46086, #19097, #85014, #100135 ) ) ;
#57615 = VERTEX_POINT ( 'NONE', #40357 ) ;
#57616 = CARTESIAN_POINT ( 'NONE',  ( 31.39117689105021114, 374.8518552428220687, 22.89618308279878534 ) ) ;
#57617 = AXIS2_PLACEMENT_3D ( 'NONE', #65636, #8978, #24669 ) ;
#57618 = EDGE_CURVE ( 'NONE', #74620, #45703, #79171, .T. ) ;
#57619 = CARTESIAN_POINT ( 'NONE',  ( -6.282481257750798243, -11.96849729169379906, 11.22390784433505218 ) ) ;
#57620 = CARTESIAN_POINT ( 'NONE',  ( 16.02154979717257177, 46.08966533359958362, 4.311187973113217886 ) ) ;
#57621 = VERTEX_POINT ( 'NONE', #916 ) ;
#57622 = AXIS2_PLACEMENT_3D ( 'NONE', #4897, #4357, #105175 ) ;
#57623 = CARTESIAN_POINT ( 'NONE',  ( 15.45347762069375008, 46.21495662470461241, -5.015962831654205090 ) ) ;
#57624 = CARTESIAN_POINT ( 'NONE',  ( 6.500000000000002665, 2.501851166488368694, -5.848636054922034866 ) ) ;
#57625 = CARTESIAN_POINT ( 'NONE',  ( 73.33904886068935980, 4.000000000000014211, 0.000000000000000000 ) ) ;
#57626 = CARTESIAN_POINT ( 'NONE',  ( -23.49283269198559765, -57.67355083020559192, 42.82390242447587525 ) ) ;
#57627 = CARTESIAN_POINT ( 'NONE',  ( 5.082755093536325930, -29.46875000204838813, -5.082755093536325042 ) ) ;
#57628 = CARTESIAN_POINT ( 'NONE',  ( 7.619135598915496743, -68.17305367784679504, 2.449260492474797601 ) ) ;
#57629 = CARTESIAN_POINT ( 'NONE',  ( -0.6457802288624886478, 26.01561404131637900, 38.41666353100805509 ) ) ;
#57630 = CARTESIAN_POINT ( 'NONE',  ( 0.7768758660237293778, 15.00000000000000000, -9.999999999999998224 ) ) ;
#57631 = ADVANCED_FACE ( 'NONE', ( #1476 ), #63142, .T. ) ;
#57632 = CARTESIAN_POINT ( 'NONE',  ( -67.59740049799954420, -60.00000000000004263, -35.88590100950167994 ) ) ;
#57633 = CARTESIAN_POINT ( 'NONE',  ( -24.85253352225967660, -29.99999999999996092, 38.32597638696945097 ) ) ;
#57634 = CARTESIAN_POINT ( 'NONE',  ( -53.14642949933918459, -32.57121755472948621, 53.87505941010853405 ) ) ;
#57635 = B_SPLINE_CURVE_WITH_KNOTS ( 'NONE', 3,
 ( #12087, #35888, #28867, #27804 ),
 .UNSPECIFIED., .F., .F.,
 ( 4, 4 ),
 ( 0.0008765341530664233537, 0.001750917060903518828 ),
 .UNSPECIFIED. ) ;
#57636 = DIRECTION ( 'NONE',  ( 0.000000000000000000, 1.000000000000000000, 0.000000000000000000 ) ) ;
#57637 = CONICAL_SURFACE ( 'NONE', #19840, 8.605212085995399107, 1.221730476396037490 ) ;
#57638 = ORIENTED_EDGE ( 'NONE', *, *, #77238, .T. ) ;
#57639 =( GEOMETRIC_REPRESENTATION_CONTEXT ( 3 ) GLOBAL_UNCERTAINTY_ASSIGNED_CONTEXT ( ( #67759 ) ) GLOBAL_UNIT_ASSIGNED_CONTEXT ( ( #50239, #35699, #75579 ) ) REPRESENTATION_CONTEXT ( 'NONE', 'WORKASPACE' ) );
#57640 = CARTESIAN_POINT ( 'NONE',  ( -101.5070894931627237, -60.23655731454778106, 194.7038192617161201 ) ) ;
#57641 =( REPRESENTATION_RELATIONSHIP ('NONE','NONE', #69581, #44072 ) REPRESENTATION_RELATIONSHIP_WITH_TRANSFORMATION ( #85339 )SHAPE_REPRESENTATION_RELATIONSHIP( ) );
#57642 = CARTESIAN_POINT ( 'NONE',  ( -3.610928090092041298, 295.9072949364792748, -10.00534087566827957 ) ) ;
#57643 = CARTESIAN_POINT ( 'NONE',  ( 14.83341732121158074, 0.1101086422626733341, 15.00090745772169498 ) ) ;
#57644 = ORIENTED_EDGE ( 'NONE', *, *, #99839, .F. ) ;
#57645 = CARTESIAN_POINT ( 'NONE',  ( -17.64329793883007014, 43.19648771793908537, 6.176246302466131155 ) ) ;
#57646 = AXIS2_PLACEMENT_3D ( 'NONE', #37261, #20577, #27585 ) ;
#57647 = CARTESIAN_POINT ( 'NONE',  ( 73.82277771826251467, -38.32584844511357147, 158.7404017193271955 ) ) ;
#57648 = CARTESIAN_POINT ( 'NONE',  ( 48.48434714564498194, 13.98045800628846536, 16.77138779655850342 ) ) ;
#57649 = CARTESIAN_POINT ( 'NONE',  ( 75.30000000000001137, 4.475777889183788807E-16, -3.309499999999999886 ) ) ;
#57650 = CARTESIAN_POINT ( 'NONE',  ( 0.000000000000000000, 0.000000000000000000, 0.000000000000000000 ) ) ;
#57651 = AXIS2_PLACEMENT_3D ( 'NONE', #37070, #12745, #93148 ) ;
#57652 = CARTESIAN_POINT ( 'NONE',  ( -41.72794603366239130, 484.6317694608798092, -3.103777363567681746 ) ) ;
#57653 = CARTESIAN_POINT ( 'NONE',  ( 85.23574709202168265, -29.99999999999999645, 172.5112148116256208 ) ) ;
#57654 = CARTESIAN_POINT ( 'NONE',  ( 37.49684268403980525, 491.2987049188978972, 12.22740886045582087 ) ) ;
#57655 = CARTESIAN_POINT ( 'NONE',  ( -29.50913623581989143, 8.560131685753201936, 42.09559527950047197 ) ) ;
#57656 = LINE ( 'NONE', #33425, #77689 ) ;
#57657 = VERTEX_POINT ( 'NONE', #73236 ) ;
#57658 = ORIENTED_EDGE ( 'NONE', *, *, #75093, .T. ) ;
#57659 = CARTESIAN_POINT ( 'NONE',  ( 50.14541849784438909, -42.97498551929375310, 52.14416430124198598 ) ) ;
#57660 = CARTESIAN_POINT ( 'NONE',  ( 5.897541335056488698, 41.82858996958378128, -58.91931118675405799 ) ) ;
#57661 = CARTESIAN_POINT ( 'NONE',  ( 9.646529840909229492, 51.27688607554693334, 3.403973221859950549 ) ) ;
#57662 = ORIENTED_EDGE ( 'NONE', *, *, #93514, .T. ) ;
#57664 = EDGE_CURVE ( 'NONE', #99282, #45623, #7990, .T. ) ;
#57663 = CARTESIAN_POINT ( 'NONE',  ( -95.04834772930165343, -38.35492584456250142, 58.17196757228544612 ) ) ;
#57665 = ORIENTED_EDGE ( 'NONE', *, *, #105092, .F. ) ;
#57666 = CARTESIAN_POINT ( 'NONE',  ( 27.71631011201982275, 34.52951940293964128, -7.705211021039788832 ) ) ;
#57667 = CARTESIAN_POINT ( 'NONE',  ( 93.01387217800777307, -38.35490714704352655, 43.55336315142127290 ) ) ;
#57668 = CARTESIAN_POINT ( 'NONE',  ( 15.50375927216468774, 22.90274012999477904, 1.420239429929072594 ) ) ;
#57669 = CARTESIAN_POINT ( 'NONE',  ( 98.39111451231792671, -45.28270231285164016, 120.6799170848443907 ) ) ;
#57670 = CARTESIAN_POINT ( 'NONE',  ( -31.32094825172531571, 438.4579161125127484, 22.73291248390550834 ) ) ;
#57671 = FACE_OUTER_BOUND ( 'NONE', #41333, .T. ) ;
#57672 = CARTESIAN_POINT ( 'NONE',  ( -30.24048965269528821, 312.5841310900376584, -7.180294356216179175 ) ) ;
#57673 = CARTESIAN_POINT ( 'NONE',  ( 3.073649067497001841, -68.88943550113336300, 13.02707457859375495 ) ) ;
#57674 = CARTESIAN_POINT ( 'NONE',  ( 76.37984825064704353, -59.99999999999997868, 188.4578851984081780 ) ) ;
#57675 = EDGE_CURVE ( 'NONE', #77299, #77294, #102788, .T. ) ;
#57676 = CIRCLE ( 'NONE', #2561, 3.400000000000000355 ) ;
#57677 = DIRECTION ( 'NONE',  ( -1.000000000000000000, -0.000000000000000000, -0.000000000000000000 ) ) ;
#57678 = ORIENTED_EDGE ( 'NONE', *, *, #18042, .F. ) ;
#57679 = CARTESIAN_POINT ( 'NONE',  ( 61.75317836559133866, -42.96044902961888567, 78.62615862502077846 ) ) ;
#57680 = CARTESIAN_POINT ( 'NONE',  ( -23.30980644977553595, 303.3900546958402060, -9.884505219500150375 ) ) ;
#57681 = ADVANCED_FACE ( 'NONE', ( #7982 ), #81858, .F. ) ;
#57682 = CARTESIAN_POINT ( 'NONE',  ( 6.928203230275510549, 30.00000000000000355, -4.000000000000000000 ) ) ;
#57683 = EDGE_CURVE ( 'NONE', #32972, #24986, #83044, .T. ) ;
#57684 = CARTESIAN_POINT ( 'NONE',  ( -9.368151975306767909, -4.999999999999999112, -18.70424021566291373 ) ) ;
#57686 = CARTESIAN_POINT ( 'NONE',  ( -37.82123075315000449, 485.6920212717419645, -4.511793510526142192 ) ) ;
#57685 = CARTESIAN_POINT ( 'NONE',  ( -77.16460649846582953, -38.35595679982836259, -28.07778984955893264 ) ) ;
#57687 = CARTESIAN_POINT ( 'NONE',  ( -40.87566242051374132, 372.2907203791197617, 25.85377625089821763 ) ) ;
#57688 = CARTESIAN_POINT ( 'NONE',  ( -38.19782146056491712, 25.52416208525854913, -11.07986758502889835 ) ) ;
#57689 = DIRECTION ( 'NONE',  ( 0.000000000000000000, 0.8363101477004194484, -0.5482566341170006519 ) ) ;
#57690 = CARTESIAN_POINT ( 'NONE',  ( -1.469576158976823947E-15, -27.87499999999999645, 8.000000000000000000 ) ) ;
#57691 = DIRECTION ( 'NONE',  ( -1.000000000000000000, -1.224606353822377258E-16, -0.000000000000000000 ) ) ;
#57692 = VERTEX_POINT ( 'NONE', #89977 ) ;
#57693 = CARTESIAN_POINT ( 'NONE',  ( 86.00659031669722765, -21.65052574614072256, 173.2934799618346062 ) ) ;
#57694 = CARTESIAN_POINT ( 'NONE',  ( 4.948897892503503648, -15.25620861757297853, -6.941426030570269745 ) ) ;
#57695 = CARTESIAN_POINT ( 'NONE',  ( 46.36650669486618881, 1.474610560812782335E-15, 0.000000000000000000 ) ) ;
#57696 = EDGE_LOOP ( 'NONE', ( #84178, #56478 ) ) ;
#57697 = FACE_OUTER_BOUND ( 'NONE', #83391, .T. ) ;
#57698 = DIRECTION ( 'NONE',  ( 0.000000000000000000, 0.000000000000000000, 1.000000000000000000 ) ) ;
#57699 = DIRECTION ( 'NONE',  ( 0.000000000000000000, -1.000000000000000000, 0.000000000000000000 ) ) ;
#57700 = CARTESIAN_POINT ( 'NONE',  ( -10.71924530989230107, -3.000000000000002665, -74.44967652503967770 ) ) ;
#57701 = FILL_AREA_STYLE ('',( #50159 ) ) ;
#57702 = SURFACE_STYLE_FILL_AREA ( #73899 ) ;
#57703 = ADVANCED_FACE ( 'NONE', ( #33356 ), #106144, .F. ) ;
#57704 = AXIS2_PLACEMENT_3D ( 'NONE', #69118, #27623, #63544 ) ;
#57705 = CARTESIAN_POINT ( 'NONE',  ( 38.54706409169610026, 25.36787315721333869, 11.41424143689304316 ) ) ;
#57706 = DIRECTION ( 'NONE',  ( 1.000000000000000000, 1.224606353822377258E-16, 0.000000000000000000 ) ) ;
#57707 = EDGE_CURVE ( 'NONE', #97355, #36385, #104461, .T. ) ;
#57709 = CARTESIAN_POINT ( 'NONE',  ( -13.41661347689002959, 22.36574897157366237, 3.535290152413994136 ) ) ;
#57708 = CARTESIAN_POINT ( 'NONE',  ( -17.36216298162189275, -24.06244604014566590, 36.30748115442920465 ) ) ;
#57710 = MECHANICAL_DESIGN_GEOMETRIC_PRESENTATION_REPRESENTATION (  '', ( #104232 ), #92208 ) ;
#57711 = CARTESIAN_POINT ( 'NONE',  ( -1.320432766682874540E-15, -15.03125000204838457, 7.188101187500000044 ) ) ;
#57712 = CYLINDRICAL_SURFACE ( 'NONE', #2713, 1.250000000000001110 ) ;
#57713 = CONICAL_SURFACE ( 'NONE', #12910, 4.172000000000001485, 0.9599310885968750373 ) ;
#57714 = VECTOR ( 'NONE', #25447, 1000.000000000000000 ) ;
#57715 = DIRECTION ( 'NONE',  ( -0.5735764363510497121, 0.8191520442889892450, 1.003171929053521665E-16 ) ) ;
#57716 = CIRCLE ( 'NONE', #88777, 4.000000000000000888 ) ;
#57717 = ORIENTED_EDGE ( 'NONE', *, *, #13889, .F. ) ;
#57718 = VECTOR ( 'NONE', #88438, 1000.000000000000000 ) ;
#57719 = CARTESIAN_POINT ( 'NONE',  ( -17.50000000000511235, 49.61376050340021493, 62.33429930757461790 ) ) ;
#57720 = EDGE_CURVE ( 'NONE', #2280, #29160, #71735, .T. ) ;
#57721 = CARTESIAN_POINT ( 'NONE',  ( 7.922811941611899833, 4.628808333142398368, -8.057670691780701944 ) ) ;
#57722 = AXIS2_PLACEMENT_3D ( 'NONE', #26597, #93423, #76154 ) ;
#57723 = CARTESIAN_POINT ( 'NONE',  ( -8.618528913615500997, 129.1314578644004598, 1.270215581529557045E-12 ) ) ;
#57724 =( BOUNDED_SURFACE ( )  B_SPLINE_SURFACE ( 3, 2, ( 
 ( #24221, #32836, #104569 ),
 ( #24745, #57592, #90514 ),
 ( #47912, #6932, #16628 ),
 ( #49516, #30722, #47391 ),
 ( #6395, #105628, #51104 ),
 ( #2557, #17704, #10645 ) ),
 .UNSPECIFIED., .F., .F., .F. ) 
 B_SPLINE_SURFACE_WITH_KNOTS ( ( 4, 2, 4 ),
 ( 3, 3 ),
 ( 0.003199762745116009350, 0.007302762474435758877, 0.01140576220375550884 ),
 ( 0.000000000000000000, 1.000000000000000000 ),
 .UNSPECIFIED. ) 
 GEOMETRIC_REPRESENTATION_ITEM ( )  RATIONAL_B_SPLINE_SURFACE ( (
 ( 1.000000000000000000, 0.8047731410850426093, 1.000000000000000000),
 ( 1.000000000000000000, 0.8125552299153956382, 1.000000000000000000),
 ( 1.000000000000000000, 0.8191520442892966658, 1.000000000000000000),
 ( 1.000000000000000000, 0.8191520442886820463, 1.000000000000000000),
 ( 1.000000000000000000, 0.8125552299158568248, 1.000000000000000000),
 ( 1.000000000000000000, 0.8047731410850429423, 1.000000000000000000) ) ) 
 REPRESENTATION_ITEM ( '' )  SURFACE ( )  );
#57725 = DIRECTION ( 'NONE',  ( -0.8191520442889881348, 1.003171929053520186E-16, 0.5735764363510513775 ) ) ;
#57727 = CARTESIAN_POINT ( 'NONE',  ( 9.442771828977239323, -34.58963171957248051, -32.44484452317096412 ) ) ;
#57726 = LINE ( 'NONE', #49104, #1930 ) ;
#57728 = VERTEX_POINT ( 'NONE', #17167 ) ;
#57729 = CARTESIAN_POINT ( 'NONE',  ( -4.472135954999578722, -85.13579204946555024, 4.000000000000001776 ) ) ;
#57730 = CARTESIAN_POINT ( 'NONE',  ( -4.648081478759306329, 52.18157122484780075, 6.195523926019952832 ) ) ;
#57731 = VERTEX_POINT ( 'NONE', #69561 ) ;
#57732 = CARTESIAN_POINT ( 'NONE',  ( 9.833493305133805151, 4.898587196589411843E-16, -4.000000000000001776 ) ) ;
#57733 = CARTESIAN_POINT ( 'NONE',  ( -34.80075338857600542, 40.47836787973446349, -59.87678982950887274 ) ) ;
#57734 = CARTESIAN_POINT ( 'NONE',  ( -96.89880926707883191, -60.00000000000000000, 62.01847588090020480 ) ) ;
#57735 = CARTESIAN_POINT ( 'NONE',  ( 28.98629307556451096, 14.82330134267482968, -41.90042541400673315 ) ) ;
#57736 = DIRECTION ( 'NONE',  ( 0.000000000000000000, 0.000000000000000000, 1.000000000000000000 ) ) ;
#57737 = CARTESIAN_POINT ( 'NONE',  ( 41.86527866917096929, 465.6949979513468065, 15.31736901429372111 ) ) ;
#57738 = DIRECTION ( 'NONE',  ( 0.000000000000000000, -1.000000000000000000, 0.000000000000000000 ) ) ;
#57740 = CARTESIAN_POINT ( 'NONE',  ( -7.063836241042545261, 41.16939184123525308, -58.51214979689661533 ) ) ;
#57739 = CARTESIAN_POINT ( 'NONE',  ( -11.99999999999999467, -5.000000000000002665, -83.42920367502566137 ) ) ;
#57741 = CARTESIAN_POINT ( 'NONE',  ( -84.47455154433566804, -32.43567151322172748, 172.8640213309939782 ) ) ;
#57742 = EDGE_LOOP ( 'NONE', ( #4179, #88284, #21503, #83432, #23844 ) ) ;
#57743 = CARTESIAN_POINT ( 'NONE',  ( 7.500000000000005329, 24.91666666666666430, -68.91429205785459544 ) ) ;
#57744 = ORIENTED_EDGE ( 'NONE', *, *, #98771, .F. ) ;
#57745 = PRESENTATION_LAYER_ASSIGNMENT (  '', '', ( #97340 ) ) ;
#57746 = ORIENTED_EDGE ( 'NONE', *, *, #80719, .F. ) ;
#57747 = DIRECTION ( 'NONE',  ( -1.000000000000000000, -1.224606353822377258E-16, -0.000000000000000000 ) ) ;
#57748 = EDGE_CURVE ( 'NONE', #66339, #65683, #86293, .T. ) ;
#57749 = CARTESIAN_POINT ( 'NONE',  ( 33.74362713068862973, 463.9326864247046274, 7.533159870298671734 ) ) ;
#57750 = ORIENTED_EDGE ( 'NONE', *, *, #94376, .F. ) ;
#57751 = CARTESIAN_POINT ( 'NONE',  ( -18.95009283723106108, 304.6966536337758384, 8.904021447602946893 ) ) ;
#57752 = DIRECTION ( 'NONE',  ( -1.000000000000000000, -1.224606353822377258E-16, -0.000000000000000000 ) ) ;
#57753 = DIRECTION ( 'NONE',  ( 0.000000000000000000, 0.000000000000000000, -1.000000000000000000 ) ) ;
#57754 = CARTESIAN_POINT ( 'NONE',  ( -7.046357527897572304, -63.69384349398997358, -3.789683693877210935 ) ) ;
#57755 = CARTESIAN_POINT ( 'NONE',  ( -0.08408805189534301894, 54.30758622938873259, 7.749999999999999112 ) ) ;
#57756 = CARTESIAN_POINT ( 'NONE',  ( 10.50000000000000711, -5.000000000000000000, -77.33514508527181874 ) ) ;
#57757 = CARTESIAN_POINT ( 'NONE',  ( 0.000000000000000000, 6.928203230275505220, -4.000000000000007105 ) ) ;
#57758 = ADVANCED_FACE ( 'NONE', ( #12890 ), #82045, .T. ) ;
#57759 = CARTESIAN_POINT ( 'NONE',  ( 108.5047413589249032, -30.00000000000003197, 153.5997199437166785 ) ) ;
#57760 = CARTESIAN_POINT ( 'NONE',  ( -105.8556346142475064, -14.21045842199439946, 186.2197870760574290 ) ) ;
#57761 = CARTESIAN_POINT ( 'NONE',  ( -60.62598618508234694, -49.91629112966251824, 78.91895544919526628 ) ) ;
#57762 = VERTEX_POINT ( 'NONE', #45814 ) ;
#57763 = CARTESIAN_POINT ( 'NONE',  ( 59.21693087040298309, 38.95252063249746044, 23.56881319470565828 ) ) ;
#57764 = CARTESIAN_POINT ( 'NONE',  ( 95.01407385562683316, -60.00000000000486011, -10.13917562263175931 ) ) ;
#57765 = VERTEX_POINT ( 'NONE', #96491 ) ;
#57766 = CARTESIAN_POINT ( 'NONE',  ( 6.057315617798289864, -32.51038067482491556, 29.29837158373775807 ) ) ;
#57767 = CARTESIAN_POINT ( 'NONE',  ( -102.4764807934955684, -52.71020093064566225, 139.6445780999559076 ) ) ;
#57768 = CARTESIAN_POINT ( 'NONE',  ( -7.188101187500000933, -11.37500000204838635, -2.977408999572651371 ) ) ;
#57769 = SURFACE_STYLE_USAGE ( .BOTH. , #16261 ) ;
#57770 = VERTEX_POINT ( 'NONE', #79232 ) ;
#57771 = CARTESIAN_POINT ( 'NONE',  ( 5.112876467197158270, -29.99999999999999289, 5.074076696858962343 ) ) ;
#57772 = ORIENTED_EDGE ( 'NONE', *, *, #37238, .F. ) ;
#57773 = DIRECTION ( 'NONE',  ( -1.000000000000000000, -1.224606353822377258E-16, -0.000000000000000000 ) ) ;
#57774 = PRESENTATION_LAYER_ASSIGNMENT (  '', '', ( #102608 ) ) ;
#57775 = CARTESIAN_POINT ( 'NONE',  ( -38.57579099119070776, -59.99999999999998579, 50.19459341522732387 ) ) ;
#57776 = SURFACE_SIDE_STYLE ('',( #89639 ) ) ;
#57777 = CARTESIAN_POINT ( 'NONE',  ( -7.188101187500002709, -20.18750000204838457, 2.977408999572648707 ) ) ;
#57778 = FACE_OUTER_BOUND ( 'NONE', #97860, .T. ) ;
#57779 = CARTESIAN_POINT ( 'NONE',  ( -36.19631612776445451, 463.3208255589807436, 20.09850791239178136 ) ) ;
#57780 = CARTESIAN_POINT ( 'NONE',  ( -11.82990717643122913, 16.52431529527237686, 9.360596964331460157 ) ) ;
#57781 = DIRECTION ( 'NONE',  ( -1.000000000000000000, -0.000000000000000000, -0.000000000000000000 ) ) ;
#57782 = CARTESIAN_POINT ( 'NONE',  ( 58.67238219402268840, -4.000000000000000000, 4.898587196589421703E-16 ) ) ;
#57783 = CARTESIAN_POINT ( 'NONE',  ( -27.40885254791232484, 296.4310517681949477, -1.657890121573132758 ) ) ;
#57784 = EDGE_CURVE ( 'NONE', #105451, #71046, #85693, .T. ) ;
#57785 = AXIS2_PLACEMENT_3D ( 'NONE', #52667, #2517, #44602 ) ;
#57786 = CARTESIAN_POINT ( 'NONE',  ( 86.85824047554997662, -59.99999999999997868, -10.30000423349464000 ) ) ;
#57787 = CARTESIAN_POINT ( 'NONE',  ( -32.25315245376670248, -39.49381076584415950, 34.00953951823751709 ) ) ;
#57788 = B_SPLINE_CURVE_WITH_KNOTS ( 'NONE', 3,
 ( #83519, #42531, #43602, #76493, #75433, #67361, #44686, #19910, #46268, #95348, #29075, #22010, #4213, #37684, #70008, #53812, #30099, #3691, #78096, #86219, #85675, #52754 ),
 .UNSPECIFIED., .F., .F.,
 ( 4, 2, 2, 2, 2, 2, 2, 2, 2, 2, 4 ),
 ( 0.006402890727434164611, 0.006802332259859119809, 0.007201773792284075874, 0.008000656857133985403, 0.008799539921983894064, 0.009598422986833804460, 0.01039730605168371486, 0.01119618911653362352, 0.01159563064895857351, 0.01199507218138352350, 0.01279395524623341308 ),
 .UNSPECIFIED. ) ;
#57789 = CARTESIAN_POINT ( 'NONE',  ( -0.9999999999999941158, -50.00000000000000000, 101.0455488498966758 ) ) ;
#57790 = CARTESIAN_POINT ( 'NONE',  ( 42.69170054815374726, -56.79417449340447632, 45.32995381252002431 ) ) ;
#57791 = AXIS2_PLACEMENT_3D ( 'NONE', #98522, #96940, #82345 ) ;
#57792 = STYLED_ITEM ( 'NONE', ( #29983 ), #9182 ) ;
#57793 = CYLINDRICAL_SURFACE ( 'NONE', #98901, 1.250000000000001110 ) ;
#57794 = ORIENTED_EDGE ( 'NONE', *, *, #26870, .F. ) ;
#57795 = CARTESIAN_POINT ( 'NONE',  ( -7.744991119775238353, 88.46438785425129936, -2.016316005557097224 ) ) ;
#57796 = CARTESIAN_POINT ( 'NONE',  ( -78.43232732503568627, -38.62599759898719753, 189.4934868374475911 ) ) ;
#57797 = ORIENTED_EDGE ( 'NONE', *, *, #35011, .T. ) ;
#57799 = CARTESIAN_POINT ( 'NONE',  ( 33.08751701378358945, 301.6823158026044780, 11.49690784967660662 ) ) ;
#57798 = CARTESIAN_POINT ( 'NONE',  ( 2.499999999999998224, -15.46059144880916669, 23.70576633280851553 ) ) ;
#57800 = CARTESIAN_POINT ( 'NONE',  ( -12.20022513325955060, 22.12076576512997761, -6.617748350316168704 ) ) ;
#57801 = CARTESIAN_POINT ( 'NONE',  ( 0.7145311798163198613, -4.618802153516998743, 7.999999999999998224 ) ) ;
#57802 = CARTESIAN_POINT ( 'NONE',  ( 5.821933341149770236, -1.421180797415668495, 6.499999999999999112 ) ) ;
#57803 = CONICAL_SURFACE ( 'NONE', #9533, 3.309500000000007880, 0.9599310885968770357 ) ;
#57804 = CARTESIAN_POINT ( 'NONE',  ( 6.960057398333424850, 40.00000000387299082, -71.11869238929793369 ) ) ;
#57805 = CARTESIAN_POINT ( 'NONE',  ( 27.61650669486618881, 4.898587196589411843E-16, -4.000000000000000888 ) ) ;
#57806 = CIRCLE ( 'NONE', #92214, 12.50000000000000000 ) ;
#57807 = CARTESIAN_POINT ( 'NONE',  ( -31.36487372896283432, 435.2119976784319419, 22.89286986970661886 ) ) ;
#57808 = DIRECTION ( 'NONE',  ( 0.2280158659356096851, 0.1533051183531252970, 0.9615125093145531210 ) ) ;
#57809 = CARTESIAN_POINT ( 'NONE',  ( 107.5845383886140070, -60.00000000000002132, 126.3434892167558417 ) ) ;
#57810 = CARTESIAN_POINT ( 'NONE',  ( -1.017643907183658269, -54.00000000000000711, 40.96503185701687499 ) ) ;
#57811 = AXIS2_PLACEMENT_3D ( 'NONE', #98831, #33087, #40610 ) ;
#57812 = ORIENTED_EDGE ( 'NONE', *, *, #99242, .T. ) ;
#57813 = EDGE_CURVE ( 'NONE', #88199, #24805, #17494, .T. ) ;
#57814 = CARTESIAN_POINT ( 'NONE',  ( -88.51094613808753309, -30.00000000000004619, 187.8829266376722558 ) ) ;
#57815 = ORIENTED_EDGE ( 'NONE', *, *, #17145, .T. ) ;
#57816 = CARTESIAN_POINT ( 'NONE',  ( 26.94560983199210469, 36.66014041605558305, -10.05698433968642291 ) ) ;
#57817 = CARTESIAN_POINT ( 'NONE',  ( -15.05785784214101675, 3.824195276787174524, 4.604276673525165009 ) ) ;
#57818 = CARTESIAN_POINT ( 'NONE',  ( 8.441132293725070568, 123.9914807902447507, 4.999999999997543298 ) ) ;
#57819 = CARTESIAN_POINT ( 'NONE',  ( 31.92850365111794986, 356.8979959129785584, 21.71365648330940346 ) ) ;
#57820 = CARTESIAN_POINT ( 'NONE',  ( -23.13516888326535081, 27.39820858062317654, -33.20617127781034839 ) ) ;
#57821 = CARTESIAN_POINT ( 'NONE',  ( -5.082755093536325042, -23.46875000204838457, -5.082755093536325930 ) ) ;
#57822 = DIRECTION ( 'NONE',  ( -0.000000000000000000, -1.000000000000000000, -0.000000000000000000 ) ) ;
#57823 = DIRECTION ( 'NONE',  ( 0.000000000000000000, 0.000000000000000000, 1.000000000000000000 ) ) ;
#57825 = EDGE_LOOP ( 'NONE', ( #22294, #17726, #83841, #87534 ) ) ;
#57824 = CARTESIAN_POINT ( 'NONE',  ( -7.461257001076914364, 40.57433524249821488, -59.19359852711440340 ) ) ;
#57826 = CARTESIAN_POINT ( 'NONE',  ( 83.18608112039279945, -22.15294338469834301, 146.6214932445938075 ) ) ;
#57827 = DIRECTION ( 'NONE',  ( -1.000000000000000000, 0.000000000000000000, 0.000000000000000000 ) ) ;
#57828 = CARTESIAN_POINT ( 'NONE',  ( 9.176803346051512378, 85.52947155797443202, 3.973598758023530131 ) ) ;
#57829 = VERTEX_POINT ( 'NONE', #70083 ) ;
#57830 = CARTESIAN_POINT ( 'NONE',  ( 11.89131030317610183, 1.482358050883964840E-15, 0.000000000000000000 ) ) ;
#57831 = DIRECTION ( 'NONE',  ( 0.000000000000000000, 1.734723475976806700E-15, 1.000000000000000000 ) ) ;
#57832 = CARTESIAN_POINT ( 'NONE',  ( 38.78087356411477060, 27.29650668150768666, -12.51507624832616195 ) ) ;
#57833 = CARTESIAN_POINT ( 'NONE',  ( 7.212408192734265810, 27.98482910679631530, -3.465038817813886229 ) ) ;
#57834 = AXIS2_PLACEMENT_3D ( 'NONE', #82952, #9047, #59221 ) ;
#57835 = LINE ( 'NONE', #79606, #11156 ) ;
#57836 = CARTESIAN_POINT ( 'NONE',  ( -24.82643806938782660, 304.4615624795510485, 10.29204873707470291 ) ) ;
#57837 = CARTESIAN_POINT ( 'NONE',  ( -33.74586796234814301, 434.0087061791907104, 12.79535379566283027 ) ) ;
#57838 = EDGE_CURVE ( 'NONE', #27223, #58214, #59898, .T. ) ;
#57839 = VERTEX_POINT ( 'NONE', #95419 ) ;
#57840 = CARTESIAN_POINT ( 'NONE',  ( 4.322797252088989239, 141.1113215272794434, 5.000000000000000000 ) ) ;
#57841 = CARTESIAN_POINT ( 'NONE',  ( 16.68184208837833538, 18.64284798592490944, -34.62135284424456927 ) ) ;
#57842 = CARTESIAN_POINT ( 'NONE',  ( 86.84319104226476327, -46.45793329604330069, 190.7102553128401894 ) ) ;
#57843 = ADVANCED_FACE ( 'NONE', ( #13953 ), #37303, .T. ) ;
#57844 = CARTESIAN_POINT ( 'NONE',  ( 1.130275170373804983, 34.42238785691029079, -29.03978118008791398 ) ) ;
#57845 = CARTESIAN_POINT ( 'NONE',  ( -5.082755093536326818, -30.21875000204838813, 5.082755093536325042 ) ) ;
#57846 = CARTESIAN_POINT ( 'NONE',  ( 36.30372750213987842, -36.17305495503135404, 45.48833120993651136 ) ) ;
#57847 = LINE ( 'NONE', #98327, #104276 ) ;
#57848 = ADVANCED_FACE ( 'NONE', ( #63604 ), #14473, .T. ) ;
#57849 = FACE_OUTER_BOUND ( 'NONE', #96559, .T. ) ;
#57850 = CARTESIAN_POINT ( 'NONE',  ( 34.11633748533821375, 439.1270573268431008, 24.05964454602017710 ) ) ;
#57851 = VECTOR ( 'NONE', #69977, 1000.000000000000000 ) ;
#57852 = APPLICATION_PROTOCOL_DEFINITION ( 'draft international standard', 'automotive_design', 1998, #28730 ) ;
#57853 = CARTESIAN_POINT ( 'NONE',  ( -9.699016383038316036, 33.17638171448344764, 2.444973590251029449 ) ) ;
#57854 = EDGE_LOOP ( 'NONE', ( #104770, #98884, #6133, #62361, #65938, #35529 ) ) ;
#57855 = EDGE_CURVE ( 'NONE', #102954, #37530, #21820, .T. ) ;
#57856 = CARTESIAN_POINT ( 'NONE',  ( 0.1691482177511390850, 43.17849576545665258, 18.74134708137945537 ) ) ;
#57857 = CARTESIAN_POINT ( 'NONE',  ( 0.000000000000000000, 0.000000000000000000, 25.00000000000000000 ) ) ;
#57858 = CARTESIAN_POINT ( 'NONE',  ( 1.262844703064978993E-15, -3.000000000000002665, -95.00000000000000000 ) ) ;
#57859 = CARTESIAN_POINT ( 'NONE',  ( 12.13034742782246767, 42.00000000000000000, -93.82352941176338845 ) ) ;
#57860 = TOROIDAL_SURFACE ( 'NONE', #54384, 8.500000000000000000, 0.5000000000000000000 ) ;
#57861 = EDGE_LOOP ( 'NONE', ( #63549, #41262, #1551, #49760, #79830, #43811, #24772, #54305 ) ) ;
#57862 = DIRECTION ( 'NONE',  ( -0.5735764363510497121, 0.8191520442889892450, 1.003171929053521665E-16 ) ) ;
#57863 = DIRECTION ( 'NONE',  ( 0.000000000000000000, 0.000000000000000000, -1.000000000000000000 ) ) ;
#57864 = VECTOR ( 'NONE', #68200, 1000.000000000000114 ) ;
#57865 = CARTESIAN_POINT ( 'NONE',  ( 107.4062233239980628, -57.67121751121231910, 112.8259166854166011 ) ) ;
#57866 = CARTESIAN_POINT ( 'NONE',  ( 36.69890166230473483, 463.9786769757893694, 19.62055820434390441 ) ) ;
#57867 = DIRECTION ( 'NONE',  ( 0.000000000000000000, 1.000000000000000000, -1.224646799147353207E-16 ) ) ;
#57868 = DIRECTION ( 'NONE',  ( -1.000000000000000000, -0.000000000000000000, -0.000000000000000000 ) ) ;
#57869 = COLOUR_RGB ( '', 0.31764706, 0.68627451, 0.89019608) ;
#57870 = CARTESIAN_POINT ( 'NONE',  ( 36.31401350675979245, 26.07298798432232090, 12.06078247660970071 ) ) ;
#57871 = CARTESIAN_POINT ( 'NONE',  ( -79.13069157080136051, -59.99999999999999289, 194.8111473548646586 ) ) ;
#57872 = AXIS2_PLACEMENT_3D ( 'NONE', #22831, #65385, #56192 ) ;
#57873 = STYLED_ITEM ( 'NONE', ( #28125 ), #57542 ) ;
#57874 = CARTESIAN_POINT ( 'NONE',  ( -22.20318009218133071, 295.0333587257888439, 9.975590323731541531 ) ) ;
#57875 = SURFACE_SIDE_STYLE ('',( #65458 ) ) ;
#57876 = CARTESIAN_POINT ( 'NONE',  ( -54.34415824576156950, 50.00000000000000000, -32.38913437803946493 ) ) ;
#57877 = CARTESIAN_POINT ( 'NONE',  ( -86.39708987185247224, -17.44928839871576542, 178.9058496263539837 ) ) ;
#57878 = ORIENTED_EDGE ( 'NONE', *, *, #51003, .T. ) ;
#57879 = CARTESIAN_POINT ( 'NONE',  ( 30.01939835712524030, 309.6846599134693747, -8.656694015688147559 ) ) ;
#57880 = AXIS2_PLACEMENT_3D ( 'NONE', #13010, #46464, #77773 ) ;
#57881 = VERTEX_POINT ( 'NONE', #62533 ) ;
#57882 = CARTESIAN_POINT ( 'NONE',  ( 40.34715123528543046, 5.000000000000015099, 6.123233995736782060E-16 ) ) ;
#57883 = EDGE_CURVE ( 'NONE', #93742, #17674, #29147, .T. ) ;
#57884 = CARTESIAN_POINT ( 'NONE',  ( -119.9999999999999432, 0.000000000000000000, -60.00000000000001421 ) ) ;
#57885 = CARTESIAN_POINT ( 'NONE',  ( -87.00156809400746738, -60.21405852097385036, -8.689177619207773873 ) ) ;
#57886 = CARTESIAN_POINT ( 'NONE',  ( -5.446322446741861611, -11.07408952718066075, -10.13262891269602228 ) ) ;
#57887 =( NAMED_UNIT ( * ) PLANE_ANGLE_UNIT ( ) SI_UNIT ( $, .RADIAN. ) );
#57888 = ORIENTED_EDGE ( 'NONE', *, *, #27558, .F. ) ;
#57889 = FACE_OUTER_BOUND ( 'NONE', #49515, .T. ) ;
#57890 = CARTESIAN_POINT ( 'NONE',  ( 12.30767636227396267, 22.34822279547523749, -6.380817737059023109 ) ) ;
#57891 = EDGE_CURVE ( 'NONE', #45623, #99282, #92370, .T. ) ;
#57892 = ADVANCED_FACE ( 'NONE', ( #87342 ), #87236, .T. ) ;
#57893 = CARTESIAN_POINT ( 'NONE',  ( -8.569529079657698389, -1.734723475976807094E-15, -14.86825985027703290 ) ) ;
#57894 = CARTESIAN_POINT ( 'NONE',  ( -35.46984665180946905, 438.0686027085576484, 4.109636340060087711 ) ) ;
#57895 = CARTESIAN_POINT ( 'NONE',  ( 8.180134260905338905, -14.21045842199436926, -37.25106736021741227 ) ) ;
#57896 = CARTESIAN_POINT ( 'NONE',  ( -79.59015944166391421, -29.08934217562258695, 133.2666643165789822 ) ) ;
#57897 = ORIENTED_EDGE ( 'NONE', *, *, #44988, .F. ) ;
#57898 = CARTESIAN_POINT ( 'NONE',  ( 71.69540001792421435, -59.99999999999999289, 172.8810247122642352 ) ) ;
#57899 = CARTESIAN_POINT ( 'NONE',  ( 7.986468734911285949, 88.97313679723080782, 0.5341897780976110344 ) ) ;
#57900 = CARTESIAN_POINT ( 'NONE',  ( 110.2837989784263044, -57.66912168954863205, 195.5935479797663277 ) ) ;
#57901 = ORIENTED_EDGE ( 'NONE', *, *, #41239, .F. ) ;
#57902 = DIRECTION ( 'NONE',  ( -1.000000000000000000, -1.224606353822377258E-16, -0.000000000000000000 ) ) ;
#57903 = DIRECTION ( 'NONE',  ( 0.4165977904505305252, 0.000000000000000000, 0.9090909090909092827 ) ) ;
#57904 = VERTEX_POINT ( 'NONE', #95961 ) ;
#57905 = CONICAL_SURFACE ( 'NONE', #81996, 4.000000000000001776, 0.9599310885968808105 ) ;
#57906 = CARTESIAN_POINT ( 'NONE',  ( 3.787655175481866809, 16.54064103469220015, -5.887936971919406126 ) ) ;
#57907 = CARTESIAN_POINT ( 'NONE',  ( -2.500000000000001332, 0.000000000000000000, 0.000000000000000000 ) ) ;
#57908 = CARTESIAN_POINT ( 'NONE',  ( 4.699999999999999289, 0.000000000000000000, 0.000000000000000000 ) ) ;
#57909 = CARTESIAN_POINT ( 'NONE',  ( -5.082755093536326818, -12.21875000204838635, 5.082755093536325042 ) ) ;
#57910 = CARTESIAN_POINT ( 'NONE',  ( -0.2779000157839468521, -8.820699686765063774, -7.928862157988307402 ) ) ;
#57911 = AXIS2_PLACEMENT_3D ( 'NONE', #94565, #20715, #53553 ) ;
#57912 = CARTESIAN_POINT ( 'NONE',  ( 9.333079356992099562, 83.22166919925130912, 3.592383266237784589 ) ) ;
#57913 =( LENGTH_UNIT ( ) NAMED_UNIT ( * ) SI_UNIT ( .MILLI., .METRE. ) );
#57914 = CARTESIAN_POINT ( 'NONE',  ( -7.908219015560238319, -3.084967917785943037, -7.795665562178440311 ) ) ;
#57915 = CARTESIAN_POINT ( 'NONE',  ( 43.00000000000000000, 436.0987441542287115, 7.567257455462728544 ) ) ;
#57916 = EDGE_CURVE ( 'NONE', #27903, #41040, #39044, .T. ) ;
#57917 = B_SPLINE_CURVE_WITH_KNOTS ( 'NONE', 3,
 ( #56316, #96817, #22949, #81140, #47179, #6188, #55784, #7249, #17499, #8315, #100516, #81654, #67638, #49293, #50889, #82199, #57923, #65505, #24542, #74105, #9907, #716 ),
 .UNSPECIFIED., .F., .F.,
 ( 4, 2, 2, 2, 2, 2, 2, 2, 2, 2, 4 ),
 ( 0.002790526113034574960, 0.003042863289720283172, 0.003295200466405991818, 0.003799874819777412146, 0.004052211996463120358, 0.004304549173148828137, 0.004809223526520248898, 0.005313897879891668792, 0.005818572233263088686, 0.006323246586634508580, 0.006827920940005928474 ),
 .UNSPECIFIED. ) ;
#57918 = B_SPLINE_CURVE_WITH_KNOTS ( 'NONE', 3,
 ( #65533, #31080, #57415, #63959 ),
 .UNSPECIFIED., .F., .F.,
 ( 4, 4 ),
 ( 0.000000000000000000, 0.0007558628827956282055 ),
 .UNSPECIFIED. ) ;
#57919 = VERTEX_POINT ( 'NONE', #53374 ) ;
#57920 = CARTESIAN_POINT ( 'NONE',  ( -6.872826227116265230, 41.26098032275474026, -70.68506212612362560 ) ) ;
#57922 = CARTESIAN_POINT ( 'NONE',  ( 30.84614831813113511, -36.01525104246629638, 32.80693974661438261 ) ) ;
#57921 =( NAMED_UNIT ( * ) PLANE_ANGLE_UNIT ( ) SI_UNIT ( $, .RADIAN. ) );
#57923 = CARTESIAN_POINT ( 'NONE',  ( -4.298373348636018498, 51.67582542842902171, -8.058508091860746347 ) ) ;
#57924 = ORIENTED_EDGE ( 'NONE', *, *, #85905, .F. ) ;
#57925 = ADVANCED_FACE ( 'NONE', ( #77651 ), #68299, .T. ) ;
#57926 = DIRECTION ( 'NONE',  ( 0.000000000000000000, -0.000000000000000000, 1.000000000000000000 ) ) ;
#57927 = ORIENTED_EDGE ( 'NONE', *, *, #31728, .T. ) ;
#57929 = CARTESIAN_POINT ( 'NONE',  ( -8.716576110315918058, -5.000000000000000000, 5.062272329162047946 ) ) ;
#57928 = FACE_OUTER_BOUND ( 'NONE', #18613, .T. ) ;
#57930 = DIRECTION ( 'NONE',  ( -1.000000000000000000, -1.224606353822377258E-16, -0.000000000000000000 ) ) ;
#57931 = CARTESIAN_POINT ( 'NONE',  ( 45.94900261086841198, 1.482358050883964840E-15, 0.000000000000000000 ) ) ;
#57932 = LINE ( 'NONE', #76249, #20590 ) ;
#57933 = DIRECTION ( 'NONE',  ( -1.000000000000000000, -1.224606353822377258E-16, -0.000000000000000000 ) ) ;
#57934 = CARTESIAN_POINT ( 'NONE',  ( -35.67416790563066087, 463.3851398029171946, 19.97299141547693324 ) ) ;
#57935 = ORIENTED_EDGE ( 'NONE', *, *, #50187, .F. ) ;
#57936 = CARTESIAN_POINT ( 'NONE',  ( 90.93490407631915673, -60.00000000000000711, -17.09726446340970440 ) ) ;
#57937 = CARTESIAN_POINT ( 'NONE',  ( -10.45113867624388071, 45.35217484112028075, -15.40779740156158084 ) ) ;
#57938 = CARTESIAN_POINT ( 'NONE',  ( -15.91602873225749981, -2.171392360670797217, 14.84268258422452291 ) ) ;
#57939 = CARTESIAN_POINT ( 'NONE',  ( 40.62042009609988469, 488.7249922674043887, 10.90475042733721978 ) ) ;
#57940 = CARTESIAN_POINT ( 'NONE',  ( 5.799999999999999822, 0.000000000000000000, 0.000000000000000000 ) ) ;
#57941 = ORIENTED_EDGE ( 'NONE', *, *, #17952, .T. ) ;
#57942 = CARTESIAN_POINT ( 'NONE',  ( -46.00000000000000000, 450.0000000000002274, 13.20242257375370976 ) ) ;
#57943 = ORIENTED_EDGE ( 'NONE', *, *, #5860, .T. ) ;
#57944 = ORIENTED_EDGE ( 'NONE', *, *, #1204, .T. ) ;
#57945 =( LENGTH_UNIT ( ) NAMED_UNIT ( * ) SI_UNIT ( .MILLI., .METRE. ) );
#57946 = CARTESIAN_POINT ( 'NONE',  ( -15.99012395148572629, 34.48504170391973389, -24.06089424805132992 ) ) ;
#57947 = CARTESIAN_POINT ( 'NONE',  ( 23.56341839161319740, 303.7214408960188621, 10.12591315008080706 ) ) ;
#57949 = CARTESIAN_POINT ( 'NONE',  ( 85.73991738122207096, -52.74049725067960281, -5.625651811223429277 ) ) ;
#57948 = AXIS2_PLACEMENT_3D ( 'NONE', #100333, #26498, #84693 ) ;
#57950 = CARTESIAN_POINT ( 'NONE',  ( -45.46260347522193968, 379.8339907270314484, 7.111986633017085779 ) ) ;
#57951 = CARTESIAN_POINT ( 'NONE',  ( -5.876235947983078134, -64.54950742897155180, 14.29271017806149047 ) ) ;
#57952 = CARTESIAN_POINT ( 'NONE',  ( 12.50000000000000711, 33.88168340297682590, -52.67689954243009964 ) ) ;
#57953 = EDGE_LOOP ( 'NONE', ( #33493, #29604, #77706, #48700 ) ) ;
#57954 = CARTESIAN_POINT ( 'NONE',  ( 30.59731729458148664, 7.793314453875814785, 41.71112871039118630 ) ) ;
#57955 = VERTEX_POINT ( 'NONE', #73241 ) ;
#57956 = CARTESIAN_POINT ( 'NONE',  ( -7.036764705882382565, 40.00000000007575807, -71.06385277390852195 ) ) ;
#57957 = CARTESIAN_POINT ( 'NONE',  ( -86.22319347886272567, -38.62792923045453364, 199.1968256833580995 ) ) ;
#57958 = CARTESIAN_POINT ( 'NONE',  ( 42.74056876569563457, 464.8122885126885535, 15.63399960026069024 ) ) ;
#57959 = CIRCLE ( 'NONE', #63140, 3.309500000000007880 ) ;
#57960 = MECHANICAL_DESIGN_GEOMETRIC_PRESENTATION_REPRESENTATION (  '', ( #4541 ), #80357 ) ;
#57961 = AXIS2_PLACEMENT_3D ( 'NONE', #98285, #66996, #16849 ) ;
#57962 = AXIS2_PLACEMENT_3D ( 'NONE', #105267, #31, #90145 ) ;
#57964 = ORIENTED_EDGE ( 'NONE', *, *, #105868, .F. ) ;
#57963 = CARTESIAN_POINT ( 'NONE',  ( 6.026974479199131350E-05, -59.99999999999998579, 33.88964995960238014 ) ) ;
#57965 = CARTESIAN_POINT ( 'NONE',  ( 70.47143424281389912, -46.43366363250593309, 107.5507350962775490 ) ) ;
#57966 = B_SPLINE_CURVE_WITH_KNOTS ( 'NONE', 3,
 ( #1142, #83157, #66988, #76122, #90725, #99869, #65911, #16839, #2218, #35168, #26042, #68035, #57266, #82080, #8199, #41110, #74, #33045, #36251, #4904, #28679, #37300, #70166, #3845, #19537, #92837, #10838, #29225, #27625, #94459, #19001, #61563 ),
 .UNSPECIFIED., .F., .F.,
 ( 4, 2, 2, 2, 2, 2, 2, 2, 2, 2, 2, 2, 2, 2, 2, 4 ),
 ( 0.01223842624040716656, 0.01316182229273517301, 0.01362352031889916930, 0.01408521834506316732, 0.01431606735814517500, 0.01454691637122718442, 0.01477776538430919037, 0.01500861439739119979, 0.01523946341047320747, 0.01547031242355521342, 0.01593201044971922359, 0.01639370847588323202, 0.01685540650204724045, 0.01777880255437524690, 0.01870219860670325335, 0.01962559465903125980 ),
 .UNSPECIFIED. ) ;
#57967 = AXIS2_PLACEMENT_3D ( 'NONE', #4722, #31149, #64036 ) ;
#57968 = ORIENTED_EDGE ( 'NONE', *, *, #94074, .T. ) ;
#57969 = CARTESIAN_POINT ( 'NONE',  ( 17.50000000000002842, 49.00623182211167972, 64.05145124195381356 ) ) ;
#57970 = CARTESIAN_POINT ( 'NONE',  ( -7.188101187500000933, -29.00000000204838813, -2.977408999572651371 ) ) ;
#57971 = CARTESIAN_POINT ( 'NONE',  ( -99.13865059541491576, -57.67127950436278638, 63.61738387431689290 ) ) ;
#57972 = ADVANCED_FACE ( 'NONE', ( #80816 ), #16623, .T. ) ;
#57973 = ORIENTED_EDGE ( 'NONE', *, *, #72818, .F. ) ;
#57974 = EDGE_CURVE ( 'NONE', #2814, #7688, #32300, .T. ) ;
#57975 = DIRECTION ( 'NONE',  ( 0.8191520442889884679, 0.000000000000000000, 0.5735764363510508224 ) ) ;
#57976 = EDGE_CURVE ( 'NONE', #68447, #56015, #6285, .T. ) ;
#57977 = CARTESIAN_POINT ( 'NONE',  ( -35.17753024347793911, 490.3634983170154555, 12.17893648721504007 ) ) ;
#57978 = DIRECTION ( 'NONE',  ( -1.000000000000000000, -1.224606353822377258E-16, -0.000000000000000000 ) ) ;
#57979 = CARTESIAN_POINT ( 'NONE',  ( -1.469576158976823947E-15, -26.56250000409677270, 8.000000000000000000 ) ) ;
#57980 = DIRECTION ( 'NONE',  ( -1.000000000000000000, -1.224606353822377258E-16, -0.000000000000000000 ) ) ;
#57981 = CARTESIAN_POINT ( 'NONE',  ( 0.000000000000000000, -30.00000000000000000, 0.000000000000000000 ) ) ;
#57982 = B_SPLINE_CURVE_WITH_KNOTS ( 'NONE', 3,
 ( #42956, #26808, #9500, #25754, #59681, #18710, #11092, #76908, #35970, #17093, #41878, #74767, #4095, #79037, #79564, #37023, #5158, #86630, #62870, #94717, #102249, #103838, #95758, #69892, #70426, #54742, #21897, #4629, #21367, #77978, #87675, #45624, #12694, #78498 ),
 .UNSPECIFIED., .F., .F.,
 ( 4, 2, 2, 2, 2, 2, 2, 2, 2, 2, 2, 2, 2, 2, 2, 2, 4 ),
 ( 0.000000000000000000, 0.03125000000000000000, 0.06250000000000000000, 0.09375000000000000000, 0.1250000000000000000, 0.1562500000000000000, 0.1875000000000000000, 0.2187500000000000000, 0.2500000000000000000, 0.2812500000000000000, 0.3125000000000000000, 0.3437500000000000000, 0.3750000000000000000, 0.4062500000000000000, 0.4375000000000000000, 0.4687500000000000000, 0.5000000000000000000 ),
 .UNSPECIFIED. ) ;
#57983 = EDGE_CURVE ( 'NONE', #45464, #86829, #59757, .T. ) ;
#57984 = CONICAL_SURFACE ( 'NONE', #51125, 5.000000000000010658, 0.9599310885968697082 ) ;
#57985 = CARTESIAN_POINT ( 'NONE',  ( 9.221216839714866609, 31.04759748168974198, 3.869414262756994294 ) ) ;
#57986 = FACE_OUTER_BOUND ( 'NONE', #40505, .T. ) ;
#57987 = DIRECTION ( 'NONE',  ( 1.000000000000000000, 0.000000000000000000, 0.000000000000000000 ) ) ;
#57988 = CARTESIAN_POINT ( 'NONE',  ( -4.210530276627872937, 14.99999999999998934, -10.00000000000003908 ) ) ;
#57989 = ORIENTED_EDGE ( 'NONE', *, *, #26674, .T. ) ;
#57990 = EDGE_CURVE ( 'NONE', #35053, #10091, #54550, .T. ) ;
#57991 = FILL_AREA_STYLE_COLOUR ( '', #93921 ) ;
#57992 = VECTOR ( 'NONE', #43734, 1000.000000000000000 ) ;
#57993 = CARTESIAN_POINT ( 'NONE',  ( -5.000000000000000000, -19.72303380912273951, -4.527417031999413588 ) ) ;
#57994 = CARTESIAN_POINT ( 'NONE',  ( -91.21773797973978049, -30.00000000000000711, 190.5815255630674585 ) ) ;
#57995 = CARTESIAN_POINT ( 'NONE',  ( 37.72580964046798613, 25.70160911691909433, -10.95617127781097899 ) ) ;
#57996 = CARTESIAN_POINT ( 'NONE',  ( 70.42594083886010026, -57.68248469520420230, 157.4904543252067981 ) ) ;
#57998 = CARTESIAN_POINT ( 'NONE',  ( -7.983737360691460339, 6.035846803540888317, 4.337628496855524318 ) ) ;
#57997 = CARTESIAN_POINT ( 'NONE',  ( 5.668940197363838251, 41.88723871811491506, -59.02759513106027356 ) ) ;
#57999 = CARTESIAN_POINT ( 'NONE',  ( 19.29301913843075411, -25.57889320560503066, -38.49290569165957976 ) ) ;
#58000 = CARTESIAN_POINT ( 'NONE',  ( -0.3334083441215401900, 43.18996287760407427, 18.70763396291626179 ) ) ;
#58001 = CARTESIAN_POINT ( 'NONE',  ( -37.50059943756144776, 490.7879993827797307, 12.38039871356719246 ) ) ;
#58002 = CARTESIAN_POINT ( 'NONE',  ( -47.20193715881740815, -60.00000000000001421, 65.23073768148172746 ) ) ;
#58003 = CARTESIAN_POINT ( 'NONE',  ( 16.52731600354976393, 43.98685737190850631, -87.77869701378344303 ) ) ;
#58004 = FACE_OUTER_BOUND ( 'NONE', #7086, .T. ) ;
#58005 = CIRCLE ( 'NONE', #33959, 9.999999999999994671 ) ;
#58006 = CARTESIAN_POINT ( 'NONE',  ( -87.01762278567609599, -46.44878082088867188, 190.9316993270498699 ) ) ;
#58007 = ORIENTED_EDGE ( 'NONE', *, *, #15874, .T. ) ;
#58008 = CARTESIAN_POINT ( 'NONE',  ( 18.91772294278459654, 48.00000000000000000, 62.18609455171460354 ) ) ;
#58009 = CARTESIAN_POINT ( 'NONE',  ( 7.157676179766298219, -15.10646866768545138, 14.96459782267552718 ) ) ;
#58010 = CARTESIAN_POINT ( 'NONE',  ( -8.339494512690995620, -60.36589398885404023, 33.94454140269643005 ) ) ;
#58011 = CARTESIAN_POINT ( 'NONE',  ( -6.511374603264941996, 41.81948973637988587, -59.12906223371311398 ) ) ;
#58012 = CARTESIAN_POINT ( 'NONE',  ( 4.691239167085950790, -66.59475614380380648, 13.79106926437629355 ) ) ;
#58013 = VERTEX_POINT ( 'NONE', #99114 ) ;
#58014 = LINE ( 'NONE', #91989, #78295 ) ;
#58015 = CARTESIAN_POINT ( 'NONE',  ( -5.689604056833319490, -4.325321803341545923, -16.92223617909959898 ) ) ;
#58016 = CARTESIAN_POINT ( 'NONE',  ( 15.52452758388592535, 34.97031437783925867, 22.76750761962476233 ) ) ;
#58017 = AXIS2_PLACEMENT_3D ( 'NONE', #22102, #86835, #45832 ) ;
#58018 = AXIS2_PLACEMENT_3D ( 'NONE', #102211, #20824, #94678 ) ;
#58019 = CARTESIAN_POINT ( 'NONE',  ( 29.85885434071563438, 307.6868234535251645, -8.901958748380083719 ) ) ;
#58020 = CARTESIAN_POINT ( 'NONE',  ( 0.000000000000000000, 6.123233995736767268E-16, -5.000000000000000888 ) ) ;
#58021 = ADVANCED_FACE ( 'NONE', ( #33361 ), #81336, .F. ) ;
#58022 = CARTESIAN_POINT ( 'NONE',  ( -7.934203308536662114, -81.13299659982200751, 1.057099537198545214 ) ) ;
#58023 = CARTESIAN_POINT ( 'NONE',  ( 32.15166163075728178, 486.0589784586659903, 5.199393881400817818 ) ) ;
#58024 = CARTESIAN_POINT ( 'NONE',  ( 105.3887446370168135, -14.21045842199438347, 188.2131443117102663 ) ) ;
#58025 = FACE_OUTER_BOUND ( 'NONE', #56484, .T. ) ;
#58026 = ORIENTED_EDGE ( 'NONE', *, *, #94623, .F. ) ;
#58027 = DIRECTION ( 'NONE',  ( 0.000000000000000000, -1.000000000000000000, 0.000000000000000000 ) ) ;
#58028 = CARTESIAN_POINT ( 'NONE',  ( 0.000000000000000000, -6.928203230275504332, 4.000000000000007105 ) ) ;
#58029 = PRESENTATION_LAYER_ASSIGNMENT (  '', '', ( #102787 ) ) ;
#58030 = AXIS2_PLACEMENT_3D ( 'NONE', #8521, #41424, #81863 ) ;
#58031 = DIRECTION ( 'NONE',  ( -1.000000000000000000, -1.224606353822377258E-16, -0.000000000000000000 ) ) ;
#58033 = ADVANCED_FACE ( 'NONE', ( #40362 ), #48965, .F. ) ;
#58032 = CARTESIAN_POINT ( 'NONE',  ( 4.322797252088743214, 10.88867847272319977, -4.999999999999997335 ) ) ;
#58034 = CARTESIAN_POINT ( 'NONE',  ( -14.29190075645216851, 12.99999999999999289, 0.000000000000000000 ) ) ;
#58035 = EDGE_LOOP ( 'NONE', ( #69086, #70462, #40451, #12246 ) ) ;
#58036 = UNCERTAINTY_MEASURE_WITH_UNIT (LENGTH_MEASURE( 1.000000000000000082E-05 ), #61330, 'distance_accuracy_value', 'NONE');
#58037 = CIRCLE ( 'NONE', #71741, 8.000000000000000000 ) ;
#58038 = CARTESIAN_POINT ( 'NONE',  ( -21.11705751644940676, 305.0273488488396083, 8.974472976378370603 ) ) ;
#58039 = VERTEX_POINT ( 'NONE', #74318 ) ;
#58040 = CARTESIAN_POINT ( 'NONE',  ( 36.23096140414229183, 484.5285253001270007, -2.435173044881263404 ) ) ;
#58041 = EDGE_CURVE ( 'NONE', #79135, #83753, #58138, .T. ) ;
#58042 = PRESENTATION_STYLE_ASSIGNMENT (( #66139 ) ) ;
#58043 = CARTESIAN_POINT ( 'NONE',  ( 9.882762594765912567, 45.48558064014432745, 15.34364832776098275 ) ) ;
#58044 = ORIENTED_EDGE ( 'NONE', *, *, #92025, .T. ) ;
#58045 = CARTESIAN_POINT ( 'NONE',  ( -28.89099332390824770, 48.00000000000000000, 58.53034795347328867 ) ) ;
#58046 = CARTESIAN_POINT ( 'NONE',  ( 5.000000000000000000, -13.99860067247109896, 11.59399192991907057 ) ) ;
#58047 = CARTESIAN_POINT ( 'NONE',  ( -74.29828176229183612, -59.99999999998045297, 190.2516943755762782 ) ) ;
#58048 = CARTESIAN_POINT ( 'NONE',  ( 46.00000000000000000, 435.9844294008496490, 14.35633708101140193 ) ) ;
#58049 = ORIENTED_EDGE ( 'NONE', *, *, #27716, .F. ) ;
#58050 = CARTESIAN_POINT ( 'NONE',  ( 111.9397786006664148, -59.99999999999998579, 163.4467576686174084 ) ) ;
#58052 = CARTESIAN_POINT ( 'NONE',  ( 16.89471477245463404, -46.43465090273242879, 31.87823083279425873 ) ) ;
#58051 = CARTESIAN_POINT ( 'NONE',  ( -99.17463707058834643, -30.00000000000003908, 199.4944348318372818 ) ) ;
#58053 = CARTESIAN_POINT ( 'NONE',  ( 83.27846995605888480, -37.99999999999998579, -8.029241552981964958 ) ) ;
#58054 = DIRECTION ( 'NONE',  ( -0.000000000000000000, -1.000000000000000000, -0.000000000000000000 ) ) ;
#58055 = EDGE_CURVE ( 'NONE', #57692, #74342, #47386, .T. ) ;
#58056 = CARTESIAN_POINT ( 'NONE',  ( -41.83504579204735307, -56.80130521720823111, 44.35147145462004659 ) ) ;
#58057 = CARTESIAN_POINT ( 'NONE',  ( 0.000000000000000000, 0.000000000000000000, 0.000000000000000000 ) ) ;
#58058 = ORIENTED_EDGE ( 'NONE', *, *, #101530, .F. ) ;
#58059 = CARTESIAN_POINT ( 'NONE',  ( 17.81438722625302518, -5.000000000000000000, 6.123233995736768255E-16 ) ) ;
#58060 = CARTESIAN_POINT ( 'NONE',  ( 24.60488647473181345, 306.9835580411500473, 10.41807558718820914 ) ) ;
#58061 =( LENGTH_UNIT ( ) NAMED_UNIT ( * ) SI_UNIT ( .MILLI., .METRE. ) );
#58062 = ADVANCED_FACE ( 'NONE', ( #80278 ), #45964, .T. ) ;
#58063 = CARTESIAN_POINT ( 'NONE',  ( 2.985641311035224431E-22, 35.08181111624585213, -27.25000000000000000 ) ) ;
#58064 = DIRECTION ( 'NONE',  ( 0.000000000000000000, -1.000000000000000000, 0.000000000000000000 ) ) ;
#58065 = ORIENTED_EDGE ( 'NONE', *, *, #47430, .T. ) ;
#58066 = CARTESIAN_POINT ( 'NONE',  ( 4.188755055078837941, -48.42812442300451892, 102.8981131900555113 ) ) ;
#58067 = ORIENTED_EDGE ( 'NONE', *, *, #21101, .F. ) ;
#58068 = CARTESIAN_POINT ( 'NONE',  ( 78.46489409920162927, -30.00000000000490630, 185.0055361782710861 ) ) ;
#58069 = DIRECTION ( 'NONE',  ( -0.000000000000000000, 0.2521971900442987469, 0.9676758637755517034 ) ) ;
#58070 = CARTESIAN_POINT ( 'NONE',  ( 40.59999999999999432, 1.533819458162526451E-15, 0.000000000000000000 ) ) ;
#58071 = AXIS2_PLACEMENT_3D ( 'NONE', #104942, #31085, #63963 ) ;
#58072 = DIRECTION ( 'NONE',  ( 0.000000000000000000, -1.000000000000000000, 0.000000000000000000 ) ) ;
#58073 = CARTESIAN_POINT ( 'NONE',  ( 81.06826635177107221, -29.99999999999999645, 22.19813494082483984 ) ) ;
#58074 = CARTESIAN_POINT ( 'NONE',  ( 7.550180524134850302, 101.9944075278681197, 2.651855549982494065 ) ) ;
#58075 = VERTEX_POINT ( 'NONE', #55987 ) ;
#58076 = VERTEX_POINT ( 'NONE', #15017 ) ;
#58077 = EDGE_LOOP ( 'NONE', ( #69898, #94226 ) ) ;
#58078 = CARTESIAN_POINT ( 'NONE',  ( -33.94783393359910662, 484.1261039197349305, 1.321740980884785532 ) ) ;
#58079 = CARTESIAN_POINT ( 'NONE',  ( 22.07915843411224444, 26.01897790090626827, 31.43308708091262105 ) ) ;
#58080 = DIRECTION ( 'NONE',  ( 1.224646799147349509E-16, 0.000000000000000000, -1.000000000000000000 ) ) ;
#58081 = CYLINDRICAL_SURFACE ( 'NONE', #18771, 1.249999999999999334 ) ;
#58082 = CARTESIAN_POINT ( 'NONE',  ( -31.35993980847401374, 436.8059452921889942, 22.71850044363437249 ) ) ;
#58083 = CARTESIAN_POINT ( 'NONE',  ( 92.82022815836235452, 1.016364837396684119E-14, 0.000000000000000000 ) ) ;
#58084 = AXIS2_PLACEMENT_3D ( 'NONE', #75026, #26021, #91771 ) ;
#58085 = ORIENTED_EDGE ( 'NONE', *, *, #55756, .T. ) ;
#58086 = EDGE_CURVE ( 'NONE', #5588, #37464, #61535, .T. ) ;
#58087 = SURFACE_STYLE_USAGE ( .BOTH. , #346 ) ;
#58088 = ORIENTED_EDGE ( 'NONE', *, *, #49927, .T. ) ;
#58089 = B_SPLINE_CURVE_WITH_KNOTS ( 'NONE', 3,
 ( #36145, #36674, #78144, #94886, #21537, #21030, #53866, #69536, #101890, #44739 ),
 .UNSPECIFIED., .F., .F.,
 ( 4, 2, 2, 2, 4 ),
 ( 1.734723475976807094E-18, 0.001638027434153875844, 0.003276054868307749952, 0.004914082302461623628, 0.006552109736615498170 ),
 .UNSPECIFIED. ) ;
#58090 = CARTESIAN_POINT ( 'NONE',  ( 0.000000000000000000, 6.123233995736770227E-16, -5.000000000000002665 ) ) ;
#58091 = CARTESIAN_POINT ( 'NONE',  ( 82.51873517505984523, -38.82767313688965061, 196.4555416342311673 ) ) ;
#58092 = CARTESIAN_POINT ( 'NONE',  ( 5.947762761376477414, 2.501851166488378908, 6.500000000000000000 ) ) ;
#58093 = CARTESIAN_POINT ( 'NONE',  ( 30.53436373644603563, 298.8120125249405419, 10.81965208238480614 ) ) ;
#58094 = AXIS2_PLACEMENT_3D ( 'NONE', #42749, #20119, #19051 ) ;
#58095 = DIRECTION ( 'NONE',  ( -1.000000000000000000, 0.000000000000000000, 0.000000000000000000 ) ) ;
#58096 = AXIS2_PLACEMENT_3D ( 'NONE', #85868, #3332, #45396 ) ;
#58097 = CARTESIAN_POINT ( 'NONE',  ( -41.70256300459701038, 461.0340457114389210, 3.032228049028218297 ) ) ;
#58098 = CARTESIAN_POINT ( 'NONE',  ( -4.999999999999993783, -45.99999999999999289, 103.2791840072761858 ) ) ;
#58099 = DIRECTION ( 'NONE',  ( -1.000000000000000000, -0.000000000000000000, -0.000000000000000000 ) ) ;
#58100 = EDGE_CURVE ( 'NONE', #62536, #40876, #56530, .T. ) ;
#58101 = VERTEX_POINT ( 'NONE', #52171 ) ;
#58102 = CARTESIAN_POINT ( 'NONE',  ( -22.22335123492370101, 303.2512051409928517, 10.02280941442790585 ) ) ;
#58103 = UNCERTAINTY_MEASURE_WITH_UNIT (LENGTH_MEASURE( 1.000000000000000082E-05 ), #75743, 'distance_accuracy_value', 'NONE');
#58104 = EDGE_CURVE ( 'NONE', #35426, #63670, #11168, .T. ) ;
#58105 = DIRECTION ( 'NONE',  ( -1.000000000000000000, -1.224606353822377258E-16, -0.000000000000000000 ) ) ;
#58106 = DIRECTION ( 'NONE',  ( -0.000000000000000000, -0.000000000000000000, -1.000000000000000000 ) ) ;
#58107 = CIRCLE ( 'NONE', #11592, 3.309500000000001663 ) ;
#58109 = CARTESIAN_POINT ( 'NONE',  ( 38.09999999999998721, 0.000000000000000000, 0.000000000000000000 ) ) ;
#58108 =( GEOMETRIC_REPRESENTATION_CONTEXT ( 3 ) GLOBAL_UNCERTAINTY_ASSIGNED_CONTEXT ( ( #14621 ) ) GLOBAL_UNIT_ASSIGNED_CONTEXT ( ( #9866, #83758, #19084 ) ) REPRESENTATION_CONTEXT ( 'NONE', 'WORKASPACE' ) );
#58110 = EDGE_CURVE ( 'NONE', #61967, #38219, #80429, .T. ) ;
#58111 = CARTESIAN_POINT ( 'NONE',  ( -7.045755811259131640, 103.6965839698644203, 3.790843699961854885 ) ) ;
#58112 = EDGE_CURVE ( 'NONE', #21850, #97131, #34445, .T. ) ;
#58113 = CIRCLE ( 'NONE', #34049, 4.000000000000007105 ) ;
#58114 = CARTESIAN_POINT ( 'NONE',  ( 0.000000000000000000, 0.000000000000000000, 0.000000000000000000 ) ) ;
#58115 = CIRCLE ( 'NONE', #61699, 3.309500000000001663 ) ;
#58116 = CARTESIAN_POINT ( 'NONE',  ( 84.46416041085834081, -53.81410151352770299, 189.8017141661123048 ) ) ;
#58117 = SURFACE_STYLE_USAGE ( .BOTH. , #72706 ) ;
#58118 = EDGE_LOOP ( 'NONE', ( #96129, #105909, #94411, #37542, #26933, #30480 ) ) ;
#58119 = CARTESIAN_POINT ( 'NONE',  ( 94.60687179076299458, -57.65605773701032888, -9.974991136142552506 ) ) ;
#58120 = CARTESIAN_POINT ( 'NONE',  ( 36.36650669486618881, 4.898587196589411843E-16, -4.000000000000000888 ) ) ;
#58121 = CARTESIAN_POINT ( 'NONE',  ( 0.000000000000000000, 0.000000000000000000, 0.000000000000000000 ) ) ;
#58122 = EDGE_CURVE ( 'NONE', #6711, #3694, #104542, .T. ) ;
#58123 = DIRECTION ( 'NONE',  ( 0.000000000000000000, -1.000000000000000000, 0.000000000000000000 ) ) ;
#58124 = AXIS2_PLACEMENT_3D ( 'NONE', #102210, #53657, #27842 ) ;
#58125 = CARTESIAN_POINT ( 'NONE',  ( -81.41044234058053064, -29.99999999999999645, -9.983906976751161011 ) ) ;
#58126 = B_SPLINE_CURVE_WITH_KNOTS ( 'NONE', 3,
 ( #81906, #99700, #51137, #8022, #25870, #65746, #2056, #24254 ),
 .UNSPECIFIED., .F., .F.,
 ( 4, 2, 2, 4 ),
 ( 0.000000000000000000, 0.002002078253806423812, 0.003003117380709634850, 0.004004156507612845889 ),
 .UNSPECIFIED. ) ;
#58127 = CIRCLE ( 'NONE', #20323, 4.000000000000000888 ) ;
#58128 = DIRECTION ( 'NONE',  ( -0.000000000000000000, 1.000000000000000000, -0.000000000000000000 ) ) ;
#58129 = CARTESIAN_POINT ( 'NONE',  ( 23.05251019904558163, 27.41544800856653197, -33.20617127781074629 ) ) ;
#58130 = CARTESIAN_POINT ( 'NONE',  ( 35.59999999999999432, -3.309499999999999886, 4.475777889183790779E-16 ) ) ;
#58132 = CYLINDRICAL_SURFACE ( 'NONE', #39601, 4.000000000000000000 ) ;
#58131 = CARTESIAN_POINT ( 'NONE',  ( 6.249999999999998224, 8.000000000000000000, 0.000000000000000000 ) ) ;
#58133 = AXIS2_PLACEMENT_3D ( 'NONE', #11512, #28834, #85429 ) ;
#58134 = SURFACE_STYLE_FILL_AREA ( #34440 ) ;
#58135 = CARTESIAN_POINT ( 'NONE',  ( -31.47286749730675837, 438.9570384604948572, 23.21156150463603396 ) ) ;
#58136 = CARTESIAN_POINT ( 'NONE',  ( 5.858881034796412202, -81.21413675997018800, 1.317748741875969687 ) ) ;
#58137 = CARTESIAN_POINT ( 'NONE',  ( -56.85792563227521157, -36.99373425697515216, -26.55165709400334606 ) ) ;
#58138 = LINE ( 'NONE', #39851, #52887 ) ;
#58139 = DIRECTION ( 'NONE',  ( -1.000000000000000000, -1.224606353822377258E-16, -0.000000000000000000 ) ) ;
#58140 = ORIENTED_EDGE ( 'NONE', *, *, #74725, .F. ) ;
#58141 = CARTESIAN_POINT ( 'NONE',  ( 6.925232610679094236, 9.132088611198859951, 1.053462737155419715 ) ) ;
#58142 = AXIS2_PLACEMENT_3D ( 'NONE', #2643, #52797, #61444 ) ;
#58143 = CARTESIAN_POINT ( 'NONE',  ( -7.986468734911287726, 81.02686320276922061, 0.5341897780976151422 ) ) ;
#58144 = CARTESIAN_POINT ( 'NONE',  ( -56.83356558749228071, -28.80307005180548074, -26.02374799800344718 ) ) ;
#58146 = CARTESIAN_POINT ( 'NONE',  ( 29.68315524076926337, -1.200000000000000030E-05, -42.10535821593530414 ) ) ;
#58145 = CARTESIAN_POINT ( 'NONE',  ( 38.51502786939645517, 460.0233756673477501, 2.043034587343977027 ) ) ;
#58147 = ORIENTED_EDGE ( 'NONE', *, *, #16049, .T. ) ;
#58148 = DIRECTION ( 'NONE',  ( 0.000000000000000000, -1.000000000000000000, 0.000000000000000000 ) ) ;
#58149 = ORIENTED_EDGE ( 'NONE', *, *, #76286, .T. ) ;
#58150 = CARTESIAN_POINT ( 'NONE',  ( -26.18202783569196157, 34.84340182765555483, 9.653642326100298376 ) ) ;
#58151 =( GEOMETRIC_REPRESENTATION_CONTEXT ( 3 ) GLOBAL_UNCERTAINTY_ASSIGNED_CONTEXT ( ( #23269 ) ) GLOBAL_UNIT_ASSIGNED_CONTEXT ( ( #62595, #79290, #54454 ) ) REPRESENTATION_CONTEXT ( 'NONE', 'WORKASPACE' ) );
#58152 = EDGE_CURVE ( 'NONE', #32589, #76808, #10641, .T. ) ;
#58153 = CARTESIAN_POINT ( 'NONE',  ( 10.61682093389897830, 43.20212652150377863, -15.36618043917111187 ) ) ;
#58154 =( NAMED_UNIT ( * ) SI_UNIT ( $, .STERADIAN. ) SOLID_ANGLE_UNIT ( ) );
#58155 = CARTESIAN_POINT ( 'NONE',  ( -21.65591802733287707, -59.99999999999999289, -41.70210173751639360 ) ) ;
#58156 = ORIENTED_EDGE ( 'NONE', *, *, #35771, .F. ) ;
#58157 = CARTESIAN_POINT ( 'NONE',  ( 68.38730731139169450, -37.97126955729439857, -23.07194479924394059 ) ) ;
#58158 = CARTESIAN_POINT ( 'NONE',  ( -9.403135590048261605, 294.6596552050577316, -3.414844070320783853 ) ) ;
#58159 = CARTESIAN_POINT ( 'NONE',  ( 102.9234337200204976, -60.17135737299345521, 192.9571753945863861 ) ) ;
#58161 = CARTESIAN_POINT ( 'NONE',  ( -0.004771297262913525017, -57.67120202554433916, -44.61186700141271899 ) ) ;
#58160 = CARTESIAN_POINT ( 'NONE',  ( 16.15566081772431062, -23.35500082345586037, 27.97597666450196741 ) ) ;
#58162 = ORIENTED_EDGE ( 'NONE', *, *, #77990, .T. ) ;
#58163 = B_SPLINE_CURVE_WITH_KNOTS ( 'NONE', 3,
 ( #9501, #66697, #8976, #41879, #74768, #33824, #42957, #92561, #75849, #99578, #25755, #91515, #42414, #84482, #59147, #10575, #51026, #50490, #83403, #75307 ),
 .UNSPECIFIED., .F., .F.,
 ( 4, 2, 2, 2, 2, 2, 2, 2, 2, 4 ),
 ( 0.006825806956960024478, 0.007331941334980166675, 0.007838075713000309738, 0.008344210091020451067, 0.008597277280030523466, 0.008850344469040594131, 0.009356478847060733725, 0.009862613225080873319, 0.01036874760310101118, 0.01087488198112114730 ),
 .UNSPECIFIED. ) ;
#58164 = ORIENTED_EDGE ( 'NONE', *, *, #35369, .T. ) ;
#58165 = ORIENTED_EDGE ( 'NONE', *, *, #80520, .F. ) ;
#58166 = CARTESIAN_POINT ( 'NONE',  ( 29.98619893519776980, 322.2519330491974756, 14.47105243112991424 ) ) ;
#58167 = ADVANCED_FACE ( 'NONE', ( #76441 ), #93030, .T. ) ;
#58168 = DIRECTION ( 'NONE',  ( -1.000000000000000000, 0.000000000000000000, 0.000000000000000000 ) ) ;
#58169 = CARTESIAN_POINT ( 'NONE',  ( 16.32527301256097374, 45.99414959098179168, 4.187920679398761337 ) ) ;
#58170 = ORIENTED_EDGE ( 'NONE', *, *, #42854, .T. ) ;
#58171 = CARTESIAN_POINT ( 'NONE',  ( 0.000000000000000000, 0.000000000000000000, -25.03750572909317285 ) ) ;
#58172 = DIRECTION ( 'NONE',  ( 0.000000000000000000, -1.000000000000000000, 0.000000000000000000 ) ) ;
#58173 = CARTESIAN_POINT ( 'NONE',  ( -18.91781669292785395, 48.00000000000000000, 62.18610382930904734 ) ) ;
#58174 = CARTESIAN_POINT ( 'NONE',  ( -67.94141844175470624, -57.68152395592925785, 141.0744097219443347 ) ) ;
#58175 = CARTESIAN_POINT ( 'NONE',  ( -1.320432766682874540E-15, -33.03125000204838813, 7.188101187500000044 ) ) ;
#58176 = CARTESIAN_POINT ( 'NONE',  ( -1.841875822471433519E-14, -3.000000000000002665, -70.00227127314062159 ) ) ;
#58177 = AXIS2_PLACEMENT_3D ( 'NONE', #42921, #2982, #101689 ) ;
#58178 = CARTESIAN_POINT ( 'NONE',  ( 13.58349330513380160, 4.000000000000003553, 0.000000000000000000 ) ) ;
#58179 =( GEOMETRIC_REPRESENTATION_CONTEXT ( 3 ) GLOBAL_UNCERTAINTY_ASSIGNED_CONTEXT ( ( #13570 ) ) GLOBAL_UNIT_ASSIGNED_CONTEXT ( ( #31284, #87905, #38827 ) ) REPRESENTATION_CONTEXT ( 'NONE', 'WORKASPACE' ) );
#58180 = DIRECTION ( 'NONE',  ( 0.000000000000000000, -1.000000000000000000, 0.000000000000000000 ) ) ;
#58181 = CARTESIAN_POINT ( 'NONE',  ( 16.35077622672217146, -14.21045842199431064, -36.83539407110947650 ) ) ;
#58182 = CARTESIAN_POINT ( 'NONE',  ( -8.310099524471651122, -29.99999999999994316, 36.98670313214555705 ) ) ;
#58183 = CARTESIAN_POINT ( 'NONE',  ( -49.07957144243162162, -53.36799748280911615, 53.76589609654883617 ) ) ;
#58184 = CARTESIAN_POINT ( 'NONE',  ( 25.53945892759312031, 1.340359594676612611E-15, 0.000000000000000000 ) ) ;
#58186 = ORIENTED_EDGE ( 'NONE', *, *, #39843, .F. ) ;
#58185 =( GEOMETRIC_REPRESENTATION_CONTEXT ( 3 ) GLOBAL_UNCERTAINTY_ASSIGNED_CONTEXT ( ( #21191 ) ) GLOBAL_UNIT_ASSIGNED_CONTEXT ( ( #57602, #82433, #74330 ) ) REPRESENTATION_CONTEXT ( 'NONE', 'WORKASPACE' ) );
#58187 = MECHANICAL_DESIGN_GEOMETRIC_PRESENTATION_REPRESENTATION (  '', ( #6518 ), #104694 ) ;
#58188 = CARTESIAN_POINT ( 'NONE',  ( -99.94755020072459217, -60.30543975612710739, 195.8429729570115114 ) ) ;
#58189 = VECTOR ( 'NONE', #66576, 1000.000000000000000 ) ;
#58190 = CARTESIAN_POINT ( 'NONE',  ( -0.2504595177851753895, 295.3551702422010976, -10.00003484568030743 ) ) ;
#58191 = EDGE_CURVE ( 'NONE', #49541, #55657, #67315, .T. ) ;
#58192 = CARTESIAN_POINT ( 'NONE',  ( 9.518831299010095393, -3.343618015359576479, 14.84779095168542185 ) ) ;
#58193 = VERTEX_POINT ( 'NONE', #50043 ) ;
#58194 = CARTESIAN_POINT ( 'NONE',  ( 4.496882872040831813, 249.4621133451038020, 3.972797206970401174 ) ) ;
#58195 = CARTESIAN_POINT ( 'NONE',  ( 82.47534791270491894, -38.83477010435220933, 196.4395726495995405 ) ) ;
#58196 = CARTESIAN_POINT ( 'NONE',  ( 35.58361799548379167, -5.000000000000000000, 6.123233995736768255E-16 ) ) ;
#58197 = CARTESIAN_POINT ( 'NONE',  ( -5.454378341225808668, 52.03812197093989766, -6.039378168782938872 ) ) ;
#58198 = CARTESIAN_POINT ( 'NONE',  ( -6.750000000000015099, -11.69134295108991495, -13.00000000000000000 ) ) ;
#58199 = CARTESIAN_POINT ( 'NONE',  ( -72.41885610115926397, 42.00000000000000000, -55.65414010186705696 ) ) ;
#58200 = CARTESIAN_POINT ( 'NONE',  ( 84.12545104255541162, -30.00000000000000000, 162.1202415754671051 ) ) ;
#58201 = ADVANCED_FACE ( 'NONE', ( #82953 ), #25357, .T. ) ;
#58202 = CARTESIAN_POINT ( 'NONE',  ( 36.22417390464762121, 491.4095951024645501, 12.30556361670505261 ) ) ;
#58203 = CARTESIAN_POINT ( 'NONE',  ( -29.35771261243686325, 8.827287181787188075, 42.06472072717348709 ) ) ;
#58204 = FACE_OUTER_BOUND ( 'NONE', #99480, .T. ) ;
#58205 = CIRCLE ( 'NONE', #52980, 1.999999999999995781 ) ;
#58206 = VERTEX_POINT ( 'NONE', #68375 ) ;
#58207 = VERTEX_POINT ( 'NONE', #34969 ) ;
#58208 = CARTESIAN_POINT ( 'NONE',  ( 51.55283957149192986, -49.90428648180873239, 57.17623228211761699 ) ) ;
#58209 = CARTESIAN_POINT ( 'NONE',  ( -4.240603921359149098, 300.6920857498121791, -10.01075349357188671 ) ) ;
#58210 = FACE_OUTER_BOUND ( 'NONE', #45596, .T. ) ;
#58211 = VERTEX_POINT ( 'NONE', #50559 ) ;
#58212 = CARTESIAN_POINT ( 'NONE',  ( -90.64891522596445839, -38.34438625522449939, 9.494094722409048615 ) ) ;
#58213 = CONICAL_SURFACE ( 'NONE', #72003, 8.605212085995399107, 1.221730476396037490 ) ;
#58214 = VERTEX_POINT ( 'NONE', #33901 ) ;
#58215 = DIRECTION ( 'NONE',  ( -1.000000000000000000, -1.224606353822377258E-16, -0.000000000000000000 ) ) ;
#58216 = CARTESIAN_POINT ( 'NONE',  ( 90.86283834997398401, -38.35177504835404960, 20.66734224468696013 ) ) ;
#58217 = CARTESIAN_POINT ( 'NONE',  ( 14.09725510805089854, 20.98540075817746597, -6.025598037645925942 ) ) ;
#58218 = CARTESIAN_POINT ( 'NONE',  ( 82.88655854197318718, -37.85212557438806869, 24.55487265319875334 ) ) ;
#58219 = CARTESIAN_POINT ( 'NONE',  ( -31.09458889425144434, 439.4642108243003236, 22.89797391519575598 ) ) ;
#58220 = CARTESIAN_POINT ( 'NONE',  ( -35.41617299308384759, 356.1013257493688116, 1.637565765989996924 ) ) ;
#58221 = FACE_OUTER_BOUND ( 'NONE', #65526, .T. ) ;
#58222 = CIRCLE ( 'NONE', #11705, 12.50000000000000533 ) ;
#58223 = CARTESIAN_POINT ( 'NONE',  ( 74.86035044006985117, -59.99999999999997868, 180.1901903545331152 ) ) ;
#58224 = CARTESIAN_POINT ( 'NONE',  ( 17.60863369925912991, 45.00000000000000711, 63.07564956641097353 ) ) ;
#58225 = ORIENTED_EDGE ( 'NONE', *, *, #83337, .T. ) ;
#58226 = CARTESIAN_POINT ( 'NONE',  ( 61.66760480045117987, -32.53592676977203979, 73.28662338893155948 ) ) ;
#58227 = CARTESIAN_POINT ( 'NONE',  ( -25.32031312100193787, 295.7141235396721868, -1.814807454844818091 ) ) ;
#58228 = CARTESIAN_POINT ( 'NONE',  ( 9.215420734788352775, -53.73264731217665968, 23.11721482942554928 ) ) ;
#58229 = CARTESIAN_POINT ( 'NONE',  ( -6.367479334539770441, -4.999999999999999112, -15.34856421866666665 ) ) ;
#58231 = CARTESIAN_POINT ( 'NONE',  ( -4.080135247164482060, 53.97828331548330283, 7.632653361217891508 ) ) ;
#58230 = CARTESIAN_POINT ( 'NONE',  ( -76.64727008412683062, -30.00000000004703438, 171.7971487496357952 ) ) ;
#58232 = VECTOR ( 'NONE', #40630, 999.9999999999998863 ) ;
#58233 = CARTESIAN_POINT ( 'NONE',  ( -33.13280996007087964, 418.5609396882045985, 25.60171976399747962 ) ) ;
#58234 = CARTESIAN_POINT ( 'NONE',  ( -38.77591069324474660, 25.24252798765403583, -11.84938028368475749 ) ) ;
#58235 = CARTESIAN_POINT ( 'NONE',  ( 8.000000000000000000, -22.90624999999999645, -3.313708498984761164 ) ) ;
#58236 = CARTESIAN_POINT ( 'NONE',  ( 5.656854249492380582, -27.31249999999999645, -5.656854249492379694 ) ) ;
#58237 = FACE_BOUND ( 'NONE', #31675, .T. ) ;
#58238 = AXIS2_PLACEMENT_3D ( 'NONE', #42969, #859, #41892 ) ;
#58239 = DIRECTION ( 'NONE',  ( 0.000000000000000000, -1.000000000000000000, 0.000000000000000000 ) ) ;
#58240 = ORIENTED_EDGE ( 'NONE', *, *, #71398, .T. ) ;
#58241 = CARTESIAN_POINT ( 'NONE',  ( 84.63126334808946183, -32.40349847066813993, 174.3450822652993395 ) ) ;
#58242 = CARTESIAN_POINT ( 'NONE',  ( 4.744389013293887736, -48.62707453416835790, 104.3204960233004357 ) ) ;
#58243 = CIRCLE ( 'NONE', #85850, 5.000000000000001776 ) ;
#58244 = CARTESIAN_POINT ( 'NONE',  ( -3.400000000000000355, 4.163799117101001052E-16, -4.987924522925830217 ) ) ;
#58245 = VERTEX_POINT ( 'NONE', #101273 ) ;
#58246 = PLANE ( 'NONE',  #63458 ) ;
#58247 = CARTESIAN_POINT ( 'NONE',  ( 4.651269564039822946, -4.999999999999991118, -15.66707428873065311 ) ) ;
#58248 = SURFACE_STYLE_FILL_AREA ( #59328 ) ;
#58249 =( NAMED_UNIT ( * ) SI_UNIT ( $, .STERADIAN. ) SOLID_ANGLE_UNIT ( ) );
#58250 = CARTESIAN_POINT ( 'NONE',  ( -43.54683447650032946, 41.43851002137547823, -50.63300042071738005 ) ) ;
#58251 = ADVANCED_FACE ( 'NONE', ( #921 ), #92455, .T. ) ;
#58252 = CARTESIAN_POINT ( 'NONE',  ( -27.75976893385707100, -28.74496449168539769, -38.27507236928394008 ) ) ;
#58253 = CARTESIAN_POINT ( 'NONE',  ( -12.41646176392127465, -3.622442468400648430, 20.56049830252581856 ) ) ;
#58254 = EDGE_CURVE ( 'NONE', #64296, #32377, #84557, .T. ) ;
#58255 = SURFACE_SIDE_STYLE ('',( #50668 ) ) ;
#58256 = CARTESIAN_POINT ( 'NONE',  ( 56.45566465188593241, -60.00000000000000000, 89.52844513896216938 ) ) ;
#58257 = AXIS2_PLACEMENT_3D ( 'NONE', #47941, #63639, #55496 ) ;
#58258 = VECTOR ( 'NONE', #14264, 1000.000000000000000 ) ;
#58259 = EDGE_CURVE ( 'NONE', #3260, #104530, #2022, .T. ) ;
#58260 = DIRECTION ( 'NONE',  ( -1.000000000000000000, -1.224606353822377258E-16, -0.000000000000000000 ) ) ;
#58261 = CARTESIAN_POINT ( 'NONE',  ( 26.80094985271070485, -20.15100958916939078, 31.71682355366501582 ) ) ;
#58262 = MECHANICAL_DESIGN_GEOMETRIC_PRESENTATION_REPRESENTATION (  '', ( #80896 ), #94719 ) ;
#58264 = CARTESIAN_POINT ( 'NONE',  ( -13.79692543861649590, 23.00056648293360695, 0.4954180079795145741 ) ) ;
#58263 = CARTESIAN_POINT ( 'NONE',  ( -15.68130581768025245, -23.07453539438714074, 36.03336598945195846 ) ) ;
#58265 = CARTESIAN_POINT ( 'NONE',  ( 4.401442555609581635E-16, -11.28125000204838457, -7.188101187500000044 ) ) ;
#58266 = SURFACE_STYLE_USAGE ( .BOTH. , #100842 ) ;
#58267 = AXIS2_PLACEMENT_3D ( 'NONE', #56772, #75076, #90757 ) ;
#58268 = DIRECTION ( 'NONE',  ( 0.000000000000000000, 1.000000000000000000, 0.000000000000000000 ) ) ;
#58269 = ORIENTED_EDGE ( 'NONE', *, *, #101671, .F. ) ;
#58270 = CARTESIAN_POINT ( 'NONE',  ( -17.49999999999995737, 48.29516379691337136, 64.09945637126308782 ) ) ;
#58271 = DIRECTION ( 'NONE',  ( -1.000000000000000000, 0.000000000000000000, 0.000000000000000000 ) ) ;
#58273 = CARTESIAN_POINT ( 'NONE',  ( 31.56406999132591906, -34.58956455767763316, -30.69127153837264999 ) ) ;
#58272 = DIRECTION ( 'NONE',  ( 0.000000000000000000, 0.000000000000000000, 1.000000000000000000 ) ) ;
#58274 = EDGE_LOOP ( 'NONE', ( #16649, #61987, #61694, #100876 ) ) ;
#58275 = CIRCLE ( 'NONE', #11693, 5.000000000000001776 ) ;
#58276 = CARTESIAN_POINT ( 'NONE',  ( 11.45228732919311554, 14.70820108121607106, -9.862212453994716910 ) ) ;
#58277 = CARTESIAN_POINT ( 'NONE',  ( 0.000000000000000000, -1.341159125180006795, 0.000000000000000000 ) ) ;
#58278 = ORIENTED_EDGE ( 'NONE', *, *, #71476, .T. ) ;
#58279 = FILL_AREA_STYLE ('',( #99251 ) ) ;
#58280 = EDGE_CURVE ( 'NONE', #102336, #7738, #52033, .T. ) ;
#58281 = FACE_OUTER_BOUND ( 'NONE', #55557, .T. ) ;
#58282 = AXIS2_PLACEMENT_3D ( 'NONE', #45874, #63666, #79821 ) ;
#58283 = CARTESIAN_POINT ( 'NONE',  ( -24.94875383206915487, 41.54882598256691040, -73.03065563107891478 ) ) ;
#58284 = CARTESIAN_POINT ( 'NONE',  ( -98.09986721704827062, -60.00000000000000000, 69.54344069125673400 ) ) ;
#58285 = DIRECTION ( 'NONE',  ( 0.000000000000000000, 0.000000000000000000, 1.000000000000000000 ) ) ;
#58286 = CARTESIAN_POINT ( 'NONE',  ( 0.000000000000000000, 0.000000000000000000, -6.606815774914157835 ) ) ;
#58287 = CARTESIAN_POINT ( 'NONE',  ( 31.00389226249483698, 502.9289871839745842, 8.047326149841639520 ) ) ;
#58289 =( NAMED_UNIT ( * ) SI_UNIT ( $, .STERADIAN. ) SOLID_ANGLE_UNIT ( ) );
#58288 = APPLICATION_CONTEXT ( 'automotive_design' ) ;
#58291 = CARTESIAN_POINT ( 'NONE',  ( 30.00000000000000355, 488.9470845376470152, 4.704489282115695836 ) ) ;
#58290 = CARTESIAN_POINT ( 'NONE',  ( 7.374560640984048732, -5.000000000000002665, -75.40399789250147933 ) ) ;
#58292 = CARTESIAN_POINT ( 'NONE',  ( -81.23148066614986362, -56.98058829986878493, 180.4918934137440090 ) ) ;
#58293 = ORIENTED_EDGE ( 'NONE', *, *, #65113, .T. ) ;
#58294 =( LENGTH_UNIT ( ) NAMED_UNIT ( * ) SI_UNIT ( .MILLI., .METRE. ) );
#58295 = VERTEX_POINT ( 'NONE', #92634 ) ;
#58296 = EDGE_LOOP ( 'NONE', ( #69159, #13343, #28546, #45698 ) ) ;
#58297 = DIRECTION ( 'NONE',  ( 0.8191520442889974607, 1.003171929053531649E-16, -0.5735764363510380548 ) ) ;
#58298 = EDGE_CURVE ( 'NONE', #71668, #22245, #3137, .T. ) ;
#58299 = DIRECTION ( 'NONE',  ( -0.000000000000000000, -0.000000000000000000, 1.000000000000000000 ) ) ;
#58300 = ORIENTED_EDGE ( 'NONE', *, *, #59223, .F. ) ;
#58301 = B_SPLINE_CURVE_WITH_KNOTS ( 'NONE', 3,
 ( #55439, #105594, #31738, #30688, #46313, #47361, #80249, #64107, #42457, #1450, #49480, #7957, #81831, #65676, #82386, #89949, #48938, #8493, #65142, #57558, #83982, #59194, #67285, #34413 ),
 .UNSPECIFIED., .F., .F.,
 ( 4, 2, 2, 2, 2, 2, 2, 2, 2, 2, 2, 4 ),
 ( 0.007007265619152588075, 0.007512813293216469464, 0.008018360967280349985, 0.008523908641344231374, 0.008776682478376171201, 0.009029456315408111028, 0.009282230152440052590, 0.009535003989471992417, 0.01004055166353587381, 0.01029332550056781537, 0.01054609933759975346, 0.01105164701166362271 ),
 .UNSPECIFIED. ) ;
#58302 = CARTESIAN_POINT ( 'NONE',  ( 32.10528697966009304, 486.1671898930079578, 5.449875171705039989 ) ) ;
#58303 =( LENGTH_UNIT ( ) NAMED_UNIT ( * ) SI_UNIT ( .MILLI., .METRE. ) );
#58304 = CYLINDRICAL_SURFACE ( 'NONE', #73105, 4.000000000000002665 ) ;
#58305 = CARTESIAN_POINT ( 'NONE',  ( 46.08349330513379982, 1.593028355512270567E-15, 0.000000000000000000 ) ) ;
#58306 = CARTESIAN_POINT ( 'NONE',  ( -1.217992623198289381, 53.93920336063153798, 8.677145619086617856 ) ) ;
#58307 = CARTESIAN_POINT ( 'NONE',  ( 95.70911704725124025, 1.016364837396684119E-14, 0.000000000000000000 ) ) ;
#58308 = CARTESIAN_POINT ( 'NONE',  ( 0.000000000000000000, -6.928203230275503444, 4.000000000000010658 ) ) ;
#58309 = AXIS2_PLACEMENT_3D ( 'NONE', #30393, #103203, #78914 ) ;
#58310 = CARTESIAN_POINT ( 'NONE',  ( 106.9311160729171917, -14.21045842199435860, 169.9238089813113390 ) ) ;
#58311 = CARTESIAN_POINT ( 'NONE',  ( -109.0466421874928074, -29.99999999999997513, 159.8085545269249224 ) ) ;
#58312 = CARTESIAN_POINT ( 'NONE',  ( -58.77907907405603538, -56.86410614522492324, 77.19366601566905217 ) ) ;
#58313 = VERTEX_POINT ( 'NONE', #79108 ) ;
#58314 = CARTESIAN_POINT ( 'NONE',  ( 63.58085507674907433, 38.95394049974004247, 6.694916254277349488 ) ) ;
#58315 = CARTESIAN_POINT ( 'NONE',  ( 112.0607394184880548, -60.00000000003897327, 140.7617073482189767 ) ) ;
#58316 = ORIENTED_EDGE ( 'NONE', *, *, #95625, .T. ) ;
#58317 = CARTESIAN_POINT ( 'NONE',  ( 8.196996272121577221, -42.95368992844134226, 31.04195210901052704 ) ) ;
#58318 = CARTESIAN_POINT ( 'NONE',  ( -99.13522008394323848, -45.26542195737069108, 125.4529771320935225 ) ) ;
#58319 = CARTESIAN_POINT ( 'NONE',  ( -7.188101187500000933, -14.37500000204838280, -2.977408999572651371 ) ) ;
#58320 = CIRCLE ( 'NONE', #60050, 13.50000000000000000 ) ;
#58321 = PRESENTATION_STYLE_ASSIGNMENT (( #57769 ) ) ;
#58322 = EDGE_CURVE ( 'NONE', #90150, #27782, #98264, .T. ) ;
#58324 = DIRECTION ( 'NONE',  ( -1.000000000000000000, -1.224606353822377258E-16, -0.000000000000000000 ) ) ;
#58323 = VECTOR ( 'NONE', #81596, 1000.000000000000114 ) ;
#58325 = ORIENTED_EDGE ( 'NONE', *, *, #55675, .T. ) ;
#58326 = CARTESIAN_POINT ( 'NONE',  ( -62.97177311229369678, -60.00000000000002842, 110.5655362465914919 ) ) ;
#58327 = CARTESIAN_POINT ( 'NONE',  ( 7.188101187500000044, -21.03125000204838813, 0.000000000000000000 ) ) ;
#58328 = CARTESIAN_POINT ( 'NONE',  ( 44.08794255037973642, 463.0964040308558651, 6.207849963035648955 ) ) ;
#58329 =( NAMED_UNIT ( * ) SI_UNIT ( $, .STERADIAN. ) SOLID_ANGLE_UNIT ( ) );
#58330 = CARTESIAN_POINT ( 'NONE',  ( 14.76969908563116540, 0.000000000000000000, -8.521411446762671815 ) ) ;
#58331 = DIRECTION ( 'NONE',  ( 0.000000000000000000, 0.000000000000000000, -1.000000000000000000 ) ) ;
#58332 = CARTESIAN_POINT ( 'NONE',  ( 1.530808498934192310E-16, -1.200000000000000030E-05, -18.75000000000000355 ) ) ;
#58333 = EDGE_CURVE ( 'NONE', #77058, #18144, #36575, .T. ) ;
#58334 = CARTESIAN_POINT ( 'NONE',  ( 8.456527595092419247, -14.17828489812255555, 15.83957000666675441 ) ) ;
#58335 = CARTESIAN_POINT ( 'NONE',  ( -24.46206431567210871, 27.53832621860372143, 31.75666539158942570 ) ) ;
#58336 = CARTESIAN_POINT ( 'NONE',  ( 85.46985710197711228, -60.00000000000000711, -15.19164742138506163 ) ) ;
#58337 = CARTESIAN_POINT ( 'NONE',  ( -32.80042515103462364, -49.90467096888802701, 36.16953263397611096 ) ) ;
#58338 = CARTESIAN_POINT ( 'NONE',  ( -2.679344702993184058, -49.64160073592847056, 103.0669469697010783 ) ) ;
#58339 = CARTESIAN_POINT ( 'NONE',  ( 46.35011507412374954, -53.35108316952277363, 49.29442306384134298 ) ) ;
#58341 = COLOUR_RGB ( '', 0.08235294, 0.09019608, 0.10196078) ;
#58340 = CARTESIAN_POINT ( 'NONE',  ( 87.62222222222222001, 1.023464760207051730E-14, 0.000000000000000000 ) ) ;
#58342 = ORIENTED_EDGE ( 'NONE', *, *, #2580, .F. ) ;
#58343 = EDGE_CURVE ( 'NONE', #39277, #63464, #2913, .T. ) ;
#58344 = CONICAL_SURFACE ( 'NONE', #75587, 4.172000000000001485, 0.9599310885968750373 ) ;
#58345 = CARTESIAN_POINT ( 'NONE',  ( 43.81012751977134911, 434.3196218770722226, 12.85389645199637876 ) ) ;
#58346 = CARTESIAN_POINT ( 'NONE',  ( -77.65106118960082426, -38.53234513354232860, 187.0520508371121764 ) ) ;
#58347 = ORIENTED_EDGE ( 'NONE', *, *, #16596, .T. ) ;
#58349 = FACE_OUTER_BOUND ( 'NONE', #3791, .T. ) ;
#58348 = CARTESIAN_POINT ( 'NONE',  ( 25.11650669486618881, -3.999999999999998224, 0.000000000000000000 ) ) ;
#58350 = CARTESIAN_POINT ( 'NONE',  ( 19.81133971885708789, -59.99999999999996447, 34.40092749390601057 ) ) ;
#58352 = EDGE_CURVE ( 'NONE', #36077, #53725, #23655, .T. ) ;
#58351 = CARTESIAN_POINT ( 'NONE',  ( 15.99452815637142322, 36.61440916976220450, 24.05462502184699858 ) ) ;
#58353 = CARTESIAN_POINT ( 'NONE',  ( -43.87189908090044810, 464.7380721632326299, 11.09531536897684845 ) ) ;
#58354 = CARTESIAN_POINT ( 'NONE',  ( 19.83349330513380693, -4.000000000000000888, 4.898587196589416773E-16 ) ) ;
#58355 = DIRECTION ( 'NONE',  ( -0.000000000000000000, -1.000000000000000000, -0.000000000000000000 ) ) ;
#58356 = CARTESIAN_POINT ( 'NONE',  ( 5.981118819178459667, -88.97183456180060546, 0.5452870891823808908 ) ) ;
#58357 =( LENGTH_UNIT ( ) NAMED_UNIT ( * ) SI_UNIT ( .MILLI., .METRE. ) );
#58358 = CARTESIAN_POINT ( 'NONE',  ( 104.1736618930692515, -60.00000000000000000, 105.4628610393546353 ) ) ;
#58359 = CARTESIAN_POINT ( 'NONE',  ( -2.625313013168337761, -53.64477807593443259, 40.75338374577381728 ) ) ;
#58360 = ADVANCED_FACE ( 'NONE', ( #29539 ), #89570, .T. ) ;
#58361 = DIRECTION ( 'NONE',  ( 0.000000000000000000, 1.000000000000000000, 0.000000000000000000 ) ) ;
#58362 = ORIENTED_EDGE ( 'NONE', *, *, #12233, .T. ) ;
#58363 = CARTESIAN_POINT ( 'NONE',  ( -101.0464925371120160, -30.00000000000000355, 176.9119907885118153 ) ) ;
#58364 = VERTEX_POINT ( 'NONE', #46220 ) ;
#58365 = CARTESIAN_POINT ( 'NONE',  ( -6.815830331203684977, -1.215378054691643734E-13, -6.171384342982610072 ) ) ;
#58366 = CARTESIAN_POINT ( 'NONE',  ( 29.38364792612947696, 318.1686199073527064, 13.45560025562014239 ) ) ;
#58367 = CARTESIAN_POINT ( 'NONE',  ( 9.537909130738274399, 27.35385169036606356, -3.010726932293859903 ) ) ;
#58368 = CONICAL_SURFACE ( 'NONE', #60094, 13.50000000000000178, 1.047197551196596077 ) ;
#58369 = CARTESIAN_POINT ( 'NONE',  ( -7.188101187500002709, -17.18750000204838813, 2.977408999572648707 ) ) ;
#58370 = SURFACE_SIDE_STYLE ('',( #7673 ) ) ;
#58371 = FACE_OUTER_BOUND ( 'NONE', #62041, .T. ) ;
#58372 = PRESENTATION_LAYER_ASSIGNMENT (  '', '', ( #56657 ) ) ;
#58373 = AXIS2_PLACEMENT_3D ( 'NONE', #80017, #6128, #63867 ) ;
#58374 = CIRCLE ( 'NONE', #11861, 4.000000000000000000 ) ;
#58376 = ORIENTED_EDGE ( 'NONE', *, *, #64149, .T. ) ;
#58375 = CARTESIAN_POINT ( 'NONE',  ( -41.46829470068448131, 485.6020146962604258, -3.691375462659010065 ) ) ;
#58377 = CARTESIAN_POINT ( 'NONE',  ( 84.14305783358679491, -29.04061733210153662, 163.8439507599780995 ) ) ;
#58378 = DIRECTION ( 'NONE',  ( 0.000000000000000000, 0.000000000000000000, 1.000000000000000000 ) ) ;
#58379 = CIRCLE ( 'NONE', #11863, 4.000000000000000888 ) ;
#58380 =( NAMED_UNIT ( * ) PLANE_ANGLE_UNIT ( ) SI_UNIT ( $, .RADIAN. ) );
#58381 = VERTEX_POINT ( 'NONE', #37099 ) ;
#58382 = CARTESIAN_POINT ( 'NONE',  ( 5.799999999999999822, 4.618802153517005848, 7.999999999999996447 ) ) ;
#58383 = CARTESIAN_POINT ( 'NONE',  ( -0.2954874734714613149, 18.79241504922601180, -49.28332135316696139 ) ) ;
#58384 = CARTESIAN_POINT ( 'NONE',  ( 37.72555958503873796, 27.83005203459011057, -10.95617127781084577 ) ) ;
#58385 = DIRECTION ( 'NONE',  ( 0.000000000000000000, -1.000000000000000000, 0.000000000000000000 ) ) ;
#58386 = PRESENTATION_STYLE_ASSIGNMENT (( #67555 ) ) ;
#58387 =( BOUNDED_SURFACE ( )  B_SPLINE_SURFACE ( 3, 2, ( 
 ( #66140, #49419, #59663 ),
 ( #17075, #99561, #75829 ),
 ( #92545, #1383, #83386 ),
 ( #49952, #92012, #25741 ),
 ( #9484, #51004, #83922 ),
 ( #34351, #8958, #67225 ),
 ( #25184, #10033, #82321 ),
 ( #100101, #42394, #26268 ) ),
 .UNSPECIFIED., .F., .F., .F. ) 
 B_SPLINE_SURFACE_WITH_KNOTS ( ( 4, 2, 2, 4 ),
 ( 3, 3 ),
 ( -2.788567987632717404E-16, 0.002319727980553370865, 0.003479591970830195943, 0.004639455961107021020 ),
 ( 0.000000000000000000, 1.000000000000000000 ),
 .UNSPECIFIED. ) 
 GEOMETRIC_REPRESENTATION_ITEM ( )  RATIONAL_B_SPLINE_SURFACE ( (
 ( 1.000000000000000000, 0.8162384603568769714, 1.000000000000000000),
 ( 1.000000000000000000, 0.8233098591463237081, 1.000000000000000000),
 ( 1.000000000000000000, 0.8247006568299118934, 1.000000000000000000),
 ( 1.000000000000000000, 0.8207129887245617761, 1.000000000000000000),
 ( 1.000000000000000000, 0.8182997519101262718, 1.000000000000000000),
 ( 1.000000000000000000, 0.8111528056802195241, 1.000000000000000000),
 ( 1.000000000000000000, 0.8064385712632257119, 1.000000000000000000),
 ( 1.000000000000000000, 0.8001746426090996511, 1.000000000000000000) ) ) 
 REPRESENTATION_ITEM ( '' )  SURFACE ( )  );
#58388 = CARTESIAN_POINT ( 'NONE',  ( -33.07157046098463837, 370.7458470923621121, 23.83779455093726440 ) ) ;
#58389 =( NAMED_UNIT ( * ) SI_UNIT ( $, .STERADIAN. ) SOLID_ANGLE_UNIT ( ) );
#58390 = ADVANCED_FACE ( 'NONE', ( #86697 ), #35681, .T. ) ;
#58391 = ORIENTED_EDGE ( 'NONE', *, *, #12027, .T. ) ;
#58392 = SURFACE_STYLE_USAGE ( .BOTH. , #19043 ) ;
#58394 = B_SPLINE_CURVE_WITH_KNOTS ( 'NONE', 3,
 ( #49847, #8325, #24553, #74645, #81665, #40693, #25626, #66038, #17508, #42287, #89791, #48773, #73582, #15894, #57399, #106485, #105954, #729, #32642, #32097, #26163, #33166, #33695, #65513 ),
 .UNSPECIFIED., .F., .F.,
 ( 4, 2, 2, 2, 2, 2, 2, 2, 2, 2, 2, 4 ),
 ( 0.003218170336905641204, 0.003470166353295009790, 0.003722162369684378375, 0.004226154402463118583, 0.004730146435241857489, 0.005234138468020597262, 0.005738130500799337036, 0.006242122533578076810, 0.006494118549967440625, 0.006746114566356804440, 0.006998110582746168255, 0.007250106599135532071 ),
 .UNSPECIFIED. ) ;
#58393 = CIRCLE ( 'NONE', #11876, 1.000000000000001554 ) ;
#58395 = LINE ( 'NONE', #17949, #63000 ) ;
#58396 = ADVANCED_FACE ( 'NONE', ( #78050 ), #37460, .T. ) ;
#58397 = CLOSED_SHELL ( 'NONE', ( #72266, #97627, #32678, #69129, #79388, #17624, #91566, #27533, #45352, #76951 ) ) ;
#58398 = FILL_AREA_STYLE ('',( #25539 ) ) ;
#58399 = CARTESIAN_POINT ( 'NONE',  ( 86.74778042868597083, -20.65970481315351037, 185.3124080711632757 ) ) ;
#58400 = CARTESIAN_POINT ( 'NONE',  ( 0.6443172923761060211, 34.22989788132813516, -29.58399804947514866 ) ) ;
#58401 = CARTESIAN_POINT ( 'NONE',  ( 7.188101187500000044, -32.65625000204838813, 0.000000000000000000 ) ) ;
#58402 = CARTESIAN_POINT ( 'NONE',  ( 11.70976969407574586, 294.5933519376489471, -2.054959583466348327 ) ) ;
#58403 = AXIS2_PLACEMENT_3D ( 'NONE', #13630, #69247, #5551 ) ;
#58404 = CARTESIAN_POINT ( 'NONE',  ( 7.350040110511026903, 52.09159772936368427, 3.137117077569001378 ) ) ;
#58405 = VECTOR ( 'NONE', #61081, 1000.000000000000000 ) ;
#58406 = CARTESIAN_POINT ( 'NONE',  ( 37.86095226302548156, 439.1110924549081460, 23.53113382162239375 ) ) ;
#58407 = CARTESIAN_POINT ( 'NONE',  ( 0.000000000000000000, 0.000000000000000000, 5.000000000000000888 ) ) ;
#58408 = VERTEX_POINT ( 'NONE', #38157 ) ;
#58409 = CARTESIAN_POINT ( 'NONE',  ( 0.08528730779465582001, 43.17555810750859280, 18.75000000000001066 ) ) ;
#58410 = CYLINDRICAL_SURFACE ( 'NONE', #71919, 7.500000000000000000 ) ;
#58411 = CARTESIAN_POINT ( 'NONE',  ( -9.998878006837353283, 7.501608443958052597, -5.000000000000000888 ) ) ;
#58412 = CARTESIAN_POINT ( 'NONE',  ( 7.592810154713590230E-15, 0.000000000000000000, -62.00000000000000000 ) ) ;
#58413 = EDGE_CURVE ( 'NONE', #61003, #44704, #19866, .T. ) ;
#58414 = ORIENTED_EDGE ( 'NONE', *, *, #63092, .T. ) ;
#58415 = FILL_AREA_STYLE ('',( #102459 ) ) ;
#58416 = DIRECTION ( 'NONE',  ( -0.000000000000000000, -1.000000000000000000, -0.000000000000000000 ) ) ;
#58417 = CARTESIAN_POINT ( 'NONE',  ( -7.500000000000004441, 9.833333333333344584, -71.71180648257555390 ) ) ;
#58418 = CARTESIAN_POINT ( 'NONE',  ( 111.9393053685597295, -57.67107339064843785, 191.5175075271729099 ) ) ;
#58419 = VECTOR ( 'NONE', #16455, 1000.000000000000000 ) ;
#58420 = FILL_AREA_STYLE_COLOUR ( '', #66131 ) ;
#58421 = ADVANCED_FACE ( 'NONE', ( #102323 ), #18417, .T. ) ;
#58422 = CARTESIAN_POINT ( 'NONE',  ( -27.99999999999999645, 1.592040838891559095E-15, 13.00000000000000000 ) ) ;
#58423 = CARTESIAN_POINT ( 'NONE',  ( 26.69900261086841198, 5.000000000000003553, 0.000000000000000000 ) ) ;
#58424 = FACE_OUTER_BOUND ( 'NONE', #9359, .T. ) ;
#58425 = CARTESIAN_POINT ( 'NONE',  ( -75.76033734085729066, -60.00000000000000711, 185.8899872020949999 ) ) ;
#58426 = MECHANICAL_DESIGN_GEOMETRIC_PRESENTATION_REPRESENTATION (  '', ( #89460 ), #79126 ) ;
#58427 = VECTOR ( 'NONE', #30522, 1000.000000000000000 ) ;
#58428 = CARTESIAN_POINT ( 'NONE',  ( 0.000000000000000000, 81.00000000000000000, -8.000000000000007105 ) ) ;
#58429 = CARTESIAN_POINT ( 'NONE',  ( -7.980179952708205483E-13, 34.17188553057791722, -29.75000000000694911 ) ) ;
#58430 = CARTESIAN_POINT ( 'NONE',  ( -20.97754405179121662, 294.8763868968453608, 9.942224931492262385 ) ) ;
#58431 = CARTESIAN_POINT ( 'NONE',  ( -85.27549786776644680, -32.22529396608707941, 179.6151387925006873 ) ) ;
#58432 = EDGE_LOOP ( 'NONE', ( #65949, #7065, #72125, #84895 ) ) ;
#58433 = CARTESIAN_POINT ( 'NONE',  ( 26.13430946603648763, 305.6458041140454611, -9.606786330514147210 ) ) ;
#58434 = ORIENTED_EDGE ( 'NONE', *, *, #58972, .F. ) ;
#58435 = CARTESIAN_POINT ( 'NONE',  ( -6.231493956936419387, 147.8264543773111654, 0.000000000000000000 ) ) ;
#58436 = EDGE_CURVE ( 'NONE', #29217, #46369, #4167, .T. ) ;
#58437 = SURFACE_STYLE_USAGE ( .BOTH. , #49261 ) ;
#58438 = CARTESIAN_POINT ( 'NONE',  ( -86.47380749082138607, -60.23397837094964302, -12.64187964145606990 ) ) ;
#58439 = CIRCLE ( 'NONE', #84304, 8.000000000000000000 ) ;
#58440 = CARTESIAN_POINT ( 'NONE',  ( -4.999999999999999112, -14.05766640829038572, -5.232782735144287933 ) ) ;
#58441 = CONICAL_SURFACE ( 'NONE', #60169, 3.309500000000001663, 0.9599310885968770357 ) ;
#58442 = CARTESIAN_POINT ( 'NONE',  ( -16.64348903516517098, 43.47556584774767430, 6.657797401561654560 ) ) ;
#58443 = CARTESIAN_POINT ( 'NONE',  ( -14.85442893618376203, -6.964787325848677213, 13.28843411678688824 ) ) ;
#58444 = DIRECTION ( 'NONE',  ( 0.000000000000000000, 0.000000000000000000, 1.000000000000000000 ) ) ;
#58445 = CARTESIAN_POINT ( 'NONE',  ( 12.26443481952583525, 5.755067855938387211, -8.492088444537413849 ) ) ;
#58446 = CARTESIAN_POINT ( 'NONE',  ( -7.499174415388573091E-15, 1.500000000000000444, 61.23540616453487218 ) ) ;
#58447 = CARTESIAN_POINT ( 'NONE',  ( -36.54117467508550021, 437.9945884957556359, 4.200333155677842711 ) ) ;
#58448 = CARTESIAN_POINT ( 'NONE',  ( -52.81151229832320126, -14.21045842199429643, -31.95502044027141153 ) ) ;
#58449 = CARTESIAN_POINT ( 'NONE',  ( -76.97108689222071121, -29.08047201166412066, 121.1803976918724999 ) ) ;
#58450 = ORIENTED_EDGE ( 'NONE', *, *, #17543, .F. ) ;
#58451 = CARTESIAN_POINT ( 'NONE',  ( 77.57360435794387854, -29.99999999999995026, 180.9683789367223596 ) ) ;
#58452 = CARTESIAN_POINT ( 'NONE',  ( 7.801777176595948937, 88.58827985812634154, -1.786991866639919380 ) ) ;
#58453 = CARTESIAN_POINT ( 'NONE',  ( 94.62282354643079429, -57.66661055993814955, -3.516479676606508953 ) ) ;
#58454 = ORIENTED_EDGE ( 'NONE', *, *, #47085, .F. ) ;
#58455 = CARTESIAN_POINT ( 'NONE',  ( 8.239573482191097753, 51.66633055143890374, -4.000019732116445681 ) ) ;
#58456 = EDGE_CURVE ( 'NONE', #60761, #39211, #90773, .T. ) ;
#58457 = DIRECTION ( 'NONE',  ( 0.000000000000000000, -1.000000000000000000, 0.000000000000000000 ) ) ;
#58458 = EDGE_LOOP ( 'NONE', ( #43131, #13454, #78078, #48781, #90354 ) ) ;
#58459 = CARTESIAN_POINT ( 'NONE',  ( 3.461320898197532525, 15.83138828300827150, -6.086543647318008787 ) ) ;
#58460 = FACE_OUTER_BOUND ( 'NONE', #97107, .T. ) ;
#58461 = CARTESIAN_POINT ( 'NONE',  ( 15.65045322250983872, 44.05828365038193084, 4.643985932004602191 ) ) ;
#58462 = CARTESIAN_POINT ( 'NONE',  ( 7.188101187499999156, -14.75000000204838457, 2.977408999572654924 ) ) ;
#58463 = DIRECTION ( 'NONE',  ( 1.000000000000000000, 2.168404344971008560E-17, 0.000000000000000000 ) ) ;
#58464 = DIRECTION ( 'NONE',  ( 0.8660254037844382635, -0.5000000000000005551, 0.000000000000000000 ) ) ;
#58465 = DIRECTION ( 'NONE',  ( 0.000000000000000000, 1.000000000000000000, 0.000000000000000000 ) ) ;
#58466 = DIRECTION ( 'NONE',  ( -1.000000000000000000, -0.000000000000000000, -0.000000000000000000 ) ) ;
#58467 = EDGE_CURVE ( 'NONE', #20623, #58101, #80512, .T. ) ;
#58468 = CARTESIAN_POINT ( 'NONE',  ( -12.49198003592475459, -3.425909553771215865, -13.84024797512535088 ) ) ;
#58469 = CARTESIAN_POINT ( 'NONE',  ( 11.43775816216263053, 48.00000000000000000, -94.77568223238719725 ) ) ;
#58470 = B_SPLINE_CURVE_WITH_KNOTS ( 'NONE', 3,
 ( #11028, #52028, #59615, #75777, #67167, #75231, #43421, #50952 ),
 .UNSPECIFIED., .F., .F.,
 ( 4, 2, 2, 4 ),
 ( 0.000000000000000000, 0.4999999999999997780, 0.7499999999999998890, 1.000000000000000000 ),
 .UNSPECIFIED. ) ;
#58471 = CIRCLE ( 'NONE', #36110, 5.000000000000001776 ) ;
#58472 = VERTEX_POINT ( 'NONE', #81729 ) ;
#58473 = CARTESIAN_POINT ( 'NONE',  ( -6.978962160530237213, 41.42610738227783429, -70.37780172426575120 ) ) ;
#58475 = CARTESIAN_POINT ( 'NONE',  ( 31.69331294291215784, -29.07918354051579257, 31.86078741099893108 ) ) ;
#58474 =( NAMED_UNIT ( * ) SI_UNIT ( $, .STERADIAN. ) SOLID_ANGLE_UNIT ( ) );
#58476 = ADVANCED_FACE ( 'NONE', ( #57462 ), #26300, .T. ) ;
#58477 = CARTESIAN_POINT ( 'NONE',  ( 27.38488877681253797, 307.9860580968508543, -8.296557478737108582 ) ) ;
#58478 = ORIENTED_EDGE ( 'NONE', *, *, #53710, .T. ) ;
#58479 = EDGE_CURVE ( 'NONE', #3882, #25775, #58113, .T. ) ;
#58480 = DIRECTION ( 'NONE',  ( 0.5735764363510440500, 0.8191520442889932418, 0.000000000000000000 ) ) ;
#58481 = AXIS2_PLACEMENT_3D ( 'NONE', #88579, #78884, #30905 ) ;
#58482 = ORIENTED_EDGE ( 'NONE', *, *, #45141, .T. ) ;
#58484 = CARTESIAN_POINT ( 'NONE',  ( 2.621086668468698200, 7.606368536631365806, -7.634085501268429219 ) ) ;
#58483 = CARTESIAN_POINT ( 'NONE',  ( -2.686788508690640676E-15, -5.948846446048903225, 2.696295709017757947 ) ) ;
#58485 = LINE ( 'NONE', #60630, #105994 ) ;
#58486 = CARTESIAN_POINT ( 'NONE',  ( -87.14767027655014431, -37.99999999998310329, 189.0874028505847662 ) ) ;
#58487 = PLANE ( 'NONE',  #79040 ) ;
#58488 = DIRECTION ( 'NONE',  ( -0.7071067811865456854, 8.659560562354953812E-17, -0.7071067811865493491 ) ) ;
#58489 = CARTESIAN_POINT ( 'NONE',  ( -35.85186990248676864, 464.1122956640483039, 19.44147592470968533 ) ) ;
#58490 = ORIENTED_EDGE ( 'NONE', *, *, #16074, .T. ) ;
#58491 = VECTOR ( 'NONE', #27313, 1000.000000000000000 ) ;
#58492 = CARTESIAN_POINT ( 'NONE',  ( 90.07666725775354166, -59.99999999999997868, -18.70346304004552707 ) ) ;
#58493 = LINE ( 'NONE', #67114, #34369 ) ;
#58495 = ADVANCED_FACE ( 'NONE', ( #96375 ), #18496, .T. ) ;
#58494 = SURFACE_STYLE_USAGE ( .BOTH. , #25632 ) ;
#58496 = CARTESIAN_POINT ( 'NONE',  ( 6.624059643703564149, 294.7379298340728724, -10.02420444108935449 ) ) ;
#58497 = DIRECTION ( 'NONE',  ( -1.000000000000000000, -1.224606353822377258E-16, -0.000000000000000000 ) ) ;
#58498 = VERTEX_POINT ( 'NONE', #56932 ) ;
#58499 = CARTESIAN_POINT ( 'NONE',  ( 74.56127108291157413, 6.975173280561618775E-15, 0.000000000000000000 ) ) ;
#58500 = ORIENTED_EDGE ( 'NONE', *, *, #43685, .F. ) ;
#58501 = EDGE_LOOP ( 'NONE', ( #83998, #96230, #40646, #39504, #63772, #43903 ) ) ;
#58502 = CARTESIAN_POINT ( 'NONE',  ( 7.551437640244097693, 81.99127537477092176, -2.648272645923386293 ) ) ;
#58503 = SURFACE_STYLE_USAGE ( .BOTH. , #43381 ) ;
#58504 = DIRECTION ( 'NONE',  ( -1.000000000000000000, -1.224606353822377258E-16, -0.000000000000000000 ) ) ;
#58505 = DIRECTION ( 'NONE',  ( -1.000000000000000000, -1.224606353822377258E-16, -0.000000000000000000 ) ) ;
#58506 = CARTESIAN_POINT ( 'NONE',  ( 84.30730976911441132, -45.28743999684999011, -1.774643925835537317 ) ) ;
#58507 = CARTESIAN_POINT ( 'NONE',  ( -34.04237759262028362, 317.4902085936202525, -6.467307987191631469 ) ) ;
#58508 = CARTESIAN_POINT ( 'NONE',  ( -1.262177448353618889E-25, 303.8518027762757470, -10.00000000000000533 ) ) ;
#58509 = CIRCLE ( 'NONE', #8513, 5.000000000000001776 ) ;
#58510 = CARTESIAN_POINT ( 'NONE',  ( 12.50000000000000888, 22.13452033257601315, -39.57065185985111100 ) ) ;
#58511 = ORIENTED_EDGE ( 'NONE', *, *, #53256, .F. ) ;
#58512 = FACE_OUTER_BOUND ( 'NONE', #268, .T. ) ;
#58513 = ORIENTED_EDGE ( 'NONE', *, *, #64113, .F. ) ;
#58514 = CARTESIAN_POINT ( 'NONE',  ( 9.807572367705720495, 51.30032996905384834, -2.672138286948423591 ) ) ;
#58515 = CARTESIAN_POINT ( 'NONE',  ( 31.08349330513380693, 1.593028355512270962E-15, 0.000000000000000000 ) ) ;
#58516 = CIRCLE ( 'NONE', #11985, 4.000000000000007105 ) ;
#58517 = ADVANCED_FACE ( 'NONE', ( #23024 ), #14885, .F. ) ;
#58519 = VERTEX_POINT ( 'NONE', #64525 ) ;
#58518 = CARTESIAN_POINT ( 'NONE',  ( 14.29190075645216851, 7.765108448534480345, 6.049455384114757805 ) ) ;
#58520 = CARTESIAN_POINT ( 'NONE',  ( 77.56784472490384985, -22.13724272177843844, 118.4967285904078835 ) ) ;
#58521 = B_SPLINE_CURVE_WITH_KNOTS ( 'NONE', 3,
 ( #5027, #48110, #46539, #6596 ),
 .UNSPECIFIED., .F., .F.,
 ( 4, 4 ),
 ( 8.842683793321775393E-16, 0.002118337988231762566 ),
 .UNSPECIFIED. ) ;
#58522 = VERTEX_POINT ( 'NONE', #90924 ) ;
#58523 = FILL_AREA_STYLE_COLOUR ( '', #53053 ) ;
#58524 = CARTESIAN_POINT ( 'NONE',  ( 4.401442555609581635E-16, -23.28125000204838457, -7.188101187500000044 ) ) ;
#58525 = CARTESIAN_POINT ( 'NONE',  ( -94.77678295284667342, -57.67204358354969429, 30.25255809810320429 ) ) ;
#58526 = ADVANCED_FACE ( 'NONE', ( #41826 ), #50436, .F. ) ;
#58527 = ORIENTED_EDGE ( 'NONE', *, *, #91450, .F. ) ;
#58528 =( GEOMETRIC_REPRESENTATION_CONTEXT ( 3 ) GLOBAL_UNCERTAINTY_ASSIGNED_CONTEXT ( ( #91562 ) ) GLOBAL_UNIT_ASSIGNED_CONTEXT ( ( #103295, #72502, #63379 ) ) REPRESENTATION_CONTEXT ( 'NONE', 'WORKASPACE' ) );
#58529 =( NAMED_UNIT ( * ) SI_UNIT ( $, .STERADIAN. ) SOLID_ANGLE_UNIT ( ) );
#58530 = CARTESIAN_POINT ( 'NONE',  ( -4.237512335919120849E-14, 43.17555810750860701, 18.75000000000000355 ) ) ;
#58531 = CIRCLE ( 'NONE', #53362, 3.000000000000001332 ) ;
#58532 = CARTESIAN_POINT ( 'NONE',  ( 102.6154386523218420, -37.84845496389469588, 165.6573751097436684 ) ) ;
#58533 = EDGE_CURVE ( 'NONE', #444, #31074, #32273, .T. ) ;
#58534 = AXIS2_PLACEMENT_3D ( 'NONE', #60817, #93707, #18786 ) ;
#58535 = CARTESIAN_POINT ( 'NONE',  ( -36.90171438448089702, 490.9796882048097473, 12.46551445837863170 ) ) ;
#58536 = DIRECTION ( 'NONE',  ( 0.000000000000000000, 0.000000000000000000, 1.000000000000000000 ) ) ;
#58537 = CARTESIAN_POINT ( 'NONE',  ( -3.313708498984765161, -25.15625000409677270, 7.999999999999998224 ) ) ;
#58538 = DIRECTION ( 'NONE',  ( 0.000000000000000000, 0.000000000000000000, 1.000000000000000000 ) ) ;
#58539 = CARTESIAN_POINT ( 'NONE',  ( -36.39101805957877644, 25.97871564576526993, 12.63848849079480807 ) ) ;
#58540 = SURFACE_SIDE_STYLE ('',( #91956 ) ) ;
#58541 = CARTESIAN_POINT ( 'NONE',  ( -10.00988628808512892, 7.485880917377090604, 0.000000000000000000 ) ) ;
#58542 = DIRECTION ( 'NONE',  ( 0.000000000000000000, -1.000000000000000000, 0.000000000000000000 ) ) ;
#58543 = CARTESIAN_POINT ( 'NONE',  ( 51.88291765283191381, 572.1183258647170078, 155.1969486012844470 ) ) ;
#58544 = CARTESIAN_POINT ( 'NONE',  ( 20.11650669486618881, 1.474610560812782335E-15, 0.000000000000000000 ) ) ;
#58545 = VERTEX_POINT ( 'NONE', #83348 ) ;
#58546 = CARTESIAN_POINT ( 'NONE',  ( 2.503857664561936320E-16, -8.660254037844401509, -7.422398894150040505 ) ) ;
#58547 = DIRECTION ( 'NONE',  ( 0.000000000000000000, -1.000000000000000000, 0.000000000000000000 ) ) ;
#58548 = CARTESIAN_POINT ( 'NONE',  ( 8.874007437334798354, -60.00000000000001421, 39.63896389924233432 ) ) ;
#58549 = AXIS2_PLACEMENT_3D ( 'NONE', #12699, #21371, #47718 ) ;
#58550 = CARTESIAN_POINT ( 'NONE',  ( -96.91417471229229363, -30.00000000000000355, 191.1098736999540790 ) ) ;
#58551 = ADVANCED_FACE ( 'NONE', ( #8920 ), #99521, .T. ) ;
#58552 = ORIENTED_EDGE ( 'NONE', *, *, #100555, .T. ) ;
#58553 = CIRCLE ( 'NONE', #105053, 4.000000000000000888 ) ;
#58554 = DIRECTION ( 'NONE',  ( -1.000000000000000000, -0.000000000000000000, -0.000000000000000000 ) ) ;
#58555 = CARTESIAN_POINT ( 'NONE',  ( 70.40112261783126257, -57.68249624625126870, 157.2928848866747842 ) ) ;
#58556 = CARTESIAN_POINT ( 'NONE',  ( -7.262644754617018528, 5.510625410730323637, 4.742616764343380531 ) ) ;
#58557 = SHAPE_REPRESENTATION ( '9. Reciprocating Link', ( #10728 ), #52234 ) ;
#58559 = CARTESIAN_POINT ( 'NONE',  ( 8.146578490534659878, -22.18916675789439097, -38.54415778659916469 ) ) ;
#58558 = CIRCLE ( 'NONE', #41293, 4.000000000000001776 ) ;
#58560 = CYLINDRICAL_SURFACE ( 'NONE', #102912, 4.000000000000000000 ) ;
#58561 = SURFACE_STYLE_FILL_AREA ( #51512 ) ;
#58562 = CARTESIAN_POINT ( 'NONE',  ( -29.20644879193481813, -60.00000000000000000, 42.65854192317066662 ) ) ;
#58563 = DIRECTION ( 'NONE',  ( -0.5735764363510510444, -0.8191520442889883569, 0.000000000000000000 ) ) ;
#58564 = CIRCLE ( 'NONE', #77508, 8.142857142857131691 ) ;
#58565 = DIRECTION ( 'NONE',  ( -0.000000000000000000, -0.000000000000000000, 1.000000000000000000 ) ) ;
#58566 = B_SPLINE_CURVE_WITH_KNOTS ( 'NONE', 3,
 ( #1741, #27139, #647, #82673, #83723, #33613 ),
 .UNSPECIFIED., .F., .F.,
 ( 4, 2, 4 ),
 ( 5.299864126966940009E-16, 0.002016319290306485372, 0.004032638580612440786 ),
 .UNSPECIFIED. ) ;
#58567 = CARTESIAN_POINT ( 'NONE',  ( -86.58668466171424427, -20.72177639861540754, 184.1452794688869687 ) ) ;
#58568 = EDGE_LOOP ( 'NONE', ( #14945, #87851, #4718, #59738, #31590, #81084 ) ) ;
#58569 = CARTESIAN_POINT ( 'NONE',  ( 9.632588565166363637, -12.91979337038410236, 16.83785788650996906 ) ) ;
#58570 = CARTESIAN_POINT ( 'NONE',  ( -6.205792356335741999, -56.88414179012536209, 33.36022572332550595 ) ) ;
#58571 = CARTESIAN_POINT ( 'NONE',  ( -6.338673264423879239, 41.81695718870634693, -59.02782128990620691 ) ) ;
#58572 = CARTESIAN_POINT ( 'NONE',  ( -42.61862769184566702, 462.7773997383516189, 13.89716539804779849 ) ) ;
#58574 = CARTESIAN_POINT ( 'NONE',  ( 4.818407882770804562, -68.11195407130082913, 13.85475016061880815 ) ) ;
#58573 = CARTESIAN_POINT ( 'NONE',  ( -1.224646799147352665E-15, -3.000000000000002665, -75.00000000000001421 ) ) ;
#58575 = EDGE_LOOP ( 'NONE', ( #97152, #49296, #97285, #26510, #18565, #66592 ) ) ;
#58576 = CARTESIAN_POINT ( 'NONE',  ( -7.154160341167064452, -5.000000000000055955, -15.39637319599203380 ) ) ;
#58577 = CARTESIAN_POINT ( 'NONE',  ( -7.150053860865850375, 31.78265453913976657, 3.590189269391290239 ) ) ;
#58578 = AXIS2_PLACEMENT_3D ( 'NONE', #74692, #774, #99501 ) ;
#58579 = CARTESIAN_POINT ( 'NONE',  ( 30.28764838604852017, 297.9584608233138283, -1.316668081967330872 ) ) ;
#58580 = DIRECTION ( 'NONE',  ( 0.000000000000000000, -1.000000000000000000, 0.000000000000000000 ) ) ;
#58581 = DIRECTION ( 'NONE',  ( -0.5735764363510494901, -0.8191520442889894671, 0.000000000000000000 ) ) ;
#58582 = CARTESIAN_POINT ( 'NONE',  ( 114.5718218735923131, -60.00000000000004974, 174.9501719601325078 ) ) ;
#58583 = CARTESIAN_POINT ( 'NONE',  ( -84.24555479967482086, -25.58375714794800970, 159.3068062033638626 ) ) ;
#58584 = ORIENTED_EDGE ( 'NONE', *, *, #30835, .T. ) ;
#58585 = DIRECTION ( 'NONE',  ( 0.000000000000000000, 0.000000000000000000, -1.000000000000000000 ) ) ;
#58586 = CARTESIAN_POINT ( 'NONE',  ( -9.918325909156587628, 253.7923523170740907, 1.298699613733163005 ) ) ;
#58587 = CYLINDRICAL_SURFACE ( 'NONE', #21439, 1.249999999999999334 ) ;
#58588 = LINE ( 'NONE', #10022, #9759 ) ;
#58589 = CARTESIAN_POINT ( 'NONE',  ( 45.42661373406953373, 432.5777411345648602, 6.977553785134991138 ) ) ;
#58590 = CARTESIAN_POINT ( 'NONE',  ( 45.71963875501239016, -29.99999999999998934, 56.30994126864623439 ) ) ;
#58591 = ORIENTED_EDGE ( 'NONE', *, *, #7373, .T. ) ;
#58592 = CARTESIAN_POINT ( 'NONE',  ( 1.380949872273418351E-15, 0.000000000000000000, -11.27631144943088515 ) ) ;
#58593 = ORIENTED_EDGE ( 'NONE', *, *, #100844, .F. ) ;
#58594 = DIRECTION ( 'NONE',  ( 0.000000000000000000, 1.000000000000000000, 0.000000000000000000 ) ) ;
#58595 = CARTESIAN_POINT ( 'NONE',  ( 4.397168787612346641, 15.00000000000000000, 9.999999999999998224 ) ) ;
#58596 = FACE_OUTER_BOUND ( 'NONE', #5456, .T. ) ;
#58597 = EDGE_CURVE ( 'NONE', #16697, #72766, #17289, .T. ) ;
#58598 = CARTESIAN_POINT ( 'NONE',  ( 62.59524157943331346, 48.00000000000000000, 18.50207713769442819 ) ) ;
#58599 = CARTESIAN_POINT ( 'NONE',  ( -6.928203230275509661, -10.00000000000000888, 4.000000000000000000 ) ) ;
#58600 = CARTESIAN_POINT ( 'NONE',  ( 46.36650669486618881, -3.851859888774471706E-31, 4.000000000000000888 ) ) ;
#58601 = ORIENTED_EDGE ( 'NONE', *, *, #5265, .T. ) ;
#58602 = CARTESIAN_POINT ( 'NONE',  ( 111.5016178170474888, -59.99999999999998579, 184.5246322086984208 ) ) ;
#58604 = CARTESIAN_POINT ( 'NONE',  ( 13.22559935364501627, -22.06780710830701864, 27.64041415630501319 ) ) ;
#58603 = CARTESIAN_POINT ( 'NONE',  ( -77.40171858393368609, -14.21045842199445630, 153.6868182409262431 ) ) ;
#58606 = CARTESIAN_POINT ( 'NONE',  ( 35.40719753841921857, 462.9391285011967057, 4.212165350506638539 ) ) ;
#58605 = UNCERTAINTY_MEASURE_WITH_UNIT (LENGTH_MEASURE( 1.000000000000000082E-05 ), #86808, 'distance_accuracy_value', 'NONE');
#58607 = CARTESIAN_POINT ( 'NONE',  ( 6.249999999999998224, 4.618802153517004960, 7.999999999999998224 ) ) ;
#58608 = CIRCLE ( 'NONE', #98233, 1.000000000000020872 ) ;
#58609 = ADVANCED_FACE ( 'NONE', ( #100594 ), #37311, .F. ) ;
#58610 = CARTESIAN_POINT ( 'NONE',  ( -41.39595481026245238, -18.78381775150863930, 34.98783307414403509 ) ) ;
#58611 = B_SPLINE_CURVE_WITH_KNOTS ( 'NONE', 3,
 ( #6797, #57997, #97931, #39717, #81723, #41822, #7850, #47775, #66100, #23019 ),
 .UNSPECIFIED., .F., .F.,
 ( 4, 2, 2, 2, 4 ),
 ( 0.000000000000000000, 0.5000000000000000000, 0.7500000000000000000, 0.8750000000000000000, 1.000000000000000000 ),
 .UNSPECIFIED. ) ;
#58612 = CARTESIAN_POINT ( 'NONE',  ( -32.23780387955194016, 18.64284798593076076, 20.91998874883119441 ) ) ;
#58613 = ORIENTED_EDGE ( 'NONE', *, *, #42895, .F. ) ;
#58614 = CARTESIAN_POINT ( 'NONE',  ( -7.500000000000006217, 152.0000000000000000, 0.000000000000000000 ) ) ;
#58615 = CARTESIAN_POINT ( 'NONE',  ( 40.75641113481592726, 360.0948485545300741, 24.37153223514695100 ) ) ;
#58616 = SURFACE_STYLE_FILL_AREA ( #25758 ) ;
#58617 = CARTESIAN_POINT ( 'NONE',  ( 20.37278541768179352, 303.8378246129572631, -10.00297115033344042 ) ) ;
#58618 = CARTESIAN_POINT ( 'NONE',  ( -30.00000000000557066, 486.8872575320209535, 5.529676739975230682 ) ) ;
#58619 = ORIENTED_EDGE ( 'NONE', *, *, #59961, .T. ) ;
#58620 = SURFACE_STYLE_USAGE ( .BOTH. , #1950 ) ;
#58621 = DIRECTION ( 'NONE',  ( 1.000000000000000000, 0.000000000000000000, -8.673617379884035472E-17 ) ) ;
#58622 = ORIENTED_EDGE ( 'NONE', *, *, #63462, .F. ) ;
#58623 = CARTESIAN_POINT ( 'NONE',  ( 77.27097837494086718, -30.00000000008570922, 177.5457258123725808 ) ) ;
#58624 = CARTESIAN_POINT ( 'NONE',  ( 46.83715889037894442, 13.71037705486508429, 15.21858309684184540 ) ) ;
#58627 = EDGE_CURVE ( 'NONE', #50280, #85444, #70213, .T. ) ;
#58626 = CARTESIAN_POINT ( 'NONE',  ( 94.84444444444443434, 4.172000000000019249, 5.109226446042768454E-16 ) ) ;
#58625 =( GEOMETRIC_REPRESENTATION_CONTEXT ( 3 ) GLOBAL_UNCERTAINTY_ASSIGNED_CONTEXT ( ( #60750 ) ) GLOBAL_UNIT_ASSIGNED_CONTEXT ( ( #102334, #59234, #51110 ) ) REPRESENTATION_CONTEXT ( 'NONE', 'WORKASPACE' ) );
#58628 = CARTESIAN_POINT ( 'NONE',  ( 7.500000000000000000, 4.330127018922189208, -7.422398894150033399 ) ) ;
#58629 = CARTESIAN_POINT ( 'NONE',  ( 81.06585882963902634, -30.00000000000000000, 22.15552175282082814 ) ) ;
#58630 = AXIS2_PLACEMENT_3D ( 'NONE', #28279, #11504, #84885 ) ;
#58631 = CARTESIAN_POINT ( 'NONE',  ( -32.11723946003972685, 433.0660616616644916, 24.32198794831119315 ) ) ;
#58632 = ORIENTED_EDGE ( 'NONE', *, *, #15856, .T. ) ;
#58633 = AXIS2_PLACEMENT_3D ( 'NONE', #27134, #18493, #60023 ) ;
#58634 = ORIENTED_EDGE ( 'NONE', *, *, #2438, .T. ) ;
#58635 = EDGE_LOOP ( 'NONE', ( #4894, #33413, #72893, #84967, #36974 ) ) ;
#58636 = CARTESIAN_POINT ( 'NONE',  ( -46.89473120401039097, 12.86731181406129565, -16.16132821689905441 ) ) ;
#58637 = FACE_BOUND ( 'NONE', #54675, .T. ) ;
#58638 = CARTESIAN_POINT ( 'NONE',  ( 4.696906829037968301, -11.43998147487893391, -3.734050370377311800 ) ) ;
#58639 = CARTESIAN_POINT ( 'NONE',  ( 6.289692432696804225, 5.239086202715451002, -4.583616368338176095 ) ) ;
#58640 = CARTESIAN_POINT ( 'NONE',  ( 0.000000000000000000, 0.000000000000000000, 4.000000000000000000 ) ) ;
#58641 = VERTEX_POINT ( 'NONE', #60176 ) ;
#58642 = FACE_OUTER_BOUND ( 'NONE', #66127, .T. ) ;
#58643 = CIRCLE ( 'NONE', #34562, 4.172000000000009479 ) ;
#58644 = ORIENTED_EDGE ( 'NONE', *, *, #102503, .F. ) ;
#58645 = DIRECTION ( 'NONE',  ( 0.000000000000000000, -1.000000000000000000, 0.000000000000000000 ) ) ;
#58646 = CARTESIAN_POINT ( 'NONE',  ( 77.32616938918349092, -38.49326352433806875, 185.8092111286713362 ) ) ;
#58647 = CARTESIAN_POINT ( 'NONE',  ( 69.67238219402268840, 6.975173280561618775E-15, 0.000000000000000000 ) ) ;
#58648 = CARTESIAN_POINT ( 'NONE',  ( 26.92115534363001927, 306.8708247227045263, 10.86266092317258014 ) ) ;
#58649 = EDGE_CURVE ( 'NONE', #63888, #49037, #93044, .T. ) ;
#58650 =( NAMED_UNIT ( * ) SI_UNIT ( $, .STERADIAN. ) SOLID_ANGLE_UNIT ( ) );
#58651 = VERTEX_POINT ( 'NONE', #60697 ) ;
#58652 = CARTESIAN_POINT ( 'NONE',  ( -40.38232636938239040, 459.8969133356654311, 1.930624307836338538 ) ) ;
#58653 = CARTESIAN_POINT ( 'NONE',  ( 35.26876087351732991, 303.5869067510492414, 3.947903635018046753 ) ) ;
#58654 = DIRECTION ( 'NONE',  ( -0.000000000000000000, 1.000000000000000000, -0.000000000000000000 ) ) ;
#58655 = ADVANCED_FACE ( 'NONE', ( #11575 ), #89155, .F. ) ;
#58656 = CARTESIAN_POINT ( 'NONE',  ( 14.97109678640431696, 2.057467188489078946, -0.8486206380088415768 ) ) ;
#58657 = ORIENTED_EDGE ( 'NONE', *, *, #86616, .F. ) ;
#58658 = CARTESIAN_POINT ( 'NONE',  ( -24.63377937114793070, 295.6205676188575922, 10.10213930309776487 ) ) ;
#58659 = FACE_OUTER_BOUND ( 'NONE', #79319, .T. ) ;
#58660 = DIRECTION ( 'NONE',  ( -0.4127509058087894256, -0.1524945595932338249, 0.8979878056234892325 ) ) ;
#58661 = CARTESIAN_POINT ( 'NONE',  ( 1.012484905089438447, 302.8485832885119180, 9.936327107362844302 ) ) ;
#58662 = VECTOR ( 'NONE', #67440, 1000.000000000000000 ) ;
#58663 = EDGE_CURVE ( 'NONE', #13600, #47858, #44503, .T. ) ;
#58664 = ADVANCED_FACE ( 'NONE', ( #77927 ), #46093, .F. ) ;
#58665 = CARTESIAN_POINT ( 'NONE',  ( 9.508870726040163035, 294.7346411812065412, 3.160106868736997754 ) ) ;
#58666 = VECTOR ( 'NONE', #45760, 999.9999999999998863 ) ;
#58667 = CARTESIAN_POINT ( 'NONE',  ( 43.71039113854127578, 464.8436985699679553, 11.74907638618312689 ) ) ;
#58668 = CARTESIAN_POINT ( 'NONE',  ( 85.83414240384524874, -35.62221213960832955, 184.8240206695177221 ) ) ;
#58669 = CARTESIAN_POINT ( 'NONE',  ( 17.53682258900642665, 36.29665952923688366, -24.04445569364184720 ) ) ;
#58670 = ORIENTED_EDGE ( 'NONE', *, *, #49682, .F. ) ;
#58671 = CARTESIAN_POINT ( 'NONE',  ( 94.62684802005594520, -57.66657240577455212, -3.586364576938546822 ) ) ;
#58672 = DIRECTION ( 'NONE',  ( 0.000000000000000000, 0.000000000000000000, -1.000000000000000000 ) ) ;
#58673 = CARTESIAN_POINT ( 'NONE',  ( 15.54266041146151167, 34.77214720869447007, -23.41113234798271847 ) ) ;
#58674 = CARTESIAN_POINT ( 'NONE',  ( -81.40333483022713779, -30.00000000000000711, -10.03578593830606813 ) ) ;
#58675 = EDGE_CURVE ( 'NONE', #21525, #42491, #61767, .T. ) ;
#58676 = CONICAL_SURFACE ( 'NONE', #43119, 4.000000000000007105, 0.9599310885968835860 ) ;
#58677 =( GEOMETRIC_REPRESENTATION_CONTEXT ( 3 ) GLOBAL_UNCERTAINTY_ASSIGNED_CONTEXT ( ( #38341 ) ) GLOBAL_UNIT_ASSIGNED_CONTEXT ( ( #10449, #51968, #34772 ) ) REPRESENTATION_CONTEXT ( 'NONE', 'WORKASPACE' ) );
#58678 = LINE ( 'NONE', #83467, #65260 ) ;
#58679 = CARTESIAN_POINT ( 'NONE',  ( -2.352174619740411643, 7.302225387955492586, -7.450218641348505422 ) ) ;
#58681 =( NAMED_UNIT ( * ) PLANE_ANGLE_UNIT ( ) SI_UNIT ( $, .RADIAN. ) );
#58680 = CARTESIAN_POINT ( 'NONE',  ( 91.95555555555554861, 1.023464760207051730E-14, 0.000000000000000000 ) ) ;
#58682 = EDGE_CURVE ( 'NONE', #14419, #35975, #95806, .T. ) ;
#58683 = DIRECTION ( 'NONE',  ( 0.000000000000000000, -1.000000000000000000, 0.000000000000000000 ) ) ;
#58684 = CARTESIAN_POINT ( 'NONE',  ( -31.33625597974778998, 438.2397719845374695, 22.62029172958331102 ) ) ;
#58685 = CARTESIAN_POINT ( 'NONE',  ( -37.83989825151947173, 491.6297408768480750, 12.44743998624971049 ) ) ;
#58686 = CARTESIAN_POINT ( 'NONE',  ( 4.658465013329192494, -83.67636120326905314, 3.783534922165390668 ) ) ;
#58687 = DIRECTION ( 'NONE',  ( -0.000000000000000000, -0.000000000000000000, 1.000000000000000000 ) ) ;
#58688 = CARTESIAN_POINT ( 'NONE',  ( 46.08349330513379982, -4.000000000000000000, 4.898587196589415787E-16 ) ) ;
#58689 = EDGE_CURVE ( 'NONE', #59238, #88742, #75356, .T. ) ;
#58690 = CARTESIAN_POINT ( 'NONE',  ( 68.62844179577130888, -29.94534991839561755, -21.42007394527319875 ) ) ;
#58691 = CIRCLE ( 'NONE', #101729, 4.000000000000000000 ) ;
#58692 = ORIENTED_EDGE ( 'NONE', *, *, #78401, .T. ) ;
#58693 = DIRECTION ( 'NONE',  ( 0.000000000000000000, 1.000000000000000000, 0.000000000000000000 ) ) ;
#58694 = FACE_OUTER_BOUND ( 'NONE', #37775, .T. ) ;
#58695 = CARTESIAN_POINT ( 'NONE',  ( -7.003653396366583017, 83.94293794440324064, -3.866846144092864535 ) ) ;
#58696 = DIRECTION ( 'NONE',  ( 0.000000000000000000, 0.000000000000000000, 1.000000000000000000 ) ) ;
#58697 =( BOUNDED_SURFACE ( )  B_SPLINE_SURFACE ( 3, 2, ( 
 ( #48625, #40550, #8180 ),
 ( #80466, #16270, #47571 ),
 ( #40028, #105811, #24924 ),
 ( #58328, #81510, #33543 ),
 ( #98772, #99299, #23876 ),
 ( #73969, #33023, #25472 ),
 ( #50, #80997, #56720 ),
 ( #49702, #64832, #39511 ),
 ( #106325, #7112, #56171 ),
 ( #6578, #32492, #31437 ) ),
 .UNSPECIFIED., .F., .F., .F. ) 
 B_SPLINE_SURFACE_WITH_KNOTS ( ( 4, 2, 2, 2, 4 ),
 ( 3, 3 ),
 ( 0.006110147660091587093, 0.007140910106262555491, 0.008171672552433523889, 0.009202434998604493155, 0.01023319744477546242 ),
 ( 0.1475238061142898349, 1.000000000000000000 ),
 .UNSPECIFIED. ) 
 GEOMETRIC_REPRESENTATION_ITEM ( )  RATIONAL_B_SPLINE_SURFACE ( (
 ( 0.9263311855299185549, 0.7503155036109609988, 1.000000000000000000),
 ( 0.9308198837936185743, 0.7655289745141671265, 1.000000000000000000),
 ( 0.9348045508654743152, 0.7790341408219316754, 1.000000000000000000),
 ( 0.9412515216610307656, 0.8008847524803706097, 1.000000000000000000),
 ( 0.9437092470908616804, 0.8092146806952340565, 1.000000000000000000),
 ( 0.9465994843889277144, 0.8190105142430310625, 1.000000000000000000),
 ( 0.9470205592359524083, 0.8204376562688353580, 1.000000000000000000),
 ( 0.9455968065556910052, 0.8156121548200778726, 1.000000000000000000),
 ( 0.9437572519950128136, 0.8093773829241677209, 1.000000000000000000),
 ( 0.9409237764627873535, 0.7997739310920261024, 1.000000000000000000) ) ) 
 REPRESENTATION_ITEM ( '' )  SURFACE ( )  );
#58698 = MECHANICAL_DESIGN_GEOMETRIC_PRESENTATION_REPRESENTATION (  '', ( #105192 ), #100028 ) ;
#58700 = CARTESIAN_POINT ( 'NONE',  ( -69.51878337118347417, -21.77025481454749212, -19.67902557026448918 ) ) ;
#58699 = CARTESIAN_POINT ( 'NONE',  ( -6.177150199754213311, 12.02207793746705278, 8.529057090219303651E-15 ) ) ;
#58701 = ORIENTED_EDGE ( 'NONE', *, *, #27110, .T. ) ;
#58702 = VECTOR ( 'NONE', #105242, 1000.000000000000000 ) ;
#58703 = FACE_OUTER_BOUND ( 'NONE', #12139, .T. ) ;
#58704 = ORIENTED_EDGE ( 'NONE', *, *, #98498, .T. ) ;
#58705 = CARTESIAN_POINT ( 'NONE',  ( 32.22503847990217452, 485.9064490506207790, 4.829857536092636572 ) ) ;
#58706 = VECTOR ( 'NONE', #104596, 1000.000000000000000 ) ;
#58707 = CIRCLE ( 'NONE', #94908, 3.309500000000007880 ) ;
#58708 = CARTESIAN_POINT ( 'NONE',  ( -1.666663072624755992, -29.99999999999999645, 28.88808002246651796 ) ) ;
#58709 = CARTESIAN_POINT ( 'NONE',  ( -66.15993367293332028, -60.00000000000000711, -33.83992077223387440 ) ) ;
#58710 = ORIENTED_EDGE ( 'NONE', *, *, #84004, .T. ) ;
#58711 = CARTESIAN_POINT ( 'NONE',  ( 28.58349330513380337, -4.000000000000000888, 4.898587196589416773E-16 ) ) ;
#58712 = CARTESIAN_POINT ( 'NONE',  ( 99.36701900970518864, -37.82354045745693583, 191.5096613616152297 ) ) ;
#58714 = CARTESIAN_POINT ( 'NONE',  ( 0.000000000000000000, -79.93083296558610584, -70.00000000000000000 ) ) ;
#58713 = CARTESIAN_POINT ( 'NONE',  ( 14.97375118833551788, -22.78136625548523497, 27.82250553508887236 ) ) ;
#58715 = B_SPLINE_CURVE_WITH_KNOTS ( 'NONE', 3,
 ( #54716, #38066, #15335, #32075, #55766, #96283 ),
 .UNSPECIFIED., .F., .F.,
 ( 4, 2, 4 ),
 ( 0.02294124189192014995, 0.02484059228024679961, 0.02673994266857345273 ),
 .UNSPECIFIED. ) ;
#58716 = ORIENTED_EDGE ( 'NONE', *, *, #26863, .F. ) ;
#58717 = ORIENTED_EDGE ( 'NONE', *, *, #24728, .T. ) ;
#58718 = EDGE_LOOP ( 'NONE', ( #79169, #90445, #40925, #80705, #34425 ) ) ;
#58719 = CARTESIAN_POINT ( 'NONE',  ( 29.25197604607760837, 322.6282941308829777, 13.32234211285258851 ) ) ;
#58720 = DIRECTION ( 'NONE',  ( -1.000000000000000000, -1.224606353822377258E-16, -0.000000000000000000 ) ) ;
#58721 = CARTESIAN_POINT ( 'NONE',  ( 29.83349330513380337, 4.898587196589405926E-16, -4.000000000000001776 ) ) ;
#58722 = VERTEX_POINT ( 'NONE', #20272 ) ;
#58723 = EDGE_CURVE ( 'NONE', #52343, #100664, #46613, .T. ) ;
#58724 = FACE_OUTER_BOUND ( 'NONE', #92125, .T. ) ;
#58725 = CYLINDRICAL_SURFACE ( 'NONE', #95552, 1.250000000000001110 ) ;
#58726 = CARTESIAN_POINT ( 'NONE',  ( 93.97977184163765685, 1.030564683017419500E-14, 0.000000000000000000 ) ) ;
#58728 = CARTESIAN_POINT ( 'NONE',  ( -33.87510863592373767, -57.69360311548409470, 48.02532427896534983 ) ) ;
#58727 = AXIS2_PLACEMENT_3D ( 'NONE', #6539, #79902, #32452 ) ;
#58729 = CARTESIAN_POINT ( 'NONE',  ( 7.188101187499999156, -32.75000000204839523, 2.977408999572654924 ) ) ;
#58730 = CARTESIAN_POINT ( 'NONE',  ( -43.87115969799085491, 464.7386531662417042, 11.09928998703223613 ) ) ;
#58731 = CARTESIAN_POINT ( 'NONE',  ( -24.60488647473181345, 306.9835580411500473, 10.41807558718820914 ) ) ;
#58732 = CARTESIAN_POINT ( 'NONE',  ( -6.894536899122033269, 41.40764853481034891, -58.61755485280149713 ) ) ;
#58733 = AXIS2_PLACEMENT_3D ( 'NONE', #62323, #5137, #22934 ) ;
#58734 = CARTESIAN_POINT ( 'NONE',  ( -88.04114847129865495, -29.99999999999995026, -17.07571352811936194 ) ) ;
#58735 = ADVANCED_FACE ( 'NONE', ( #45045 ), #8135, .F. ) ;
#58736 = LINE ( 'NONE', #3146, #31073 ) ;
#58737 = EDGE_CURVE ( 'NONE', #60770, #19214, #56397, .T. ) ;
#58738 = CARTESIAN_POINT ( 'NONE',  ( -49.01629296738340003, -56.83013498245147588, 54.79628526633861441 ) ) ;
#58739 = VECTOR ( 'NONE', #74274, 1000.000000000000000 ) ;
#58740 = CARTESIAN_POINT ( 'NONE',  ( 3.313708498984780260, -27.21874999999999289, -7.999999999999981348 ) ) ;
#58741 = ORIENTED_EDGE ( 'NONE', *, *, #102106, .F. ) ;
#58742 = CARTESIAN_POINT ( 'NONE',  ( 36.04632348377495532, 437.4611277465810986, 4.334040331412323255 ) ) ;
#58743 = CARTESIAN_POINT ( 'NONE',  ( -9.970195021759460374, 302.6460196488378642, -10.04373974541436887 ) ) ;
#58744 = CARTESIAN_POINT ( 'NONE',  ( 11.08738460869479425, -1.234896052969738811, 20.41726963649704985 ) ) ;
#58745 = VERTEX_POINT ( 'NONE', #102734 ) ;
#58746 = CARTESIAN_POINT ( 'NONE',  ( -17.85383517427097999, 34.21385402367462802, -23.65294179858045354 ) ) ;
#58747 = CARTESIAN_POINT ( 'NONE',  ( 76.94667806338644311, -38.45205237156240941, 184.1492322625157954 ) ) ;
#58748 = CARTESIAN_POINT ( 'NONE',  ( 49.15106604892599051, 13.74065395669558498, 15.05054071407064420 ) ) ;
#58749 = DIRECTION ( 'NONE',  ( 0.000000000000000000, -1.000000000000000000, 0.000000000000000000 ) ) ;
#58751 = EDGE_CURVE ( 'NONE', #66199, #55140, #44348, .T. ) ;
#58750 = CARTESIAN_POINT ( 'NONE',  ( -19.03547406814728404, 294.6738091296812740, 9.899165902142932794 ) ) ;
#58752 = CARTESIAN_POINT ( 'NONE',  ( 88.20421627921849961, 42.00000000000000000, -23.70422451876603631 ) ) ;
#58753 = CARTESIAN_POINT ( 'NONE',  ( 87.87841627987471327, -30.00000000000000000, 186.4696136827627981 ) ) ;
#58754 = DIRECTION ( 'NONE',  ( 0.000000000000000000, 1.000000000000000000, 0.000000000000000000 ) ) ;
#58755 = SURFACE_STYLE_FILL_AREA ( #97582 ) ;
#58756 = CIRCLE ( 'NONE', #62157, 9.000000000000000000 ) ;
#58757 = ORIENTED_EDGE ( 'NONE', *, *, #104559, .F. ) ;
#58758 = ORIENTED_EDGE ( 'NONE', *, *, #99537, .F. ) ;
#58759 = CARTESIAN_POINT ( 'NONE',  ( 53.13899645154318563, -46.43671994497447741, 59.08478548976397349 ) ) ;
#58760 = CARTESIAN_POINT ( 'NONE',  ( 6.228838983406037144, 41.78908903116954576, -58.91794007031819547 ) ) ;
#58761 = FACE_OUTER_BOUND ( 'NONE', #29588, .T. ) ;
#58762 = ORIENTED_EDGE ( 'NONE', *, *, #103365, .F. ) ;
#58763 = CARTESIAN_POINT ( 'NONE',  ( -93.96138925245962525, -38.35488083088926459, 50.68657296838828330 ) ) ;
#58764 = VERTEX_POINT ( 'NONE', #86573 ) ;
#58765 = CARTESIAN_POINT ( 'NONE',  ( 15.85122647056153689, 4.114663126756284761, 4.288211754877275794 ) ) ;
#58766 = CARTESIAN_POINT ( 'NONE',  ( 107.1090246246218385, -38.36360799944018396, 194.6594831697806001 ) ) ;
#58767 = CARTESIAN_POINT ( 'NONE',  ( 15.37770065074485792, 22.74086236292912488, -2.279734282488619979 ) ) ;
#58768 = CARTESIAN_POINT ( 'NONE',  ( 85.46809269451053126, -37.84908238006404702, 49.13086642071656485 ) ) ;
#58769 = CARTESIAN_POINT ( 'NONE',  ( -17.26451694828253736, 43.28515295384694639, -6.504635002224487650 ) ) ;
#58770 = CARTESIAN_POINT ( 'NONE',  ( 32.65817089032879750, 465.7881089174891827, 12.85132715800152425 ) ) ;
#58771 = CARTESIAN_POINT ( 'NONE',  ( -1.224646799147352665E-15, -3.000000000000002665, -75.00000000000001421 ) ) ;
#58772 = SURFACE_STYLE_FILL_AREA ( #99747 ) ;
#58773 = CARTESIAN_POINT ( 'NONE',  ( 75.34722298054580847, -60.00000000000000000, 183.6044144055699405 ) ) ;
#58774 = CARTESIAN_POINT ( 'NONE',  ( -34.84618260875200946, 489.9833681528629654, 11.97975507378840732 ) ) ;
#58775 = VECTOR ( 'NONE', #99381, 1000.000000000000000 ) ;
#58776 = CARTESIAN_POINT ( 'NONE',  ( 18.29504988740597327, 45.00000000000001421, 62.40888277855877675 ) ) ;
#58777 = VECTOR ( 'NONE', #104940, 1000.000000000000000 ) ;
#58778 = VERTEX_POINT ( 'NONE', #37505 ) ;
#58779 = CARTESIAN_POINT ( 'NONE',  ( 61.04332100541591188, -42.96093274966459319, 76.66569307471927175 ) ) ;
#58780 = FILL_AREA_STYLE_COLOUR ( '', #63479 ) ;
#58781 = CARTESIAN_POINT ( 'NONE',  ( 31.14131030317610538, 1.482358050883964840E-15, 0.000000000000000000 ) ) ;
#58782 = CARTESIAN_POINT ( 'NONE',  ( -7.560791642129985668, -4.999999999999999112, -15.61553843468903935 ) ) ;
#58783 = CIRCLE ( 'NONE', #8790, 1.000000000000000888 ) ;
#58784 = CARTESIAN_POINT ( 'NONE',  ( -36.53342718661301802, 485.2762471673754590, -2.915875507118013577 ) ) ;
#58785 = CARTESIAN_POINT ( 'NONE',  ( -42.72184728503030726, 427.3449066199571575, 19.12547310894770547 ) ) ;
#58786 = CARTESIAN_POINT ( 'NONE',  ( -32.10528697966014278, 486.1671898930081284, 5.449875171704950283 ) ) ;
#58787 = DIRECTION ( 'NONE',  ( 1.000000000000000000, 1.224606353822377258E-16, 0.000000000000000000 ) ) ;
#58788 = CARTESIAN_POINT ( 'NONE',  ( -3.313708498984765161, -24.96874999999999645, 7.999999999999998224 ) ) ;
#58789 = CARTESIAN_POINT ( 'NONE',  ( -34.90990072193579863, -24.02533811425226418, 33.43583568697357578 ) ) ;
#58790 = AXIS2_PLACEMENT_3D ( 'NONE', #72635, #14386, #88309 ) ;
#58791 = EDGE_CURVE ( 'NONE', #94292, #36949, #83991, .T. ) ;
#58792 = STYLED_ITEM ( 'NONE', ( #39826 ), #73803 ) ;
#58793 = CARTESIAN_POINT ( 'NONE',  ( 16.48470368732129643, 43.81217145385495826, -4.157797401561333928 ) ) ;
#58794 = ORIENTED_EDGE ( 'NONE', *, *, #82665, .F. ) ;
#58795 = CARTESIAN_POINT ( 'NONE',  ( 84.24501642249120437, -39.42684420198852280, 179.9136778439357442 ) ) ;
#58796 = DIRECTION ( 'NONE',  ( 0.000000000000000000, 0.000000000000000000, 1.000000000000000000 ) ) ;
#58797 = CARTESIAN_POINT ( 'NONE',  ( -40.16961380562399597, 438.0191182675681034, 22.24568332716581764 ) ) ;
#58798 = ORIENTED_EDGE ( 'NONE', *, *, #104878, .F. ) ;
#58799 = LINE ( 'NONE', #12748, #80739 ) ;
#58800 = CARTESIAN_POINT ( 'NONE',  ( 9.474439531901662548, -5.000000000000000888, -19.39817504954017480 ) ) ;
#58801 = CARTESIAN_POINT ( 'NONE',  ( 35.11650669486618170, 1.474610560812782335E-15, 0.000000000000000000 ) ) ;
#58802 = DIRECTION ( 'NONE',  ( 1.096832036894112098E-16, 0.000000000000000000, 1.000000000000000000 ) ) ;
#58803 = LINE ( 'NONE', #19447, #98799 ) ;
#58804 = CARTESIAN_POINT ( 'NONE',  ( -27.97116258485550944, -28.82356970829601650, -38.26646285370772915 ) ) ;
#58805 = DIRECTION ( 'NONE',  ( 0.000000000000000000, 0.000000000000000000, 1.000000000000000000 ) ) ;
#58806 = EDGE_CURVE ( 'NONE', #30981, #105946, #54684, .T. ) ;
#58807 =( NAMED_UNIT ( * ) PLANE_ANGLE_UNIT ( ) SI_UNIT ( $, .RADIAN. ) );
#58808 = CONICAL_SURFACE ( 'NONE', #100137, 4.000000000000001776, 0.9599310885968774798 ) ;
#58809 = CARTESIAN_POINT ( 'NONE',  ( 47.39775995135304498, -60.00000000000000711, 65.66615658238637820 ) ) ;
#58810 = AXIS2_PLACEMENT_3D ( 'NONE', #105288, #94568, #22806 ) ;
#58811 = CARTESIAN_POINT ( 'NONE',  ( -37.56673239365863282, 27.60449318992554879, -13.45617127781024891 ) ) ;
#58813 = CARTESIAN_POINT ( 'NONE',  ( -15.19979302622828854, 22.50962311628596879, -3.105710245049020379 ) ) ;
#58812 = CARTESIAN_POINT ( 'NONE',  ( -8.884123413888394438, -19.77486597863934747, 35.29550976858007516 ) ) ;
#58814 = COLOUR_RGB ( '', 0.09019608, 0.27058824, 0.51372549) ;
#58815 = CARTESIAN_POINT ( 'NONE',  ( -9.165151389911679658, 85.00000000000000000, 4.000000000000000000 ) ) ;
#58816 = CARTESIAN_POINT ( 'NONE',  ( 7.188101187500001821, -11.56250000204838635, -2.977408999572650483 ) ) ;
#58817 = CARTESIAN_POINT ( 'NONE',  ( 31.46099760824767344, 298.7896251960808627, -1.127419728356056972 ) ) ;
#58818 = CARTESIAN_POINT ( 'NONE',  ( 80.97977184163765685, 5.000000000000021316, 0.000000000000000000 ) ) ;
#58819 = ORIENTED_EDGE ( 'NONE', *, *, #82452, .T. ) ;
#58820 = EDGE_CURVE ( 'NONE', #38588, #60788, #76482, .T. ) ;
#58821 = CARTESIAN_POINT ( 'NONE',  ( -49.50172129736240123, -35.49676079082828295, -36.27236392705374612 ) ) ;
#58822 = CARTESIAN_POINT ( 'NONE',  ( -17.49999999999920419, 50.00907933620717927, 60.12834585266249121 ) ) ;
#58823 = CARTESIAN_POINT ( 'NONE',  ( 0.06730325657896424341, -1.557442666625489025, 7.999999999999996447 ) ) ;
#58824 = CARTESIAN_POINT ( 'NONE',  ( 4.000000000000000000, 4.898587196589412829E-16, -4.567799999999999194 ) ) ;
#58826 = CARTESIAN_POINT ( 'NONE',  ( 22.38858659560567688, -47.40902890394536939, -33.77719791820585016 ) ) ;
#58825 = CARTESIAN_POINT ( 'NONE',  ( 4.963148786227262299, 54.27416207544131055, 6.071804965689750588 ) ) ;
#58827 = AXIS2_PLACEMENT_3D ( 'NONE', #57940, #6747, #66046 ) ;
#58828 = ORIENTED_EDGE ( 'NONE', *, *, #49537, .F. ) ;
#58829 = CARTESIAN_POINT ( 'NONE',  ( -5.476751506168961114, -88.16357122866993734, -2.461144630687910784 ) ) ;
#58830 = CARTESIAN_POINT ( 'NONE',  ( -4.079459744843447311, 51.85061720702498178, 7.630866904860004851 ) ) ;
#58831 = VERTEX_POINT ( 'NONE', #98348 ) ;
#58832 = CARTESIAN_POINT ( 'NONE',  ( 27.99999999999999645, 0.000000000000000000, 0.000000000000000000 ) ) ;
#58833 = CARTESIAN_POINT ( 'NONE',  ( 30.36574723454804925, 11.76891213769397027, -39.80121650896548147 ) ) ;
#58834 = CARTESIAN_POINT ( 'NONE',  ( -28.42068399381476951, 41.23824823255147010, -68.38603598170872999 ) ) ;
#58835 = PRODUCT_DEFINITION ( 'UNKNOWN', '', #73079, #8968 ) ;
#58836 = CARTESIAN_POINT ( 'NONE',  ( -96.18239882089940807, -60.00000000000000000, 57.27770282568545923 ) ) ;
#58837 = CARTESIAN_POINT ( 'NONE',  ( 25.59999999999999787, 3.309500000000003439, 4.052968581778167743E-16 ) ) ;
#58838 = CARTESIAN_POINT ( 'NONE',  ( 28.17977184163764193, 1.482358050883964840E-15, 0.000000000000000000 ) ) ;
#58839 = CARTESIAN_POINT ( 'NONE',  ( 33.58349330513379982, -4.000000000000000000, 4.898587196589415787E-16 ) ) ;
#58840 = CARTESIAN_POINT ( 'NONE',  ( -4.441657994893222217, -48.84245552582405736, 104.3851447015591418 ) ) ;
#58842 = DIRECTION ( 'NONE',  ( -1.000000000000000000, -1.224606353822377258E-16, -0.000000000000000000 ) ) ;
#58841 = CARTESIAN_POINT ( 'NONE',  ( 8.737863884121436442, -3.000000000000002665, -90.03618980231149749 ) ) ;
#58843 = CARTESIAN_POINT ( 'NONE',  ( -82.82505532928985303, -42.97746237936155467, 173.7292924292479768 ) ) ;
#58844 = ORIENTED_EDGE ( 'NONE', *, *, #7083, .F. ) ;
#58845 = DIRECTION ( 'NONE',  ( -1.000000000000000000, 0.000000000000000000, 0.000000000000000000 ) ) ;
#58846 = AXIS2_PLACEMENT_3D ( 'NONE', #24877, #90656, #7069 ) ;
#58847 = AXIS2_PLACEMENT_3D ( 'NONE', #101884, #2648, #45262 ) ;
#58848 = ORIENTED_EDGE ( 'NONE', *, *, #78866, .T. ) ;
#58849 = ORIENTED_EDGE ( 'NONE', *, *, #88801, .T. ) ;
#58850 = CARTESIAN_POINT ( 'NONE',  ( 4.000000000000000000, 4.898587196589412829E-16, -2.296599999999999753 ) ) ;
#58851 =( NAMED_UNIT ( * ) SI_UNIT ( $, .STERADIAN. ) SOLID_ANGLE_UNIT ( ) );
#58853 = EDGE_LOOP ( 'NONE', ( #77009, #37930, #79690, #45000, #27654 ) ) ;
#58852 = B_SPLINE_CURVE_WITH_KNOTS ( 'NONE', 3,
 ( #40157, #98391, #104356, #30504, #96298, #31570, #105943, #55267 ),
 .UNSPECIFIED., .F., .F.,
 ( 4, 2, 2, 4 ),
 ( 0.004673709593152147908, 0.005837709341827639065, 0.007001709090503129354, 0.009329708587854111668 ),
 .UNSPECIFIED. ) ;
#58854 = CARTESIAN_POINT ( 'NONE',  ( -18.13825514061547040, 304.6380168175756467, 9.891557803754992051 ) ) ;
#58855 = CARTESIAN_POINT ( 'NONE',  ( -11.25758791135831594, -57.67118876967119689, -44.34807234721190383 ) ) ;
#58856 = CARTESIAN_POINT ( 'NONE',  ( -6.815830331203684977, -1.215378054691643734E-13, -6.171384342982610072 ) ) ;
#58857 = CARTESIAN_POINT ( 'NONE',  ( -7.986468734911287726, -61.02686320276919929, 0.5341897780976098131 ) ) ;
#58858 = CARTESIAN_POINT ( 'NONE',  ( -1.098502313920018514, 54.05124254343373735, 8.382720770029662205 ) ) ;
#58859 = CARTESIAN_POINT ( 'NONE',  ( -13.83893552277105776, -50.53287629637878098, 29.12875707416400317 ) ) ;
#58860 = CARTESIAN_POINT ( 'NONE',  ( -5.000000000000000000, -13.90189243245667683, 9.982568754601910399 ) ) ;
#58861 = CARTESIAN_POINT ( 'NONE',  ( 94.21232436905559382, -59.99999999999992895, 13.85190642028294761 ) ) ;
#58862 = EDGE_CURVE ( 'NONE', #58519, #15506, #85486, .T. ) ;
#58863 = CIRCLE ( 'NONE', #79483, 4.000000000000001776 ) ;
#58864 = CARTESIAN_POINT ( 'NONE',  ( -114.5289996431801853, -60.00000000000001421, 168.5344195898668715 ) ) ;
#58865 = CARTESIAN_POINT ( 'NONE',  ( -59.97350474172178281, -36.01739892119061182, 70.51521107528617449 ) ) ;
#58866 = EDGE_LOOP ( 'NONE', ( #29076, #12081 ) ) ;
#58867 = CARTESIAN_POINT ( 'NONE',  ( 51.84565611112584804, -38.00000000000000711, 53.44666998630373911 ) ) ;
#58868 = CARTESIAN_POINT ( 'NONE',  ( 5.684014467335788190, -59.99999999999997868, 39.61781131791439492 ) ) ;
#58869 = VERTEX_POINT ( 'NONE', #40637 ) ;
#58870 = CARTESIAN_POINT ( 'NONE',  ( 6.142263938024425052, -46.43461817693559368, 31.61885644024033226 ) ) ;
#58871 = CARTESIAN_POINT ( 'NONE',  ( -105.0581500925937064, -52.71025171956128474, 179.5698562497290425 ) ) ;
#58872 = LINE ( 'NONE', #83129, #102888 ) ;
#58873 = ORIENTED_EDGE ( 'NONE', *, *, #74065, .F. ) ;
#58874 = CARTESIAN_POINT ( 'NONE',  ( -2.500000000000001776, -30.00000000000000000, 30.00000000000000000 ) ) ;
#58875 = CARTESIAN_POINT ( 'NONE',  ( -38.12866332992163620, -60.00000000000000000, 49.64653705277643780 ) ) ;
#58876 = CARTESIAN_POINT ( 'NONE',  ( -3.096827034336463669, -0.5867034388794662991, 103.2812265879066729 ) ) ;
#58877 = CARTESIAN_POINT ( 'NONE',  ( -2.977408999572654480, -23.00000000204839523, 7.188101187499999156 ) ) ;
#58878 = CARTESIAN_POINT ( 'NONE',  ( -0.1699131888054048189, 37.20682675849905507, -27.25876984853695006 ) ) ;
#58880 = EDGE_CURVE ( 'NONE', #27209, #48389, #39198, .T. ) ;
#58879 = CARTESIAN_POINT ( 'NONE',  ( 16.96501886467141063, 43.37102725060984199, -6.626625013246036922 ) ) ;
#58881 = CARTESIAN_POINT ( 'NONE',  ( 7.151217271224852290, -83.21250599554284122, -3.587901469523284259 ) ) ;
#58882 = CARTESIAN_POINT ( 'NONE',  ( 84.71872414438772125, -56.33750704051404767, -15.23125129459240235 ) ) ;
#58883 = CARTESIAN_POINT ( 'NONE',  ( -29.99999999998746603, 464.1079104336457704, 10.87617013708814895 ) ) ;
#58884 = EDGE_CURVE ( 'NONE', #26380, #72809, #72669, .T. ) ;
#58885 = CARTESIAN_POINT ( 'NONE',  ( 10.09816733998641780, -12.27101698752137260, 17.29391650327562857 ) ) ;
#58886 = LINE ( 'NONE', #91777, #9945 ) ;
#58887 = CARTESIAN_POINT ( 'NONE',  ( 88.37306242433965053, -60.00000000000005684, 42.86595577526252043 ) ) ;
#58888 = CARTESIAN_POINT ( 'NONE',  ( -31.76327952289363665, -36.02191956708324483, 33.16672948225943429 ) ) ;
#58889 = SURFACE_STYLE_USAGE ( .BOTH. , #41628 ) ;
#58890 = CARTESIAN_POINT ( 'NONE',  ( 42.83239352544314471, -32.61479595472991377, 39.59629545049001109 ) ) ;
#58891 = AXIS2_PLACEMENT_3D ( 'NONE', #66564, #1267, #33690 ) ;
#58892 = CARTESIAN_POINT ( 'NONE',  ( 0.000000000000000000, 50.00000000000000000, 60.50000000000000000 ) ) ;
#58893 = ORIENTED_EDGE ( 'NONE', *, *, #90747, .T. ) ;
#58894 = CARTESIAN_POINT ( 'NONE',  ( 43.78405977006951844, 434.9821340022160712, 12.01170688373657747 ) ) ;
#58895 = VECTOR ( 'NONE', #58563, 1000.000000000000000 ) ;
#58896 = CARTESIAN_POINT ( 'NONE',  ( -76.78645060016569346, -38.43796788105258599, 183.2978527434968896 ) ) ;
#58897 = ORIENTED_EDGE ( 'NONE', *, *, #65772, .T. ) ;
#58899 =( LENGTH_UNIT ( ) NAMED_UNIT ( * ) SI_UNIT ( .MILLI., .METRE. ) );
#58898 = LINE ( 'NONE', #99317, #88289 ) ;
#58900 = CARTESIAN_POINT ( 'NONE',  ( 46.08503313555994652, -59.99999999999999289, 50.75047870711125597 ) ) ;
#58901 = CARTESIAN_POINT ( 'NONE',  ( 15.93287854420844596, 36.64197083639892583, 24.00465449142940244 ) ) ;
#58902 = CARTESIAN_POINT ( 'NONE',  ( -7.302131129577486668, 41.45639756854046709, -59.68093842325847476 ) ) ;
#58903 = CARTESIAN_POINT ( 'NONE',  ( -3.594033448928638297, -9.156975712238446974, 6.225088131883843801 ) ) ;
#58904 = CARTESIAN_POINT ( 'NONE',  ( 8.866506694866188809, 1.474610560812782335E-15, 0.000000000000000000 ) ) ;
#58905 = CARTESIAN_POINT ( 'NONE',  ( -25.95735158692081512, 308.9733421463816399, 9.899401087310158331 ) ) ;
#58906 = CARTESIAN_POINT ( 'NONE',  ( -8.000000000000001776, -25.34375000409676915, 3.313708498984759387 ) ) ;
#58907 = CARTESIAN_POINT ( 'NONE',  ( 106.3924386375468600, -60.00000000000000000, 118.8468287196073305 ) ) ;
#58908 = LINE ( 'NONE', #91799, #32189 ) ;
#58909 = ORIENTED_EDGE ( 'NONE', *, *, #18809, .T. ) ;
#58910 = CARTESIAN_POINT ( 'NONE',  ( -90.43823507282537832, -29.99999999999981171, 190.1885770241697742 ) ) ;
#58911 = VERTEX_POINT ( 'NONE', #89738 ) ;
#58912 = CARTESIAN_POINT ( 'NONE',  ( 42.51801476543153768, 435.0274750839332114, 8.236762145192395579 ) ) ;
#58913 = CARTESIAN_POINT ( 'NONE',  ( 43.03357534759653191, 463.2291678140142608, 4.675918524165872725 ) ) ;
#58914 = CARTESIAN_POINT ( 'NONE',  ( 24.32063559030665090, 305.3189669248208133, 10.26072861867763031 ) ) ;
#58915 = CYLINDRICAL_SURFACE ( 'NONE', #95431, 5.000000000000002665 ) ;
#58916 = CARTESIAN_POINT ( 'NONE',  ( 2.977408999572651815, -21.31250000204838813, 7.188101187500000933 ) ) ;
#58917 = EDGE_CURVE ( 'NONE', #97550, #88846, #2991, .T. ) ;
#58918 = B_SPLINE_CURVE_WITH_KNOTS ( 'NONE', 3,
 ( #44742, #101373, #86272, #85184, #76546 ),
 .UNSPECIFIED., .F., .F.,
 ( 4, 1, 4 ),
 ( 0.000000000000000000, 0.003752776749732570066, 0.007505553499465140131 ),
 .UNSPECIFIED. ) ;
#58919 = CARTESIAN_POINT ( 'NONE',  ( -8.000000000000000000, -11.93750000409677092, -9.797174393178825657E-16 ) ) ;
#58921 = ORIENTED_EDGE ( 'NONE', *, *, #86469, .T. ) ;
#58920 = SURFACE_STYLE_USAGE ( .BOTH. , #19028 ) ;
#58922 = CARTESIAN_POINT ( 'NONE',  ( 81.07868691173642617, -53.41880775793396197, 174.1642699562374901 ) ) ;
#58923 = CARTESIAN_POINT ( 'NONE',  ( 6.800000000000000711, 0.000000000000000000, 5.000000000000000888 ) ) ;
#58924 = SURFACE_STYLE_USAGE ( .BOTH. , #18477 ) ;
#58925 = ORIENTED_EDGE ( 'NONE', *, *, #87726, .T. ) ;
#58926 = MECHANICAL_DESIGN_GEOMETRIC_PRESENTATION_REPRESENTATION (  '', ( #31380 ), #84703 ) ;
#58927 = CARTESIAN_POINT ( 'NONE',  ( -62.95721822007438107, 50.00000000000000000, 4.916537939864575435 ) ) ;
#58928 = FACE_OUTER_BOUND ( 'NONE', #57387, .T. ) ;
#58929 = CARTESIAN_POINT ( 'NONE',  ( 4.401442555609581635E-16, -9.781250002048384573, -7.188101187500000044 ) ) ;
#58930 = CARTESIAN_POINT ( 'NONE',  ( 32.25691083757155297, 485.8985639246220103, 4.832559767444084997 ) ) ;
#58931 = CARTESIAN_POINT ( 'NONE',  ( -5.092539576892240127, 252.4432346720841167, 3.177249149099059977 ) ) ;
#58932 = CARTESIAN_POINT ( 'NONE',  ( -33.14133759817422487, 415.2060550120342555, 25.73546352636587287 ) ) ;
#58933 = CARTESIAN_POINT ( 'NONE',  ( -32.04918168811659740, 435.9039269519959134, 19.85355728535080644 ) ) ;
#58934 = EDGE_CURVE ( 'NONE', #106160, #23116, #75127, .T. ) ;
#58935 = VERTEX_POINT ( 'NONE', #14758 ) ;
#58937 = CARTESIAN_POINT ( 'NONE',  ( -1.128077836147719282, 302.8478239976500390, 9.936168295454388399 ) ) ;
#58936 =( GEOMETRIC_REPRESENTATION_CONTEXT ( 3 ) GLOBAL_UNCERTAINTY_ASSIGNED_CONTEXT ( ( #50501 ) ) GLOBAL_UNIT_ASSIGNED_CONTEXT ( ( #65367, #31954, #40554 ) ) REPRESENTATION_CONTEXT ( 'NONE', 'WORKASPACE' ) );
#58938 = CARTESIAN_POINT ( 'NONE',  ( 34.35000000000000142, -3.309499999999999886, 0.000000000000000000 ) ) ;
#58939 = AXIS2_PLACEMENT_3D ( 'NONE', #78560, #64518, #104976 ) ;
#58940 = CARTESIAN_POINT ( 'NONE',  ( -6.874999999999997335, 4.690970937165706900, -7.298562697733107285 ) ) ;
#58941 = CARTESIAN_POINT ( 'NONE',  ( 2.977408999572650927, -33.87500000204838813, -7.188101187500001821 ) ) ;
#58942 = DIRECTION ( 'NONE',  ( -0.5735764363510497121, 0.8191520442889892450, 1.003171929053521665E-16 ) ) ;
#58943 = DIRECTION ( 'NONE',  ( 0.000000000000000000, 0.000000000000000000, -1.000000000000000000 ) ) ;
#58944 = ADVANCED_FACE ( 'NONE', ( #80556 ), #6676, .T. ) ;
#58945 = CARTESIAN_POINT ( 'NONE',  ( 41.36052874979234417, 437.1976709138604065, 21.04111601629670858 ) ) ;
#58946 = VERTEX_POINT ( 'NONE', #25566 ) ;
#58947 = CARTESIAN_POINT ( 'NONE',  ( 0.4153015812548951913, 43.19870208648286791, 18.68195870105203937 ) ) ;
#58948 = CARTESIAN_POINT ( 'NONE',  ( 0.000000000000000000, 0.000000000000000000, 0.000000000000000000 ) ) ;
#58949 = EDGE_CURVE ( 'NONE', #7253, #8789, #26625, .T. ) ;
#58950 = CARTESIAN_POINT ( 'NONE',  ( 24.83349330513380693, 4.000000000000002665, 0.000000000000000000 ) ) ;
#58951 = B_SPLINE_CURVE_WITH_KNOTS ( 'NONE', 3,
 ( #35674, #9211, #33524, #100358 ),
 .UNSPECIFIED., .F., .F.,
 ( 4, 4 ),
 ( 6.938893903907227607E-18, 0.001714393297546037542 ),
 .UNSPECIFIED. ) ;
#58952 = VECTOR ( 'NONE', #23598, 1000.000000000000000 ) ;
#58953 = ORIENTED_EDGE ( 'NONE', *, *, #42951, .F. ) ;
#58954 = FACE_OUTER_BOUND ( 'NONE', #11323, .T. ) ;
#58955 = DIRECTION ( 'NONE',  ( 0.000000000000000000, 0.000000000000000000, 1.000000000000000000 ) ) ;
#58956 = CARTESIAN_POINT ( 'NONE',  ( 107.1550168409930137, -57.67119843336974583, 111.3111582704399041 ) ) ;
#58957 = AXIS2_PLACEMENT_3D ( 'NONE', #18575, #30924, #96169 ) ;
#58958 = ORIENTED_EDGE ( 'NONE', *, *, #5066, .F. ) ;
#58959 = ADVANCED_FACE ( 'NONE', ( #25016 ), #41178, .F. ) ;
#58960 = LINE ( 'NONE', #91846, #57489 ) ;
#58961 = CONICAL_SURFACE ( 'NONE', #96852, 3.400000000000000355, 0.9599310885968748153 ) ;
#58962 = CARTESIAN_POINT ( 'NONE',  ( -9.686475303456768771, 51.27220077796494735, -3.328476344197629277 ) ) ;
#58963 = CARTESIAN_POINT ( 'NONE',  ( 6.928203230275510549, -10.00000000000000888, 4.000000000000000000 ) ) ;
#58964 = DIRECTION ( 'NONE',  ( -1.000000000000000000, 0.000000000000000000, 0.000000000000000000 ) ) ;
#58965 = CARTESIAN_POINT ( 'NONE',  ( -77.43895560779745324, -59.99999999999999289, 191.5917464367579157 ) ) ;
#58967 = AXIS2_PLACEMENT_3D ( 'NONE', #48260, #96840, #89279 ) ;
#58966 = CARTESIAN_POINT ( 'NONE',  ( 9.038828898411519930, 43.85145043581746904, -14.27146690660104511 ) ) ;
#58968 = DIRECTION ( 'NONE',  ( -1.000000000000000000, 0.000000000000000000, 0.000000000000000000 ) ) ;
#58969 = DIRECTION ( 'NONE',  ( 1.000000000000000000, 0.000000000000000000, -0.000000000000000000 ) ) ;
#58970 = CARTESIAN_POINT ( 'NONE',  ( -83.68245790527700478, -53.75685130900239272, 188.1406773380694801 ) ) ;
#58972 = EDGE_CURVE ( 'NONE', #80654, #56333, #84132, .T. ) ;
#58971 = ORIENTED_EDGE ( 'NONE', *, *, #14482, .T. ) ;
#58973 =( NAMED_UNIT ( * ) SI_UNIT ( $, .STERADIAN. ) SOLID_ANGLE_UNIT ( ) );
#58974 = ORIENTED_EDGE ( 'NONE', *, *, #17013, .F. ) ;
#58975 = DIRECTION ( 'NONE',  ( 0.8308658609248572580, 0.5564727496918387972, 0.000000000000000000 ) ) ;
#58976 = CARTESIAN_POINT ( 'NONE',  ( 4.195612334302333046, -1.058759987296113314, 104.4881327927231922 ) ) ;
#58977 = CARTESIAN_POINT ( 'NONE',  ( -83.18894126570232572, -37.77377736952604437, -9.182727467238077423 ) ) ;
#58978 = CARTESIAN_POINT ( 'NONE',  ( -3.717184411740621197, -9.782292260249612070, -11.42823731287377242 ) ) ;
#58979 = CARTESIAN_POINT ( 'NONE',  ( -3.948926469565266828, 15.90677080288882905, -5.000000000000000888 ) ) ;
#58980 = DIRECTION ( 'NONE',  ( 0.000000000000000000, 1.000000000000000000, 0.000000000000000000 ) ) ;
#58981 = DIRECTION ( 'NONE',  ( 0.000000000000000000, 0.000000000000000000, 1.000000000000000000 ) ) ;
#58982 = CARTESIAN_POINT ( 'NONE',  ( 3.415272474501187094, -0.8295767683060059072, 103.8818886975935385 ) ) ;
#58983 = CARTESIAN_POINT ( 'NONE',  ( -1.309564884278361513E-05, -14.21045842199434972, 34.36840973699906243 ) ) ;
#58984 = FACE_OUTER_BOUND ( 'NONE', #35313, .T. ) ;
#58985 = CARTESIAN_POINT ( 'NONE',  ( -8.309739744518550353, -29.99999999999999289, -39.88085837097889197 ) ) ;
#58986 = CARTESIAN_POINT ( 'NONE',  ( -70.47106563611271213, -46.43826247965927223, 107.5521328375196646 ) ) ;
#58987 = VERTEX_POINT ( 'NONE', #8799 ) ;
#58988 = CARTESIAN_POINT ( 'NONE',  ( 70.37902863207267501, -59.99999999999998579, 160.1157867729151576 ) ) ;
#58989 = CARTESIAN_POINT ( 'NONE',  ( -11.84571380832733567, 40.83929531345456354, 63.98140447915187679 ) ) ;
#58990 = CARTESIAN_POINT ( 'NONE',  ( 93.55289619466658735, -57.65399935213944360, -15.69912234267622786 ) ) ;
#58991 = ORIENTED_EDGE ( 'NONE', *, *, #55756, .F. ) ;
#58992 = CARTESIAN_POINT ( 'NONE',  ( 14.73061849464112782, 41.88685504477518862, -82.04001408458998412 ) ) ;
#58993 = DIRECTION ( 'NONE',  ( -1.000000000000000000, -0.000000000000000000, -0.000000000000000000 ) ) ;
#58994 = VERTEX_POINT ( 'NONE', #84290 ) ;
#58995 = DIRECTION ( 'NONE',  ( 0.000000000000000000, 1.000000000000000000, 0.000000000000000000 ) ) ;
#58996 =( LENGTH_UNIT ( ) NAMED_UNIT ( * ) SI_UNIT ( .MILLI., .METRE. ) );
#58997 = CARTESIAN_POINT ( 'NONE',  ( 13.09999999999999787, -3.309499999999999886, 0.000000000000000000 ) ) ;
#58998 = CARTESIAN_POINT ( 'NONE',  ( 2.977408999572651815, -13.43750000204838457, 7.188101187500000933 ) ) ;
#58999 = CARTESIAN_POINT ( 'NONE',  ( -5.656854249492379694, -18.12500000409676915, -5.656854249492380582 ) ) ;
#59000 = CONICAL_SURFACE ( 'NONE', #17662, 4.000000000000001776, 0.9599310885968808105 ) ;
#59001 = CARTESIAN_POINT ( 'NONE',  ( 25.05982991920905079, -4.285714285714295357, 3.301565691951511727 ) ) ;
#59002 = FILL_AREA_STYLE_COLOUR ( '', #1273 ) ;
#59003 = CYLINDRICAL_SURFACE ( 'NONE', #69269, 4.000000000000000888 ) ;
#59004 = EDGE_CURVE ( 'NONE', #48048, #52425, #20304, .T. ) ;
#59005 = CARTESIAN_POINT ( 'NONE',  ( 6.901579824520447382, -4.675625068323824962, -0.7022220667781352565 ) ) ;
#59006 = DIRECTION ( 'NONE',  ( 0.000000000000000000, 0.000000000000000000, 1.000000000000000000 ) ) ;
#59007 = ORIENTED_EDGE ( 'NONE', *, *, #75502, .T. ) ;
#59008 = CARTESIAN_POINT ( 'NONE',  ( -7.432465545960663000, 40.29241764077763577, -70.20619433869296699 ) ) ;
#59010 = CARTESIAN_POINT ( 'NONE',  ( 31.01919067370845440, -22.13396283368982509, 30.33425209178049897 ) ) ;
#59009 = CARTESIAN_POINT ( 'NONE',  ( -3.626288723284335713, -48.95575889185635532, 104.3502830461760453 ) ) ;
#59011 = CARTESIAN_POINT ( 'NONE',  ( 28.72726883065406156, 309.6741498678223365, -7.894823244335800183 ) ) ;
#59012 = EDGE_CURVE ( 'NONE', #10346, #57566, #40374, .T. ) ;
#59013 = ORIENTED_EDGE ( 'NONE', *, *, #9459, .T. ) ;
#59014 = CARTESIAN_POINT ( 'NONE',  ( 58.18888888888888999, 6.915964383211875250E-15, 0.000000000000000000 ) ) ;
#59015 = UNCERTAINTY_MEASURE_WITH_UNIT (LENGTH_MEASURE( 1.000000000000000082E-05 ), #89263, 'distance_accuracy_value', 'NONE');
#59016 = VERTEX_POINT ( 'NONE', #65975 ) ;
#59018 = CARTESIAN_POINT ( 'NONE',  ( 4.606548227981510202, 6.456511556909250160, -7.591235721156635030 ) ) ;
#59017 = DIRECTION ( 'NONE',  ( -1.000000000000000000, -1.224606353822377258E-16, -0.000000000000000000 ) ) ;
#59019 = DIRECTION ( 'NONE',  ( -1.000000000000000000, -0.000000000000000000, -0.000000000000000000 ) ) ;
#59020 = DIRECTION ( 'NONE',  ( 0.000000000000000000, 0.000000000000000000, -1.000000000000000000 ) ) ;
#59021 = CARTESIAN_POINT ( 'NONE',  ( -33.77559172535808329, 464.7834715296605737, 7.192701217093241617 ) ) ;
#59022 = CARTESIAN_POINT ( 'NONE',  ( -30.00000000000000000, 7.347880794884117764E-16, -5.999999999999998224 ) ) ;
#59023 = CARTESIAN_POINT ( 'NONE',  ( -37.13212445136107931, 463.5388707510370523, 19.67708231431734234 ) ) ;
#59024 = VERTEX_POINT ( 'NONE', #49789 ) ;
#59025 = CARTESIAN_POINT ( 'NONE',  ( 87.62530314318119906, -60.00000000000001421, -22.00415342985933620 ) ) ;
#59026 = CARTESIAN_POINT ( 'NONE',  ( -9.522120649308517315, 45.61249502152109159, 15.15976961885335328 ) ) ;
#59027 = FACE_OUTER_BOUND ( 'NONE', #38307, .T. ) ;
#59028 = SURFACE_SIDE_STYLE ('',( #49854 ) ) ;
#59029 =( BOUNDED_SURFACE ( )  B_SPLINE_SURFACE ( 3, 2, ( 
 ( #104772, #80478, #81010 ),
 ( #38470, #37959, #46019 ),
 ( #64331, #71865, #70821 ),
 ( #22825, #103711, #22295 ),
 ( #88072, #55141, #29858 ),
 ( #62736, #97201, #72402 ) ),
 .UNSPECIFIED., .F., .F., .F. ) 
 B_SPLINE_SURFACE_WITH_KNOTS ( ( 4, 2, 4 ),
 ( 3, 3 ),
 ( 0.003199762745115995472, 0.007302762474435748469, 0.01140576220375550190 ),
 ( 0.000000000000000000, 1.000000000000000000 ),
 .UNSPECIFIED. ) 
 GEOMETRIC_REPRESENTATION_ITEM ( )  RATIONAL_B_SPLINE_SURFACE ( (
 ( 1.000000000000000000, 0.8047731410850431644, 1.000000000000000000),
 ( 1.000000000000000000, 0.8125552299162031034, 1.000000000000000000),
 ( 1.000000000000000000, 0.8191520442882217479, 1.000000000000000000),
 ( 1.000000000000000000, 0.8191520442897580745, 1.000000000000000000),
 ( 1.000000000000000000, 0.8125552299150486935, 1.000000000000000000),
 ( 1.000000000000000000, 0.8047731410850426093, 1.000000000000000000) ) ) 
 REPRESENTATION_ITEM ( '' )  SURFACE ( )  );
#59030 = CARTESIAN_POINT ( 'NONE',  ( 8.559508646656350805, -1.200000000000000030E-05, -4.031152949374623873 ) ) ;
#59031 = ORIENTED_EDGE ( 'NONE', *, *, #80906, .F. ) ;
#59032 = EDGE_CURVE ( 'NONE', #88005, #50075, #49489, .T. ) ;
#59033 = CARTESIAN_POINT ( 'NONE',  ( 93.39999999999999147, 4.172000000000019249, 5.109226446042768454E-16 ) ) ;
#59034 = ORIENTED_EDGE ( 'NONE', *, *, #53828, .F. ) ;
#59035 = VERTEX_POINT ( 'NONE', #26107 ) ;
#59036 = CARTESIAN_POINT ( 'NONE',  ( 8.000086790516061086, 80.99982641893991797, 0.2639471549312809029 ) ) ;
#59037 = FACE_OUTER_BOUND ( 'NONE', #102090, .T. ) ;
#59038 = CARTESIAN_POINT ( 'NONE',  ( 38.54515645702225868, 1.482358050883964840E-15, 0.000000000000000000 ) ) ;
#59039 = CARTESIAN_POINT ( 'NONE',  ( 39.34999999999999432, -3.309499999999999886, 4.475777889183790779E-16 ) ) ;
#59040 = CARTESIAN_POINT ( 'NONE',  ( 84.53209051610372171, -52.74422840206830898, -14.22539307012042897 ) ) ;
#59041 = AXIS2_PLACEMENT_3D ( 'NONE', #50136, #83045, #15643 ) ;
#59042 = CARTESIAN_POINT ( 'NONE',  ( -35.84216525457394198, 303.7309719522399405, 0.04073617280396817086 ) ) ;
#59043 = CARTESIAN_POINT ( 'NONE',  ( -5.285714285714286476, 0.1991252733425830368, 103.1763305333244318 ) ) ;
#59044 = CARTESIAN_POINT ( 'NONE',  ( 12.50000000000000178, 40.45931421048912568, -67.96789048815475098 ) ) ;
#59045 = ORIENTED_EDGE ( 'NONE', *, *, #64195, .F. ) ;
#59046 = CARTESIAN_POINT ( 'NONE',  ( -7.000000000000000000, 8.572527594031471218E-16, -13.00000000000000000 ) ) ;
#59047 = VERTEX_POINT ( 'NONE', #90797 ) ;
#59048 = ADVANCED_FACE ( 'NONE', ( #58424 ), #42722, .T. ) ;
#59049 = CARTESIAN_POINT ( 'NONE',  ( 9.307029794195086581, 51.55217658689417703, -1.766585395468054376 ) ) ;
#59050 =( NAMED_UNIT ( * ) PLANE_ANGLE_UNIT ( ) SI_UNIT ( $, .RADIAN. ) );
#59052 = VERTEX_POINT ( 'NONE', #50836 ) ;
#59051 = CARTESIAN_POINT ( 'NONE',  ( 5.373715277452113526, 41.43915641971339170, -58.48990532576927848 ) ) ;
#59053 = CARTESIAN_POINT ( 'NONE',  ( 74.57620098502422934, -56.84629149567740569, 131.8975596435294051 ) ) ;
#59054 = VERTEX_POINT ( 'NONE', #33631 ) ;
#59055 = DIRECTION ( 'NONE',  ( -1.000000000000000000, -0.000000000000000000, -0.000000000000000000 ) ) ;
#59056 = CARTESIAN_POINT ( 'NONE',  ( 2.977408999572650927, -23.37500000204838457, -7.188101187500000933 ) ) ;
#59057 = CARTESIAN_POINT ( 'NONE',  ( -114.2112478298105174, -57.67107988235927252, 175.3835541016526349 ) ) ;
#59058 = ADVANCED_FACE ( 'NONE', ( #1208 ), #99383, .F. ) ;
#59059 = B_SPLINE_CURVE_WITH_KNOTS ( 'NONE', 3,
 ( #82781, #57958, #18067, #90883, #98429, #8355, #16998, #42314, #74144, #17535, #8883, #50925 ),
 .UNSPECIFIED., .F., .F.,
 ( 4, 2, 2, 2, 2, 4 ),
 ( 5.204170427930421283E-18, 0.001828837400933321523, 0.002743256101399958215, 0.003657674801866594907, 0.005486512202799889541, 0.007315349603733184609 ),
 .UNSPECIFIED. ) ;
#59060 = ORIENTED_EDGE ( 'NONE', *, *, #53704, .F. ) ;
#59061 =( NAMED_UNIT ( * ) PLANE_ANGLE_UNIT ( ) SI_UNIT ( $, .RADIAN. ) );
#59062 = CARTESIAN_POINT ( 'NONE',  ( 16.08349330513380337, -4.000000000000000000, 4.898587196589415787E-16 ) ) ;
#59063 = CARTESIAN_POINT ( 'NONE',  ( 103.3363776539765837, -45.28277147255930402, 183.6174014516545014 ) ) ;
#59064 = CARTESIAN_POINT ( 'NONE',  ( -37.40765518169981618, 27.94113209487581528, -10.95617127781004108 ) ) ;
#59065 = CARTESIAN_POINT ( 'NONE',  ( 5.000000000000000000, 6.123233995736766282E-16, -5.710657142857142432 ) ) ;
#59066 = CARTESIAN_POINT ( 'NONE',  ( -8.000000000000000000, -20.93750000409676915, -9.797174393178825657E-16 ) ) ;
#59067 = FACE_OUTER_BOUND ( 'NONE', #35898, .T. ) ;
#59068 = CARTESIAN_POINT ( 'NONE',  ( 38.58349330513380693, 1.593028355512270567E-15, 0.000000000000000000 ) ) ;
#59069 = AXIS2_PLACEMENT_3D ( 'NONE', #45731, #70547, #27999 ) ;
#59070 = DIRECTION ( 'NONE',  ( 0.000000000000000000, -1.000000000000000000, 0.000000000000000000 ) ) ;
#59071 = CARTESIAN_POINT ( 'NONE',  ( 9.177080501238306098, 30.53346942854269841, -3.972956046786646489 ) ) ;
#59072 = DIRECTION ( 'NONE',  ( 0.000000000000000000, -1.000000000000000000, 0.000000000000000000 ) ) ;
#59073 = CARTESIAN_POINT ( 'NONE',  ( 51.88291765283136669, 392.2656245483042312, 267.1969486012846460 ) ) ;
#59074 = CARTESIAN_POINT ( 'NONE',  ( -2.563280883359797091, 15.30085158940939394, -9.673800154114783112 ) ) ;
#59075 = EDGE_LOOP ( 'NONE', ( #13657, #70243 ) ) ;
#59076 = CARTESIAN_POINT ( 'NONE',  ( 32.89379909751026076, 463.7243792478176942, 7.148845075438556407 ) ) ;
#59077 = CARTESIAN_POINT ( 'NONE',  ( 89.06666666666666288, 4.172000000000019249, 5.109226446042768454E-16 ) ) ;
#59078 = LINE ( 'NONE', #85482, #79004 ) ;
#59079 = CARTESIAN_POINT ( 'NONE',  ( -87.74548785222465597, -29.99999999999999645, 186.1198533190938065 ) ) ;
#59080 = ADVANCED_FACE ( 'NONE', ( #4970 ), #47866, .F. ) ;
#59081 = ORIENTED_EDGE ( 'NONE', *, *, #42553, .T. ) ;
#59082 = DIRECTION ( 'NONE',  ( 0.5564727496918402405, -0.8308658609248562588, -0.000000000000000000 ) ) ;
#59083 = CONICAL_SURFACE ( 'NONE', #12559, 3.309500000000001663, 0.9599310885968770357 ) ;
#59084 = CARTESIAN_POINT ( 'NONE',  ( 71.42520752688669461, -57.67999775105185023, 166.3006026438890501 ) ) ;
#59086 = DIRECTION ( 'NONE',  ( -0.000000000000000000, 1.000000000000000000, -0.000000000000000000 ) ) ;
#59085 = CARTESIAN_POINT ( 'NONE',  ( -14.11595029532502110, 2.410436752314748521, -5.024000119269303788 ) ) ;
#59087 = EDGE_CURVE ( 'NONE', #89914, #104058, #1770, .T. ) ;
#59088 = CARTESIAN_POINT ( 'NONE',  ( 50.68724043103767940, -35.71711597358190460, -36.05002623880317714 ) ) ;
#59089 = FACE_OUTER_BOUND ( 'NONE', #31776, .T. ) ;
#59090 = CARTESIAN_POINT ( 'NONE',  ( 21.08349330513380337, 1.593028355512270567E-15, 0.000000000000000000 ) ) ;
#59091 = CARTESIAN_POINT ( 'NONE',  ( -35.74889062647464755, -60.00000000000000711, 47.10998833530662466 ) ) ;
#59092 = ADVANCED_FACE ( 'NONE', ( #20679 ), #103008, .F. ) ;
#59093 = LINE ( 'NONE', #69317, #67513 ) ;
#59094 = CARTESIAN_POINT ( 'NONE',  ( 11.91432047182400211, 48.00000000000000000, 64.17585289259234571 ) ) ;
#59095 = CARTESIAN_POINT ( 'NONE',  ( -86.70368346074813815, -35.45285400290258337, 187.4689298322265927 ) ) ;
#59096 = EDGE_CURVE ( 'NONE', #64859, #18717, #89234, .T. ) ;
#59097 = VERTEX_POINT ( 'NONE', #71282 ) ;
#59098 = CARTESIAN_POINT ( 'NONE',  ( 22.57792046605466041, 1.340359594676612611E-15, 0.000000000000000000 ) ) ;
#59099 = CARTESIAN_POINT ( 'NONE',  ( -7.031243609050225274, -25.54944219989091536, 28.13822752949184292 ) ) ;
#59100 = DIRECTION ( 'NONE',  ( -1.000000000000000000, -0.000000000000000000, -0.000000000000000000 ) ) ;
#59101 = CARTESIAN_POINT ( 'NONE',  ( -1.469576158976823947E-15, -11.37499999999999289, 8.000000000000000000 ) ) ;
#59102 = CIRCLE ( 'NONE', #36734, 4.000000000000000888 ) ;
#59103 = B_SPLINE_CURVE_WITH_KNOTS ( 'NONE', 3,
 ( #56031, #39884, #46382, #79271, #105143, #5395, #7486, #38830 ),
 .UNSPECIFIED., .F., .F.,
 ( 4, 2, 2, 4 ),
 ( -5.999999999613023197E-08, 0.002878992039937437828, 0.005758044079874871830, 0.01151614815974974504 ),
 .UNSPECIFIED. ) ;
#59105 = CARTESIAN_POINT ( 'NONE',  ( 5.125760364506777300, -62.79129649437295058, 13.92958920382542232 ) ) ;
#59104 = CARTESIAN_POINT ( 'NONE',  ( -42.58872141072839668, 362.7331401274527138, 16.77583143465006899 ) ) ;
#59106 = ORIENTED_EDGE ( 'NONE', *, *, #85721, .F. ) ;
#59107 = CARTESIAN_POINT ( 'NONE',  ( 26.02871520198998923, 34.91972164802428580, 9.463174369590962698 ) ) ;
#59108 = PRESENTATION_LAYER_ASSIGNMENT (  '', '', ( #22943 ) ) ;
#59109 = CARTESIAN_POINT ( 'NONE',  ( -8.068282690937467194, -4.999999999999939604, -15.79776062907038714 ) ) ;
#59110 = CARTESIAN_POINT ( 'NONE',  ( -30.42698073564638150, 7.740609016700346956, -41.86289218232771248 ) ) ;
#59111 = AXIS2_PLACEMENT_3D ( 'NONE', #35591, #96463, #105079 ) ;
#59112 = CARTESIAN_POINT ( 'NONE',  ( 29.27755364888704648, 297.1129628640473470, -9.507834925361459355 ) ) ;
#59113 = CARTESIAN_POINT ( 'NONE',  ( 24.37088254901632567, 295.3567874699774620, -9.892597027135842325 ) ) ;
#59114 = FILL_AREA_STYLE ('',( #9466 ) ) ;
#59115 = CARTESIAN_POINT ( 'NONE',  ( -43.00000000000000000, 488.9831568219305495, 4.757012338623821890 ) ) ;
#59116 = CARTESIAN_POINT ( 'NONE',  ( 104.7858654919042465, -14.21045842199433018, 190.1692295410596785 ) ) ;
#59117 = CARTESIAN_POINT ( 'NONE',  ( -80.89312144681923655, -39.50098901946147123, 151.8499635546424713 ) ) ;
#59118 = ORIENTED_EDGE ( 'NONE', *, *, #64902, .F. ) ;
#59119 = DIRECTION ( 'NONE',  ( 0.000000000000000000, 0.000000000000000000, 1.000000000000000000 ) ) ;
#59120 = CARTESIAN_POINT ( 'NONE',  ( -9.797372177749780420, 253.4650949484755813, 2.014953862275830954 ) ) ;
#59121 = CARTESIAN_POINT ( 'NONE',  ( -7.500000000000000000, 4.330127018922188320, -0.9999999999999904521 ) ) ;
#59122 = CARTESIAN_POINT ( 'NONE',  ( 43.65263200446639047, 415.3088531594569304, 15.97955559133532688 ) ) ;
#59123 = EDGE_LOOP ( 'NONE', ( #45475, #28949, #73426, #66146 ) ) ;
#59124 = B_SPLINE_CURVE_WITH_KNOTS ( 'NONE', 3,
 ( #2825, #101538, #44366, #93457 ),
 .UNSPECIFIED., .F., .F.,
 ( 4, 4 ),
 ( 1.250926888277100303E-17, 0.001935030059085742068 ),
 .UNSPECIFIED. ) ;
#59125 = UNCERTAINTY_MEASURE_WITH_UNIT (LENGTH_MEASURE( 1.000000000000000082E-05 ), #25521, 'distance_accuracy_value', 'NONE');
#59126 = CARTESIAN_POINT ( 'NONE',  ( -19.70764564238368877, 304.7954121406193053, 9.925013215726828264 ) ) ;
#59127 = VERTEX_POINT ( 'NONE', #22768 ) ;
#59128 = DIRECTION ( 'NONE',  ( 0.5735764363510557073, -0.8191520442889850262, 1.003171929053516612E-16 ) ) ;
#59129 = CARTESIAN_POINT ( 'NONE',  ( -0.7018335428337032500, 15.23280014800325866, 9.981531048852463783 ) ) ;
#59130 = DIRECTION ( 'NONE',  ( 0.000000000000000000, -0.8802307401770257389, 0.4745459346021264069 ) ) ;
#59131 = ADVANCED_FACE ( 'NONE', ( #38933 ), #96103, .F. ) ;
#59132 = CARTESIAN_POINT ( 'NONE',  ( 62.91825180719526145, 50.00000000000000000, 6.605622457241173251 ) ) ;
#59133 = CARTESIAN_POINT ( 'NONE',  ( 5.977446511978467214, -14.23238268869237544, 14.05797248975824409 ) ) ;
#59134 = CARTESIAN_POINT ( 'NONE',  ( 46.00000000000000000, 436.1561742938424118, 10.01163487455054657 ) ) ;
#59135 = VERTEX_POINT ( 'NONE', #41439 ) ;
#59136 = CARTESIAN_POINT ( 'NONE',  ( 103.6331730138933835, -59.99999999999997868, 200.2368587013084777 ) ) ;
#59138 = CARTESIAN_POINT ( 'NONE',  ( 18.94558499360540438, -35.99294546495131186, 30.30127317126159170 ) ) ;
#59137 = CARTESIAN_POINT ( 'NONE',  ( -79.57248154261856143, -14.21045842199419873, 190.0114072710836979 ) ) ;
#59139 = DIRECTION ( 'NONE',  ( 0.000000000000000000, 0.000000000000000000, 1.000000000000000000 ) ) ;
#59141 = ADVANCED_FACE ( 'NONE', ( #41968 ), #99127, .F. ) ;
#59140 = DIRECTION ( 'NONE',  ( -0.000000000000000000, 1.000000000000000000, 0.000000000000000000 ) ) ;
#59142 = CARTESIAN_POINT ( 'NONE',  ( -39.50170393843561811, -46.43499008709606812, 39.80097614461234912 ) ) ;
#59143 = CARTESIAN_POINT ( 'NONE',  ( -25.95755237147325545, 18.64284798593299186, -28.33950252051109686 ) ) ;
#59144 = UNCERTAINTY_MEASURE_WITH_UNIT (LENGTH_MEASURE( 1.000000000000000082E-05 ), #11342, 'distance_accuracy_value', 'NONE');
#59145 = ORIENTED_EDGE ( 'NONE', *, *, #48835, .T. ) ;
#59146 = DIRECTION ( 'NONE',  ( -1.000000000000000000, -0.000000000000000000, -0.000000000000000000 ) ) ;
#59147 = CARTESIAN_POINT ( 'NONE',  ( 7.578349687282027958, 54.07909211381803516, 3.571884340861890994 ) ) ;
#59148 = CARTESIAN_POINT ( 'NONE',  ( 23.61963550967466574, 306.0340374937824777, 10.19690224617928287 ) ) ;
#59149 = COLOUR_RGB ( '', 0.09019608, 0.27058824, 0.51372549) ;
#59150 = CARTESIAN_POINT ( 'NONE',  ( 6.562974947121713143, 7.579827465851454171, 0.5629870116737619723 ) ) ;
#59151 = CARTESIAN_POINT ( 'NONE',  ( -30.00000000000000355, 490.5636507776912367, 7.413185101876573313 ) ) ;
#59152 = VERTEX_POINT ( 'NONE', #95572 ) ;
#59153 = CARTESIAN_POINT ( 'NONE',  ( 3.636386562469240082E-15, 36.30024107553216339, 29.75000000000000355 ) ) ;
#59154 = ORIENTED_EDGE ( 'NONE', *, *, #2047, .F. ) ;
#59155 = CARTESIAN_POINT ( 'NONE',  ( 45.71963875501239016, -29.99999999999998934, 56.30994126864622729 ) ) ;
#59156 = CARTESIAN_POINT ( 'NONE',  ( 21.52118987190722166, 41.77684893734424776, -77.65348390093303976 ) ) ;
#59157 = AXIS2_PLACEMENT_3D ( 'NONE', #92234, #34051, #57736 ) ;
#59158 = UNCERTAINTY_MEASURE_WITH_UNIT (LENGTH_MEASURE( 1.000000000000000082E-05 ), #69373, 'distance_accuracy_value', 'NONE');
#59159 = LINE ( 'NONE', #92041, #1315 ) ;
#59160 = CARTESIAN_POINT ( 'NONE',  ( 96.86866073052655679, 1.030564683017419500E-14, 0.000000000000000000 ) ) ;
#59161 = CARTESIAN_POINT ( 'NONE',  ( 83.28690719690919764, -30.00000000000000000, 45.18924137544603070 ) ) ;
#59162 = CONICAL_SURFACE ( 'NONE', #12622, 8.000000000000000000, 0.9599310885968911355 ) ;
#59163 = EDGE_LOOP ( 'NONE', ( #43389, #14744 ) ) ;
#59164 = ADVANCED_FACE ( 'NONE', ( #22236 ), #81343, .F. ) ;
#59165 = B_SPLINE_CURVE_WITH_KNOTS ( 'NONE', 3,
 ( #38204, #79683, #61942, #93756, #37143, #61401, #5794, #38715, #94293, #20458, #53299, #102909, #62456, #94835, #63523, #14397, #49431, #31176, #80204, #64578 ),
 .UNSPECIFIED., .F., .F.,
 ( 4, 2, 2, 2, 2, 2, 2, 2, 2, 4 ),
 ( 0.000000000000000000, 0.0008044152215796346881, 0.001608830443159269376, 0.002413245664738903739, 0.003217660886318538752, 0.004826491329477807478, 0.006435321772637075770, 0.008044152215796343194, 0.009652982658955611486, 0.01287064354527419144 ),
 .UNSPECIFIED. ) ;
#59166 = ORIENTED_EDGE ( 'NONE', *, *, #105476, .F. ) ;
#59167 = VERTEX_POINT ( 'NONE', #36056 ) ;
#59168 = CARTESIAN_POINT ( 'NONE',  ( -32.72541600402464468, 465.0324911293606647, 11.87889517178131982 ) ) ;
#59169 = CARTESIAN_POINT ( 'NONE',  ( 21.36650669486618881, 1.474610560812782335E-15, 0.000000000000000000 ) ) ;
#59170 = CIRCLE ( 'NONE', #91867, 62.00000000000000000 ) ;
#59171 = CARTESIAN_POINT ( 'NONE',  ( -37.17158346111747136, 25.88889118293631952, -11.01749528737839157 ) ) ;
#59172 = CARTESIAN_POINT ( 'NONE',  ( 37.98996485649870891, 439.4613508614656325, 23.87710038502308763 ) ) ;
#59173 = CARTESIAN_POINT ( 'NONE',  ( 5.975663821521734143, 4.257391242883570293, -5.625982059626840837 ) ) ;
#59174 = FACE_OUTER_BOUND ( 'NONE', #32535, .T. ) ;
#59175 = ORIENTED_EDGE ( 'NONE', *, *, #90372, .F. ) ;
#59176 = CARTESIAN_POINT ( 'NONE',  ( 9.739726766101595601, 49.99999999999999289, -87.61747884500120165 ) ) ;
#59177 = VERTEX_POINT ( 'NONE', #2034 ) ;
#59178 = CARTESIAN_POINT ( 'NONE',  ( 33.12944332324993013, 439.4248878830264857, 23.85028906779293223 ) ) ;
#59179 = CARTESIAN_POINT ( 'NONE',  ( 71.08938320489261287, -38.32842224238075346, 140.5796315854678653 ) ) ;
#59180 = CARTESIAN_POINT ( 'NONE',  ( 5.819846122303830249, 6.321060697775074289, -2.051601713726794785 ) ) ;
#59181 = CARTESIAN_POINT ( 'NONE',  ( 32.84946521457204227, 300.3690703675980558, 3.178420029388444146 ) ) ;
#59182 = CARTESIAN_POINT ( 'NONE',  ( -4.497431761510337189, 249.4590187574896731, -3.972160586670089089 ) ) ;
#59183 = AXIS2_PLACEMENT_3D ( 'NONE', #10616, #58105, #74811 ) ;
#59184 = EDGE_LOOP ( 'NONE', ( #11894, #5055, #44107, #53128 ) ) ;
#59185 = DIRECTION ( 'NONE',  ( 0.000000000000000000, 0.000000000000000000, 1.000000000000000000 ) ) ;
#59186 = CARTESIAN_POINT ( 'NONE',  ( 7.592810154713590230E-15, 48.50000000000000000, -62.00000000000000000 ) ) ;
#59187 = AXIS2_PLACEMENT_3D ( 'NONE', #21266, #103212, #11518 ) ;
#59188 = CARTESIAN_POINT ( 'NONE',  ( 0.000000000000000000, 48.50000000000000000, 66.00000000000000000 ) ) ;
#59189 = COLOUR_RGB ( '', 0.09019608, 0.27058824, 0.51372549) ;
#59190 = CARTESIAN_POINT ( 'NONE',  ( -1.469576158976823947E-15, -20.37499999999999289, 8.000000000000000000 ) ) ;
#59192 = ORIENTED_EDGE ( 'NONE', *, *, #84078, .T. ) ;
#59191 = CIRCLE ( 'NONE', #67805, 5.000000000000002665 ) ;
#59193 = LINE ( 'NONE', #41925, #2989 ) ;
#59194 = CARTESIAN_POINT ( 'NONE',  ( 8.240390551120709617, 54.07589417944840449, -1.561599642362494489 ) ) ;
#59195 = UNCERTAINTY_MEASURE_WITH_UNIT (LENGTH_MEASURE( 1.000000000000000082E-05 ), #105425, 'distance_accuracy_value', 'NONE');
#59196 =( NAMED_UNIT ( * ) PLANE_ANGLE_UNIT ( ) SI_UNIT ( $, .RADIAN. ) );
#59197 = CARTESIAN_POINT ( 'NONE',  ( 36.84999999999999432, 1.533819458162526451E-15, 0.000000000000000000 ) ) ;
#59198 = AXIS2_PLACEMENT_3D ( 'NONE', #34544, #83060, #1036 ) ;
#59199 = DIRECTION ( 'NONE',  ( 0.000000000000000000, 0.000000000000000000, 1.000000000000000000 ) ) ;
#59200 = CYLINDRICAL_SURFACE ( 'NONE', #73631, 4.000000000000000000 ) ;
#59201 = CARTESIAN_POINT ( 'NONE',  ( -3.400000000000000355, 4.163799117101001052E-16, -0.4455245229258316120 ) ) ;
#59202 = CARTESIAN_POINT ( 'NONE',  ( 85.50848406000137913, -39.28767163080398461, 185.4887185101361524 ) ) ;
#59203 = CARTESIAN_POINT ( 'NONE',  ( 1.400881274228121143, 15.45483377860037955, -9.907626560209529032 ) ) ;
#59204 = CARTESIAN_POINT ( 'NONE',  ( -3.310848799520615504, 32.66010184960634888, 5.000000000000000000 ) ) ;
#59205 = ORIENTED_EDGE ( 'NONE', *, *, #88501, .F. ) ;
#59206 = CARTESIAN_POINT ( 'NONE',  ( 91.44632344411692770, -57.66251709069995002, -20.24473181102453623 ) ) ;
#59207 = DIRECTION ( 'NONE',  ( 0.000000000000000000, 0.000000000000000000, 1.000000000000000000 ) ) ;
#59208 = CARTESIAN_POINT ( 'NONE',  ( -2.141486166123598434, 6.269165884987821791, -0.07763482564820649301 ) ) ;
#59209 = CARTESIAN_POINT ( 'NONE',  ( 0.000000000000000000, 0.000000000000000000, 4.000000000000000000 ) ) ;
#59210 = CARTESIAN_POINT ( 'NONE',  ( -83.12949059038693633, -29.99999999999998934, 43.93815505698431423 ) ) ;
#59211 = EDGE_CURVE ( 'NONE', #91113, #104064, #34457, .T. ) ;
#59212 = ADVANCED_FACE ( 'NONE', ( #68929 ), #51331, .T. ) ;
#59213 = CARTESIAN_POINT ( 'NONE',  ( 22.88839214066227967, 27.45938914059933467, -33.17277703389370203 ) ) ;
#59214 = DIRECTION ( 'NONE',  ( 0.000000000000000000, -1.000000000000000000, 0.000000000000000000 ) ) ;
#59215 = CARTESIAN_POINT ( 'NONE',  ( -9.537909130738299268, 247.3538516903660138, -3.010726932293848801 ) ) ;
#59216 = EDGE_CURVE ( 'NONE', #288, #36397, #4841, .T. ) ;
#59217 = CARTESIAN_POINT ( 'NONE',  ( -29.59231420605931717, 13.59660068169549696, 42.10535821593509098 ) ) ;
#59218 = B_SPLINE_CURVE_WITH_KNOTS ( 'NONE', 3,
 ( #12900, #79244, #272, #87355, #15434, #97949 ),
 .UNSPECIFIED., .F., .F.,
 ( 4, 2, 4 ),
 ( 2.380733003139562229E-07, 0.001898835937927373114, 0.003797433802554431997 ),
 .UNSPECIFIED. ) ;
#59219 = DIRECTION ( 'NONE',  ( 0.000000000000000000, -1.000000000000000000, 0.000000000000000000 ) ) ;
#59220 = CARTESIAN_POINT ( 'NONE',  ( 5.728413875956868573, -81.41935773546600785, 1.802282772585248605 ) ) ;
#59221 = DIRECTION ( 'NONE',  ( 0.000000000000000000, -1.000000000000000000, 0.000000000000000000 ) ) ;
#59222 = CARTESIAN_POINT ( 'NONE',  ( -5.000000000000000888, 0.000000000000000000, 5.000000000000000000 ) ) ;
#59223 = EDGE_CURVE ( 'NONE', #36789, #88651, #23805, .T. ) ;
#59224 = AXIS2_PLACEMENT_3D ( 'NONE', #51908, #2281, #84821 ) ;
#59225 = CARTESIAN_POINT ( 'NONE',  ( 58.40792008327016305, -29.03551547989282966, -25.51115080894792442 ) ) ;
#59226 = AXIS2_PLACEMENT_3D ( 'NONE', #73263, #24238, #90001 ) ;
#59227 = CARTESIAN_POINT ( 'NONE',  ( -24.27889609124726533, -22.08348835334177096, 28.63685605476302953 ) ) ;
#59228 = ADVANCED_FACE ( 'NONE', ( #58703 ), #65129, .T. ) ;
#59229 = ORIENTED_EDGE ( 'NONE', *, *, #96370, .T. ) ;
#59230 = CARTESIAN_POINT ( 'NONE',  ( 6.084941413214105310, 10.98348070165863888, 3.464128533964752510 ) ) ;
#59231 = DIRECTION ( 'NONE',  ( 0.000000000000000000, 0.000000000000000000, 1.000000000000000000 ) ) ;
#59232 = CARTESIAN_POINT ( 'NONE',  ( -7.801642220026313801, 81.41203173850969677, 1.787233835843583307 ) ) ;
#59233 = CARTESIAN_POINT ( 'NONE',  ( -47.35410119362553161, -26.87184004367228951, -28.63942663572363045 ) ) ;
#59235 = DIRECTION ( 'NONE',  ( 0.000000000000000000, 0.000000000000000000, 1.000000000000000000 ) ) ;
#59234 =( NAMED_UNIT ( * ) PLANE_ANGLE_UNIT ( ) SI_UNIT ( $, .RADIAN. ) );
#59236 = ORIENTED_EDGE ( 'NONE', *, *, #104553, .T. ) ;
#59237 = CYLINDRICAL_SURFACE ( 'NONE', #13373, 60.00000000000000000 ) ;
#59238 = VERTEX_POINT ( 'NONE', #35513 ) ;
#59239 = CARTESIAN_POINT ( 'NONE',  ( 0.000000000000000000, -30.00000000000000000, 0.000000000000000000 ) ) ;
#59240 = CARTESIAN_POINT ( 'NONE',  ( 15.93262767509089350, 3.183098147203142769, 1.443311391229760376 ) ) ;
#59241 = CARTESIAN_POINT ( 'NONE',  ( -90.37139598638705706, -60.00000000000000711, -18.17949969827632017 ) ) ;
#59242 = ORIENTED_EDGE ( 'NONE', *, *, #103147, .F. ) ;
#59243 = FACE_OUTER_BOUND ( 'NONE', #29801, .T. ) ;
#59244 = CARTESIAN_POINT ( 'NONE',  ( -1.140137277112188485, 294.8483051625062217, -9.950919916537934284 ) ) ;
#59245 = CARTESIAN_POINT ( 'NONE',  ( 101.7209338708262862, -60.22223593363352023, 194.4975265031006586 ) ) ;
#59247 = CARTESIAN_POINT ( 'NONE',  ( -4.147911490760923137, -1.050630162886936780, 104.5115833471886191 ) ) ;
#59246 = CARTESIAN_POINT ( 'NONE',  ( 10.28624191512063746, 46.12099395432516502, -12.90779740155508826 ) ) ;
#59248 = EDGE_LOOP ( 'NONE', ( #94670, #91821, #42312, #76240 ) ) ;
#59249 = VECTOR ( 'NONE', #33205, 1000.000000000000000 ) ;
#59250 = EDGE_LOOP ( 'NONE', ( #28887, #67511, #79948, #42795, #57526, #14404 ) ) ;
#59251 = ORIENTED_EDGE ( 'NONE', *, *, #12565, .F. ) ;
#59252 = CARTESIAN_POINT ( 'NONE',  ( 30.38819389726869602, 339.6136208926041604, 18.22926607251833531 ) ) ;
#59253 = AXIS2_PLACEMENT_3D ( 'NONE', #98552, #82378, #57551 ) ;
#59254 = CARTESIAN_POINT ( 'NONE',  ( 35.58361799548379167, 6.123233995736772199E-16, -5.000000000000001776 ) ) ;
#59255 = CARTESIAN_POINT ( 'NONE',  ( 8.559508646656407649, 53.96349637827586321, 1.531152949374444239 ) ) ;
#59256 = ORIENTED_EDGE ( 'NONE', *, *, #80996, .T. ) ;
#59257 = EDGE_CURVE ( 'NONE', #85895, #6296, #9588, .T. ) ;
#59258 = CARTESIAN_POINT ( 'NONE',  ( -4.336808689942017736E-16, 0.6351314446054990848, -6.500000000000000000 ) ) ;
#59259 = CARTESIAN_POINT ( 'NONE',  ( 23.21751746555220564, -1.200000000000000030E-05, -31.95617127781077116 ) ) ;
#59260 = CIRCLE ( 'NONE', #45493, 2.000000000000000000 ) ;
#59261 = CARTESIAN_POINT ( 'NONE',  ( 0.000000000000000000, 0.000000000000000000, 5.000000000000000888 ) ) ;
#59262 = CARTESIAN_POINT ( 'NONE',  ( -28.75444143438830835, -57.68095489456369762, 44.62365432283354494 ) ) ;
#59263 = CARTESIAN_POINT ( 'NONE',  ( -30.93388328643640151, 14.00942575955928682, 40.91282515498028260 ) ) ;
#59264 = CARTESIAN_POINT ( 'NONE',  ( -22.91885868373643831, 305.6172567281201964, 10.10309701371861912 ) ) ;
#59265 = CARTESIAN_POINT ( 'NONE',  ( 47.33349330513379982, 1.593028355512270567E-15, 0.000000000000000000 ) ) ;
#59266 = CARTESIAN_POINT ( 'NONE',  ( -89.53165980454747341, -30.00000000000000000, -13.19740150267569767 ) ) ;
#59267 = EDGE_CURVE ( 'NONE', #3901, #54377, #78820, .T. ) ;
#59269 = ADVANCED_FACE ( 'NONE', ( #42501 ), #59237, .F. ) ;
#59268 = FILL_AREA_STYLE ('',( #91633 ) ) ;
#59270 = CARTESIAN_POINT ( 'NONE',  ( -49.21489589265689801, -60.29422131675831764, 56.32659531772773676 ) ) ;
#59271 = CARTESIAN_POINT ( 'NONE',  ( -39.08667504521158520, 48.00000000000000000, -56.76470588235294912 ) ) ;
#59272 = ORIENTED_EDGE ( 'NONE', *, *, #39352, .T. ) ;
#59273 = CARTESIAN_POINT ( 'NONE',  ( 12.50000000000000355, 11.21173235486268105, -29.16573252495493307 ) ) ;
#59274 = CARTESIAN_POINT ( 'NONE',  ( 15.17407431220850533, 1.340359594676612611E-15, 0.000000000000000000 ) ) ;
#59275 = CARTESIAN_POINT ( 'NONE',  ( 11.22451676794676168, -1.339060030482434271, 20.46088173027341028 ) ) ;
#59276 = EDGE_LOOP ( 'NONE', ( #8192, #79230 ) ) ;
#59277 = CARTESIAN_POINT ( 'NONE',  ( 5.646888413699860720, 246.5502584402960053, 2.040714635159918799 ) ) ;
#59278 = CARTESIAN_POINT ( 'NONE',  ( 92.16345255951654281, -38.49867825655345399, 201.0232676182550620 ) ) ;
#59279 = DIRECTION ( 'NONE',  ( -1.000000000000000000, -1.224606353822377258E-16, -0.000000000000000000 ) ) ;
#59280 = DIRECTION ( 'NONE',  ( 0.000000000000000000, -1.000000000000000000, 0.000000000000000000 ) ) ;
#59281 = CARTESIAN_POINT ( 'NONE',  ( -17.49999999999997513, 46.00000000000000000, 64.09953197959339377 ) ) ;
#59282 = CARTESIAN_POINT ( 'NONE',  ( 94.15963719096482976, -29.99999999999999289, 191.2924193907763311 ) ) ;
#59283 = FACE_OUTER_BOUND ( 'NONE', #51247, .T. ) ;
#59284 = CARTESIAN_POINT ( 'NONE',  ( 3.337161262018383995E-15, 37.21016666119768246, 27.25000000000000000 ) ) ;
#59285 = EDGE_CURVE ( 'NONE', #696, #98784, #28996, .T. ) ;
#59286 = AXIS2_PLACEMENT_3D ( 'NONE', #1134, #17373, #57258 ) ;
#59287 = B_SPLINE_CURVE_WITH_KNOTS ( 'NONE', 3,
 ( #9255, #99322, #25496, #34119, #100933, #83678, #27092, #17914, #35170, #33047, #41641, #83159 ),
 .UNSPECIFIED., .F., .F.,
 ( 4, 2, 2, 2, 2, 4 ),
 ( 9.220181747203676555E-18, 0.002064083228126805183, 0.003096124842190242903, 0.004128166456253680623, 0.006192249684380478868, 0.008256332912507276245 ),
 .UNSPECIFIED. ) ;
#59288 = ORIENTED_EDGE ( 'NONE', *, *, #91739, .F. ) ;
#59289 = ORIENTED_EDGE ( 'NONE', *, *, #80046, .T. ) ;
#59290 = CARTESIAN_POINT ( 'NONE',  ( 52.19444971213442841, -29.11002465084732549, 50.88288585126180408 ) ) ;
#59291 = DIRECTION ( 'NONE',  ( -1.000000000000000000, 0.000000000000000000, 0.000000000000000000 ) ) ;
#59292 = DIRECTION ( 'NONE',  ( 0.000000000000000000, -1.000000000000000000, 0.000000000000000000 ) ) ;
#59293 = ADVANCED_FACE ( 'NONE', ( #93188 ), #15209, .T. ) ;
#59294 = ORIENTED_EDGE ( 'NONE', *, *, #11970, .T. ) ;
#59295 = CARTESIAN_POINT ( 'NONE',  ( -89.24754036418538305, -38.38798525287715080, -17.62771086576031365 ) ) ;
#59296 = VERTEX_POINT ( 'NONE', #37650 ) ;
#59297 = CARTESIAN_POINT ( 'NONE',  ( 39.83349330513380693, 1.593028355512270567E-15, 0.000000000000000000 ) ) ;
#59298 = CARTESIAN_POINT ( 'NONE',  ( 110.2493868441466844, -38.35601182983472768, 184.3356547549451818 ) ) ;
#59299 = CARTESIAN_POINT ( 'NONE',  ( 13.59349846140866447, 24.77249653569413823, 0.2813197656736000085 ) ) ;
#59300 = CARTESIAN_POINT ( 'NONE',  ( 83.98334445332307041, -37.85010976468362287, 36.91978127714231306 ) ) ;
#59301 = CARTESIAN_POINT ( 'NONE',  ( 1.778928937981565150, -4.332661967054583840, -18.07496135556122141 ) ) ;
#59302 = CARTESIAN_POINT ( 'NONE',  ( -23.81822736121795003, 305.6269812178131247, -9.833007305667777587 ) ) ;
#59303 =( GEOMETRIC_REPRESENTATION_CONTEXT ( 3 ) GLOBAL_UNCERTAINTY_ASSIGNED_CONTEXT ( ( #15695 ) ) GLOBAL_UNIT_ASSIGNED_CONTEXT ( ( #8663, #74453, #105248 ) ) REPRESENTATION_CONTEXT ( 'NONE', 'WORKASPACE' ) );
#59304 = CARTESIAN_POINT ( 'NONE',  ( 5.000000000000000888, -14.05766640829038394, -5.232782735144291486 ) ) ;
#59305 = EDGE_CURVE ( 'NONE', #94819, #57770, #33972, .T. ) ;
#59306 = CARTESIAN_POINT ( 'NONE',  ( -23.21751746555235840, 25.25267828308461304, -33.20617127781177658 ) ) ;
#59307 = LINE ( 'NONE', #84102, #52641 ) ;
#59308 = VERTEX_POINT ( 'NONE', #37113 ) ;
#59309 = CARTESIAN_POINT ( 'NONE',  ( 60.10615156299768103, -46.43600144855555811, 75.82275319019012727 ) ) ;
#59310 = CARTESIAN_POINT ( 'NONE',  ( 0.1696663817233923233, 37.20684969797608943, 27.25870950959922467 ) ) ;
#59311 = CARTESIAN_POINT ( 'NONE',  ( 40.92692307692308162, 1.411358822780289120E-15, 0.000000000000000000 ) ) ;
#59312 = ORIENTED_EDGE ( 'NONE', *, *, #77865, .F. ) ;
#59313 = LINE ( 'NONE', #34000, #66527 ) ;
#59314 = CARTESIAN_POINT ( 'NONE',  ( -42.08109764087019755, 343.1592929535903522, 13.36121580716647372 ) ) ;
#59315 = FACE_OUTER_BOUND ( 'NONE', #62547, .T. ) ;
#59316 = CARTESIAN_POINT ( 'NONE',  ( 17.81438722625302518, 1.482358050883964840E-15, 0.000000000000000000 ) ) ;
#59317 = CARTESIAN_POINT ( 'NONE',  ( 3.313708498984762496, -24.78124999999999289, 7.999999999999998224 ) ) ;
#59318 = CARTESIAN_POINT ( 'NONE',  ( -46.01638873010887920, -28.64614323415289121, 41.14871410708547472 ) ) ;
#59319 = DIRECTION ( 'NONE',  ( 0.000000000000000000, 0.000000000000000000, 1.000000000000000000 ) ) ;
#59320 = VERTEX_POINT ( 'NONE', #79647 ) ;
#59321 = CARTESIAN_POINT ( 'NONE',  ( 85.08258324672883077, -32.28520541998505422, 178.2135383856105761 ) ) ;
#59322 = FACE_OUTER_BOUND ( 'NONE', #35921, .T. ) ;
#59323 = CARTESIAN_POINT ( 'NONE',  ( -40.30332470629049624, 437.2182582767285908, 22.21307012533235792 ) ) ;
#59324 = ORIENTED_EDGE ( 'NONE', *, *, #53722, .F. ) ;
#59325 = CARTESIAN_POINT ( 'NONE',  ( -39.56197461363974810, -0.1944580884125578779, -19.78098730681986339 ) ) ;
#59326 = CONICAL_SURFACE ( 'NONE', #97180, 4.000000000000007105, 0.9599310885968835860 ) ;
#59327 = CARTESIAN_POINT ( 'NONE',  ( -7.500000000000000000, -4.330127018922203419, -0.9999999999999974465 ) ) ;
#59328 = FILL_AREA_STYLE ('',( #1589 ) ) ;
#59329 =( NAMED_UNIT ( * ) PLANE_ANGLE_UNIT ( ) SI_UNIT ( $, .RADIAN. ) );
#59330 = CARTESIAN_POINT ( 'NONE',  ( -14.33052326666859777, -3.000000000000003109, -89.63170281047537458 ) ) ;
#59331 = CARTESIAN_POINT ( 'NONE',  ( -19.47912966778427446, -25.64570046021258776, -38.49086459474126087 ) ) ;
#59332 =( BOUNDED_SURFACE ( )  B_SPLINE_SURFACE ( 3, 2, ( 
 ( #48069, #31925, #89085 ),
 ( #98739, #32465, #80969 ),
 ( #40525, #31409, #90140 ),
 ( #7088, #57749, #40001 ) ),
 .UNSPECIFIED., .F., .F., .F. ) 
 B_SPLINE_SURFACE_WITH_KNOTS ( ( 4, 4 ),
 ( 3, 3 ),
 ( -4.996003610813204432E-16, 0.003677210556160862790 ),
 ( 0.000000000000000000, 1.000000000000000000 ),
 .UNSPECIFIED. ) 
 GEOMETRIC_REPRESENTATION_ITEM ( )  RATIONAL_B_SPLINE_SURFACE ( (
 ( 1.000000000000000000, 0.7874655377939757672, 1.000000000000000000),
 ( 1.000000000000000000, 0.7709584336437098617, 1.000000000000000000),
 ( 1.000000000000000000, 0.7542748649868799005, 1.000000000000000000),
 ( 1.000000000000000000, 0.7370557512815874013, 1.000000000000000000) ) ) 
 REPRESENTATION_ITEM ( '' )  SURFACE ( )  );
#59333 = CIRCLE ( 'NONE', #761, 10.00000000000000533 ) ;
#59334 = EDGE_CURVE ( 'NONE', #65995, #51662, #22516, .T. ) ;
#59335 = PRODUCT_DEFINITION_FORMATION_WITH_SPECIFIED_SOURCE ( 'ANY', '', #28705, .NOT_KNOWN. ) ;
#59336 = AXIS2_PLACEMENT_3D ( 'NONE', #72178, #88375, #31739 ) ;
#59337 = ADVANCED_FACE ( 'NONE', ( #13842 ), #48281, .F. ) ;
#59338 = CARTESIAN_POINT ( 'NONE',  ( 44.20361967343200149, -60.00000000000000000, 59.06671950064491483 ) ) ;
#59339 = CARTESIAN_POINT ( 'NONE',  ( 7.897196874019792645, 108.7912720416780559, -1.302055520192085369 ) ) ;
#59340 = CARTESIAN_POINT ( 'NONE',  ( 7.438636493593315357, -13.23942326510881173, 32.01358503952575774 ) ) ;
#59341 = EDGE_CURVE ( 'NONE', #93999, #40311, #7633, .T. ) ;
#59343 = CARTESIAN_POINT ( 'NONE',  ( -15.58067260655142761, 23.00073928917876032, 0.5609666062011725574 ) ) ;
#59342 = CARTESIAN_POINT ( 'NONE',  ( -27.76376690927586566, -30.93432701297266973, 39.41148924507555051 ) ) ;
#59344 = EDGE_CURVE ( 'NONE', #6924, #79431, #13216, .T. ) ;
#59345 = CARTESIAN_POINT ( 'NONE',  ( 4.250000000000000000, 0.000000000000000000, -4.814498510800145681 ) ) ;
#59346 = CARTESIAN_POINT ( 'NONE',  ( 25.93947128054312756, 296.0094280503604978, 10.18659011856751384 ) ) ;
#59347 = CYLINDRICAL_SURFACE ( 'NONE', #100803, 8.000000000000000000 ) ;
#59348 = EDGE_CURVE ( 'NONE', #35464, #67362, #35673, .T. ) ;
#59349 = CARTESIAN_POINT ( 'NONE',  ( -1.000000000000002442, 0.000000000000000000, 27.00000000000000000 ) ) ;
#59350 = B_SPLINE_CURVE_WITH_KNOTS ( 'NONE', 3,
 ( #72530, #106479, #7255, #81660, #41225, #55273, #32637, #30513, #65509, #56324, #98397, #88726, #90310, #16418, #49298, #73039, #82205, #8321, #63411, #89259 ),
 .UNSPECIFIED., .F., .F.,
 ( 4, 2, 2, 2, 2, 2, 2, 2, 2, 4 ),
 ( 0.003141903260821411921, 0.003645771108259603446, 0.004149638955697794972, 0.004653506803135986497, 0.005157374650574178890, 0.005661242498012371283, 0.006165110345450562808, 0.006668978192888754333, 0.006920912116607849662, 0.007172846040326944991 ),
 .UNSPECIFIED. ) ;
#59351 = EDGE_CURVE ( 'NONE', #54223, #87110, #17591, .T. ) ;
#59352 = ORIENTED_EDGE ( 'NONE', *, *, #29778, .T. ) ;
#59353 = CARTESIAN_POINT ( 'NONE',  ( -17.24303157407923237, 294.5700599009814482, 9.877113118490870036 ) ) ;
#59354 = CARTESIAN_POINT ( 'NONE',  ( 31.14131030317610538, 1.482358050883964840E-15, 0.000000000000000000 ) ) ;
#59355 = UNCERTAINTY_MEASURE_WITH_UNIT (LENGTH_MEASURE( 1.000000000000000082E-05 ), #38317, 'distance_accuracy_value', 'NONE');
#59356 = EDGE_CURVE ( 'NONE', #64041, #54339, #2902, .T. ) ;
#59357 = CARTESIAN_POINT ( 'NONE',  ( -12.37144696128342147, -4.000000000000002665, 20.44658103856077602 ) ) ;
#59358 = CARTESIAN_POINT ( 'NONE',  ( -41.58466061806753800, 465.5764877067418865, 15.80465680671442819 ) ) ;
#59360 = CARTESIAN_POINT ( 'NONE',  ( 31.16062950921062225, -21.77023875782602857, -28.58741295160539053 ) ) ;
#59359 = DIRECTION ( 'NONE',  ( -0.5735764363510510444, -0.8191520442889883569, 0.000000000000000000 ) ) ;
#59361 = AXIS2_PLACEMENT_3D ( 'NONE', #29096, #38222, #63546 ) ;
#59362 = VERTEX_POINT ( 'NONE', #27843 ) ;
#59363 = CARTESIAN_POINT ( 'NONE',  ( 27.85375964729074383, 36.60111159598967134, 7.793250597500285259 ) ) ;
#59364 = CARTESIAN_POINT ( 'NONE',  ( 0.000000000000000000, -1.200583151104947843, 120.8571428571428612 ) ) ;
#59365 = ORIENTED_EDGE ( 'NONE', *, *, #17824, .T. ) ;
#59366 = LINE ( 'NONE', #42628, #83376 ) ;
#59367 = DIRECTION ( 'NONE',  ( -1.000000000000000000, -1.224606353822377258E-16, -0.000000000000000000 ) ) ;
#59368 = DIRECTION ( 'NONE',  ( 0.000000000000000000, -1.000000000000000000, 0.000000000000000000 ) ) ;
#59369 = CIRCLE ( 'NONE', #50698, 4.000000000000001776 ) ;
#59370 = CARTESIAN_POINT ( 'NONE',  ( -102.2988307860546655, -60.00000000000000711, 94.48776800051813041 ) ) ;
#59371 = CIRCLE ( 'NONE', #9370, 15.00000000000001421 ) ;
#59372 = CARTESIAN_POINT ( 'NONE',  ( -16.85961028550735463, 304.5626392334940533, -9.061460871365316194 ) ) ;
#59373 = CARTESIAN_POINT ( 'NONE',  ( 35.57955382936916067, 363.3973965622570859, 2.919629247011395368 ) ) ;
#59374 = CARTESIAN_POINT ( 'NONE',  ( 40.21064024339792553, 459.8708642436264995, 1.907892319915238888 ) ) ;
#59375 = COLOUR_RGB ( '', 0.09019608, 0.27058824, 0.51372549) ;
#59377 = DIRECTION ( 'NONE',  ( -0.000000000000000000, -0.000000000000000000, -1.000000000000000000 ) ) ;
#59376 = FACE_OUTER_BOUND ( 'NONE', #10127, .T. ) ;
#59378 = CARTESIAN_POINT ( 'NONE',  ( -85.20515625194583720, -25.43333465146562489, 169.0116749862556276 ) ) ;
#59379 = ORIENTED_EDGE ( 'NONE', *, *, #42280, .T. ) ;
#59380 = AXIS2_PLACEMENT_3D ( 'NONE', #104764, #22820, #89121 ) ;
#59381 = CYLINDRICAL_SURFACE ( 'NONE', #100473, 4.000000000000001776 ) ;
#59382 = ORIENTED_EDGE ( 'NONE', *, *, #91938, .T. ) ;
#59383 = VECTOR ( 'NONE', #83830, 1000.000000000000000 ) ;
#59384 = ORIENTED_EDGE ( 'NONE', *, *, #90120, .F. ) ;
#59385 = CARTESIAN_POINT ( 'NONE',  ( -11.89098014788630664, 303.5914335720564168, -10.05534211649429643 ) ) ;
#59386 = DIRECTION ( 'NONE',  ( -1.000000000000000000, -1.224606353822377258E-16, -0.000000000000000000 ) ) ;
#59387 = EDGE_LOOP ( 'NONE', ( #68045, #30183, #72005, #39726 ) ) ;
#59388 = CARTESIAN_POINT ( 'NONE',  ( 31.99156825197944798, 486.4558694464275277, 6.110232253381057355 ) ) ;
#59389 = FACE_OUTER_BOUND ( 'NONE', #73988, .T. ) ;
#59390 = DIRECTION ( 'NONE',  ( -1.000000000000000000, -1.224606353822377258E-16, -0.000000000000000000 ) ) ;
#59391 = CARTESIAN_POINT ( 'NONE',  ( -32.99999999999993605, 464.4386723251832905, 6.308603495333271916 ) ) ;
#59392 = CARTESIAN_POINT ( 'NONE',  ( 43.20037042670922744, 463.4262835534589158, 5.016616955632313690 ) ) ;
#59393 = CARTESIAN_POINT ( 'NONE',  ( -13.42014116845449934, -52.95667802455457718, 30.98782490008220236 ) ) ;
#59394 = CARTESIAN_POINT ( 'NONE',  ( -4.999999999999999112, -15.43654613828065969, 12.61250543006183378 ) ) ;
#59395 = CARTESIAN_POINT ( 'NONE',  ( 94.21214616282756538, -60.00000000000006395, 9.573485886066015027 ) ) ;
#59396 = EDGE_CURVE ( 'NONE', #43850, #24510, #53195, .T. ) ;
#59397 = CARTESIAN_POINT ( 'NONE',  ( -86.50885295532998498, -60.00000000000009237, 203.5147570966663011 ) ) ;
#59398 = CARTESIAN_POINT ( 'NONE',  ( -58.31099076156637295, -22.13342643865365744, 60.29576011847133543 ) ) ;
#59399 = ORIENTED_EDGE ( 'NONE', *, *, #18875, .T. ) ;
#59400 = CARTESIAN_POINT ( 'NONE',  ( 6.705020855549795655, 16.46018158102737061, 2.023228926981749165 ) ) ;
#59401 = CARTESIAN_POINT ( 'NONE',  ( 92.92862678600012316, -59.99999999999997868, -18.42878329021216643 ) ) ;
#59402 = ORIENTED_EDGE ( 'NONE', *, *, #49103, .T. ) ;
#59403 = CARTESIAN_POINT ( 'NONE',  ( 2.969152809838174978, -18.58611397292780154, 26.98299902465180367 ) ) ;
#59404 = CARTESIAN_POINT ( 'NONE',  ( -104.1964872485443436, -52.71017148545060849, 185.8560034257230598 ) ) ;
#59405 = CYLINDRICAL_SURFACE ( 'NONE', #71274, 4.000000000000000000 ) ;
#59406 = CARTESIAN_POINT ( 'NONE',  ( 14.83349330513380337, 4.898587196589405926E-16, -4.000000000000001776 ) ) ;
#59407 = ORIENTED_EDGE ( 'NONE', *, *, #11871, .F. ) ;
#59408 = CARTESIAN_POINT ( 'NONE',  ( 6.256238905933717120, -3.000000000000470290, -71.20382035666703757 ) ) ;
#59409 = CARTESIAN_POINT ( 'NONE',  ( -44.21061720778400428, -60.00000000000001421, 59.05736679842440395 ) ) ;
#59410 = CARTESIAN_POINT ( 'NONE',  ( 36.80450393364946393, 25.99766569896315715, -11.20157930558040249 ) ) ;
#59411 = CARTESIAN_POINT ( 'NONE',  ( -7.188101187500000044, -23.28125000204838457, -8.802885111219163269E-16 ) ) ;
#59412 = CARTESIAN_POINT ( 'NONE',  ( -1.249548360227116905, 36.80417223094376311, -28.33792551024971118 ) ) ;
#59413 = DIRECTION ( 'NONE',  ( -0.5735764363510461594, 0.8191520442889916875, 1.003171929053524870E-16 ) ) ;
#59414 = CIRCLE ( 'NONE', #4276, 4.000000000000000888 ) ;
#59415 = CARTESIAN_POINT ( 'NONE',  ( 14.76977913855438906, -0.000000000000000000, 8.521464936429580916 ) ) ;
#59416 = CARTESIAN_POINT ( 'NONE',  ( -22.42417502586373246, 305.3961751430792333, 10.05444931189341773 ) ) ;
#59417 = PRESENTATION_STYLE_ASSIGNMENT (( #3291 ) ) ;
#59418 = FACE_OUTER_BOUND ( 'NONE', #38702, .T. ) ;
#59419 = CARTESIAN_POINT ( 'NONE',  ( 37.52579488121515539, 438.0832148649091096, 4.091984033318603053 ) ) ;
#59420 = PRODUCT_DEFINITION_FORMATION_WITH_SPECIFIED_SOURCE ( 'ANY', '', #69145, .NOT_KNOWN. ) ;
#59421 = CARTESIAN_POINT ( 'NONE',  ( -30.49126993251524098, -29.07187388107037407, 31.42370632120385920 ) ) ;
#59422 = PRESENTATION_STYLE_ASSIGNMENT (( #93378 ) ) ;
#59423 = CARTESIAN_POINT ( 'NONE',  ( 45.04133914164980013, -60.25292661424882823, 49.29860799678134953 ) ) ;
#59424 = CARTESIAN_POINT ( 'NONE',  ( -32.11826742301046522, 487.8588087913806817, 8.620620385259270435 ) ) ;
#59425 = ORIENTED_EDGE ( 'NONE', *, *, #73750, .T. ) ;
#59426 = CARTESIAN_POINT ( 'NONE',  ( -1.218812433689057118, 45.85957784483471045, 17.18021691162306652 ) ) ;
#59427 = EDGE_CURVE ( 'NONE', #99841, #23394, #59642, .T. ) ;
#59428 = CARTESIAN_POINT ( 'NONE',  ( -78.45624996374505145, -38.62884931123382870, 189.5593364397898313 ) ) ;
#59429 = VERTEX_POINT ( 'NONE', #82837 ) ;
#59431 = DIRECTION ( 'NONE',  ( 0.000000000000000000, 0.000000000000000000, -1.000000000000000000 ) ) ;
#59430 = CARTESIAN_POINT ( 'NONE',  ( 7.960204194457797252E-15, 50.50000000000000000, -65.00000000000000000 ) ) ;
#59432 = CARTESIAN_POINT ( 'NONE',  ( 26.97198470160383721, -60.00000000000000711, 35.68917358449845523 ) ) ;
#59433 = CARTESIAN_POINT ( 'NONE',  ( 0.000000000000000000, 0.000000000000000000, -6.275264681066861527 ) ) ;
#59434 = CARTESIAN_POINT ( 'NONE',  ( -7.320805857562880270, 41.41776710089564517, -59.82972164228972645 ) ) ;
#59435 = DIRECTION ( 'NONE',  ( 0.000000000000000000, 1.000000000000000000, 0.000000000000000000 ) ) ;
#59436 = CARTESIAN_POINT ( 'NONE',  ( 4.235164736271502188E-16, 0.6351314446025461136, -6.500000000000000000 ) ) ;
#59437 = CARTESIAN_POINT ( 'NONE',  ( 0.000000000000000000, 0.000000000000000000, 5.000000000000000888 ) ) ;
#59438 = CARTESIAN_POINT ( 'NONE',  ( 88.20199406385988539, 1.030564683017419500E-14, 0.000000000000000000 ) ) ;
#59439 = EDGE_CURVE ( 'NONE', #52182, #30449, #8938, .T. ) ;
#59440 = CARTESIAN_POINT ( 'NONE',  ( 110.0424928893739747, -59.99999999999999289, 143.7894636553020007 ) ) ;
#59441 = CARTESIAN_POINT ( 'NONE',  ( 1.104211576045294407, 14.95094041744785862, -0.8377008405913628497 ) ) ;
#59442 = CARTESIAN_POINT ( 'NONE',  ( -33.74742351813127073, 478.7265835501554534, 3.791636934804474279 ) ) ;
#59443 = VERTEX_POINT ( 'NONE', #77942 ) ;
#59444 = CARTESIAN_POINT ( 'NONE',  ( 3.301573598373775287, -49.28812056075076953, 103.9445864789744149 ) ) ;
#59445 = COLOUR_RGB ( '', 0.72549020, 0.75294118, 0.79215686) ;
#59446 = CARTESIAN_POINT ( 'NONE',  ( -72.66216753198708034, -30.00000000000000711, -19.29909516204710229 ) ) ;
#59447 = ORIENTED_EDGE ( 'NONE', *, *, #1576, .T. ) ;
#59448 = CARTESIAN_POINT ( 'NONE',  ( 26.34344435950205465, 37.12862132004229210, -7.801778736123593738 ) ) ;
#59449 = CARTESIAN_POINT ( 'NONE',  ( 0.000000000000000000, 0.000000000000000000, 5.000000000000002665 ) ) ;
#59450 = SURFACE_STYLE_FILL_AREA ( #2237 ) ;
#59451 = FILL_AREA_STYLE ('',( #67005 ) ) ;
#59452 = CARTESIAN_POINT ( 'NONE',  ( 5.082755093536325930, -20.84375000204838813, -5.082755093536325042 ) ) ;
#59453 = AXIS2_PLACEMENT_3D ( 'NONE', #95779, #86117, #95254 ) ;
#59454 = EDGE_CURVE ( 'NONE', #29601, #49147, #23570, .T. ) ;
#59455 = TOROIDAL_SURFACE ( 'NONE', #88692, 7.500000000000000888, 5.000000000000000000 ) ;
#59456 = CIRCLE ( 'NONE', #93854, 60.00000000000000000 ) ;
#59457 = CARTESIAN_POINT ( 'NONE',  ( 30.36547348172748073, 16.93923362554433965, -39.80091097816919188 ) ) ;
#59458 = CIRCLE ( 'NONE', #12914, 5.000000000000002665 ) ;
#59459 = ORIENTED_EDGE ( 'NONE', *, *, #72817, .F. ) ;
#59460 = CARTESIAN_POINT ( 'NONE',  ( 84.74724864891217635, -18.65598358680870561, 153.2857099555950526 ) ) ;
#59461 = CARTESIAN_POINT ( 'NONE',  ( -44.17094014566056615, 463.2864587933497091, 6.608468562565803950 ) ) ;
#59462 = VECTOR ( 'NONE', #31819, 999.9999999999998863 ) ;
#59463 = DIRECTION ( 'NONE',  ( 1.000000000000000000, 0.000000000000000000, 0.000000000000000000 ) ) ;
#59464 = EDGE_LOOP ( 'NONE', ( #78102, #75330, #59484, #103003 ) ) ;
#59465 = CARTESIAN_POINT ( 'NONE',  ( -11.72692804380855591, 302.5954534377697200, -10.05449581651908453 ) ) ;
#59466 = CARTESIAN_POINT ( 'NONE',  ( 40.34715123528543046, -5.000000000000009770, 0.000000000000000000 ) ) ;
#59467 = DIRECTION ( 'NONE',  ( 0.000000000000000000, 0.000000000000000000, 1.000000000000000000 ) ) ;
#59468 = CARTESIAN_POINT ( 'NONE',  ( 29.99999999999996092, 486.4444101590605101, 4.645498354857360290 ) ) ;
#59469 = AXIS2_PLACEMENT_3D ( 'NONE', #30292, #45930, #62653 ) ;
#59470 = DIRECTION ( 'NONE',  ( 1.000000000000000000, 0.000000000000000000, 0.000000000000000000 ) ) ;
#59471 = CARTESIAN_POINT ( 'NONE',  ( -29.56778029646497075, 314.0584236046759656, 12.66027079984575821 ) ) ;
#59472 = CARTESIAN_POINT ( 'NONE',  ( 16.75187969033515145, -1.200000000000000030E-05, -23.05698433968624528 ) ) ;
#59473 = ORIENTED_EDGE ( 'NONE', *, *, #89865, .T. ) ;
#59474 =( NAMED_UNIT ( * ) PLANE_ANGLE_UNIT ( ) SI_UNIT ( $, .RADIAN. ) );
#59475 = EDGE_CURVE ( 'NONE', #99399, #29309, #37364, .T. ) ;
#59476 = DIRECTION ( 'NONE',  ( 0.000000000000000000, 0.000000000000000000, -1.000000000000000000 ) ) ;
#59477 = DIRECTION ( 'NONE',  ( 0.000000000000000000, 1.000000000000000000, 0.000000000000000000 ) ) ;
#59478 = EDGE_CURVE ( 'NONE', #58193, #27470, #92444, .T. ) ;
#59479 = CARTESIAN_POINT ( 'NONE',  ( 0.000000000000000000, 0.000000000000000000, 0.000000000000000000 ) ) ;
#59480 = CARTESIAN_POINT ( 'NONE',  ( -2.977408999572654480, -25.62500000204838813, 7.188101187499999156 ) ) ;
#59481 = PLANE ( 'NONE',  #49123 ) ;
#59482 = DIRECTION ( 'NONE',  ( -0.000000000000000000, -0.000000000000000000, 1.000000000000000000 ) ) ;
#59483 = CARTESIAN_POINT ( 'NONE',  ( 41.84139522851419457, 436.8002711404864726, 20.35041468290338429 ) ) ;
#59484 = ORIENTED_EDGE ( 'NONE', *, *, #103994, .T. ) ;
#59485 = CARTESIAN_POINT ( 'NONE',  ( 43.00000000000000000, 500.0000000000002274, 0.000000000000000000 ) ) ;
#59486 = EDGE_CURVE ( 'NONE', #96624, #35336, #59747, .T. ) ;
#59487 = FACE_OUTER_BOUND ( 'NONE', #98605, .T. ) ;
#59488 = CARTESIAN_POINT ( 'NONE',  ( -9.993183759060100257, 7.509940706430752400, -5.000000000000000888 ) ) ;
#59489 = ADVANCED_FACE ( 'NONE', ( #62827 ), #21857, .F. ) ;
#59490 =( LENGTH_UNIT ( ) NAMED_UNIT ( * ) SI_UNIT ( .MILLI., .METRE. ) );
#59491 = VERTEX_POINT ( 'NONE', #71419 ) ;
#59492 = CARTESIAN_POINT ( 'NONE',  ( -30.00000000000000355, 462.0139486977119532, 13.78583326881746096 ) ) ;
#59493 = FILL_AREA_STYLE ('',( #1750 ) ) ;
#59494 = CARTESIAN_POINT ( 'NONE',  ( 31.80647371913423171, 437.2005603137831145, 20.73398510949202489 ) ) ;
#59495 = FILL_AREA_STYLE ('',( #44364 ) ) ;
#59496 = FACE_OUTER_BOUND ( 'NONE', #64502, .T. ) ;
#59497 = CARTESIAN_POINT ( 'NONE',  ( 24.63846153846153797, 4.172000000000003261, 5.109226446042759579E-16 ) ) ;
#59498 = CARTESIAN_POINT ( 'NONE',  ( -79.80355888509041051, -60.00000000000000711, 195.7382001822659845 ) ) ;
#59499 = DIRECTION ( 'NONE',  ( -1.000000000000000000, -0.000000000000000000, -0.000000000000000000 ) ) ;
#59500 = DIRECTION ( 'NONE',  ( 0.000000000000000000, 1.000000000000000000, 0.000000000000000000 ) ) ;
#59501 = CARTESIAN_POINT ( 'NONE',  ( 0.000000000000000000, 0.000000000000000000, 0.000000000000000000 ) ) ;
#59502 = CARTESIAN_POINT ( 'NONE',  ( -83.88690842771663370, -50.15420337227475756, 186.5806298538265082 ) ) ;
#59503 = CIRCLE ( 'NONE', #95681, 4.000000000000001776 ) ;
#59504 = ORIENTED_EDGE ( 'NONE', *, *, #20829, .F. ) ;
#59505 = LINE ( 'NONE', #92379, #66445 ) ;
#59507 = CARTESIAN_POINT ( 'NONE',  ( 3.369683342533197123, -0.9132179776671599525, 104.1613013819149245 ) ) ;
#59506 = AXIS2_PLACEMENT_3D ( 'NONE', #3606, #43531, #83975 ) ;
#59508 = CARTESIAN_POINT ( 'NONE',  ( -82.50475734907109882, -37.83346213134558411, 7.442256542465846003 ) ) ;
#59509 = CARTESIAN_POINT ( 'NONE',  ( 0.000000000000000000, 0.000000000000000000, 0.000000000000000000 ) ) ;
#59510 = CARTESIAN_POINT ( 'NONE',  ( -15.65000555345723576, 44.05838121548723052, 4.644554625135834058 ) ) ;
#59511 = PRESENTATION_LAYER_ASSIGNMENT (  '', '', ( #35450 ) ) ;
#59512 = CARTESIAN_POINT ( 'NONE',  ( -9.858452382526078139, -11.68277816304066796, 9.415667523937807815 ) ) ;
#59513 = CARTESIAN_POINT ( 'NONE',  ( -6.224163897435901482, -12.02839407259639870, 11.51386142893533560 ) ) ;
#59514 = CARTESIAN_POINT ( 'NONE',  ( -55.65414010186720617, 42.00000000000000000, -72.41885610115910765 ) ) ;
#59515 = DIRECTION ( 'NONE',  ( -1.224646799147353454E-16, 0.000000000000000000, -1.000000000000000000 ) ) ;
#59516 = CARTESIAN_POINT ( 'NONE',  ( 65.47680943546976096, -59.99999999999998579, 130.5870305019238913 ) ) ;
#59517 = CARTESIAN_POINT ( 'NONE',  ( -2.071635198146551533E-15, 58.72416816948006613, 16.91618513671782509 ) ) ;
#59518 = EDGE_CURVE ( 'NONE', #17909, #54959, #6360, .T. ) ;
#59519 = CARTESIAN_POINT ( 'NONE',  ( -78.96607584984282369, -14.21045842199439946, -22.44766605243856361 ) ) ;
#59520 = CARTESIAN_POINT ( 'NONE',  ( -67.81647983110465816, -49.91373542098716598, 100.7778688019408833 ) ) ;
#59521 = AXIS2_PLACEMENT_3D ( 'NONE', #6951, #15040, #57089 ) ;
#59522 = ORIENTED_EDGE ( 'NONE', *, *, #54468, .F. ) ;
#59523 = CARTESIAN_POINT ( 'NONE',  ( 69.35339668739648289, -14.21045842199427511, 113.5888189438209537 ) ) ;
#59524 = CARTESIAN_POINT ( 'NONE',  ( -65.03121895707504052, 40.83786248443141176, -2.178857803530889647 ) ) ;
#59525 = ORIENTED_EDGE ( 'NONE', *, *, #45792, .T. ) ;
#59526 = CARTESIAN_POINT ( 'NONE',  ( 29.58605556073463561, -60.00000000000126477, 45.46635059003261858 ) ) ;
#59528 = ORIENTED_EDGE ( 'NONE', *, *, #79860, .F. ) ;
#59527 = CIRCLE ( 'NONE', #69837, 4.000000000000001776 ) ;
#59529 = CARTESIAN_POINT ( 'NONE',  ( 14.73587750591858736, -7.217011146677200450, 13.15299077803314809 ) ) ;
#59531 = AXIS2_PLACEMENT_3D ( 'NONE', #38430, #103146, #104723 ) ;
#59530 = CARTESIAN_POINT ( 'NONE',  ( 7.188101187500000044, -22.53125000204838457, 0.000000000000000000 ) ) ;
#59532 = CARTESIAN_POINT ( 'NONE',  ( -0.4139109374140990671, 28.18113469921472714, -38.31751619540018794 ) ) ;
#59533 = ORIENTED_EDGE ( 'NONE', *, *, #98033, .T. ) ;
#59534 = PRODUCT_DEFINITION_SHAPE ( 'NONE', 'NONE',  #19320 ) ;
#59535 = CARTESIAN_POINT ( 'NONE',  ( 16.65484354297773351, 0.000000000000000000, 5.000000000000002665 ) ) ;
#59536 = CIRCLE ( 'NONE', #81896, 4.000000000000007105 ) ;
#59537 = CARTESIAN_POINT ( 'NONE',  ( 1.053235267753768190, 13.99157560668549749, -6.921504917287050418 ) ) ;
#59538 = CARTESIAN_POINT ( 'NONE',  ( -11.51407961100473010, 43.27659971821058349, 14.44561041839115312 ) ) ;
#59539 = CARTESIAN_POINT ( 'NONE',  ( -7.188101187500002709, -13.81250000204838280, 2.977408999572648707 ) ) ;
#59540 = CARTESIAN_POINT ( 'NONE',  ( -3.313708498984765161, -17.65625000409676559, 7.999999999999998224 ) ) ;
#59541 = DIRECTION ( 'NONE',  ( 0.000000000000000000, 1.000000000000000000, 0.000000000000000000 ) ) ;
#59542 = DIRECTION ( 'NONE',  ( 0.000000000000000000, 0.000000000000000000, 1.000000000000000000 ) ) ;
#59543 = CARTESIAN_POINT ( 'NONE',  ( -8.737863884120026015, 49.99999999999999289, -79.96381019768847409 ) ) ;
#59544 = ADVANCED_FACE ( 'NONE', ( #28359 ), #97588, .T. ) ;
#59545 = CARTESIAN_POINT ( 'NONE',  ( -3.313708498984798467, -15.03124999999999289, -7.999999999999961808 ) ) ;
#59546 = UNCERTAINTY_MEASURE_WITH_UNIT (LENGTH_MEASURE( 1.000000000000000082E-05 ), #77584, 'distance_accuracy_value', 'NONE');
#59547 = ORIENTED_EDGE ( 'NONE', *, *, #85871, .F. ) ;
#59548 = CARTESIAN_POINT ( 'NONE',  ( 4.642888266381937967, -2.342832151813803332, 102.5319024079573751 ) ) ;
#59549 = CARTESIAN_POINT ( 'NONE',  ( 30.83049859532185266, -18.66191575932449709, 29.63070459022076619 ) ) ;
#59550 = CARTESIAN_POINT ( 'NONE',  ( 34.54626167956425320, 338.5217528747888309, -0.8335436382952816636 ) ) ;
#59551 = EDGE_LOOP ( 'NONE', ( #35066, #91267, #11720, #24707 ) ) ;
#59552 = VERTEX_POINT ( 'NONE', #53138 ) ;
#59554 = CARTESIAN_POINT ( 'NONE',  ( 1.301042606982605321E-15, -5.000000000000000000, -10.00000000000000000 ) ) ;
#59553 = CYLINDRICAL_SURFACE ( 'NONE', #58957, 4.000000000000000000 ) ;
#59555 = CARTESIAN_POINT ( 'NONE',  ( 4.852941176821355285, 40.28748324523049007, -70.80672828646224559 ) ) ;
#59556 = CARTESIAN_POINT ( 'NONE',  ( -44.26939524490970967, 485.3791217652519663, 2.298766312372937826 ) ) ;
#59557 = CARTESIAN_POINT ( 'NONE',  ( 7.500000000000001776, 0.000000000000000000, 0.000000000000000000 ) ) ;
#59558 = B_SPLINE_CURVE_WITH_KNOTS ( 'NONE', 3,
 ( #86171, #70497, #51638, #53251 ),
 .UNSPECIFIED., .F., .F.,
 ( 4, 4 ),
 ( 0.000000000000000000, 1.000000000000000000 ),
 .UNSPECIFIED. ) ;
#59559 = CARTESIAN_POINT ( 'NONE',  ( 32.71046359557010419, 465.7618366408551651, 11.82978892796172765 ) ) ;
#59560 = CARTESIAN_POINT ( 'NONE',  ( -36.69926874265555483, 463.5184712008561974, 19.71956904107290143 ) ) ;
#59561 = ORIENTED_EDGE ( 'NONE', *, *, #5866, .F. ) ;
#59562 = ADVANCED_FACE ( 'NONE', ( #103799 ), #38559, .T. ) ;
#59563 = CARTESIAN_POINT ( 'NONE',  ( 88.80472574437827404, -60.00000000000001421, -20.62865011427019368 ) ) ;
#59564 = DIRECTION ( 'NONE',  ( 0.5735764363510554853, 0.8191520442889852482, 0.000000000000000000 ) ) ;
#59565 = DIRECTION ( 'NONE',  ( 0.000000000000000000, 0.000000000000000000, 1.000000000000000000 ) ) ;
#59566 = CARTESIAN_POINT ( 'NONE',  ( 68.45015997180047407, -4.000000000000000888, 4.898587196589422689E-16 ) ) ;
#59567 = AXIS2_PLACEMENT_3D ( 'NONE', #21050, #11831, #60424 ) ;
#59568 = EDGE_CURVE ( 'NONE', #51711, #98765, #70908, .T. ) ;
#59569 = DIRECTION ( 'NONE',  ( 4.738110706560371839E-17, -0.9221233147934838614, 0.3868961001538753219 ) ) ;
#59570 = VERTEX_POINT ( 'NONE', #21329 ) ;
#59571 = LINE ( 'NONE', #91404, #103897 ) ;
#59572 = VERTEX_POINT ( 'NONE', #86056 ) ;
#59573 = VERTEX_POINT ( 'NONE', #62305 ) ;
#59574 = CARTESIAN_POINT ( 'NONE',  ( 5.656854249492378806, -11.18749999999999289, 5.656854249492381470 ) ) ;
#59575 = DIRECTION ( 'NONE',  ( 0.000000000000000000, 0.000000000000000000, 1.000000000000000000 ) ) ;
#59576 = DIRECTION ( 'NONE',  ( -1.000000000000000000, 0.000000000000000000, 0.000000000000000000 ) ) ;
#59577 = DIRECTION ( 'NONE',  ( 0.000000000000000000, 1.000000000000000000, 0.000000000000000000 ) ) ;
#59578 = CARTESIAN_POINT ( 'NONE',  ( 84.46485305342990557, -45.28549382349953589, -8.213565521267117475 ) ) ;
#59579 = CARTESIAN_POINT ( 'NONE',  ( -39.22939421798824355, 311.7623099566353062, 2.037218283543303698 ) ) ;
#59580 = CARTESIAN_POINT ( 'NONE',  ( -46.00000000000000000, 450.0000000000002274, 13.20242257375370976 ) ) ;
#59581 = CARTESIAN_POINT ( 'NONE',  ( -17.53081013949648437, 34.17129575104124939, 24.03823396542000879 ) ) ;
#59582 = VERTEX_POINT ( 'NONE', #94121 ) ;
#59583 = CARTESIAN_POINT ( 'NONE',  ( 6.500000000000000000, 2.536640449112291140, -0.3753468889000200481 ) ) ;
#59584 = ORIENTED_EDGE ( 'NONE', *, *, #84976, .T. ) ;
#59585 = FACE_OUTER_BOUND ( 'NONE', #53298, .T. ) ;
#59587 = EDGE_LOOP ( 'NONE', ( #17228, #28246, #18951, #6320, #77010 ) ) ;
#59586 = DIRECTION ( 'NONE',  ( -1.000000000000000000, -1.224606353822377258E-16, -0.000000000000000000 ) ) ;
#59588 = CARTESIAN_POINT ( 'NONE',  ( 76.65407396917700567, -42.96273530073847269, 130.6257724894647083 ) ) ;
#59589 = EDGE_CURVE ( 'NONE', #10296, #101939, #13717, .T. ) ;
#59590 = ORIENTED_EDGE ( 'NONE', *, *, #60833, .F. ) ;
#59591 = CARTESIAN_POINT ( 'NONE',  ( 4.571169277359397043, -52.34660364318141035, 40.23372900632212890 ) ) ;
#59592 = FACE_OUTER_BOUND ( 'NONE', #98996, .T. ) ;
#59593 = CARTESIAN_POINT ( 'NONE',  ( -7.188101187500000044, -25.90625000204838813, -8.802885111219163269E-16 ) ) ;
#59594 = CARTESIAN_POINT ( 'NONE',  ( -98.27571109168336250, -57.67134109913899209, 58.06786128689789450 ) ) ;
#59595 = VECTOR ( 'NONE', #81297, 1000.000000000000000 ) ;
#59596 = ORIENTED_EDGE ( 'NONE', *, *, #104943, .F. ) ;
#59597 = SURFACE_STYLE_USAGE ( .BOTH. , #75760 ) ;
#59598 = FACE_BOUND ( 'NONE', #28697, .T. ) ;
#59599 = CARTESIAN_POINT ( 'NONE',  ( 102.3723399798224278, -37.84840448700200710, 181.3185192590994461 ) ) ;
#59600 = DIRECTION ( 'NONE',  ( 0.000000000000000000, 0.000000000000000000, 1.000000000000000000 ) ) ;
#59601 = DIRECTION ( 'NONE',  ( -1.000000000000000000, -1.224606353822377258E-16, -0.000000000000000000 ) ) ;
#59602 = COLOUR_RGB ( '', 0.72549020, 0.75294118, 0.79215686) ;
#59603 = CARTESIAN_POINT ( 'NONE',  ( 3.313708498984762496, -24.96875000409677270, 7.999999999999998224 ) ) ;
#59604 = AXIS2_PLACEMENT_3D ( 'NONE', #63680, #5430, #71214 ) ;
#59605 = CARTESIAN_POINT ( 'NONE',  ( 0.000000000000000000, -6.938893903907228378E-15, 7.000000000000000000 ) ) ;
#59606 = CONICAL_SURFACE ( 'NONE', #32045, 5.000000000000001776, 0.9599310885968803664 ) ;
#59607 = CARTESIAN_POINT ( 'NONE',  ( -36.95256697677980640, 25.70493088644785828, 13.30651231931578415 ) ) ;
#59608 = VECTOR ( 'NONE', #101428, 1000.000000000000000 ) ;
#59609 = SURFACE_STYLE_USAGE ( .BOTH. , #58540 ) ;
#59610 = FILL_AREA_STYLE_COLOUR ( '', #17684 ) ;
#59611 = DIRECTION ( 'NONE',  ( -0.5735764363510497121, 0.8191520442889892450, 1.003171929053521665E-16 ) ) ;
#59612 = DIRECTION ( 'NONE',  ( -1.000000000000000000, -4.493451613004600994E-20, 9.836563810794311799E-22 ) ) ;
#59613 = CARTESIAN_POINT ( 'NONE',  ( 12.61650669486618881, 4.000000000000003553, 4.898587196589414801E-16 ) ) ;
#59614 = ORIENTED_EDGE ( 'NONE', *, *, #15609, .T. ) ;
#59615 = CARTESIAN_POINT ( 'NONE',  ( -5.437559411288403588, 41.94910065564111790, -59.21852893438062893 ) ) ;
#59616 = DIRECTION ( 'NONE',  ( 0.000000000000000000, -1.000000000000000000, 0.000000000000000000 ) ) ;
#59617 = AXIS2_PLACEMENT_3D ( 'NONE', #43683, #18374, #27014 ) ;
#59618 = EDGE_CURVE ( 'NONE', #79335, #741, #78994, .T. ) ;
#59619 = DIRECTION ( 'NONE',  ( 0.000000000000000000, 1.000000000000000000, 0.000000000000000000 ) ) ;
#59620 = CARTESIAN_POINT ( 'NONE',  ( -85.49209400632499012, -29.99999999999999289, 174.7575250798003594 ) ) ;
#59621 = EDGE_CURVE ( 'NONE', #67362, #77056, #79522, .T. ) ;
#59622 = EDGE_LOOP ( 'NONE', ( #54232, #27436, #45756, #98947 ) ) ;
#59623 = FACE_OUTER_BOUND ( 'NONE', #40952, .T. ) ;
#59624 = CARTESIAN_POINT ( 'NONE',  ( 72.13773045038885812, -57.67273300135423142, 173.4418561065998290 ) ) ;
#59625 = EDGE_CURVE ( 'NONE', #1485, #84857, #16693, .T. ) ;
#59627 = DIRECTION ( 'NONE',  ( -1.000000000000000000, -1.224606353822377258E-16, -0.000000000000000000 ) ) ;
#59626 = CARTESIAN_POINT ( 'NONE',  ( -14.85111941933941360, 2.241372557327220960, -2.058092574375395500 ) ) ;
#59628 = CARTESIAN_POINT ( 'NONE',  ( 62.79636538027480697, -37.67681387382631897, -33.45663682702740971 ) ) ;
#59629 = CARTESIAN_POINT ( 'NONE',  ( -15.76884112491384649, 22.48937974161067999, -2.489079047167402692 ) ) ;
#59630 = CARTESIAN_POINT ( 'NONE',  ( -31.93456279712680868, -60.00000000000000000, 44.12512568447651518 ) ) ;
#59631 =( NAMED_UNIT ( * ) PLANE_ANGLE_UNIT ( ) SI_UNIT ( $, .RADIAN. ) );
#59632 = CARTESIAN_POINT ( 'NONE',  ( -86.49709195177823062, -42.82432661300771315, 189.1473926100390202 ) ) ;
#59633 = EDGE_LOOP ( 'NONE', ( #54400, #94139, #57430, #10064, #80951 ) ) ;
#59634 = CARTESIAN_POINT ( 'NONE',  ( -3.050654622591071341, -46.43922741216240269, 31.62448634903992328 ) ) ;
#59635 = CIRCLE ( 'NONE', #57911, 4.172000000000009479 ) ;
#59636 = FACE_OUTER_BOUND ( 'NONE', #69463, .T. ) ;
#59637 = FACE_OUTER_BOUND ( 'NONE', #33244, .T. ) ;
#59639 = DIRECTION ( 'NONE',  ( 0.000000000000000000, 0.000000000000000000, -1.000000000000000000 ) ) ;
#59638 = CARTESIAN_POINT ( 'NONE',  ( -42.77874154194343248, 403.4964952544876837, 19.98380564842762652 ) ) ;
#59640 = EDGE_LOOP ( 'NONE', ( #71493, #8014, #3426, #1665, #3493 ) ) ;
#59641 = DIRECTION ( 'NONE',  ( -1.000000000000000000, 0.000000000000000000, 0.000000000000000000 ) ) ;
#59642 = LINE ( 'NONE', #92516, #44265 ) ;
#59643 = CARTESIAN_POINT ( 'NONE',  ( -30.23149608710439651, 7.786108077162772645, -41.98074016422817323 ) ) ;
#59644 = CARTESIAN_POINT ( 'NONE',  ( 25.15391212174589342, 295.6014252248689331, -9.839392187590416228 ) ) ;
#59645 = CARTESIAN_POINT ( 'NONE',  ( 43.29658055318886767, 324.1952503670673877, -2.852919881210743913 ) ) ;
#59646 = SURFACE_STYLE_FILL_AREA ( #59114 ) ;
#59647 = ADVANCED_FACE ( 'NONE', ( #45585 ), #5117, .T. ) ;
#59648 = CARTESIAN_POINT ( 'NONE',  ( 109.5313825839763382, -30.00000000000004619, 176.4140126643321196 ) ) ;
#59649 = CARTESIAN_POINT ( 'NONE',  ( -79.06061194151560301, -53.37725854339807796, 155.5602507423176064 ) ) ;
#59650 = VERTEX_POINT ( 'NONE', #81106 ) ;
#59651 = LINE ( 'NONE', #75273, #41268 ) ;
#59652 = CARTESIAN_POINT ( 'NONE',  ( 5.911778709945828325, 253.8666183941656413, 1.058844270818172451 ) ) ;
#59653 = CARTESIAN_POINT ( 'NONE',  ( 41.27118623434287059, -57.68915202794213570, 57.80005340834581062 ) ) ;
#59654 = FACE_OUTER_BOUND ( 'NONE', #100157, .T. ) ;
#59655 = CARTESIAN_POINT ( 'NONE',  ( 51.01037695545453232, 450.0000000000002274, 8.202422573753707979 ) ) ;
#59656 = EDGE_CURVE ( 'NONE', #13309, #44189, #90766, .T. ) ;
#59657 = CARTESIAN_POINT ( 'NONE',  ( 43.71037717921920773, 462.3391554988764369, 4.824299547763891027 ) ) ;
#59658 = ORIENTED_EDGE ( 'NONE', *, *, #8488, .T. ) ;
#59659 = CARTESIAN_POINT ( 'NONE',  ( 31.31558333044079845, 439.0792886710837593, 22.75757024719011667 ) ) ;
#59660 = EDGE_LOOP ( 'NONE', ( #86998, #87393, #48456, #71371, #85315 ) ) ;
#59661 =( BOUNDED_SURFACE ( )  B_SPLINE_SURFACE ( 3, 2, ( 
 ( #16830, #8724, #75588 ),
 ( #34110, #41632, #82622 ),
 ( #50249, #593, #74516 ),
 ( #23891, #17906, #33038 ),
 ( #82075, #42693, #48639 ),
 ( #98269, #58894, #73447 ),
 ( #1687, #33558, #25486 ),
 ( #91785, #83150, #32506 ),
 ( #58345, #98785, #66433 ),
 ( #57260, #50759, #99314 ),
 ( #91264, #83667, #66982 ),
 ( #42156, #75038, #8193 ) ),
 .UNSPECIFIED., .F., .F., .F. ) 
 B_SPLINE_SURFACE_WITH_KNOTS ( ( 4, 2, 2, 2, 2, 4 ),
 ( 3, 3 ),
 ( -7.849623728795052102E-17, 0.001471464792628909357, 0.002942929585257897211, 0.003678661981572391246, 0.004414394377886885282, 0.005885859170515872485 ),
 ( 0.000000000000000000, 1.000000000000000000 ),
 .UNSPECIFIED. ) 
 GEOMETRIC_REPRESENTATION_ITEM ( )  RATIONAL_B_SPLINE_SURFACE ( (
 ( 1.000000000000000000, 0.8274249441181704690, 1.000000000000000000),
 ( 1.000000000000000000, 0.8369779515072608422, 1.000000000000000000),
 ( 1.000000000000000000, 0.8428664650367967415, 1.000000000000000000),
 ( 1.000000000000000000, 0.8506961607541885240, 1.000000000000000000),
 ( 1.000000000000000000, 0.8526029425214399771, 1.000000000000000000),
 ( 1.000000000000000000, 0.8531612821180112327, 1.000000000000000000),
 ( 1.000000000000000000, 0.8529462785843203720, 1.000000000000000000),
 ( 1.000000000000000000, 0.8517601151918051672, 1.000000000000000000),
 ( 1.000000000000000000, 0.8507906177104697099, 1.000000000000000000),
 ( 1.000000000000000000, 0.8467143344647574121, 1.000000000000000000),
 ( 1.000000000000000000, 0.8424736042939275915, 1.000000000000000000),
 ( 1.000000000000000000, 0.8360809698953391988, 1.000000000000000000) ) ) 
 REPRESENTATION_ITEM ( '' )  SURFACE ( )  );
#59662 = DIRECTION ( 'NONE',  ( 0.000000000000000000, -1.000000000000000000, 0.000000000000000000 ) ) ;
#59663 = CARTESIAN_POINT ( 'NONE',  ( 32.28930913498002298, 488.2717154064769147, 9.213726894932324996 ) ) ;
#59664 = EDGE_CURVE ( 'NONE', #30747, #3039, #80419, .T. ) ;
#59665 = CARTESIAN_POINT ( 'NONE',  ( 62.34828826643940403, 50.00000000000000000, -10.72527895994504199 ) ) ;
#59666 = CARTESIAN_POINT ( 'NONE',  ( 5.000000000000000000, -14.13517361223990498, 11.83579766570910508 ) ) ;
#59667 = DIRECTION ( 'NONE',  ( -0.3108677890940485522, 0.06041750367991206849, 0.9485309393756568008 ) ) ;
#59668 = EDGE_LOOP ( 'NONE', ( #15453, #23613, #14916 ) ) ;
#59669 = CARTESIAN_POINT ( 'NONE',  ( 102.6668771475679307, -60.00000000000000000, 96.69110907683354128 ) ) ;
#59670 = AXIS2_PLACEMENT_3D ( 'NONE', #61056, #62650, #95532 ) ;
#59672 = CARTESIAN_POINT ( 'NONE',  ( 20.66686156031881083, -60.35595528423025513, 34.55852652023040861 ) ) ;
#59671 = CARTESIAN_POINT ( 'NONE',  ( -78.95080019145578376, -30.00000000000002842, 188.4626203831212479 ) ) ;
#59674 = DIRECTION ( 'NONE',  ( -1.000000000000000000, -0.000000000000000000, -0.000000000000000000 ) ) ;
#59673 = UNCERTAINTY_MEASURE_WITH_UNIT (LENGTH_MEASURE( 1.000000000000000082E-05 ), #87462, 'distance_accuracy_value', 'NONE');
#59675 = CARTESIAN_POINT ( 'NONE',  ( 37.65939668336066148, 425.4643409788083659, 5.784973202707226037 ) ) ;
#59676 = CARTESIAN_POINT ( 'NONE',  ( -42.83329106564534783, -32.61700632504245334, 39.59767786645361554 ) ) ;
#59677 = CARTESIAN_POINT ( 'NONE',  ( 38.86650669486618881, 4.898587196589411843E-16, -4.000000000000000888 ) ) ;
#59678 = CIRCLE ( 'NONE', #28675, 4.250000000000000000 ) ;
#59679 =( GEOMETRIC_REPRESENTATION_CONTEXT ( 3 ) GLOBAL_UNCERTAINTY_ASSIGNED_CONTEXT ( ( #45877 ) ) GLOBAL_UNIT_ASSIGNED_CONTEXT ( ( #60632, #54084, #86509 ) ) REPRESENTATION_CONTEXT ( 'NONE', 'WORKASPACE' ) );
#59680 = ORIENTED_EDGE ( 'NONE', *, *, #81241, .T. ) ;
#59681 = CARTESIAN_POINT ( 'NONE',  ( -8.127057321558263325, -4.285714285714295357, 23.93420880016847718 ) ) ;
#59682 = AXIS2_PLACEMENT_3D ( 'NONE', #55466, #45290, #13418 ) ;
#59683 = DIRECTION ( 'NONE',  ( -1.000000000000000000, -1.224606353822377258E-16, -0.000000000000000000 ) ) ;
#59684 = CARTESIAN_POINT ( 'NONE',  ( -43.99367409961224240, 462.7719748076324322, 5.584664003525471543 ) ) ;
#59685 =( GEOMETRIC_REPRESENTATION_CONTEXT ( 3 ) GLOBAL_UNCERTAINTY_ASSIGNED_CONTEXT ( ( #95756 ) ) GLOBAL_UNIT_ASSIGNED_CONTEXT ( ( #21727, #37391, #20697 ) ) REPRESENTATION_CONTEXT ( 'NONE', 'WORKASPACE' ) );
#59686 = CARTESIAN_POINT ( 'NONE',  ( 6.333820801329741457, 6.982605850968585770, 0.9057718968909901358 ) ) ;
#59687 = CARTESIAN_POINT ( 'NONE',  ( 5.385673916453011856, 0.000000000000000000, 18.57417562100670949 ) ) ;
#59688 = ORIENTED_EDGE ( 'NONE', *, *, #56017, .F. ) ;
#59689 = CARTESIAN_POINT ( 'NONE',  ( -15.53259594841271962, 37.09623604092400484, -22.76975648258506268 ) ) ;
#59690 = VERTEX_POINT ( 'NONE', #40127 ) ;
#59691 = CARTESIAN_POINT ( 'NONE',  ( 100.3476047149571428, -30.00000000000000355, 183.8784433964002574 ) ) ;
#59692 = CARTESIAN_POINT ( 'NONE',  ( 32.97698008590906227, 40.71205098343299511, -62.29860342917670835 ) ) ;
#59693 = CARTESIAN_POINT ( 'NONE',  ( 24.31925498810626607, 25.21059430657137312, -32.55251039702583427 ) ) ;
#59694 = MECHANICAL_DESIGN_GEOMETRIC_PRESENTATION_REPRESENTATION (  '', ( #52820 ), #37382 ) ;
#59695 = CARTESIAN_POINT ( 'NONE',  ( 86.83990384507222871, -30.00000000000000000, 69.50558600361652850 ) ) ;
#59696 = ADVANCED_FACE ( 'NONE', ( #73004 ), #97118, .F. ) ;
#59697 = CARTESIAN_POINT ( 'NONE',  ( -27.73415475396909358, 311.1673401819404603, 11.68908720022844783 ) ) ;
#59698 = ORIENTED_EDGE ( 'NONE', *, *, #64576, .F. ) ;
#59699 = ORIENTED_EDGE ( 'NONE', *, *, #50323, .F. ) ;
#59700 = EDGE_LOOP ( 'NONE', ( #56438, #56382, #105982, #33689, #88807 ) ) ;
#59701 = VECTOR ( 'NONE', #67003, 999.9999999999998863 ) ;
#59703 = VERTEX_POINT ( 'NONE', #88159 ) ;
#59702 = CARTESIAN_POINT ( 'NONE',  ( -32.12958771267405211, 464.7275665249412668, 11.12424126545829495 ) ) ;
#59704 = FACE_OUTER_BOUND ( 'NONE', #1033, .T. ) ;
#59705 = CARTESIAN_POINT ( 'NONE',  ( -18.18913180585775180, 303.6389006221185696, 9.891726125135546610 ) ) ;
#59706 = CARTESIAN_POINT ( 'NONE',  ( 5.646888413699863385, -13.44974155970390406, 2.040714635159913914 ) ) ;
#59707 = ADVANCED_FACE ( 'NONE', ( #7744 ), #105396, .T. ) ;
#59708 = CARTESIAN_POINT ( 'NONE',  ( -31.16747616410718180, 425.0719001433796507, 24.76640343511496312 ) ) ;
#59709 = ORIENTED_EDGE ( 'NONE', *, *, #34650, .F. ) ;
#59710 = CARTESIAN_POINT ( 'NONE',  ( -1.308996937480700895, 49.99999999999999289, -75.00000000000001421 ) ) ;
#59712 = ADVANCED_FACE ( 'NONE', ( #96783 ), #14990, .T. ) ;
#59711 = ORIENTED_EDGE ( 'NONE', *, *, #55688, .F. ) ;
#59713 = CARTESIAN_POINT ( 'NONE',  ( 17.33349330513380693, 1.593028355512270962E-15, 0.000000000000000000 ) ) ;
#59714 = CARTESIAN_POINT ( 'NONE',  ( 74.46552664185318804, -38.32957883525645570, 164.4766580072155193 ) ) ;
#59715 = CARTESIAN_POINT ( 'NONE',  ( 16.65484354297773351, 5.000000000000004441, 6.123233995736770227E-16 ) ) ;
#59716 = EDGE_CURVE ( 'NONE', #57410, #27178, #92685, .T. ) ;
#59717 = CARTESIAN_POINT ( 'NONE',  ( 35.23215581420184606, 303.5527974176312114, 3.940093505360380721 ) ) ;
#59718 = PRESENTATION_LAYER_ASSIGNMENT (  '', '', ( #7945 ) ) ;
#59719 = CARTESIAN_POINT ( 'NONE',  ( 37.62251730745840916, 437.3427388312647395, 4.535622330043188377 ) ) ;
#59720 = EDGE_CURVE ( 'NONE', #103692, #8947, #91780, .T. ) ;
#59721 = ORIENTED_EDGE ( 'NONE', *, *, #58737, .T. ) ;
#59722 = DIRECTION ( 'NONE',  ( -1.000000000000000000, -1.224606353822377258E-16, -0.000000000000000000 ) ) ;
#59723 = DIRECTION ( 'NONE',  ( 0.000000000000000000, 1.000000000000000000, -1.224646799147353207E-16 ) ) ;
#59724 = DIRECTION ( 'NONE',  ( 1.000000000000000000, 0.000000000000000000, 0.000000000000000000 ) ) ;
#59725 = DIRECTION ( 'NONE',  ( 1.000000000000000000, 1.224606353822377258E-16, 0.000000000000000000 ) ) ;
#59726 = CARTESIAN_POINT ( 'NONE',  ( 15.22818746203032703, 3.929489829918875632, 4.609438620807825515 ) ) ;
#59727 = ORIENTED_EDGE ( 'NONE', *, *, #62626, .T. ) ;
#59728 = CARTESIAN_POINT ( 'NONE',  ( 7.045755811259133417, -86.30341603013555130, 3.790843699961855773 ) ) ;
#59729 = DIRECTION ( 'NONE',  ( 1.000000000000000000, 0.000000000000000000, 0.000000000000000000 ) ) ;
#59730 = CARTESIAN_POINT ( 'NONE',  ( -5.147825380260277583, -5.688155668810499499, -7.450218641349906079 ) ) ;
#59731 = CARTESIAN_POINT ( 'NONE',  ( 7.169685563733668943, 294.7252197711828785, 1.910215062213532544 ) ) ;
#59732 =( NAMED_UNIT ( * ) PLANE_ANGLE_UNIT ( ) SI_UNIT ( $, .RADIAN. ) );
#59733 = DIRECTION ( 'NONE',  ( 0.000000000000000000, -1.000000000000000000, 0.000000000000000000 ) ) ;
#59734 = CARTESIAN_POINT ( 'NONE',  ( 84.69561524692119292, -53.82596867418983777, 190.2036044253954117 ) ) ;
#59735 = CARTESIAN_POINT ( 'NONE',  ( 17.39534200550397713, 36.29816465214055654, -24.14189926133832387 ) ) ;
#59736 = AXIS2_PLACEMENT_3D ( 'NONE', #21798, #22328, #14183 ) ;
#59737 = CARTESIAN_POINT ( 'NONE',  ( -8.241419208044183264, 35.69988999158558585, 0.000000000000000000 ) ) ;
#59738 = ORIENTED_EDGE ( 'NONE', *, *, #83198, .F. ) ;
#59739 = CARTESIAN_POINT ( 'NONE',  ( -5.698650001973517121, 4.592339236403556235, -6.344532336093704039 ) ) ;
#59740 = CARTESIAN_POINT ( 'NONE',  ( 41.49004662521136311, 469.3948935002796929, 1.006167576246231654 ) ) ;
#59741 = CARTESIAN_POINT ( 'NONE',  ( -10.00000000000000000, 0.000000000000000000, 10.00000000000000178 ) ) ;
#59742 = CARTESIAN_POINT ( 'NONE',  ( 4.898587196589412829E-16, -18.12499999999999645, -8.000000000000000000 ) ) ;
#59743 = CARTESIAN_POINT ( 'NONE',  ( -83.07394592710599568, -30.00000000000000355, 43.49111805028168476 ) ) ;
#59744 = EDGE_CURVE ( 'NONE', #56662, #54299, #1257, .T. ) ;
#59745 = TOROIDAL_SURFACE ( 'NONE', #30425, 57.86910460382442523, 0.5000000000000000000 ) ;
#59746 = DIRECTION ( 'NONE',  ( 0.000000000000000000, 0.000000000000000000, 1.000000000000000000 ) ) ;
#59747 = CIRCLE ( 'NONE', #101081, 4.000000000000001776 ) ;
#59748 = CARTESIAN_POINT ( 'NONE',  ( -8.000000000000000000, -29.93750000409677270, -9.797174393178825657E-16 ) ) ;
#59749 = FACE_OUTER_BOUND ( 'NONE', #13660, .T. ) ;
#59750 = EDGE_CURVE ( 'NONE', #47858, #105570, #85699, .T. ) ;
#59752 = DIRECTION ( 'NONE',  ( 0.000000000000000000, 0.000000000000000000, 1.000000000000000000 ) ) ;
#59751 = CARTESIAN_POINT ( 'NONE',  ( -9.948513602188008065, 246.1302205665613201, 1.045942665286136775 ) ) ;
#59753 = DIRECTION ( 'NONE',  ( -1.000000000000000000, 0.000000000000000000, 0.000000000000000000 ) ) ;
#59754 = CARTESIAN_POINT ( 'NONE',  ( -23.11910152252719186, -26.95796857353470699, 29.27772215835345548 ) ) ;
#59755 = CARTESIAN_POINT ( 'NONE',  ( 105.5353273971932140, -5.000000000000000888, 6.123233995736779101E-16 ) ) ;
#59756 = CARTESIAN_POINT ( 'NONE',  ( 0.06682554136338283990, -6.264794173742283867, -2.149058192116890531 ) ) ;
#59757 = CIRCLE ( 'NONE', #56325, 10.00000000000000178 ) ;
#59758 = AXIS2_PLACEMENT_3D ( 'NONE', #96926, #56445, #47822 ) ;
#59759 = CARTESIAN_POINT ( 'NONE',  ( 56.05738515965948920, -28.67099341655612221, -26.25941955160380203 ) ) ;
#59760 = CARTESIAN_POINT ( 'NONE',  ( -22.60355412798201868, -42.95868515067972027, 31.91959776729930098 ) ) ;
#59761 = CIRCLE ( 'NONE', #28766, 4.000000000000000888 ) ;
#59762 = EDGE_LOOP ( 'NONE', ( #51465, #75168, #94733, #90825 ) ) ;
#59763 = CARTESIAN_POINT ( 'NONE',  ( 37.61650669486618881, 1.474610560812782335E-15, 0.000000000000000000 ) ) ;
#59764 = CARTESIAN_POINT ( 'NONE',  ( -9.948561005166130400, 108.8699027374820076, -1.045755304005130393 ) ) ;
#59765 = MECHANICAL_DESIGN_GEOMETRIC_PRESENTATION_REPRESENTATION (  '', ( #78749 ), #21907 ) ;
#59766 = CARTESIAN_POINT ( 'NONE',  ( -19.91006257873084806, -29.03434590422582318, 29.21953239927981016 ) ) ;
#59767 = CARTESIAN_POINT ( 'NONE',  ( -43.81237681895566283, -25.95568800022653733, -29.47119608928409207 ) ) ;
#59769 = CARTESIAN_POINT ( 'NONE',  ( -74.86581005675350298, -60.22815006648220759, -24.22472159026646210 ) ) ;
#59768 = DIRECTION ( 'NONE',  ( 0.000000000000000000, 0.000000000000000000, 1.000000000000000000 ) ) ;
#59770 = EDGE_CURVE ( 'NONE', #42175, #104525, #77637, .T. ) ;
#59771 = ORIENTED_EDGE ( 'NONE', *, *, #96152, .F. ) ;
#59772 = CARTESIAN_POINT ( 'NONE',  ( -36.04676067413578977, 437.4614642643933848, 4.333815353352441058 ) ) ;
#59773 = VERTEX_POINT ( 'NONE', #57351 ) ;
#59774 = DIRECTION ( 'NONE',  ( 0.000000000000000000, 0.000000000000000000, 1.000000000000000000 ) ) ;
#59775 = CARTESIAN_POINT ( 'NONE',  ( 31.46253585067004721, 0.000000000000000000, 5.000000000000002665 ) ) ;
#59776 = EDGE_CURVE ( 'NONE', #58911, #65010, #80042, .T. ) ;
#59777 = CARTESIAN_POINT ( 'NONE',  ( -17.43438663440721470, -60.00000000000000711, -42.00932408933469731 ) ) ;
#59778 = ORIENTED_EDGE ( 'NONE', *, *, #40426, .T. ) ;
#59779 = DIRECTION ( 'NONE',  ( 1.000000000000000000, 0.000000000000000000, 0.000000000000000000 ) ) ;
#59780 = CARTESIAN_POINT ( 'NONE',  ( 0.000000000000000000, 294.8518027762758038, -10.00000000000000178 ) ) ;
#59781 = CARTESIAN_POINT ( 'NONE',  ( 98.83619226181630779, -37.79122241413045913, 192.0200725842609017 ) ) ;
#59783 = CARTESIAN_POINT ( 'NONE',  ( -7.046357527897575856, -8.693843493989968252, -3.789683693877206050 ) ) ;
#59782 = CARTESIAN_POINT ( 'NONE',  ( 5.765378947742160420, -19.37891530848101240, 27.10972434534570397 ) ) ;
#59784 = AXIS2_PLACEMENT_3D ( 'NONE', #76881, #68819, #19771 ) ;
#59785 = ORIENTED_EDGE ( 'NONE', *, *, #53247, .F. ) ;
#59786 = VERTEX_POINT ( 'NONE', #104871 ) ;
#59787 = AXIS2_PLACEMENT_3D ( 'NONE', #52630, #27358, #83409 ) ;
#59788 = ORIENTED_EDGE ( 'NONE', *, *, #65240, .T. ) ;
#59789 = CARTESIAN_POINT ( 'NONE',  ( 25.77159080061642982, 308.6327058502350837, 9.816061668938694140 ) ) ;
#59790 = FACE_OUTER_BOUND ( 'NONE', #55080, .T. ) ;
#59791 = CARTESIAN_POINT ( 'NONE',  ( 37.33349330513379982, -4.000000000000000888, 4.898587196589416773E-16 ) ) ;
#59793 = ADVANCED_FACE ( 'NONE', ( #67600 ), #104606, .T. ) ;
#59792 = ORIENTED_EDGE ( 'NONE', *, *, #85599, .T. ) ;
#59794 = ADVANCED_FACE ( 'NONE', ( #100478 ), #9329, .T. ) ;
#59795 = CARTESIAN_POINT ( 'NONE',  ( 17.61650669486618881, -3.851859888774471706E-31, 4.000000000000000888 ) ) ;
#59796 = CARTESIAN_POINT ( 'NONE',  ( 31.56688555236322102, 439.0033367035658216, 23.33558518086852374 ) ) ;
#59797 = CARTESIAN_POINT ( 'NONE',  ( -99.52194594362661917, -60.00000000003903722, 63.55695574102755074 ) ) ;
#59798 = CARTESIAN_POINT ( 'NONE',  ( 7.413471587080151082, -67.64352159168328171, -3.013058070223549656 ) ) ;
#59799 = CARTESIAN_POINT ( 'NONE',  ( -34.72474116627837759, 338.3618661353910966, -1.881472242819908436 ) ) ;
#59800 = CARTESIAN_POINT ( 'NONE',  ( -6.767547366757451499, 41.65232185610268090, -58.92985803237888121 ) ) ;
#59801 = CARTESIAN_POINT ( 'NONE',  ( -92.19364677446148448, -60.00000000000002842, -19.86446420722052153 ) ) ;
#59802 = CARTESIAN_POINT ( 'NONE',  ( -43.55333112596417067, 465.2342844084853937, 9.238213423004422609 ) ) ;
#59803 = CARTESIAN_POINT ( 'NONE',  ( -49.43394015148312093, -32.59389012172065492, 47.58532889687595002 ) ) ;
#59804 = ORIENTED_EDGE ( 'NONE', *, *, #30652, .F. ) ;
#59805 = DIRECTION ( 'NONE',  ( -1.000000000000000000, -1.224606353822377258E-16, -0.000000000000000000 ) ) ;
#59806 = ORIENTED_EDGE ( 'NONE', *, *, #106183, .T. ) ;
#59807 = CARTESIAN_POINT ( 'NONE',  ( -96.11536361813142548, -52.81603231299632739, 195.4403539845496880 ) ) ;
#59808 = DIRECTION ( 'NONE',  ( 1.000000000000000000, -0.000000000000000000, -0.000000000000000000 ) ) ;
#59809 = CARTESIAN_POINT ( 'NONE',  ( 9.918658701378005205, -2.743202263443990763, 15.35583465422220861 ) ) ;
#59810 = ORIENTED_EDGE ( 'NONE', *, *, #3730, .F. ) ;
#59811 = CARTESIAN_POINT ( 'NONE',  ( 4.660674839411950821, 248.6821751469559274, -3.778981567323782986 ) ) ;
#59812 = CIRCLE ( 'NONE', #58096, 4.000000000000000888 ) ;
#59813 = CARTESIAN_POINT ( 'NONE',  ( 97.76259370245983860, -38.48107996425336808, 201.0305891777979070 ) ) ;
#59814 = CARTESIAN_POINT ( 'NONE',  ( 49.27896781154971961, 13.08675713149488473, 15.56311823694137786 ) ) ;
#59815 = FILL_AREA_STYLE ('',( #53309 ) ) ;
#59816 = DIRECTION ( 'NONE',  ( 0.000000000000000000, 0.000000000000000000, 1.000000000000000000 ) ) ;
#59817 = FACE_OUTER_BOUND ( 'NONE', #39135, .T. ) ;
#59818 = CARTESIAN_POINT ( 'NONE',  ( 85.96525886290406504, -30.00000000000000000, 178.3582022700497021 ) ) ;
#59819 = CARTESIAN_POINT ( 'NONE',  ( -10.28624191511830155, 43.99263840937192782, -12.90779740156156841 ) ) ;
#59820 = EDGE_CURVE ( 'NONE', #58545, #22313, #34043, .T. ) ;
#59821 = CARTESIAN_POINT ( 'NONE',  ( 26.08349330513380693, 4.000000000000003553, 0.000000000000000000 ) ) ;
#59822 = B_SPLINE_CURVE_WITH_KNOTS ( 'NONE', 3,
 ( #101820, #27986, #12801, #77556, #13328, #4197 ),
 .UNSPECIFIED., .F., .F.,
 ( 4, 2, 4 ),
 ( 9.697399036122160616E-19, 0.002016319290324490501, 0.004032638580648980134 ),
 .UNSPECIFIED. ) ;
#59823 = ORIENTED_EDGE ( 'NONE', *, *, #54093, .F. ) ;
#59824 = ORIENTED_EDGE ( 'NONE', *, *, #51619, .T. ) ;
#59825 = CARTESIAN_POINT ( 'NONE',  ( 53.07978571422346192, -18.70625430049756943, 48.69073338330034062 ) ) ;
#59826 = CIRCLE ( 'NONE', #30574, 3.999999999999999112 ) ;
#59827 = CARTESIAN_POINT ( 'NONE',  ( -44.28898793531455880, 435.1858057187417899, 13.53393906085753784 ) ) ;
#59828 = AXIS2_PLACEMENT_3D ( 'NONE', #105787, #64288, #40526 ) ;
#59829 = CARTESIAN_POINT ( 'NONE',  ( 0.000000000000000000, 0.000000000000000000, 0.000000000000000000 ) ) ;
#59830 = SHAPE_REPRESENTATION ( '12. Movable Jaw', ( #10728 ), #21183 ) ;
#59831 = ADVANCED_FACE ( 'NONE', ( #34191 ), #41984, .F. ) ;
#59832 = ORIENTED_EDGE ( 'NONE', *, *, #4912, .F. ) ;
#59833 = CARTESIAN_POINT ( 'NONE',  ( -91.43458545515113656, -38.37511409388242356, -4.844227564306105904 ) ) ;
#59834 = ORIENTED_EDGE ( 'NONE', *, *, #18767, .F. ) ;
#59835 = CARTESIAN_POINT ( 'NONE',  ( 108.0216010846900048, -38.35838589254169051, 192.8427407754958836 ) ) ;
#59836 = CARTESIAN_POINT ( 'NONE',  ( 15.26512326535558373, 22.59485187131588901, -2.832032051335056533 ) ) ;
#59838 = CARTESIAN_POINT ( 'NONE',  ( 88.90319265580640717, -60.14988975799602855, 46.79599450796897742 ) ) ;
#59837 = AXIS2_PLACEMENT_3D ( 'NONE', #13518, #14574, #5961 ) ;
#59839 = AXIS2_PLACEMENT_3D ( 'NONE', #30456, #6141, #73521 ) ;
#59840 = CARTESIAN_POINT ( 'NONE',  ( -0.1691415264582396272, 46.21383923812596350, -16.25000000000000355 ) ) ;
#59842 = CIRCLE ( 'NONE', #13294, 4.172000000000009479 ) ;
#59841 = CARTESIAN_POINT ( 'NONE',  ( -23.07177167684715258, 305.3941994803996067, -8.883507296546389043 ) ) ;
#59843 = SURFACE_STYLE_FILL_AREA ( #101349 ) ;
#59844 =( BOUNDED_SURFACE ( )  B_SPLINE_SURFACE ( 3, 2, ( 
 ( #38012, #95677, #70346 ),
 ( #85473, #103765, #69297 ),
 ( #5599, #28320, #53620 ),
 ( #29903, #94641, #62789 ) ),
 .UNSPECIFIED., .F., .F., .T. ) 
 B_SPLINE_SURFACE_WITH_KNOTS ( ( 4, 4 ),
 ( 3, 3 ),
 ( 0.01539444365212263265, 0.01716277291646237796 ),
 ( 0.000000000000000000, 0.8371568960141710924 ),
 .UNSPECIFIED. ) 
 GEOMETRIC_REPRESENTATION_ITEM ( )  RATIONAL_B_SPLINE_SURFACE ( (
 ( 1.000000000000000000, 0.7548024220745215285, 0.9201425306416157746),
 ( 1.000000000000000000, 0.7704228259270500256, 0.9252298807393316560),
 ( 1.000000000000000000, 0.7855210260306706438, 0.9301471562782772651),
 ( 1.000000000000000000, 0.8001206121096573476, 0.9349020401062981822) ) ) 
 REPRESENTATION_ITEM ( '' )  SURFACE ( )  );
#59845 = CARTESIAN_POINT ( 'NONE',  ( -23.54446046888081412, 25.90716391019113729, -30.73896312393745234 ) ) ;
#59846 = ADVANCED_FACE ( 'NONE', ( #46498, #78856 ), #93992, .T. ) ;
#59847 = AXIS2_PLACEMENT_3D ( 'NONE', #79781, #103534, #5882 ) ;
#59848 = CARTESIAN_POINT ( 'NONE',  ( -43.78231969043007155, 434.3019752265992679, 13.50801524700046663 ) ) ;
#59849 = CARTESIAN_POINT ( 'NONE',  ( 7.849086896556030979, 70.34805173277894141, 4.999999999997544187 ) ) ;
#59850 = CONICAL_SURFACE ( 'NONE', #92542, 4.000000000000007105, 0.9599310885968835860 ) ;
#59851 = EDGE_LOOP ( 'NONE', ( #78203, #60793, #1963, #55292, #17936, #58591, #31193, #85487, #18262, #80407 ) ) ;
#59852 = DIRECTION ( 'NONE',  ( -1.000000000000000000, -3.469446951953614189E-16, 0.000000000000000000 ) ) ;
#59853 = CARTESIAN_POINT ( 'NONE',  ( -32.74881744694416597, 438.8767316144407573, 23.82550921047223014 ) ) ;
#59854 = VERTEX_POINT ( 'NONE', #11457 ) ;
#59855 = CARTESIAN_POINT ( 'NONE',  ( -4.959320189265015166, 53.54750726706794950, 8.497478219416661815 ) ) ;
#59856 = CARTESIAN_POINT ( 'NONE',  ( -35.10875260009915877, 305.4746754961840338, 12.42697074198600049 ) ) ;
#59857 = DIRECTION ( 'NONE',  ( 0.000000000000000000, -1.000000000000000000, 0.000000000000000000 ) ) ;
#59858 = CYLINDRICAL_SURFACE ( 'NONE', #48981, 9.999999999999998224 ) ;
#59859 = CARTESIAN_POINT ( 'NONE',  ( 5.656854249492380582, -24.31249999999999289, -5.656854249492379694 ) ) ;
#59860 = CARTESIAN_POINT ( 'NONE',  ( -35.95693203196412213, -24.51584111823862244, 33.83773937951661281 ) ) ;
#59861 = AXIS2_PLACEMENT_3D ( 'NONE', #13107, #5042, #99749 ) ;
#59862 = CARTESIAN_POINT ( 'NONE',  ( 15.39683056650771675, 44.03739065760672133, -5.597885347425531677 ) ) ;
#59863 = VERTEX_POINT ( 'NONE', #86978 ) ;
#59864 = CARTESIAN_POINT ( 'NONE',  ( 85.74124393967994706, -25.14955279151848089, 175.6267594608600007 ) ) ;
#59865 = CARTESIAN_POINT ( 'NONE',  ( 18.86650669486618881, 1.474610560812782335E-15, 0.000000000000000000 ) ) ;
#59866 = B_SPLINE_CURVE_WITH_KNOTS ( 'NONE', 3,
 ( #5797, #38208, #61945, #28524, #53302, #71586, #70012, #30103, #94296, #95888, #71068, #22013, #21488, #87796, #69488, #70550, #29079, #13878 ),
 .UNSPECIFIED., .F., .F.,
 ( 4, 2, 2, 2, 2, 2, 2, 2, 4 ),
 ( 0.007125849503216027947, 0.007630052828287933048, 0.008134256153359838148, 0.008638459478431743249, 0.009142662803503648350, 0.009646866128575553451, 0.01015106945364745855, 0.01065527277871936365, 0.01115947610379126875 ),
 .UNSPECIFIED. ) ;
#59867 = CARTESIAN_POINT ( 'NONE',  ( -16.64348903516517098, 45.60392139269950462, 6.657797401561654560 ) ) ;
#59868 = ORIENTED_EDGE ( 'NONE', *, *, #31393, .T. ) ;
#59869 = CARTESIAN_POINT ( 'NONE',  ( -90.29365882781722519, -60.15431844855726951, 56.70093613217015616 ) ) ;
#59870 = DIRECTION ( 'NONE',  ( 0.000000000000000000, 1.000000000000000000, 0.000000000000000000 ) ) ;
#59871 = CARTESIAN_POINT ( 'NONE',  ( -15.17227823171737100, -3.000000000000002665, -86.54073391196324394 ) ) ;
#59872 = CARTESIAN_POINT ( 'NONE',  ( -14.67571981731716946, -3.000000000000003109, -81.61772031542342631 ) ) ;
#59873 = AXIS2_PLACEMENT_3D ( 'NONE', #66463, #10727, #45257 ) ;
#59874 = CARTESIAN_POINT ( 'NONE',  ( -27.77336646784004515, -28.75003309865570600, -38.27452486851665014 ) ) ;
#59875 = EDGE_CURVE ( 'NONE', #22095, #1493, #24937, .T. ) ;
#59876 = CARTESIAN_POINT ( 'NONE',  ( 43.67329148970010522, -60.00000000000000711, 58.07957383741103286 ) ) ;
#59877 = CARTESIAN_POINT ( 'NONE',  ( 29.82243961713350444, -32.33238811108731170, 40.47282013833249437 ) ) ;
#59878 = CARTESIAN_POINT ( 'NONE',  ( 17.50000000000000711, 2.500000000000000444, 25.00000000000000000 ) ) ;
#59879 = CARTESIAN_POINT ( 'NONE',  ( 6.071286224229995199, -13.01951455890936415, 32.06810514125731260 ) ) ;
#59880 = EDGE_CURVE ( 'NONE', #4655, #71461, #94258, .T. ) ;
#59881 = CIRCLE ( 'NONE', #8194, 8.000000000000000000 ) ;
#59883 = CARTESIAN_POINT ( 'NONE',  ( -11.97156449694083946, 19.60962570912202096, -7.534720397356830190 ) ) ;
#59882 = CARTESIAN_POINT ( 'NONE',  ( -27.50695561155405855, -30.75843596377781708, 39.29379600943582318 ) ) ;
#59884 = CARTESIAN_POINT ( 'NONE',  ( 9.041223236726795065, 295.5670253727153067, -10.03755077321263123 ) ) ;
#59885 = CARTESIAN_POINT ( 'NONE',  ( 45.49982102694234953, 388.3127959276886827, 7.886590035822850453 ) ) ;
#59886 = FACE_OUTER_BOUND ( 'NONE', #55923, .T. ) ;
#59887 = CARTESIAN_POINT ( 'NONE',  ( 88.20199406385988539, 1.030564683017419500E-14, 0.000000000000000000 ) ) ;
#59888 = AXIS2_PLACEMENT_3D ( 'NONE', #69832, #4035, #19733 ) ;
#59889 = ORIENTED_EDGE ( 'NONE', *, *, #105393, .T. ) ;
#59890 = CARTESIAN_POINT ( 'NONE',  ( -43.71039113854124736, 464.8436985699681827, 11.74907638618257444 ) ) ;
#59891 = VECTOR ( 'NONE', #70474, 1000.000000000000000 ) ;
#59892 = CARTESIAN_POINT ( 'NONE',  ( 1.224646799147353256E-15, 80.00000000000000000, 10.00000000000000000 ) ) ;
#59893 = LINE ( 'NONE', #19463, #103192 ) ;
#59894 = CARTESIAN_POINT ( 'NONE',  ( 1.224646799147353454E-15, 2.999999999999993339, 10.00000000000000178 ) ) ;
#59895 = CARTESIAN_POINT ( 'NONE',  ( 21.81973643089116877, -21.77046491071190815, -29.53594053394288466 ) ) ;
#59896 = ADVANCED_FACE ( 'NONE', ( #4444 ), #35755, .T. ) ;
#59897 = ORIENTED_EDGE ( 'NONE', *, *, #83486, .F. ) ;
#59898 = B_SPLINE_CURVE_WITH_KNOTS ( 'NONE', 3,
 ( #28597, #12364, #21559, #29663 ),
 .UNSPECIFIED., .F., .F.,
 ( 4, 4 ),
 ( 1.040834085586084257E-17, 0.002002928617504300471 ),
 .UNSPECIFIED. ) ;
#59899 = CARTESIAN_POINT ( 'NONE',  ( -44.14911905790387436, 464.3766534541992996, 9.623404994945699897 ) ) ;
#59900 = CARTESIAN_POINT ( 'NONE',  ( 24.34999999999999787, 1.533819458162526451E-15, 0.000000000000000000 ) ) ;
#59901 = COLOUR_RGB ( '', 0.09019608, 0.27058824, 0.51372549) ;
#59902 = VECTOR ( 'NONE', #42523, 1000.000000000000000 ) ;
#59903 = ORIENTED_EDGE ( 'NONE', *, *, #82380, .F. ) ;
#59904 = EDGE_CURVE ( 'NONE', #80083, #38642, #6429, .T. ) ;
#59905 = CARTESIAN_POINT ( 'NONE',  ( 46.00000000000000000, 450.0000000000002274, 13.20242257375370976 ) ) ;
#59906 = DIRECTION ( 'NONE',  ( 1.000000000000000000, 0.000000000000000000, -0.000000000000000000 ) ) ;
#59907 = CARTESIAN_POINT ( 'NONE',  ( 17.61650669486618881, 4.898587196589411843E-16, -4.000000000000000888 ) ) ;
#59908 = CARTESIAN_POINT ( 'NONE',  ( -92.18718249619901428, -60.00000000000002132, 3.090949594964520042 ) ) ;
#59909 = COLOUR_RGB ( '', 0.09019608, 0.27058824, 0.51372549) ;
#59910 = FILL_AREA_STYLE_COLOUR ( '', #25687 ) ;
#59911 = AXIS2_PLACEMENT_3D ( 'NONE', #45839, #95984, #38814 ) ;
#59912 = CARTESIAN_POINT ( 'NONE',  ( 6.289692432696789126, 0.6629690750393447685, 6.828989928337166226 ) ) ;
#59913 = COLOUR_RGB ( '', 0.72549020, 0.75294118, 0.79215686) ;
#59914 = CARTESIAN_POINT ( 'NONE',  ( 31.02212611900126760, 360.5725590293961318, 22.12937154125974715 ) ) ;
#59915 = CARTESIAN_POINT ( 'NONE',  ( 40.71513924616333213, 459.9692486989943063, 1.994549889840352419 ) ) ;
#59917 = DIRECTION ( 'NONE',  ( -0.000000000000000000, 1.000000000000000000, -0.000000000000000000 ) ) ;
#59916 = CARTESIAN_POINT ( 'NONE',  ( 9.739726766100236688, -3.000000000000002665, -82.38252115499993522 ) ) ;
#59918 = CARTESIAN_POINT ( 'NONE',  ( -81.10093029976930268, -56.96112622887682164, 179.5505663864836947 ) ) ;
#59919 = EDGE_LOOP ( 'NONE', ( #59154, #10487, #54708, #29878, #46275 ) ) ;
#59920 = B_SPLINE_CURVE_WITH_KNOTS ( 'NONE', 3,
 ( #86555, #12613, #4544, #54127, #87070, #105363, #6119, #48695, #88645, #47109, #22880, #16342, #72455, #32021, #31503, #14737 ),
 .UNSPECIFIED., .F., .F.,
 ( 4, 2, 2, 2, 2, 2, 2, 4 ),
 ( 0.0004635561819301090036, 0.004837973112655610287, 0.009212390043381110324, 0.01796122390483211387, 0.02671005776628311568, 0.03545889162773411402, 0.05295655935063611763, 0.07045422707353812819 ),
 .UNSPECIFIED. ) ;
#59921 = PRESENTATION_STYLE_ASSIGNMENT (( #27036 ) ) ;
#59922 = ORIENTED_EDGE ( 'NONE', *, *, #95483, .F. ) ;
#59923 = VERTEX_POINT ( 'NONE', #70248 ) ;
#59924 = AXIS2_PLACEMENT_3D ( 'NONE', #33822, #44017, #68841 ) ;
#59925 = CARTESIAN_POINT ( 'NONE',  ( -29.68315524077004852, -1.200000000000000030E-05, -39.60535821593474282 ) ) ;
#59926 = CARTESIAN_POINT ( 'NONE',  ( -18.00094660900732535, -4.332661967061336661, 2.683237397145228798 ) ) ;
#59927 = CARTESIAN_POINT ( 'NONE',  ( 42.79755424932702113, 462.9502418795238441, 4.193817862676425534 ) ) ;
#59928 = ORIENTED_EDGE ( 'NONE', *, *, #4941, .F. ) ;
#59929 = VECTOR ( 'NONE', #105755, 1000.000000000000000 ) ;
#59930 = CARTESIAN_POINT ( 'NONE',  ( -72.51657142920434751, -41.65816625502668558, -21.93281331008283175 ) ) ;
#59931 = DIRECTION ( 'NONE',  ( -1.000000000000000000, -1.224606353822377258E-16, -0.000000000000000000 ) ) ;
#59932 = CARTESIAN_POINT ( 'NONE',  ( 6.928203230275510549, -10.00000000000000888, 4.000000000000000000 ) ) ;
#59933 = CARTESIAN_POINT ( 'NONE',  ( -7.619135598915495855, -61.82694632215322628, 2.449260492474798045 ) ) ;
#59934 = DIRECTION ( 'NONE',  ( 0.000000000000000000, 1.000000000000000000, 0.000000000000000000 ) ) ;
#59935 =( NAMED_UNIT ( * ) PLANE_ANGLE_UNIT ( ) SI_UNIT ( $, .RADIAN. ) );
#59936 = CARTESIAN_POINT ( 'NONE',  ( 0.000000000000000000, 0.000000000000000000, 0.000000000000000000 ) ) ;
#59937 = CARTESIAN_POINT ( 'NONE',  ( 89.80793189580856506, -29.99999999999993250, 26.19443836851201723 ) ) ;
#59938 = ADVANCED_FACE ( 'NONE', ( #93472 ), #54627, .T. ) ;
#59939 = CARTESIAN_POINT ( 'NONE',  ( -78.65018897216694427, -14.21045842199436571, 174.1869015730407000 ) ) ;
#59940 = CARTESIAN_POINT ( 'NONE',  ( -59.39683832124948282, -32.54576957150244709, 67.45736975201289454 ) ) ;
#59941 = AXIS2_PLACEMENT_3D ( 'NONE', #106468, #25060, #8839 ) ;
#59942 = ORIENTED_EDGE ( 'NONE', *, *, #23113, .F. ) ;
#59943 = SURFACE_STYLE_FILL_AREA ( #19508 ) ;
#59944 = VERTEX_POINT ( 'NONE', #11996 ) ;
#59945 = CARTESIAN_POINT ( 'NONE',  ( -103.8271769637748321, -45.26534194648037612, 179.3901650331305859 ) ) ;
#59946 = DIRECTION ( 'NONE',  ( 1.000000000000000000, 0.000000000000000000, 0.000000000000000000 ) ) ;
#59947 = CARTESIAN_POINT ( 'NONE',  ( -6.069413552714997273, 51.26876837080258298, 8.262085557432884642 ) ) ;
#59948 = AXIS2_PLACEMENT_3D ( 'NONE', #87543, #47583, #78901 ) ;
#59949 = CARTESIAN_POINT ( 'NONE',  ( 14.91338090413193918, 41.98696021714861359, -86.62221405687449760 ) ) ;
#59950 = ORIENTED_EDGE ( 'NONE', *, *, #38653, .F. ) ;
#59951 = CARTESIAN_POINT ( 'NONE',  ( -77.10094283560533768, -60.00000000000001421, 190.8546130424477667 ) ) ;
#59952 = CARTESIAN_POINT ( 'NONE',  ( -4.003587701499479401, -1.050376533302832094, 104.5574048719304443 ) ) ;
#59953 = CARTESIAN_POINT ( 'NONE',  ( -5.082755093536326818, -18.59375000204838457, 5.082755093536325042 ) ) ;
#59954 = CARTESIAN_POINT ( 'NONE',  ( 1.196618058419959393E-20, 36.30024107553216339, -29.75000000000000355 ) ) ;
#59955 = DIRECTION ( 'NONE',  ( 1.000000000000000000, 1.224606353822377258E-16, 0.000000000000000000 ) ) ;
#59956 = DIRECTION ( 'NONE',  ( 0.000000000000000000, 0.000000000000000000, 1.000000000000000000 ) ) ;
#59957 = CARTESIAN_POINT ( 'NONE',  ( -31.00389226642222340, 485.8187364282109115, 14.27494812388583512 ) ) ;
#59958 = CARTESIAN_POINT ( 'NONE',  ( 43.51882896341788864, 485.1238987962695433, -1.698943142573151599 ) ) ;
#59959 = CARTESIAN_POINT ( 'NONE',  ( 10.05948821411846872, -11.59943296283969971, 9.519649634508279945 ) ) ;
#59960 = CARTESIAN_POINT ( 'NONE',  ( 26.08349330513380337, 1.593028355512270567E-15, 0.000000000000000000 ) ) ;
#59961 = EDGE_CURVE ( 'NONE', #20128, #67515, #44928, .T. ) ;
#59962 = CARTESIAN_POINT ( 'NONE',  ( 16.64348903516523848, 43.47556584774768851, 6.657797401561421857 ) ) ;
#59963 = CARTESIAN_POINT ( 'NONE',  ( -29.62358194419280366, -36.01352107502461308, 32.38646520989296107 ) ) ;
#59964 = EDGE_CURVE ( 'NONE', #95526, #26814, #27130, .T. ) ;
#59965 = SURFACE_SIDE_STYLE ('',( #44837 ) ) ;
#59966 =( GEOMETRIC_REPRESENTATION_CONTEXT ( 3 ) GLOBAL_UNCERTAINTY_ASSIGNED_CONTEXT ( ( #76346 ) ) GLOBAL_UNIT_ASSIGNED_CONTEXT ( ( #70229, #35777, #11435 ) ) REPRESENTATION_CONTEXT ( 'NONE', 'WORKASPACE' ) );
#59967 = CARTESIAN_POINT ( 'NONE',  ( 42.40293126982735572, -18.78677026436083608, 35.79721704996967446 ) ) ;
#59968 = DIRECTION ( 'NONE',  ( 0.000000000000000000, -1.000000000000000000, 0.000000000000000000 ) ) ;
#59970 = VECTOR ( 'NONE', #85267, 1000.000000000000114 ) ;
#59969 = CARTESIAN_POINT ( 'NONE',  ( 13.50000000000000355, 7.794228634059978233, -1.205771365940065953 ) ) ;
#59971 = EDGE_CURVE ( 'NONE', #49207, #101661, #71895, .T. ) ;
#59972 = CARTESIAN_POINT ( 'NONE',  ( -94.82196696671130098, -38.48945518997164328, 201.2291303048070290 ) ) ;
#59973 = ORIENTED_EDGE ( 'NONE', *, *, #63726, .F. ) ;
#59974 = CARTESIAN_POINT ( 'NONE',  ( 84.49906736890430636, -38.35837216793694893, -23.28434020672035842 ) ) ;
#59975 = CARTESIAN_POINT ( 'NONE',  ( 61.60681234083082813, -59.99999999999999289, 86.74538964701946497 ) ) ;
#59976 = CARTESIAN_POINT ( 'NONE',  ( -19.17233543272195462, 49.75016788851922911, 61.61326636310676719 ) ) ;
#59977 = CARTESIAN_POINT ( 'NONE',  ( -7.436486834768465393, 40.68079689291138124, -59.06589860020129379 ) ) ;
#59978 = CARTESIAN_POINT ( 'NONE',  ( 9.999999999999998224, 15.00000000000000000, -1.734723475976806897E-15 ) ) ;
#59979 = CARTESIAN_POINT ( 'NONE',  ( -7.681258945454893382E-14, -1.200000000000000030E-05, -38.25000000000000000 ) ) ;
#59980 = CARTESIAN_POINT ( 'NONE',  ( -22.55472503455973410, 305.4464812988970834, 9.065450513355358453 ) ) ;
#59981 = LINE ( 'NONE', #92843, #88349 ) ;
#59982 = VECTOR ( 'NONE', #48483, 1000.000000000000114 ) ;
#59983 = CARTESIAN_POINT ( 'NONE',  ( 108.9514231372410507, -60.00000000000000711, 193.8007399767856498 ) ) ;
#59984 = FACE_OUTER_BOUND ( 'NONE', #88404, .T. ) ;
#59985 = EDGE_CURVE ( 'NONE', #62536, #73940, #8128, .T. ) ;
#59986 =( BOUNDED_SURFACE ( )  B_SPLINE_SURFACE ( 2, 3, ( 
 ( #52167, #85080, #19862, #92094, #29026, #52696, #55342, #46737, #79626, #105500 ),
 ( #31124, #88793, #5744, #88271, #96886, #45686, #38663, #6800, #54269, #95830 ),
 ( #87211, #22501, #95302, #37632, #70495, #47255, #87744, #103386, #14882, #62936 ) ),
 .UNSPECIFIED., .F., .F., .F. ) 
 B_SPLINE_SURFACE_WITH_KNOTS ( ( 3, 3 ),
 ( 4, 2, 2, 2, 4 ),
 ( 0.000000000000000000, 1.000000000000000000 ),
 ( 0.000000000000000000, 0.01533609458748647764, 0.03067218917497295527, 0.04600828376245943291, 0.06134437834994591054 ),
 .UNSPECIFIED. ) 
 GEOMETRIC_REPRESENTATION_ITEM ( )  RATIONAL_B_SPLINE_SURFACE ( (
 ( 1.000000000000000000, 1.000000000000000000, 1.000000000000000000, 1.000000000000000000, 1.000000000000000000, 1.000000000000000000, 1.000000000000000000, 1.000000000000000000, 1.000000000000000000, 1.000000000000000000),
 ( 1.857142857142858317, 1.857142857142858317, 1.857142857142858317, 1.857142857142858317, 1.857142857142858317, 1.857142857142858317, 1.857142857142858317, 1.857142857142858317, 1.857142857142858317, 1.857142857142858317),
 ( 1.000000000000000000, 1.000000000000000000, 1.000000000000000000, 1.000000000000000000, 1.000000000000000000, 1.000000000000000000, 1.000000000000000000, 1.000000000000000000, 1.000000000000000000, 1.000000000000000000) ) ) 
 REPRESENTATION_ITEM ( '' )  SURFACE ( )  );
#59987 = LINE ( 'NONE', #69648, #68047 ) ;
#59988 = VERTEX_POINT ( 'NONE', #45453 ) ;
#59989 = CARTESIAN_POINT ( 'NONE',  ( 0.9999999999999940048, -50.00000000000000000, 101.0455488498966758 ) ) ;
#59990 = CARTESIAN_POINT ( 'NONE',  ( -80.70619913987853522, -30.00000000000000711, -12.62841071653336122 ) ) ;
#59991 = ORIENTED_EDGE ( 'NONE', *, *, #10236, .T. ) ;
#59993 = CARTESIAN_POINT ( 'NONE',  ( 42.80417301746438596, 434.8807528697740281, 8.723038671912201281 ) ) ;
#59992 = CARTESIAN_POINT ( 'NONE',  ( -46.16323595244445954, -38.31912878070681217, 60.03967466318334800 ) ) ;
#59994 = CYLINDRICAL_SURFACE ( 'NONE', #49403, 9.999999999999994671 ) ;
#59995 = CARTESIAN_POINT ( 'NONE',  ( 25.78981311250976916, 306.9324440203532731, 10.64094596872064358 ) ) ;
#59997 = CARTESIAN_POINT ( 'NONE',  ( 9.482856158761276077, 27.55692884145275201, 3.177891129109640556 ) ) ;
#59996 = AXIS2_PLACEMENT_3D ( 'NONE', #89492, #82453, #9609 ) ;
#59998 = CIRCLE ( 'NONE', #72050, 4.000000000000001776 ) ;
#59999 = CARTESIAN_POINT ( 'NONE',  ( 7.188101187500000044, -18.03125000204838457, 0.000000000000000000 ) ) ;
#60000 = CONICAL_SURFACE ( 'NONE', #46193, 5.000000000000010658, 0.9599310885968697082 ) ;
#60001 = CARTESIAN_POINT ( 'NONE',  ( -11.68767211932491179, -5.000000000000002665, -88.14097461399494193 ) ) ;
#60002 = UNCERTAINTY_MEASURE_WITH_UNIT (LENGTH_MEASURE( 1.000000000000000082E-05 ), #2939, 'distance_accuracy_value', 'NONE');
#60003 = DIRECTION ( 'NONE',  ( 0.000000000000000000, 0.000000000000000000, 1.000000000000000000 ) ) ;
#60005 = EDGE_LOOP ( 'NONE', ( #97322, #38025, #78761, #60287 ) ) ;
#60004 = FILL_AREA_STYLE ('',( #50275 ) ) ;
#60006 = CARTESIAN_POINT ( 'NONE',  ( 84.55948629711632236, -22.11309726741666992, 156.8062503804032417 ) ) ;
#60007 = DIRECTION ( 'NONE',  ( -1.000000000000000000, -1.224606353822377258E-16, -0.000000000000000000 ) ) ;
#60008 = CARTESIAN_POINT ( 'NONE',  ( 6.837824896291513355, -3.947820044545448326, -6.564402953523719830 ) ) ;
#60009 = ORIENTED_EDGE ( 'NONE', *, *, #66231, .F. ) ;
#60010 = CARTESIAN_POINT ( 'NONE',  ( -32.20052651335440430, 485.9558351764622444, 4.953748807553719935 ) ) ;
#60011 = CARTESIAN_POINT ( 'NONE',  ( 6.692326732991420724E-21, 18.87382441218278828, -49.25000000000000000 ) ) ;
#60012 = DIRECTION ( 'NONE',  ( 0.9861333108788017388, 0.1659550938513568163, 0.000000000000000000 ) ) ;
#60013 = LINE ( 'NONE', #100431, #95123 ) ;
#60014 = CARTESIAN_POINT ( 'NONE',  ( -5.475947152006328977, 253.1621773010911909, 2.462898245435118039 ) ) ;
#60015 = CARTESIAN_POINT ( 'NONE',  ( 1.231285353216601708, 16.44838349168128033, 50.25257280200809618 ) ) ;
#60016 = ORIENTED_EDGE ( 'NONE', *, *, #72214, .F. ) ;
#60017 = EDGE_CURVE ( 'NONE', #58745, #55679, #103672, .T. ) ;
#60018 = AXIS2_PLACEMENT_3D ( 'NONE', #52439, #2286, #44915 ) ;
#60019 = CARTESIAN_POINT ( 'NONE',  ( 22.33349330513380337, 1.593028355512270567E-15, 0.000000000000000000 ) ) ;
#60020 = DIRECTION ( 'NONE',  ( 0.000000000000000000, 0.000000000000000000, 1.000000000000000000 ) ) ;
#60021 = CARTESIAN_POINT ( 'NONE',  ( 3.400000000000000355, 0.000000000000000000, -7.554475477074167777 ) ) ;
#60022 = EDGE_CURVE ( 'NONE', #28485, #22572, #52455, .T. ) ;
#60023 = DIRECTION ( 'NONE',  ( 0.000000000000000000, 0.000000000000000000, 1.000000000000000000 ) ) ;
#60024 = COLOUR_RGB ( '', 0.40784314, 0.44705882, 0.49803922) ;
#60025 = CARTESIAN_POINT ( 'NONE',  ( 2.977408999572651815, -26.93750000204838457, 7.188101187500000933 ) ) ;
#60026 = FACE_OUTER_BOUND ( 'NONE', #31388, .T. ) ;
#60027 = CARTESIAN_POINT ( 'NONE',  ( 1.058054217398698871, -6.894685612232814620, -0.3576316571898649488 ) ) ;
#60028 = CARTESIAN_POINT ( 'NONE',  ( 42.78577943797455418, 436.7963452923233376, 20.33379556194504900 ) ) ;
#60029 = CONTEXT_DEPENDENT_SHAPE_REPRESENTATION ( #8672, #101754 ) ;
#60030 = ORIENTED_EDGE ( 'NONE', *, *, #50364, .F. ) ;
#60031 = CARTESIAN_POINT ( 'NONE',  ( 39.64792090968624905, 485.8593029974497881, -5.004078333543738211 ) ) ;
#60032 = CARTESIAN_POINT ( 'NONE',  ( 18.86650669486618881, 4.898587196589413815E-16, -4.000000000000000888 ) ) ;
#60033 = CARTESIAN_POINT ( 'NONE',  ( -5.603881765357392908, 5.085926155681621097, -5.000000000000000000 ) ) ;
#60034 = CARTESIAN_POINT ( 'NONE',  ( 96.86866073052655679, -2.002967142162725287E-29, 5.000000000000011546 ) ) ;
#60035 = ADVANCED_FACE ( 'NONE', ( #19622 ), #85370, .F. ) ;
#60036 = ORIENTED_EDGE ( 'NONE', *, *, #1396, .T. ) ;
#60037 = AXIS2_PLACEMENT_3D ( 'NONE', #97401, #89342, #81742 ) ;
#60038 = CARTESIAN_POINT ( 'NONE',  ( 35.99392181574479821, 473.1311165566888235, 18.08664358306795705 ) ) ;
#60039 = CARTESIAN_POINT ( 'NONE',  ( 4.080003621828020677, 50.00000000000000000, -97.51073764067400873 ) ) ;
#60040 = ORIENTED_EDGE ( 'NONE', *, *, #18625, .T. ) ;
#60041 = COLOUR_RGB ( '', 0.40784314, 0.44705882, 0.49803922) ;
#60042 = CARTESIAN_POINT ( 'NONE',  ( 31.32079490055140170, 437.4203400336787126, 20.45846139775142802 ) ) ;
#60043 = CARTESIAN_POINT ( 'NONE',  ( -5.656854249492379694, -22.62500000409676915, -5.656854249492380582 ) ) ;
#60044 = CARTESIAN_POINT ( 'NONE',  ( 9.483056940782029542, 102.5561220989342388, -3.177305548492599829 ) ) ;
#60045 = CARTESIAN_POINT ( 'NONE',  ( 36.58412289726538802, 25.86933424275333238, 12.99557124040957490 ) ) ;
#60046 = CARTESIAN_POINT ( 'NONE',  ( -90.36280461092469807, -60.00000000000002132, 202.0446456219443689 ) ) ;
#60047 = CARTESIAN_POINT ( 'NONE',  ( 17.49999999999959144, 49.99999999999815259, 59.82664205501160382 ) ) ;
#60048 = CARTESIAN_POINT ( 'NONE',  ( 10.28624191511773844, 43.25714326066793092, -15.40779740156427202 ) ) ;
#60050 = AXIS2_PLACEMENT_3D ( 'NONE', #8438, #74231, #33275 ) ;
#60049 = FACE_OUTER_BOUND ( 'NONE', #18571, .T. ) ;
#60051 = ADVANCED_FACE ( 'NONE', ( #39485 ), #94319, .T. ) ;
#60052 = CARTESIAN_POINT ( 'NONE',  ( 24.83349330513380693, 1.593028355512270962E-15, 0.000000000000000000 ) ) ;
#60053 = CONICAL_SURFACE ( 'NONE', #49694, 3.309500000000001663, 0.9599310885968770357 ) ;
#60054 = CARTESIAN_POINT ( 'NONE',  ( -83.08181241973555586, -57.30282313777087921, 188.7210544118925668 ) ) ;
#60055 = CARTESIAN_POINT ( 'NONE',  ( -4.661090069372093581, 53.64050244245383681, -8.373412985213160908 ) ) ;
#60056 = ORIENTED_EDGE ( 'NONE', *, *, #15135, .T. ) ;
#60057 = CARTESIAN_POINT ( 'NONE',  ( -1.469576158976823947E-15, -26.37499999999999645, 8.000000000000000000 ) ) ;
#60058 = CARTESIAN_POINT ( 'NONE',  ( -83.05971922487898951, -37.81386008383282871, -1.851040229428762451 ) ) ;
#60059 = AXIS2_PLACEMENT_3D ( 'NONE', #55778, #56308, #89248 ) ;
#60060 = CARTESIAN_POINT ( 'NONE',  ( -4.698741327953603886, 7.940184299454766226, -5.000000000000000888 ) ) ;
#60061 = CARTESIAN_POINT ( 'NONE',  ( 27.59999999999999787, -4.171999999999999709, 5.616230220889763424E-16 ) ) ;
#60062 = DIRECTION ( 'NONE',  ( -1.000000000000000000, -0.000000000000000000, -0.000000000000000000 ) ) ;
#60063 = CARTESIAN_POINT ( 'NONE',  ( -90.56128410203886858, 42.00000000000000000, 11.85444436786840328 ) ) ;
#60064 = PRESENTATION_LAYER_ASSIGNMENT (  '', '', ( #1497 ) ) ;
#60065 = CARTESIAN_POINT ( 'NONE',  ( 69.85392978727392688, -60.00000000000004263, 155.8703566448706113 ) ) ;
#60066 = CARTESIAN_POINT ( 'NONE',  ( -95.02173393737120932, -60.00000000000007105, -3.234914688897275070 ) ) ;
#60067 = CARTESIAN_POINT ( 'NONE',  ( -72.21540169979105883, -22.11768858647452873, 98.80481924642175784 ) ) ;
#60068 = ORIENTED_EDGE ( 'NONE', *, *, #34746, .F. ) ;
#60069 = CARTESIAN_POINT ( 'NONE',  ( 75.56757797150578426, -14.21045842199434439, 141.5459454228812319 ) ) ;
#60070 = CARTESIAN_POINT ( 'NONE',  ( -51.64414839223339015, 40.83902574785438588, 39.58156097992099376 ) ) ;
#60071 = EDGE_LOOP ( 'NONE', ( #99064, #48919, #3812, #58007, #97681, #35642 ) ) ;
#60072 = CARTESIAN_POINT ( 'NONE',  ( 33.76319574111100508, -59.99999999999999289, 48.40639849824221130 ) ) ;
#60073 = EDGE_LOOP ( 'NONE', ( #41527, #78921, #36799, #104886, #42004, #42976, #37580, #82642 ) ) ;
#60074 = CARTESIAN_POINT ( 'NONE',  ( 15.90614609307868399, -3.157894736842107530, 14.66382285868950675 ) ) ;
#60075 = CARTESIAN_POINT ( 'NONE',  ( -7.188101187500000933, -26.37500000204838457, -2.977408999572651371 ) ) ;
#60076 = CARTESIAN_POINT ( 'NONE',  ( -5.909155701201248334, -6.137383198112712712, 1.073778020691672275 ) ) ;
#60077 = EDGE_LOOP ( 'NONE', ( #75456, #16157, #78668, #71156 ) ) ;
#60078 = DIRECTION ( 'NONE',  ( 1.000000000000000000, 0.000000000000000000, 0.000000000000000000 ) ) ;
#60079 = EDGE_LOOP ( 'NONE', ( #73056, #74864, #95390, #106631 ) ) ;
#60080 = CARTESIAN_POINT ( 'NONE',  ( -8.169585525225413036, 41.99999999999999289, -72.41994148081866456 ) ) ;
#60081 = CARTESIAN_POINT ( 'NONE',  ( -43.00000000000000000, 450.0000000000002274, 13.20242257375370976 ) ) ;
#60082 = CARTESIAN_POINT ( 'NONE',  ( -64.82079882110336655, -60.00000000003903722, 127.4591902977199567 ) ) ;
#60083 = CARTESIAN_POINT ( 'NONE',  ( 33.96241883181121324, 322.0929539439751466, -5.546615967778726564 ) ) ;
#60084 = CARTESIAN_POINT ( 'NONE',  ( 5.082755093536325930, -11.46875000204838635, -5.082755093536325042 ) ) ;
#60085 = CARTESIAN_POINT ( 'NONE',  ( 29.83349330513380337, 1.593028355512270567E-15, 0.000000000000000000 ) ) ;
#60086 = CYLINDRICAL_SURFACE ( 'NONE', #24068, 8.000000000000000000 ) ;
#60087 = DIRECTION ( 'NONE',  ( -0.000000000000000000, -0.000000000000000000, 1.000000000000000000 ) ) ;
#60088 =( NAMED_UNIT ( * ) PLANE_ANGLE_UNIT ( ) SI_UNIT ( $, .RADIAN. ) );
#60089 = CARTESIAN_POINT ( 'NONE',  ( -12.49018806437142715, -3.466428895744098515, -13.79302967849227457 ) ) ;
#60090 = CARTESIAN_POINT ( 'NONE',  ( 39.62826361664807706, 437.5693818447161334, 4.806172978292440945 ) ) ;
#60091 = ADVANCED_FACE ( 'NONE', ( #104191, #79915, #31411, #72876, #31926 ), #97661, .T. ) ;
#60092 = ORIENTED_EDGE ( 'NONE', *, *, #50399, .T. ) ;
#60093 = CARTESIAN_POINT ( 'NONE',  ( 4.902312018372324331, -3.082176157930677451, 103.3400275729950835 ) ) ;
#60094 = AXIS2_PLACEMENT_3D ( 'NONE', #24731, #5858, #7438 ) ;
#60096 = CARTESIAN_POINT ( 'NONE',  ( 32.10088869842463311, -25.61432814849804984, 31.36898226149570235 ) ) ;
#60095 = CARTESIAN_POINT ( 'NONE',  ( -3.685905252139206834, -48.95891067205180747, 104.2837900504744368 ) ) ;
#60097 =( NAMED_UNIT ( * ) PLANE_ANGLE_UNIT ( ) SI_UNIT ( $, .RADIAN. ) );
#60098 = ORIENTED_EDGE ( 'NONE', *, *, #93246, .F. ) ;
#60099 = EDGE_CURVE ( 'NONE', #33845, #98395, #47772, .T. ) ;
#60100 = CARTESIAN_POINT ( 'NONE',  ( 14.83349330513380337, -7.703719777548943412E-31, 4.000000000000001776 ) ) ;
#60101 = AXIS2_PLACEMENT_3D ( 'NONE', #6607, #39534, #40048 ) ;
#60102 = EDGE_CURVE ( 'NONE', #86885, #6164, #61606, .T. ) ;
#60103 = AXIS2_PLACEMENT_3D ( 'NONE', #77916, #45031, #18639 ) ;
#60104 = ORIENTED_EDGE ( 'NONE', *, *, #31054, .F. ) ;
#60105 = CARTESIAN_POINT ( 'NONE',  ( 9.349999999999997868, -3.309499999999999886, 4.475777889183790779E-16 ) ) ;
#60106 = CYLINDRICAL_SURFACE ( 'NONE', #21667, 4.000000000000001776 ) ;
#60107 = CARTESIAN_POINT ( 'NONE',  ( -44.24885999147608828, 485.2873706794252371, 1.656249348737429683 ) ) ;
#60108 = CARTESIAN_POINT ( 'NONE',  ( 61.37206225042174879, 6.856755485862130937E-15, 0.000000000000000000 ) ) ;
#60109 = DIRECTION ( 'NONE',  ( 1.000000000000000000, 0.000000000000000000, 0.000000000000000000 ) ) ;
#60110 = EDGE_LOOP ( 'NONE', ( #3734, #12070, #102450, #26292, #8995 ) ) ;
#60111 = CARTESIAN_POINT ( 'NONE',  ( 81.02257714386620080, -59.99999999999999289, -27.32370658691883136 ) ) ;
#60112 = CARTESIAN_POINT ( 'NONE',  ( 32.70293721676337384, 464.5899875799881897, 16.75272535697877885 ) ) ;
#60113 = EDGE_CURVE ( 'NONE', #103513, #9744, #102854, .T. ) ;
#60114 = DIRECTION ( 'NONE',  ( -1.000000000000000000, 0.000000000000000000, 0.000000000000000000 ) ) ;
#60115 = CARTESIAN_POINT ( 'NONE',  ( -6.924711584187146940, 40.92328497002484511, -70.90711766174086961 ) ) ;
#60116 = CARTESIAN_POINT ( 'NONE',  ( -46.86404804693351878, 18.87323894068644137, -15.14441118170511835 ) ) ;
#60117 = ORIENTED_EDGE ( 'NONE', *, *, #97004, .F. ) ;
#60118 = CARTESIAN_POINT ( 'NONE',  ( -106.9243038568529869, -29.99999999998815170, 191.8946513620529970 ) ) ;
#60119 = ORIENTED_EDGE ( 'NONE', *, *, #32524, .F. ) ;
#60120 = AXIS2_PLACEMENT_3D ( 'NONE', #83182, #24460, #15793 ) ;
#60121 = VERTEX_POINT ( 'NONE', #80970 ) ;
#60122 = CARTESIAN_POINT ( 'NONE',  ( 0.000000000000000000, -6.928203230275504332, 4.000000000000007105 ) ) ;
#60123 = CARTESIAN_POINT ( 'NONE',  ( 6.692588830498428010, -3.932766476276041256, -6.892929031562515796 ) ) ;
#60124 = CARTESIAN_POINT ( 'NONE',  ( 7.922281120364393914, 4.573931137438267847, -8.047472243342932430 ) ) ;
#60125 = FACE_OUTER_BOUND ( 'NONE', #65223, .T. ) ;
#60126 = CARTESIAN_POINT ( 'NONE',  ( 85.13361819880341841, -52.75518388885414822, -12.49988904550194135 ) ) ;
#60127 = CARTESIAN_POINT ( 'NONE',  ( -38.29550411296874302, 308.8267097740885561, 1.300001675379448551 ) ) ;
#60128 = FACE_OUTER_BOUND ( 'NONE', #22719, .T. ) ;
#60129 = CARTESIAN_POINT ( 'NONE',  ( -17.59737154672216164, 45.00000000000000000, 63.11098746908783141 ) ) ;
#60130 = CARTESIAN_POINT ( 'NONE',  ( 59.89460441624491693, 6.975173280561618775E-15, 0.000000000000000000 ) ) ;
#60131 = CLOSED_SHELL ( 'NONE', ( #92536, #37525, #51526, #1341, #61836, #18327, #104446, #22180, #80840, #3605, #100451, #10332, #81057, #76232, #66837, #83214, #43171, #97407, #83026, #11692, #42206, #11960, #4049, #37230, #17785, #22819, #45648, #52901, #74681, #39301, #98866, #99633, #77930, #15803, #29571, #69617, #54079, #45805, #14106, #72932, #31718, #22427, #101611, #96719, #98518, #78322, #33243, #65606, #92608, #95968, #75886, #13251, #86094, #39801, #22559, #69158, #8365, #9661, #10276, #6297, #64886, #104567, #7331, #60625, #6831, #83666, #106412, #8942, #99717, #99162, #11818, #31536 ) ) ;
#60132 = ORIENTED_EDGE ( 'NONE', *, *, #52997, .F. ) ;
#60133 = CARTESIAN_POINT ( 'NONE',  ( -6.815962252199544658, 1.383413844632507717, -6.173425845474766582 ) ) ;
#60134 = VERTEX_POINT ( 'NONE', #47015 ) ;
#60135 = CARTESIAN_POINT ( 'NONE',  ( 48.69302399950104387, 8.421789753111580623, -16.66702170536975913 ) ) ;
#60136 = AXIS2_PLACEMENT_3D ( 'NONE', #59557, #35298, #51442 ) ;
#60138 = ORIENTED_EDGE ( 'NONE', *, *, #86349, .F. ) ;
#60137 = CARTESIAN_POINT ( 'NONE',  ( 11.08349330513380160, 4.000000000000003553, 0.000000000000000000 ) ) ;
#60139 = CARTESIAN_POINT ( 'NONE',  ( 73.66839973556383825, -56.84817161155148568, 127.7600820225604537 ) ) ;
#60140 = CIRCLE ( 'NONE', #89443, 5.000000000000002665 ) ;
#60141 = ORIENTED_EDGE ( 'NONE', *, *, #72182, .T. ) ;
#60142 = CARTESIAN_POINT ( 'NONE',  ( 3.116130668582941965, -49.50076467470627506, 40.80225857358325925 ) ) ;
#60143 = CARTESIAN_POINT ( 'NONE',  ( -37.62251730745840916, 437.3427388312646258, 4.535622330043208805 ) ) ;
#60144 = CARTESIAN_POINT ( 'NONE',  ( 5.082755093536325930, -26.46875000204838813, -5.082755093536325042 ) ) ;
#60145 = CARTESIAN_POINT ( 'NONE',  ( -104.7047915100801987, -57.67116545479915857, 96.89679091199744221 ) ) ;
#60146 = EDGE_LOOP ( 'NONE', ( #21882, #104956, #61943, #104792, #98169, #21332 ) ) ;
#60147 = PRESENTATION_STYLE_ASSIGNMENT (( #59597 ) ) ;
#60148 = CARTESIAN_POINT ( 'NONE',  ( -25.23529853069842588, 43.63852619275398581, -75.80720028947999367 ) ) ;
#60149 = CARTESIAN_POINT ( 'NONE',  ( 104.1886421374867382, -52.71694715348233728, 185.8499235192266497 ) ) ;
#60150 = AXIS2_PLACEMENT_3D ( 'NONE', #2538, #1998, #34946 ) ;
#60151 = CARTESIAN_POINT ( 'NONE',  ( -9.381394091586573225, 82.98650394418388032, 3.465950112474263989 ) ) ;
#60152 = EDGE_CURVE ( 'NONE', #57765, #52893, #56695, .T. ) ;
#60153 = CARTESIAN_POINT ( 'NONE',  ( 48.76595811598669883, 13.46359178982426563, -16.61915017902559910 ) ) ;
#60154 = CARTESIAN_POINT ( 'NONE',  ( 5.656854249492380582, -17.00000000409676915, -5.656854249492379694 ) ) ;
#60155 = CARTESIAN_POINT ( 'NONE',  ( 16.75187969033571989, 36.38380281757302726, 24.30698433968583316 ) ) ;
#60156 = VECTOR ( 'NONE', #17696, 1000.000000000000000 ) ;
#60157 = CARTESIAN_POINT ( 'NONE',  ( 9.699189539447139907, 246.8230777175328399, -2.444343703917226218 ) ) ;
#60158 = CARTESIAN_POINT ( 'NONE',  ( 10.50000000000000711, -5.000000000000000000, -77.33514508527181874 ) ) ;
#60159 = B_SPLINE_CURVE_WITH_KNOTS ( 'NONE', 3,
 ( #83853, #84929, #43410, #84400 ),
 .UNSPECIFIED., .F., .F.,
 ( 4, 4 ),
 ( 0.0008553712708089381608, 0.02105700498847944482 ),
 .UNSPECIFIED. ) ;
#60160 = DIRECTION ( 'NONE',  ( 0.9999999999999998890, 1.110223024625156540E-16, 0.000000000000000000 ) ) ;
#60161 = CARTESIAN_POINT ( 'NONE',  ( 7.074371941841917533, -30.00000000000001066, -1.589546009095287982 ) ) ;
#60162 = ORIENTED_EDGE ( 'NONE', *, *, #8255, .T. ) ;
#60163 = CARTESIAN_POINT ( 'NONE',  ( 43.62595639791993563, 434.3202349548960797, 14.43462880160996953 ) ) ;
#60164 = CARTESIAN_POINT ( 'NONE',  ( 0.07800279179579312772, 13.70447791526912873, 49.25000000000000711 ) ) ;
#60165 = CARTESIAN_POINT ( 'NONE',  ( -89.27843304015721060, -30.00000000000000711, 189.0996331995533524 ) ) ;
#60166 = EDGE_CURVE ( 'NONE', #81897, #99736, #23652, .T. ) ;
#60167 = MECHANICAL_DESIGN_GEOMETRIC_PRESENTATION_REPRESENTATION (  '', ( #63616 ), #80756 ) ;
#60168 = EDGE_LOOP ( 'NONE', ( #84388, #32780, #79983, #6956, #30372 ) ) ;
#60169 = AXIS2_PLACEMENT_3D ( 'NONE', #25269, #35491, #90503 ) ;
#60170 = CYLINDRICAL_SURFACE ( 'NONE', #20420, 4.000000000000000888 ) ;
#60171 = CARTESIAN_POINT ( 'NONE',  ( 86.12462942110903441, -57.57595555861249181, 202.7575993840488593 ) ) ;
#60173 = DIRECTION ( 'NONE',  ( 0.000000000000000000, -1.000000000000000000, 0.000000000000000000 ) ) ;
#60172 = CARTESIAN_POINT ( 'NONE',  ( -15.47474416541280995, 2.749750016663679464, 1.674624973627630187 ) ) ;
#60174 = CARTESIAN_POINT ( 'NONE',  ( 57.07624943773998893, -36.90585292959303132, -34.83277310691430984 ) ) ;
#60175 = CARTESIAN_POINT ( 'NONE',  ( 9.500000000000007105, -5.000000000000000000, -68.91429205785459544 ) ) ;
#60176 = CARTESIAN_POINT ( 'NONE',  ( 65.52222222222222570, -3.309500000000000774, 4.475777889183797681E-16 ) ) ;
#60177 = CARTESIAN_POINT ( 'NONE',  ( -41.75932222925875692, -60.00000000000000711, 54.76167985618531731 ) ) ;
#60178 = CARTESIAN_POINT ( 'NONE',  ( 100.6222222222222200, 4.172000000000019249, 5.109226446042768454E-16 ) ) ;
#60179 = AXIS2_PLACEMENT_3D ( 'NONE', #13741, #45083, #87660 ) ;
#60180 = ADVANCED_FACE ( 'NONE', ( #88031 ), #18489, .F. ) ;
#60181 = CARTESIAN_POINT ( 'NONE',  ( -23.38163988261910831, 48.00000000000000000, 60.94087333798633210 ) ) ;
#60182 = CARTESIAN_POINT ( 'NONE',  ( -85.01242186521922406, -61.08653189438597764, 193.5097775706131245 ) ) ;
#60183 = ORIENTED_EDGE ( 'NONE', *, *, #9605, .F. ) ;
#60184 = CARTESIAN_POINT ( 'NONE',  ( 4.226620391573794039E-15, 29.56666008184760130, 34.51297463494397988 ) ) ;
#60185 = CARTESIAN_POINT ( 'NONE',  ( -1.016815886943048142, -53.40265724237126932, 32.79009283333092384 ) ) ;
#60186 = CARTESIAN_POINT ( 'NONE',  ( 0.000000000000000000, 0.000000000000000000, 0.000000000000000000 ) ) ;
#60187 = CARTESIAN_POINT ( 'NONE',  ( -1.450084842030770593, -49.97618070428583081, 101.4852282631765661 ) ) ;
#60189 = CARTESIAN_POINT ( 'NONE',  ( -7.938137630668183675, 54.17496235756595979, 1.684399108843077864 ) ) ;
#60188 = DIRECTION ( 'NONE',  ( -0.000000000000000000, -0.000000000000000000, -1.000000000000000000 ) ) ;
#60190 = VERTEX_POINT ( 'NONE', #48070 ) ;
#60191 = CARTESIAN_POINT ( 'NONE',  ( -36.73878763022428728, 390.5162264143924062, 5.892410784837893267 ) ) ;
#60192 = CARTESIAN_POINT ( 'NONE',  ( 39.74142865886215503, 490.7355817146180357, 11.79841936045182926 ) ) ;
#60193 = VECTOR ( 'NONE', #4800, 1000.000000000000114 ) ;
#60194 = CARTESIAN_POINT ( 'NONE',  ( 4.988960626530190971E-15, 27.29656849860388235, 40.75000000000000000 ) ) ;
#60195 = CARTESIAN_POINT ( 'NONE',  ( 104.9555555555555486, -4.171999999999998820, 5.616230220889773285E-16 ) ) ;
#60196 = CARTESIAN_POINT ( 'NONE',  ( 20.49977525862258076, 302.8459220885799823, -10.00124997875689203 ) ) ;
#60197 = CARTESIAN_POINT ( 'NONE',  ( 22.91651842568165165, 295.0901107613288445, -9.949346074078587066 ) ) ;
#60198 = DIRECTION ( 'NONE',  ( 0.000000000000000000, 0.000000000000000000, 1.000000000000000000 ) ) ;
#60199 = CARTESIAN_POINT ( 'NONE',  ( 96.66679845751455957, -59.99999999999993605, 43.68127598107410847 ) ) ;
#60200 = CARTESIAN_POINT ( 'NONE',  ( -82.94229579353957149, -29.08663412309721608, 153.6279066531906494 ) ) ;
#60201 = ORIENTED_EDGE ( 'NONE', *, *, #22891, .T. ) ;
#60202 = CARTESIAN_POINT ( 'NONE',  ( 88.48689482502902592, 1.016364837396684119E-14, 0.000000000000000000 ) ) ;
#60203 = CARTESIAN_POINT ( 'NONE',  ( 0.000000000000000000, 47.29617335651134624, 13.27631144943088515 ) ) ;
#60204 = CARTESIAN_POINT ( 'NONE',  ( 14.12267823962728386, -57.67128902998698692, 41.72226490217841643 ) ) ;
#60205 = DIRECTION ( 'NONE',  ( 0.000000000000000000, -0.3420201433256725987, -0.9396926207859068736 ) ) ;
#60206 = CARTESIAN_POINT ( 'NONE',  ( 41.63141214886829999, 315.3601224161185428, -5.077054131032955553 ) ) ;
#60207 = COLOUR_RGB ( '', 0.31764706, 0.68627451, 0.89019608) ;
#60208 = DIRECTION ( 'NONE',  ( 0.000000000000000000, -1.000000000000000000, 0.000000000000000000 ) ) ;
#60209 = ORIENTED_EDGE ( 'NONE', *, *, #43432, .T. ) ;
#60210 = UNCERTAINTY_MEASURE_WITH_UNIT (LENGTH_MEASURE( 1.000000000000000082E-05 ), #39591, 'distance_accuracy_value', 'NONE');
#60211 = CARTESIAN_POINT ( 'NONE',  ( 4.724649144056972006, 54.30202410408965363, -6.163116443844200987 ) ) ;
#60212 = CARTESIAN_POINT ( 'NONE',  ( 31.48563847630141765, 438.9650070649207123, 23.22938501193561223 ) ) ;
#60213 = EDGE_LOOP ( 'NONE', ( #14699, #36117, #43067, #32899 ) ) ;
#60214 = FILL_AREA_STYLE ('',( #94145 ) ) ;
#60215 = FACE_OUTER_BOUND ( 'NONE', #22112, .T. ) ;
#60216 = CARTESIAN_POINT ( 'NONE',  ( 5.700740065103228282, 42.00193813223110340, -69.19507478788203514 ) ) ;
#60217 = CARTESIAN_POINT ( 'NONE',  ( -64.32759900501736183, 49.99999999999999289, -11.06576400629343659 ) ) ;
#60218 = DIRECTION ( 'NONE',  ( -1.000000000000000000, -0.000000000000000000, 0.000000000000000000 ) ) ;
#60219 = CARTESIAN_POINT ( 'NONE',  ( 43.00000000000000000, 464.8825480873695710, 15.07585856869435936 ) ) ;
#60220 = ORIENTED_EDGE ( 'NONE', *, *, #25422, .T. ) ;
#60221 = CARTESIAN_POINT ( 'NONE',  ( 4.464296094009049476, 13.01099471650158002, -12.88508357975252139 ) ) ;
#60223 = CARTESIAN_POINT ( 'NONE',  ( 20.24742129507015420, -42.95413648879811319, 31.59189836021716857 ) ) ;
#60222 = CARTESIAN_POINT ( 'NONE',  ( -103.2140057312332715, -60.00000000000000000, 203.2732544657875167 ) ) ;
#60224 = STYLED_ITEM ( 'NONE', ( #27273 ), #90947 ) ;
#60225 = CARTESIAN_POINT ( 'NONE',  ( 119.0671996398097008, 7.666536031838888654, -59.53359981990482908 ) ) ;
#60226 = DIRECTION ( 'NONE',  ( 1.000000000000000000, 1.224606353822377258E-16, 0.000000000000000000 ) ) ;
#60227 = CARTESIAN_POINT ( 'NONE',  ( -38.79755192928217156, -53.35182168183835927, 40.67521693547091388 ) ) ;
#60228 = UNCERTAINTY_MEASURE_WITH_UNIT (LENGTH_MEASURE( 1.000000000000000082E-05 ), #106042, 'distance_accuracy_value', 'NONE');
#60229 = EDGE_LOOP ( 'NONE', ( #78489, #61366, #27833, #90158 ) ) ;
#60230 = DIRECTION ( 'NONE',  ( 0.000000000000000000, 0.000000000000000000, 1.000000000000000000 ) ) ;
#60231 = CARTESIAN_POINT ( 'NONE',  ( -43.37536761788616957, 434.6169042472839692, 10.05068736166123067 ) ) ;
#60232 = CARTESIAN_POINT ( 'NONE',  ( -13.93078765908243710, -57.79386853345808106, 28.41172023899451560 ) ) ;
#60233 = AXIS2_PLACEMENT_3D ( 'NONE', #54751, #13763, #105445 ) ;
#60234 = CARTESIAN_POINT ( 'NONE',  ( 0.000000000000000000, 16.00000000000000000, 0.000000000000000000 ) ) ;
#60235 = CARTESIAN_POINT ( 'NONE',  ( 7.212408192734266699, -62.98482910679632596, -3.465038817813884009 ) ) ;
#60236 = CARTESIAN_POINT ( 'NONE',  ( -15.64030048137934870, 6.456385560660732104, 7.561819230134807945 ) ) ;
#60237 = VERTEX_POINT ( 'NONE', #32466 ) ;
#60238 = ORIENTED_EDGE ( 'NONE', *, *, #19211, .T. ) ;
#60239 = CARTESIAN_POINT ( 'NONE',  ( 101.1293268413511726, -29.99999999999999289, 173.2232745131870786 ) ) ;
#60240 = DIRECTION ( 'NONE',  ( 1.000000000000000000, 0.000000000000000000, -0.000000000000000000 ) ) ;
#60241 = CARTESIAN_POINT ( 'NONE',  ( -5.909155701201243893, -81.13738319811274380, 1.073778020691686486 ) ) ;
#60242 = ADVANCED_FACE ( 'NONE', ( #63228 ), #63758, .T. ) ;
#60243 = CARTESIAN_POINT ( 'NONE',  ( 86.62138541769266453, -30.00000000000000000, 68.13828909135614254 ) ) ;
#60244 = ADVANCED_FACE ( 'NONE', ( #71299 ), #96499, .T. ) ;
#60245 = CARTESIAN_POINT ( 'NONE',  ( -24.59793477076208035, 305.5470220219680755, 10.31311235332461962 ) ) ;
#60246 = ORIENTED_EDGE ( 'NONE', *, *, #94511, .F. ) ;
#60247 = CONICAL_SURFACE ( 'NONE', #32680, 3.309500000000001663, 0.9599310885968770357 ) ;
#60248 = EDGE_LOOP ( 'NONE', ( #6837, #23034, #49919, #67319 ) ) ;
#60249 = VERTEX_POINT ( 'NONE', #33518 ) ;
#60251 = VECTOR ( 'NONE', #74169, 1000.000000000000000 ) ;
#60250 = CARTESIAN_POINT ( 'NONE',  ( -32.65804572401754058, 465.7880960007716453, 12.84163515238938658 ) ) ;
#60252 = DIRECTION ( 'NONE',  ( 0.000000000000000000, 0.000000000000000000, 1.000000000000000000 ) ) ;
#60253 = CARTESIAN_POINT ( 'NONE',  ( -1.469576158976823947E-15, -15.87499999999999289, 8.000000000000000000 ) ) ;
#60254 = CARTESIAN_POINT ( 'NONE',  ( 4.656390720430125363, -11.31646185960546624, 3.786082374785829430 ) ) ;
#60255 = CARTESIAN_POINT ( 'NONE',  ( -31.21592496536052153, 336.6237673982246292, 17.82514839731485168 ) ) ;
#60256 = FILL_AREA_STYLE_COLOUR ( '', #7013 ) ;
#60258 = ORIENTED_EDGE ( 'NONE', *, *, #82521, .F. ) ;
#60257 = VECTOR ( 'NONE', #43108, 1000.000000000000000 ) ;
#60259 = CARTESIAN_POINT ( 'NONE',  ( -7.996668422907487361, 49.99999999999999289, -91.14546720082822162 ) ) ;
#60260 = ORIENTED_EDGE ( 'NONE', *, *, #58456, .F. ) ;
#60261 = CARTESIAN_POINT ( 'NONE',  ( -5.092539576892241904, -62.55676532791567013, 3.177249149099056869 ) ) ;
#60262 = CARTESIAN_POINT ( 'NONE',  ( 74.24099750797692820, -38.32798285832743801, 162.4509745339827589 ) ) ;
#60263 = DIRECTION ( 'NONE',  ( -1.000000000000000000, -1.224606353822377258E-16, -0.000000000000000000 ) ) ;
#60264 = CARTESIAN_POINT ( 'NONE',  ( 24.52975191904706165, 295.5903344108262445, 10.09557803800713316 ) ) ;
#60265 = AXIS2_PLACEMENT_3D ( 'NONE', #95611, #3952, #30365 ) ;
#60266 = CARTESIAN_POINT ( 'NONE',  ( 14.34999999999999787, 1.533819458162526451E-15, 0.000000000000000000 ) ) ;
#60267 = VERTEX_POINT ( 'NONE', #1643 ) ;
#60268 = CARTESIAN_POINT ( 'NONE',  ( 28.73053610125072410, 13.62316949804204391, -40.04352587319223744 ) ) ;
#60269 = CARTESIAN_POINT ( 'NONE',  ( 16.80263806300985863, 45.55013935554967475, -6.657797401561987627 ) ) ;
#60270 = LINE ( 'NONE', #85597, #95426 ) ;
#60271 = STYLED_ITEM ( 'NONE', ( #32221 ), #48764 ) ;
#60272 = CARTESIAN_POINT ( 'NONE',  ( -44.61777206441702504, 434.3429578869024112, 14.57557122161328600 ) ) ;
#60273 = SURFACE_STYLE_FILL_AREA ( #70329 ) ;
#60274 = ORIENTED_EDGE ( 'NONE', *, *, #47419, .T. ) ;
#60275 = AXIS2_PLACEMENT_3D ( 'NONE', #91311, #16338, #49224 ) ;
#60277 = CARTESIAN_POINT ( 'NONE',  ( 7.896254658894418021, -88.78929182754201577, 1.307282859663298158 ) ) ;
#60276 =( NAMED_UNIT ( * ) SI_UNIT ( $, .STERADIAN. ) SOLID_ANGLE_UNIT ( ) );
#60278 = FACE_OUTER_BOUND ( 'NONE', #60213, .T. ) ;
#60279 = DIRECTION ( 'NONE',  ( 1.000000000000000000, 0.000000000000000000, 0.000000000000000000 ) ) ;
#60280 = CARTESIAN_POINT ( 'NONE',  ( 32.99999999999930367, 489.5971041675264246, 10.80646835458744803 ) ) ;
#60281 = CARTESIAN_POINT ( 'NONE',  ( 0.000000000000000000, 0.000000000000000000, -8.000000000000000000 ) ) ;
#60282 = EDGE_CURVE ( 'NONE', #31665, #25443, #13283, .T. ) ;
#60283 = CARTESIAN_POINT ( 'NONE',  ( 46.00000000000000000, 461.7884530657001392, 10.79543072748596977 ) ) ;
#60284 = CARTESIAN_POINT ( 'NONE',  ( 86.12526957674350570, -50.15648532675116655, 190.9329294407513089 ) ) ;
#60285 = CIRCLE ( 'NONE', #86073, 13.00000000000000000 ) ;
#60286 = CARTESIAN_POINT ( 'NONE',  ( -2.860285599241079169, 85.38585347072158527, 5.000000000000000000 ) ) ;
#60287 = ORIENTED_EDGE ( 'NONE', *, *, #19652, .F. ) ;
#60288 = CARTESIAN_POINT ( 'NONE',  ( 76.07691912369757858, -57.67120883703200462, -32.16632477336341367 ) ) ;
#60289 = DIRECTION ( 'NONE',  ( 0.000000000000000000, -1.000000000000000000, 0.000000000000000000 ) ) ;
#60290 = CARTESIAN_POINT ( 'NONE',  ( 7.999999999999998224, -18.59374999999999289, 3.313708498984766049 ) ) ;
#60291 = CARTESIAN_POINT ( 'NONE',  ( -81.90484931453705997, -30.00000000000000000, 32.97508095190593025 ) ) ;
#60292 = EDGE_CURVE ( 'NONE', #65608, #38217, #73568, .T. ) ;
#60293 = EDGE_CURVE ( 'NONE', #102372, #62199, #3071, .T. ) ;
#60294 = CARTESIAN_POINT ( 'NONE',  ( 32.07628956478022531, -57.68926933952037928, 46.61244027368547194 ) ) ;
#60295 = CIRCLE ( 'NONE', #99908, 8.400000000000000355 ) ;
#60297 = CARTESIAN_POINT ( 'NONE',  ( 18.69420657816679210, 304.6310092840336097, -10.04693110555010982 ) ) ;
#60296 = CARTESIAN_POINT ( 'NONE',  ( 0.000000000000000000, 0.000000000000000000, 0.000000000000000000 ) ) ;
#60298 = CARTESIAN_POINT ( 'NONE',  ( 6.474469369223094795, -49.25375315074590787, 39.41384094684381267 ) ) ;
#60299 = CARTESIAN_POINT ( 'NONE',  ( -21.97839536960432838, -26.35170283925622314, 29.01137685833781532 ) ) ;
#60300 = CARTESIAN_POINT ( 'NONE',  ( -12.39854599882998976, -8.430153398135471932, -0.8386200322165905385 ) ) ;
#60301 = DIRECTION ( 'NONE',  ( -1.000000000000000000, -0.000000000000000000, -0.000000000000000000 ) ) ;
#60302 = CARTESIAN_POINT ( 'NONE',  ( 57.44923501886911055, -28.89280837408547598, -25.82236834149354721 ) ) ;
#60303 = EDGE_CURVE ( 'NONE', #32012, #76835, #80574, .T. ) ;
#60304 = CARTESIAN_POINT ( 'NONE',  ( -21.87228149277378719, -60.36180085709548848, 34.72076190976543586 ) ) ;
#60305 = VERTEX_POINT ( 'NONE', #27044 ) ;
#60306 = CARTESIAN_POINT ( 'NONE',  ( -4.999999999999993783, -4.000000000000003553, 102.2532056551910387 ) ) ;
#60307 = SURFACE_STYLE_FILL_AREA ( #27430 ) ;
#60308 = CARTESIAN_POINT ( 'NONE',  ( -18.94606539149997815, -35.99581223526647733, 30.30179149493963919 ) ) ;
#60309 = EDGE_CURVE ( 'NONE', #75687, #35302, #9410, .T. ) ;
#60310 = CARTESIAN_POINT ( 'NONE',  ( 0.3381605861720692330, 37.19676752111978857, -27.28514138315811266 ) ) ;
#60311 = ORIENTED_EDGE ( 'NONE', *, *, #29511, .T. ) ;
#60312 = AXIS2_PLACEMENT_3D ( 'NONE', #103433, #95883, #22007 ) ;
#60313 = CARTESIAN_POINT ( 'NONE',  ( -36.56384560112791604, 437.5716728810670588, 4.260240708029983558 ) ) ;
#60314 = EDGE_LOOP ( 'NONE', ( #39009, #57329, #91911, #4605, #53186, #57371, #83383, #64424, #68179 ) ) ;
#60315 =( NAMED_UNIT ( * ) SI_UNIT ( $, .STERADIAN. ) SOLID_ANGLE_UNIT ( ) );
#60316 = CONICAL_SURFACE ( 'NONE', #86123, 5.000000000000010658, 0.9599310885968697082 ) ;
#60317 = FACE_OUTER_BOUND ( 'NONE', #64235, .T. ) ;
#60318 = CARTESIAN_POINT ( 'NONE',  ( -7.585180042662256578E-16, 0.6351314446025488891, 6.500000000000000000 ) ) ;
#60320 = EDGE_CURVE ( 'NONE', #53605, #91474, #17079, .T. ) ;
#60319 = VERTEX_POINT ( 'NONE', #50718 ) ;
#60321 = CARTESIAN_POINT ( 'NONE',  ( 72.37206225042174879, -4.000000000000000000, 0.000000000000000000 ) ) ;
#60322 =( NAMED_UNIT ( * ) PLANE_ANGLE_UNIT ( ) SI_UNIT ( $, .RADIAN. ) );
#60323 = CARTESIAN_POINT ( 'NONE',  ( 99.48073951191379649, -45.27021486848132525, 193.0246297540120963 ) ) ;
#60325 = CARTESIAN_POINT ( 'NONE',  ( -7.801642220026312025, -6.412031738509686107, 1.787233835843581531 ) ) ;
#60324 = CARTESIAN_POINT ( 'NONE',  ( 8.838746709400247425, 294.6759852208345478, -4.712208899071270274 ) ) ;
#60326 = ORIENTED_EDGE ( 'NONE', *, *, #79363, .F. ) ;
#60327 = AXIS2_PLACEMENT_3D ( 'NONE', #91471, #97951, #17587 ) ;
#60328 = EDGE_LOOP ( 'NONE', ( #50119, #105258, #36433, #58478, #76683, #13322 ) ) ;
#60329 = ORIENTED_EDGE ( 'NONE', *, *, #105426, .T. ) ;
#60330 = CARTESIAN_POINT ( 'NONE',  ( 24.23626286421126252, 305.2563944236501356, 10.24644595435697880 ) ) ;
#60331 = PRESENTATION_LAYER_ASSIGNMENT (  '', '', ( #60271 ) ) ;
#60332 = CARTESIAN_POINT ( 'NONE',  ( -8.000000000000000000, -28.24999999999999645, -9.797174393178825657E-16 ) ) ;
#60333 = CARTESIAN_POINT ( 'NONE',  ( 31.46253585067004721, 1.340359594676612611E-15, 0.000000000000000000 ) ) ;
#60334 = ORIENTED_EDGE ( 'NONE', *, *, #99094, .F. ) ;
#60335 = CARTESIAN_POINT ( 'NONE',  ( 9.797174393178825657E-16, 0.9999999999999970024, -8.000000000000000000 ) ) ;
#60336 = CARTESIAN_POINT ( 'NONE',  ( 39.34999999999999432, 1.533819458162526451E-15, 0.000000000000000000 ) ) ;
#60337 = CARTESIAN_POINT ( 'NONE',  ( -93.97829082725922945, -60.00000000000243006, -15.75854254785690500 ) ) ;
#60338 = CIRCLE ( 'NONE', #68955, 2.999999999999999112 ) ;
#60339 = DIRECTION ( 'NONE',  ( 0.000000000000000000, -1.000000000000000000, 0.000000000000000000 ) ) ;
#60340 = CARTESIAN_POINT ( 'NONE',  ( 88.48689482502902592, 1.016364837396684119E-14, 0.000000000000000000 ) ) ;
#60341 = CARTESIAN_POINT ( 'NONE',  ( 89.99999999999997158, -60.00000000000000000, 196.0238439516549818 ) ) ;
#60342 = CARTESIAN_POINT ( 'NONE',  ( -85.44375122223560481, -14.21045842199445630, -16.44937377337592466 ) ) ;
#60343 =( NAMED_UNIT ( * ) SI_UNIT ( $, .STERADIAN. ) SOLID_ANGLE_UNIT ( ) );
#60344 = CARTESIAN_POINT ( 'NONE',  ( -51.03670451184174794, -49.90889464192031966, 56.18977702641336691 ) ) ;
#60345 = CIRCLE ( 'NONE', #27650, 11.00000000000000000 ) ;
#60346 = ORIENTED_EDGE ( 'NONE', *, *, #54265, .T. ) ;
#60347 = FACE_OUTER_BOUND ( 'NONE', #51350, .T. ) ;
#60348 = VERTEX_POINT ( 'NONE', #10279 ) ;
#60349 = CARTESIAN_POINT ( 'NONE',  ( -8.000000000000000000, -13.34374999999999467, -3.313708498984762496 ) ) ;
#60350 = CARTESIAN_POINT ( 'NONE',  ( -8.019147853987105279, 302.4786514485144835, -10.03165473704664201 ) ) ;
#60351 = CIRCLE ( 'NONE', #53403, 5.000000000000010658 ) ;
#60352 = CARTESIAN_POINT ( 'NONE',  ( 4.589357672516649167, -8.937939690227786116, -3.865585121226769338 ) ) ;
#60353 = ORIENTED_EDGE ( 'NONE', *, *, #71269, .T. ) ;
#60354 = CARTESIAN_POINT ( 'NONE',  ( -6.903421418544427368, -12.56552240113756014, 8.191925706847577260 ) ) ;
#60355 = CARTESIAN_POINT ( 'NONE',  ( 50.51862023164185445, -38.33298512735416352, 69.71478400885560234 ) ) ;
#60356 = CARTESIAN_POINT ( 'NONE',  ( 61.85555555555556140, -3.309500000000000774, 4.475777889183797681E-16 ) ) ;
#60357 = CARTESIAN_POINT ( 'NONE',  ( 81.84444444444444855, 1.023464760207051730E-14, 0.000000000000000000 ) ) ;
#60358 = CARTESIAN_POINT ( 'NONE',  ( 6.711450852063899575, 41.78336497133594207, -59.19447471094596835 ) ) ;
#60359 = CARTESIAN_POINT ( 'NONE',  ( 33.52312678242137167, 18.64316884714798306, 19.32152200346563120 ) ) ;
#60360 = CARTESIAN_POINT ( 'NONE',  ( 86.89255445192647187, -30.00000000000000355, 183.2879409112302369 ) ) ;
#60361 = CARTESIAN_POINT ( 'NONE',  ( 43.61075255792288630, 434.4875743724471135, 10.88293886035321734 ) ) ;
#60362 = EDGE_CURVE ( 'NONE', #16458, #9982, #51232, .T. ) ;
#60363 = CARTESIAN_POINT ( 'NONE',  ( 43.86650669486618881, 1.474610560812782335E-15, 0.000000000000000000 ) ) ;
#60364 = ORIENTED_EDGE ( 'NONE', *, *, #48044, .T. ) ;
#60365 = VERTEX_POINT ( 'NONE', #35127 ) ;
#60366 = CARTESIAN_POINT ( 'NONE',  ( 55.42290428782216338, -36.02733805088502805, 59.79522858329378465 ) ) ;
#60367 = CARTESIAN_POINT ( 'NONE',  ( 6.592761323367946069, 41.57274267171208493, -58.68933690419966354 ) ) ;
#60368 = EDGE_CURVE ( 'NONE', #103221, #45098, #100881, .T. ) ;
#60369 = DIRECTION ( 'NONE',  ( -1.000000000000000000, 0.000000000000000000, 0.000000000000000000 ) ) ;
#60370 = ORIENTED_EDGE ( 'NONE', *, *, #80508, .F. ) ;
#60371 = CARTESIAN_POINT ( 'NONE',  ( -90.26554477178873981, -38.40034450972390090, -15.28474180237319757 ) ) ;
#60372 = ORIENTED_EDGE ( 'NONE', *, *, #65905, .F. ) ;
#60373 = CARTESIAN_POINT ( 'NONE',  ( 16.13590653351296211, 6.313628335806327208, 5.716602451448080657 ) ) ;
#60374 = CARTESIAN_POINT ( 'NONE',  ( 110.6785498806628851, -38.35606011449173991, 180.6793801968407251 ) ) ;
#60375 = CARTESIAN_POINT ( 'NONE',  ( 12.69243684000737993, 23.10840795830348782, 5.362199319019091526 ) ) ;
#60376 = CARTESIAN_POINT ( 'NONE',  ( 88.45222707626928127, -52.71650411927125646, 52.49135111675786192 ) ) ;
#60377 = CARTESIAN_POINT ( 'NONE',  ( 0.000000000000000000, 0.000000000000000000, 5.000000000000002665 ) ) ;
#60378 = CARTESIAN_POINT ( 'NONE',  ( -25.59639872491835177, 305.3408274204018653, -9.675241084463289454 ) ) ;
#60379 = CARTESIAN_POINT ( 'NONE',  ( 1.000000000000000000, -5.000000000000018652, -14.14213562373094568 ) ) ;
#60380 =( REPRESENTATION_RELATIONSHIP ('NONE','NONE', #69581, #52881 ) REPRESENTATION_RELATIONSHIP_WITH_TRANSFORMATION ( #1192 )SHAPE_REPRESENTATION_RELATIONSHIP( ) );
#60381 = DIRECTION ( 'NONE',  ( 0.000000000000000000, 1.000000000000000000, 0.000000000000000000 ) ) ;
#60382 = CARTESIAN_POINT ( 'NONE',  ( -43.71675722380574314, 435.0430370928003185, 11.37024750954368635 ) ) ;
#60383 = CARTESIAN_POINT ( 'NONE',  ( 3.768877481699944632, 132.6348382055886646, 5.000000000000000888 ) ) ;
#60384 = VERTEX_POINT ( 'NONE', #8155 ) ;
#60385 = EDGE_CURVE ( 'NONE', #2149, #76395, #68517, .T. ) ;
#60386 = CARTESIAN_POINT ( 'NONE',  ( 0.3334405834852849360, 36.31501813831545888, 29.70764397845630000 ) ) ;
#60387 = CARTESIAN_POINT ( 'NONE',  ( 16.12471489245790224, 36.55922634087983880, -24.15021214291702378 ) ) ;
#60388 = CIRCLE ( 'NONE', #20853, 5.000000000000010658 ) ;
#60389 = DIRECTION ( 'NONE',  ( 0.000000000000000000, -0.000000000000000000, 1.000000000000000000 ) ) ;
#60390 = ORIENTED_EDGE ( 'NONE', *, *, #72319, .T. ) ;
#60391 = CARTESIAN_POINT ( 'NONE',  ( -31.17618607851400725, 315.1976444128995354, -6.525171466224566785 ) ) ;
#60392 = CARTESIAN_POINT ( 'NONE',  ( -31.53578816574763266, 327.5873836966717931, 15.99885046268745548 ) ) ;
#60393 = CARTESIAN_POINT ( 'NONE',  ( 0.000000000000000000, 4.898587196589413815E-16, -4.000000000000000888 ) ) ;
#60394 = CARTESIAN_POINT ( 'NONE',  ( 1.078140322363270668E-05, -30.00000000000000000, 28.88964995960238014 ) ) ;
#60395 = CARTESIAN_POINT ( 'NONE',  ( 5.656854249492380582, -18.31249999999999289, -5.656854249492379694 ) ) ;
#60396 = CARTESIAN_POINT ( 'NONE',  ( -46.78455459927008064, -28.88905235460685006, 42.05601398093777021 ) ) ;
#60397 = ADVANCED_FACE ( 'NONE', ( #73944 ), #32996, .T. ) ;
#60398 = VECTOR ( 'NONE', #37772, 1000.000000000000000 ) ;
#60399 = CARTESIAN_POINT ( 'NONE',  ( 24.83349330513380337, 4.898587196589405926E-16, -4.000000000000001776 ) ) ;
#60400 = ORIENTED_EDGE ( 'NONE', *, *, #9671, .T. ) ;
#60401 = CARTESIAN_POINT ( 'NONE',  ( 85.51531819923015121, -28.66246248194799051, 177.8895563405388032 ) ) ;
#60402 = LINE ( 'NONE', #19440, #94677 ) ;
#60403 = CARTESIAN_POINT ( 'NONE',  ( -15.66258511614958593, 45.99742480776466635, 6.198981311147433004 ) ) ;
#60404 = ORIENTED_EDGE ( 'NONE', *, *, #65619, .T. ) ;
#60405 = CARTESIAN_POINT ( 'NONE',  ( -97.56669589868897674, -60.15515597314767859, 100.7599927763139505 ) ) ;
#60406 = CIRCLE ( 'NONE', #55205, 4.000000000000000888 ) ;
#60407 = DIRECTION ( 'NONE',  ( 0.000000000000000000, 1.000000000000000000, 0.000000000000000000 ) ) ;
#60408 = CARTESIAN_POINT ( 'NONE',  ( -42.61140200160144786, 465.9030374194822457, 13.21253569360411895 ) ) ;
#60409 = CARTESIAN_POINT ( 'NONE',  ( 13.83769416169610444, -3.000000000000003109, -79.05569278145411261 ) ) ;
#60410 = CARTESIAN_POINT ( 'NONE',  ( -23.06278213417854062, -26.97848082407063330, -38.42385101396828873 ) ) ;
#60411 = AXIS2_PLACEMENT_3D ( 'NONE', #44976, #85974, #12044 ) ;
#60412 = ADVANCED_FACE ( 'NONE', ( #16786 ), #82579, .F. ) ;
#60413 =( NAMED_UNIT ( * ) PLANE_ANGLE_UNIT ( ) SI_UNIT ( $, .RADIAN. ) );
#60414 = AXIS2_PLACEMENT_3D ( 'NONE', #104703, #63738, #55597 ) ;
#60415 = CARTESIAN_POINT ( 'NONE',  ( 41.84377380827102400, -60.00000000000000000, 54.90543347242942218 ) ) ;
#60416 = CARTESIAN_POINT ( 'NONE',  ( 36.47095910356380699, -36.25311398404432595, 45.65967941635479121 ) ) ;
#60417 = DIRECTION ( 'NONE',  ( 0.000000000000000000, 0.000000000000000000, -1.000000000000000000 ) ) ;
#60418 = CARTESIAN_POINT ( 'NONE',  ( 27.77029367025814111, -20.61067439569943360, 31.81999448069623071 ) ) ;
#60420 = CARTESIAN_POINT ( 'NONE',  ( -11.51927709202785266, 20.60355208861105325, 7.999819647742008044 ) ) ;
#60419 = CARTESIAN_POINT ( 'NONE',  ( -36.83723954793523347, -36.42387658263878336, 46.04340430436438680 ) ) ;
#60421 = CIRCLE ( 'NONE', #36340, 4.000000000000001776 ) ;
#60422 = CARTESIAN_POINT ( 'NONE',  ( 6.864655157673967167, 294.7328080983106133, -7.282300054020917734 ) ) ;
#60423 = CARTESIAN_POINT ( 'NONE',  ( 45.40507512465600115, 439.2794387026467575, 6.273370203490043373 ) ) ;
#60424 = DIRECTION ( 'NONE',  ( 0.000000000000000000, 0.000000000000000000, -1.000000000000000000 ) ) ;
#60425 = DIRECTION ( 'NONE',  ( -1.000000000000000000, -0.000000000000000000, -0.000000000000000000 ) ) ;
#60426 = ORIENTED_EDGE ( 'NONE', *, *, #49055, .F. ) ;
#60427 = CONICAL_SURFACE ( 'NONE', #8650, 4.000000000000001776, 0.9599310885968774798 ) ;
#60428 = CARTESIAN_POINT ( 'NONE',  ( 0.000000000000000000, 294.8518027762758038, 9.936999415352289589 ) ) ;
#60429 = CARTESIAN_POINT ( 'NONE',  ( -2.026006894917399492, -60.00000000000001421, 39.63628641406589992 ) ) ;
#60430 = ORIENTED_EDGE ( 'NONE', *, *, #3666, .T. ) ;
#60431 = DIRECTION ( 'NONE',  ( -0.8714291948011178013, 0.000000000000000000, -0.4905213129398923178 ) ) ;
#60432 = LINE ( 'NONE', #2687, #35065 ) ;
#60433 = DIRECTION ( 'NONE',  ( -0.000000000000000000, -0.000000000000000000, -1.000000000000000000 ) ) ;
#60434 = ADVANCED_FACE ( 'NONE', ( #29183 ), #47855, .T. ) ;
#60436 = CARTESIAN_POINT ( 'NONE',  ( -3.214504396424240795, -60.22813258367417433, -36.90743551004686651 ) ) ;
#60435 = DIRECTION ( 'NONE',  ( 1.000000000000000000, 0.000000000000000000, 0.000000000000000000 ) ) ;
#60437 = EDGE_LOOP ( 'NONE', ( #24396, #96953, #1989, #36206 ) ) ;
#60438 = CARTESIAN_POINT ( 'NONE',  ( 27.10511071441197117, 36.60571256639528315, 10.05698433968570704 ) ) ;
#60439 = CARTESIAN_POINT ( 'NONE',  ( 18.09999999999999787, 1.533819458162526451E-15, 0.000000000000000000 ) ) ;
#60440 = ORIENTED_EDGE ( 'NONE', *, *, #39618, .T. ) ;
#60441 = CIRCLE ( 'NONE', #63826, 14.00000000000000178 ) ;
#60442 = ADVANCED_FACE ( 'NONE', ( #28638 ), #29699, .T. ) ;
#60443 = PLANE ( 'NONE',  #47260 ) ;
#60444 = CARTESIAN_POINT ( 'NONE',  ( 12.79230769230769305, -4.171999999999999709, 5.616230220889763424E-16 ) ) ;
#60445 = CIRCLE ( 'NONE', #8666, 4.000000000000000888 ) ;
#60446 = LINE ( 'NONE', #69583, #82120 ) ;
#60447 = CARTESIAN_POINT ( 'NONE',  ( -92.04877409173086278, -60.00000000000000711, 19.49932517706979240 ) ) ;
#60448 = LINE ( 'NONE', #52855, #73825 ) ;
#60449 = CARTESIAN_POINT ( 'NONE',  ( -3.313708498984798467, -12.03124999999999112, -7.999999999999961808 ) ) ;
#60450 =( NAMED_UNIT ( * ) SI_UNIT ( $, .STERADIAN. ) SOLID_ANGLE_UNIT ( ) );
#60451 = CARTESIAN_POINT ( 'NONE',  ( 40.38232636938073483, 459.8969133356638963, 1.930624307834942321 ) ) ;
#60452 = CARTESIAN_POINT ( 'NONE',  ( -35.32911723019088157, 437.0667969981770966, 5.602639083907458684 ) ) ;
#60453 = CARTESIAN_POINT ( 'NONE',  ( -82.49914212121935009, -42.97583219876662497, 170.7411135741228918 ) ) ;
#60454 = ORIENTED_EDGE ( 'NONE', *, *, #12855, .F. ) ;
#60455 = CARTESIAN_POINT ( 'NONE',  ( -43.61500121660905904, 434.9783708497643602, 14.40566113421481553 ) ) ;
#60456 = EDGE_CURVE ( 'NONE', #57731, #82593, #52331, .T. ) ;
#60457 = VERTEX_POINT ( 'NONE', #95456 ) ;
#60458 = ORIENTED_EDGE ( 'NONE', *, *, #45381, .T. ) ;
#60459 = CARTESIAN_POINT ( 'NONE',  ( -4.391938347788321373, -1.138802597855428589, 104.3926446507461065 ) ) ;
#60460 = CARTESIAN_POINT ( 'NONE',  ( -9.999008799017543581, -5.000000000000578204, -14.11099437790245226 ) ) ;
#60461 = CARTESIAN_POINT ( 'NONE',  ( -4.633158437802761763E-12, -9.016621985895911351, -7.999704684617491068 ) ) ;
#60462 = VERTEX_POINT ( 'NONE', #86333 ) ;
#60463 = CONICAL_SURFACE ( 'NONE', #63925, 3.309500000000007880, 0.9599310885968770357 ) ;
#60464 =( LENGTH_UNIT ( ) NAMED_UNIT ( * ) SI_UNIT ( .MILLI., .METRE. ) );
#60465 = CARTESIAN_POINT ( 'NONE',  ( -90.36739715925041594, -57.66608071200965213, -21.81949331871602382 ) ) ;
#60466 = CARTESIAN_POINT ( 'NONE',  ( 7.896254658894418021, -13.78929182754201044, 1.307282859663291719 ) ) ;
#60467 = AXIS2_PLACEMENT_3D ( 'NONE', #96826, #22956, #55792 ) ;
#60468 = CARTESIAN_POINT ( 'NONE',  ( 43.51760155599759372, 464.6236256767953137, 9.550830537168854661 ) ) ;
#60469 = CARTESIAN_POINT ( 'NONE',  ( 24.00351036083323564, 27.29299690957943980, 32.94270042870552828 ) ) ;
#60470 = CARTESIAN_POINT ( 'NONE',  ( -13.44292909870241459, -52.70664433108516533, 30.91132584605806244 ) ) ;
#60471 = CARTESIAN_POINT ( 'NONE',  ( -97.48274675841855696, -52.68933714276726477, 195.2152360717980741 ) ) ;
#60472 = CARTESIAN_POINT ( 'NONE',  ( 90.15648792673195544, -30.00000000000007816, 30.33492934306279309 ) ) ;
#60473 =( BOUNDED_CURVE ( )  B_SPLINE_CURVE ( 2, ( #92708, #18868, #99190, #49589, #99739, #43630, #50630, #25352, #35043 ),
 .UNSPECIFIED., .F., .F. ) 
 B_SPLINE_CURVE_WITH_KNOTS ( ( 3, 2, 2, 2, 3 ),
 ( 0.1617647058823529216, 0.1691176470588235115, 0.1764705882352941013, 0.1838235294117647189, 0.1911764705882352811 ),
 .UNSPECIFIED. ) 
 CURVE ( )  GEOMETRIC_REPRESENTATION_ITEM ( )  RATIONAL_B_SPLINE_CURVE ( ( 1.000000000000000222, 0.9238795325112864054, 1.000000000000000000, 0.9238795325112867385, 1.000000000000000000, 0.9238795325112867385, 1.000000000000000000, 0.9238795325112867385, 1.000000000000000000 ) ) 
 REPRESENTATION_ITEM ( '' )  );
#60474 = CARTESIAN_POINT ( 'NONE',  ( -80.78871696068775066, -30.00000000000004974, 192.9492619026495390 ) ) ;
#60475 = CARTESIAN_POINT ( 'NONE',  ( -60.56849898340908567, -25.59444836810600776, 67.17426576971645602 ) ) ;
#60476 = ORIENTED_EDGE ( 'NONE', *, *, #74995, .T. ) ;
#60477 = CARTESIAN_POINT ( 'NONE',  ( 0.000000000000000000, 300.0000000000000000, 9.936999415352289589 ) ) ;
#60478 = ORIENTED_EDGE ( 'NONE', *, *, #54490, .T. ) ;
#60479 = CARTESIAN_POINT ( 'NONE',  ( -105.5953457684452701, -60.15498359724100652, 185.0758216606398321 ) ) ;
#60480 = DIRECTION ( 'NONE',  ( 0.000000000000000000, 0.000000000000000000, -1.000000000000000000 ) ) ;
#60481 = CARTESIAN_POINT ( 'NONE',  ( -29.87260017595988515, 13.22901743408734276, -42.09629626707205574 ) ) ;
#60482 = ORIENTED_EDGE ( 'NONE', *, *, #67120, .F. ) ;
#60483 = CARTESIAN_POINT ( 'NONE',  ( 7.230783165913826416, -2.999999999999999112, -70.90935356275363688 ) ) ;
#60484 = AXIS2_PLACEMENT_3D ( 'NONE', #4428, #22234, #38931 ) ;
#60485 = CARTESIAN_POINT ( 'NONE',  ( -3.883877898720556665, -1.065320993063029631, 104.5781496044265424 ) ) ;
#60486 = CARTESIAN_POINT ( 'NONE',  ( 2.977408999572650927, -11.75000000204838813, -7.188101187500001821 ) ) ;
#60487 = CIRCLE ( 'NONE', #58847, 4.000000000000000888 ) ;
#60488 = FACE_BOUND ( 'NONE', #29628, .T. ) ;
#60489 = CYLINDRICAL_SURFACE ( 'NONE', #42605, 2.000000000000000000 ) ;
#60490 = CARTESIAN_POINT ( 'NONE',  ( 12.81917055448646359, 0.000000000000000000, -11.24487389204835353 ) ) ;
#60491 = CARTESIAN_POINT ( 'NONE',  ( -11.99733130326054997, -4.773999631974040092, -12.57663782514888240 ) ) ;
#60492 = CIRCLE ( 'NONE', #74223, 4.000000000000000888 ) ;
#60493 = DIRECTION ( 'NONE',  ( -1.000000000000000000, -0.000000000000000000, -0.000000000000000000 ) ) ;
#60494 = CARTESIAN_POINT ( 'NONE',  ( 13.50000000000000355, -1.317096457811611332, -13.00000000000000000 ) ) ;
#60495 = EDGE_CURVE ( 'NONE', #69309, #31339, #42625, .T. ) ;
#60496 = CARTESIAN_POINT ( 'NONE',  ( -31.99613883384627755, -46.43541966511591568, 35.16710097061795892 ) ) ;
#60497 = CARTESIAN_POINT ( 'NONE',  ( 45.48381414773980680, -36.07135055825224157, 43.31344887555280110 ) ) ;
#60498 = CARTESIAN_POINT ( 'NONE',  ( -33.00540147334732666, 487.4196752801200887, 9.523982417603956918 ) ) ;
#60499 = EDGE_CURVE ( 'NONE', #88227, #48464, #90917, .T. ) ;
#60500 = CARTESIAN_POINT ( 'NONE',  ( -5.000000000000000000, -15.62228920881133298, 12.61250543006184088 ) ) ;
#60501 = CARTESIAN_POINT ( 'NONE',  ( -98.19059862094080415, -38.47942618394503711, 200.9491795779894971 ) ) ;
#60502 = ORIENTED_EDGE ( 'NONE', *, *, #81930, .F. ) ;
#60504 = DIRECTION ( 'NONE',  ( 0.9077394194966191820, -0.1875825441123765147, 0.3752624887145921684 ) ) ;
#60503 = CARTESIAN_POINT ( 'NONE',  ( 64.29999999999999716, 3.309500000000014541, 4.052968581778174646E-16 ) ) ;
#60505 = CARTESIAN_POINT ( 'NONE',  ( 13.11292558562340815, 8.306547552537741907, -8.834142966937790220 ) ) ;
#60506 = CARTESIAN_POINT ( 'NONE',  ( -18.91781669292785395, 48.00000000000000000, 62.18610382930904734 ) ) ;
#60507 = CARTESIAN_POINT ( 'NONE',  ( -7.274255425475363523, 41.49770500802092243, -59.52552341803120584 ) ) ;
#60508 = CARTESIAN_POINT ( 'NONE',  ( 4.854898838401722649, 40.57569111244889370, -70.80100276615310406 ) ) ;
#60509 = CARTESIAN_POINT ( 'NONE',  ( 0.000000000000000000, 6.123233995736770227E-16, -5.000000000000002665 ) ) ;
#60510 = CARTESIAN_POINT ( 'NONE',  ( 1.153719650317168133E-13, -1.200000000000000030E-05, 49.25000000000000000 ) ) ;
#60511 = DIRECTION ( 'NONE',  ( 1.000000000000000000, 0.000000000000000000, 0.000000000000000000 ) ) ;
#60512 = CARTESIAN_POINT ( 'NONE',  ( 111.2651448867182182, -59.99999999999999289, 185.8803051558543018 ) ) ;
#60513 = CARTESIAN_POINT ( 'NONE',  ( -7.550180524134849414, -68.00559247213185188, 2.651855549982493176 ) ) ;
#60514 = ORIENTED_EDGE ( 'NONE', *, *, #43835, .F. ) ;
#60515 = CARTESIAN_POINT ( 'NONE',  ( 2.893255198029168973, -49.53525371043113523, 103.3592142771324518 ) ) ;
#60516 = CIRCLE ( 'NONE', #55316, 8.000000000000000000 ) ;
#60517 = CARTESIAN_POINT ( 'NONE',  ( -82.23392483931314700, -29.99999999999997158, 36.79773247150587423 ) ) ;
#60518 = VERTEX_POINT ( 'NONE', #28107 ) ;
#60519 = CARTESIAN_POINT ( 'NONE',  ( 5.311458304196372104, 22.41101449600902740, -41.39308602215781718 ) ) ;
#60520 = CARTESIAN_POINT ( 'NONE',  ( 12.48910114120020687, -3.488630791343517945, -13.76724771964344640 ) ) ;
#60521 = CARTESIAN_POINT ( 'NONE',  ( -6.990291106834062518, -3.000000000000000444, 4.028951842967197550 ) ) ;
#60522 = DIRECTION ( 'NONE',  ( -1.000000000000000000, -1.224606353822377258E-16, -0.000000000000000000 ) ) ;
#60523 = CARTESIAN_POINT ( 'NONE',  ( 5.082755093536324154, -18.21875000204838457, 5.082755093536326818 ) ) ;
#60524 = FILL_AREA_STYLE_COLOUR ( '', #55352 ) ;
#60525 = PRODUCT_DEFINITION_SHAPE ( 'NONE', 'NONE',  #98978 ) ;
#60526 = CARTESIAN_POINT ( 'NONE',  ( -5.656854249492381470, -11.75000000409677092, 5.656854249492379694 ) ) ;
#60528 = ORIENTED_EDGE ( 'NONE', *, *, #22963, .F. ) ;
#60527 = SURFACE_STYLE_FILL_AREA ( #42186 ) ;
#60529 = CARTESIAN_POINT ( 'NONE',  ( 83.46195034026524695, -29.07547344062109573, 157.7160910814760939 ) ) ;
#60530 = CARTESIAN_POINT ( 'NONE',  ( -45.99999999999995737, 461.9152041119569390, 5.112156919902204777 ) ) ;
#60531 = CARTESIAN_POINT ( 'NONE',  ( 9.699189539447123920, 88.17692228246710329, -2.444343703917210231 ) ) ;
#60532 = ORIENTED_EDGE ( 'NONE', *, *, #7720, .F. ) ;
#60533 = DIRECTION ( 'NONE',  ( -0.000000000000000000, 1.000000000000000000, -0.000000000000000000 ) ) ;
#60534 =( NAMED_UNIT ( * ) SI_UNIT ( $, .STERADIAN. ) SOLID_ANGLE_UNIT ( ) );
#60535 = CARTESIAN_POINT ( 'NONE',  ( 37.88797360199545494, 27.49820559598491343, -13.42505087926272189 ) ) ;
#60536 = CARTESIAN_POINT ( 'NONE',  ( 40.02592568779148507, 1.482358050883964840E-15, 0.000000000000000000 ) ) ;
#60537 = CARTESIAN_POINT ( 'NONE',  ( -5.383284837158160308, 253.0004934351577504, 2.657356347551687037 ) ) ;
#60538 = CARTESIAN_POINT ( 'NONE',  ( 1.251110940609005739, 15.60643737211089110, 50.60543736410414084 ) ) ;
#60539 = CARTESIAN_POINT ( 'NONE',  ( 8.644795791334905388, -0.2475540741395084177, 19.58096426192390638 ) ) ;
#60540 = ORIENTED_EDGE ( 'NONE', *, *, #91369, .T. ) ;
#60541 = CIRCLE ( 'NONE', #32968, 4.172000000000001485 ) ;
#60542 = CARTESIAN_POINT ( 'NONE',  ( -80.58034289023321151, -29.99999999999999289, -12.88258808325728566 ) ) ;
#60543 = SURFACE_STYLE_FILL_AREA ( #58398 ) ;
#60544 = CARTESIAN_POINT ( 'NONE',  ( 86.93474114976024225, -53.74889697056932647, 192.8288056809579984 ) ) ;
#60546 =( NAMED_UNIT ( * ) SI_UNIT ( $, .STERADIAN. ) SOLID_ANGLE_UNIT ( ) );
#60545 = CARTESIAN_POINT ( 'NONE',  ( 45.11650669486618881, 4.898587196589411843E-16, -4.000000000000000888 ) ) ;
#60547 = CARTESIAN_POINT ( 'NONE',  ( -2.977408999572654480, -22.62500000204838813, 7.188101187499999156 ) ) ;
#60548 = CARTESIAN_POINT ( 'NONE',  ( 1.224646799147353454E-15, 0.000000000000000000, 10.00000000000000178 ) ) ;
#60549 = CARTESIAN_POINT ( 'NONE',  ( 1.301042606982605321E-15, -5.000000000000000000, -10.00000000000000000 ) ) ;
#60550 = CARTESIAN_POINT ( 'NONE',  ( -7.549004593702462351, -4.358419834287845518, -7.700121441565844549 ) ) ;
#60551 = ORIENTED_EDGE ( 'NONE', *, *, #55586, .F. ) ;
#60552 = CIRCLE ( 'NONE', #1922, 5.000000000000002665 ) ;
#60553 = CARTESIAN_POINT ( 'NONE',  ( 40.16087957073692394, 485.8454018306723015, -4.964645702805086103 ) ) ;
#60554 = SURFACE_STYLE_USAGE ( .BOTH. , #35772 ) ;
#60555 = AXIS2_PLACEMENT_3D ( 'NONE', #98813, #26062, #81552 ) ;
#60556 = CARTESIAN_POINT ( 'NONE',  ( -9.998878006819809983, 7.501608443945841032, 0.000000000000000000 ) ) ;
#60557 = LINE ( 'NONE', #17967, #48064 ) ;
#60558 = EDGE_CURVE ( 'NONE', #62868, #83521, #102930, .T. ) ;
#60559 = EDGE_LOOP ( 'NONE', ( #75399, #42364, #34185, #51127, #30959, #76281, #105435 ) ) ;
#60560 = AXIS2_PLACEMENT_3D ( 'NONE', #72611, #24100, #73122 ) ;
#60561 = ADVANCED_FACE ( 'NONE', ( #44259 ), #1336, .T. ) ;
#60562 = CARTESIAN_POINT ( 'NONE',  ( 37.50813744631010849, 482.1291867456659475, 15.12800786539085784 ) ) ;
#60564 = ORIENTED_EDGE ( 'NONE', *, *, #44800, .F. ) ;
#60563 = AXIS2_PLACEMENT_3D ( 'NONE', #97429, #47814, #31158 ) ;
#60565 = EDGE_CURVE ( 'NONE', #57292, #55329, #56389, .T. ) ;
#60567 = CARTESIAN_POINT ( 'NONE',  ( 33.05104704987640929, 434.2951118972601421, 15.74527730978287110 ) ) ;
#60566 = TOROIDAL_SURFACE ( 'NONE', #76083, 12.00000000000000711, 3.000000000000000000 ) ;
#60568 = CARTESIAN_POINT ( 'NONE',  ( 9.176855344542989457, 104.4703957302259028, -3.973472207155928970 ) ) ;
#60569 = PRESENTATION_STYLE_ASSIGNMENT (( #101539 ) ) ;
#60570 = CARTESIAN_POINT ( 'NONE',  ( -100.6730827315817010, -59.99999999999999289, 201.6981752365160219 ) ) ;
#60571 = CARTESIAN_POINT ( 'NONE',  ( 19.21238756580750717, 49.78778941994806218, 61.53710458952721041 ) ) ;
#60572 = CARTESIAN_POINT ( 'NONE',  ( 5.799999999999999822, 8.000000000000000000, 0.000000000000000000 ) ) ;
#60573 = DIRECTION ( 'NONE',  ( 0.000000000000000000, 0.000000000000000000, -1.000000000000000000 ) ) ;
#60574 = LINE ( 'NONE', #67059, #87020 ) ;
#60575 = CARTESIAN_POINT ( 'NONE',  ( -86.40560123953810034, -17.60749286260778135, 177.3355119052273494 ) ) ;
#60576 = SURFACE_STYLE_FILL_AREA ( #43832 ) ;
#60577 = ADVANCED_FACE ( 'NONE', ( #43715 ), #49555, .T. ) ;
#60578 = VERTEX_POINT ( 'NONE', #93870 ) ;
#60579 = FACE_OUTER_BOUND ( 'NONE', #88751, .T. ) ;
#60580 = CARTESIAN_POINT ( 'NONE',  ( 3.352941176471716744, -1.200583151107622815, 104.5794940929782797 ) ) ;
#60581 = CARTESIAN_POINT ( 'NONE',  ( -85.46236302623604786, -52.71435437274617897, -0.4815862223618528892 ) ) ;
#60582 = CIRCLE ( 'NONE', #22717, 4.000000000000000888 ) ;
#60583 = CARTESIAN_POINT ( 'NONE',  ( 33.88469969133011261, 464.6054137899092211, 6.797944932417496311 ) ) ;
#60584 = DIRECTION ( 'NONE',  ( 0.000000000000000000, -1.000000000000000000, 0.000000000000000000 ) ) ;
#60585 = AXIS2_PLACEMENT_3D ( 'NONE', #35145, #99844, #85264 ) ;
#60586 = CARTESIAN_POINT ( 'NONE',  ( 11.08349330513380160, 4.000000000000002665, 0.000000000000000000 ) ) ;
#60587 = CARTESIAN_POINT ( 'NONE',  ( 0.000000000000000000, 0.000000000000000000, 0.000000000000000000 ) ) ;
#60588 =( NAMED_UNIT ( * ) SI_UNIT ( $, .STERADIAN. ) SOLID_ANGLE_UNIT ( ) );
#60589 = CARTESIAN_POINT ( 'NONE',  ( 66.01776342811430709, -14.21045842199433373, 101.7751388943407989 ) ) ;
#60590 = CARTESIAN_POINT ( 'NONE',  ( -26.13315753361836613, 60.33964880548970910, -13.06657876680918662 ) ) ;
#60591 = CARTESIAN_POINT ( 'NONE',  ( -77.20948002450832348, -29.99999999999995737, -26.53460153345886496 ) ) ;
#60592 = VECTOR ( 'NONE', #28074, 1000.000000000000000 ) ;
#60593 = CARTESIAN_POINT ( 'NONE',  ( -74.77681607752303705, -18.65167433089163751, 105.3459956964869235 ) ) ;
#60594 = ORIENTED_EDGE ( 'NONE', *, *, #47383, .T. ) ;
#60595 = CARTESIAN_POINT ( 'NONE',  ( 78.42622819757743002, -14.21045842199428932, 178.5071270543957951 ) ) ;
#60596 = CARTESIAN_POINT ( 'NONE',  ( 11.87327623748599770, 40.83929701193095951, 63.97656400230257390 ) ) ;
#60597 = CARTESIAN_POINT ( 'NONE',  ( 44.60816201714979456, -57.67117032717165870, -40.90560715985412799 ) ) ;
#60598 = ORIENTED_EDGE ( 'NONE', *, *, #45267, .F. ) ;
#60599 = CARTESIAN_POINT ( 'NONE',  ( 14.83349330513380693, 4.000000000000003553, 0.000000000000000000 ) ) ;
#60600 = CARTESIAN_POINT ( 'NONE',  ( -5.082755093536326818, -26.09375000204838813, 5.082755093536325042 ) ) ;
#60601 = CARTESIAN_POINT ( 'NONE',  ( 21.36650669486618881, 1.474610560812782335E-15, 0.000000000000000000 ) ) ;
#60602 = ORIENTED_EDGE ( 'NONE', *, *, #39209, .T. ) ;
#60603 =( NAMED_UNIT ( * ) SI_UNIT ( $, .STERADIAN. ) SOLID_ANGLE_UNIT ( ) );
#60604 = ORIENTED_EDGE ( 'NONE', *, *, #57675, .T. ) ;
#60605 = LINE ( 'NONE', #103172, #71685 ) ;
#60606 = CARTESIAN_POINT ( 'NONE',  ( 0.000000000000000000, 0.000000000000000000, 0.000000000000000000 ) ) ;
#60607 = CARTESIAN_POINT ( 'NONE',  ( -33.63572111039716361, -59.99999999999509015, 48.29151853392890104 ) ) ;
#60608 = CARTESIAN_POINT ( 'NONE',  ( 23.29688253297234724, 304.4092765216364000, -9.880365301581617743 ) ) ;
#60609 = CARTESIAN_POINT ( 'NONE',  ( -1.320432766682874540E-15, -30.40625000204838813, 7.188101187500000044 ) ) ;
#60610 = CARTESIAN_POINT ( 'NONE',  ( 13.37207953394533355, 6.123233995736772199E-16, -5.000000000000001776 ) ) ;
#60611 =( BOUNDED_SURFACE ( )  B_SPLINE_SURFACE ( 3, 2, ( 
 ( #30907, #22811, #105292 ),
 ( #45487, #38978, #14663 ),
 ( #4478, #88058, #80469 ),
 ( #63788, #70280, #103700 ),
 ( #95612, #5013, #71851 ),
 ( #6580, #104757, #13610 ),
 ( #54062, #39513, #72387 ),
 ( #97189, #53560, #46524 ),
 ( #103179, #87007, #13078 ),
 ( #46007, #37947, #70806 ),
 ( #5533, #38459, #104219 ),
 ( #54, #24928, #64835 ),
 ( #82610, #31953, #17364 ),
 ( #98258, #73972, #23333 ),
 ( #1125, #89115, #34099 ),
 ( #57250, #99303, #50237 ) ),
 .UNSPECIFIED., .F., .F., .T. ) 
 B_SPLINE_SURFACE_WITH_KNOTS ( ( 4, 2, 2, 2, 2, 2, 2, 4 ),
 ( 3, 3 ),
 ( -2.388584351323025812E-05, 0.004361143453687739771, 0.008746172750888710559, 0.01751623134529065040, 0.02628628993969259198, 0.03505634853409453355, 0.05259646572289841671, 0.07013658291170229986 ),
 ( 0.000000000000000000, 1.000000000000000000 ),
 .UNSPECIFIED. ) 
 GEOMETRIC_REPRESENTATION_ITEM ( )  RATIONAL_B_SPLINE_SURFACE ( (
 ( 1.000000000000000000, 0.7071067811865475727, 1.000000000000000000),
 ( 1.000000000000000000, 0.7071067811865475727, 1.000000000000000000),
 ( 1.000000000000000000, 0.7071067811865475727, 1.000000000000000000),
 ( 1.000000000000000000, 0.7071067811865475727, 1.000000000000000000),
 ( 1.000000000000000000, 0.7071067811865475727, 1.000000000000000000),
 ( 1.000000000000000000, 0.7071067811865475727, 1.000000000000000000),
 ( 1.000000000000000000, 0.7071067811865473507, 1.000000000000000000),
 ( 1.000000000000000000, 0.7071067811865473507, 1.000000000000000000),
 ( 1.000000000000000000, 0.7071067811865475727, 1.000000000000000000),
 ( 1.000000000000000000, 0.7071067811865475727, 1.000000000000000000),
 ( 1.000000000000000000, 0.7071067811865475727, 1.000000000000000000),
 ( 1.000000000000000000, 0.7071067811865475727, 1.000000000000000000),
 ( 1.000000000000000000, 0.7071067811865475727, 1.000000000000000000),
 ( 1.000000000000000000, 0.7071067811865475727, 1.000000000000000000),
 ( 1.000000000000000000, 0.7071067811865475727, 1.000000000000000000),
 ( 1.000000000000000000, 0.7071067811865475727, 1.000000000000000000) ) ) 
 REPRESENTATION_ITEM ( '' )  SURFACE ( )  );
#60612 = CARTESIAN_POINT ( 'NONE',  ( 3.202572202863678275, -1.001691937163285528, 104.2977074219132447 ) ) ;
#60613 = CARTESIAN_POINT ( 'NONE',  ( 105.5720000000000312, 0.000000000000000000, 5.000000000000000888 ) ) ;
#60614 =( LENGTH_UNIT ( ) NAMED_UNIT ( * ) SI_UNIT ( .MILLI., .METRE. ) );
#60615 = CARTESIAN_POINT ( 'NONE',  ( -5.656854249492381470, -14.56249999999999289, 5.656854249492379694 ) ) ;
#60616 = CARTESIAN_POINT ( 'NONE',  ( 40.54863160047459303, 437.2386745228082532, 5.317148167334600828 ) ) ;
#60617 = EDGE_CURVE ( 'NONE', #1310, #71316, #40937, .T. ) ;
#60618 = UNCERTAINTY_MEASURE_WITH_UNIT (LENGTH_MEASURE( 1.000000000000000082E-05 ), #97027, 'distance_accuracy_value', 'NONE');
#60619 = ORIENTED_EDGE ( 'NONE', *, *, #55931, .T. ) ;
#60620 = CARTESIAN_POINT ( 'NONE',  ( 4.999999999999993783, -3.737948356800089300, 102.2532056550983128 ) ) ;
#60622 = CARTESIAN_POINT ( 'NONE',  ( 32.61996141319230702, -46.43004813113018514, 35.44677629655089390 ) ) ;
#60621 = CARTESIAN_POINT ( 'NONE',  ( -3.558939058151462831, -48.93902971889401954, 104.4181685828932871 ) ) ;
#60623 = CARTESIAN_POINT ( 'NONE',  ( 24.56594385547430903, -4.285714285713612348, -6.601913983211183279 ) ) ;
#60624 = ORIENTED_EDGE ( 'NONE', *, *, #54281, .F. ) ;
#60625 = ADVANCED_FACE ( 'NONE', ( #85800 ), #56473, .F. ) ;
#60626 = EDGE_CURVE ( 'NONE', #82654, #102083, #53041, .T. ) ;
#60627 = DIRECTION ( 'NONE',  ( 0.000000000000000000, 0.000000000000000000, -1.000000000000000000 ) ) ;
#60629 = CARTESIAN_POINT ( 'NONE',  ( -35.74483125092430669, 413.6409941285803598, 6.029078300230034770 ) ) ;
#60628 = FACE_OUTER_BOUND ( 'NONE', #84610, .T. ) ;
#60630 = CARTESIAN_POINT ( 'NONE',  ( 66.74444444444444002, -3.309500000000000774, 0.000000000000000000 ) ) ;
#60631 = LINE ( 'NONE', #84355, #48289 ) ;
#60632 =( LENGTH_UNIT ( ) NAMED_UNIT ( * ) SI_UNIT ( .MILLI., .METRE. ) );
#60633 = LINE ( 'NONE', #85420, #89645 ) ;
#60634 = CARTESIAN_POINT ( 'NONE',  ( -35.22347075582651144, 464.3861918352932889, 19.05313339797837102 ) ) ;
#60635 = ORIENTED_EDGE ( 'NONE', *, *, #100844, .T. ) ;
#60636 = CARTESIAN_POINT ( 'NONE',  ( 92.56520787782876880, -60.00000000000000711, -2.232329057168804365 ) ) ;
#60637 = DIRECTION ( 'NONE',  ( -1.000000000000000000, 0.000000000000000000, 0.000000000000000000 ) ) ;
#60638 = CIRCLE ( 'NONE', #55429, 3.309500000000001663 ) ;
#60639 = CARTESIAN_POINT ( 'NONE',  ( -36.68211027471578234, 426.6599842481110159, 5.461410629243083292 ) ) ;
#60640 = STYLED_ITEM ( 'NONE', ( #106371 ), #50979 ) ;
#60641 = CARTESIAN_POINT ( 'NONE',  ( -6.060118994825670846, 40.55658335032454431, -71.16215350181603583 ) ) ;
#60642 = LINE ( 'NONE', #59030, #71925 ) ;
#60643 = ORIENTED_EDGE ( 'NONE', *, *, #76977, .F. ) ;
#60644 = EDGE_CURVE ( 'NONE', #46447, #85900, #54433, .T. ) ;
#60645 = CARTESIAN_POINT ( 'NONE',  ( -105.0046858871420028, -29.99999999999525713, 195.3910615991270561 ) ) ;
#60646 = ORIENTED_EDGE ( 'NONE', *, *, #82398, .F. ) ;
#60647 = CARTESIAN_POINT ( 'NONE',  ( 8.000000000000000000, -10.99999999999999289, 0.000000000000000000 ) ) ;
#60648 = DIRECTION ( 'NONE',  ( -1.000000000000000000, -0.000000000000000000, -0.000000000000000000 ) ) ;
#60649 = DIRECTION ( 'NONE',  ( -1.000000000000000000, -1.224606353822377258E-16, -0.000000000000000000 ) ) ;
#60650 = CARTESIAN_POINT ( 'NONE',  ( 86.78321768392551405, -60.22672886896445021, -10.97222102851997150 ) ) ;
#60651 = CARTESIAN_POINT ( 'NONE',  ( -37.65068595401864116, 305.0254819914457016, -7.656417700763605616 ) ) ;
#60652 = DIRECTION ( 'NONE',  ( 0.000000000000000000, -0.8660254037844380415, 0.5000000000000012212 ) ) ;
#60653 = CARTESIAN_POINT ( 'NONE',  ( -18.28239497294003968, 45.00000000000002132, 62.41453136349703357 ) ) ;
#60654 = VERTEX_POINT ( 'NONE', #40399 ) ;
#60655 =( GEOMETRIC_REPRESENTATION_CONTEXT ( 3 ) GLOBAL_UNCERTAINTY_ASSIGNED_CONTEXT ( ( #91493 ) ) GLOBAL_UNIT_ASSIGNED_CONTEXT ( ( #99651, #18231, #45161 ) ) REPRESENTATION_CONTEXT ( 'NONE', 'WORKASPACE' ) );
#60656 = VERTEX_POINT ( 'NONE', #64685 ) ;
#60657 = CARTESIAN_POINT ( 'NONE',  ( 48.49490330227207124, 10.48921555948079387, -14.43974515806029579 ) ) ;
#60658 = DIRECTION ( 'NONE',  ( 0.000000000000000000, 0.000000000000000000, -1.000000000000000000 ) ) ;
#60659 = B_SPLINE_CURVE_WITH_KNOTS ( 'NONE', 3,
 ( #48442, #81333, #40359, #73238, #99659, #67312, #60300, #42483 ),
 .UNSPECIFIED., .F., .F.,
 ( 4, 2, 2, 4 ),
 ( 0.007886720825438852528, 0.009850969036564046280, 0.01181521724768924003, 0.01574371366993963101 ),
 .UNSPECIFIED. ) ;
#60660 = EDGE_CURVE ( 'NONE', #94269, #66369, #6509, .T. ) ;
#60662 = ORIENTED_EDGE ( 'NONE', *, *, #5866, .T. ) ;
#60661 = LINE ( 'NONE', #104266, #32164 ) ;
#60663 = CARTESIAN_POINT ( 'NONE',  ( 71.96604720757427742, -25.59085233378921842, 100.0522785706842228 ) ) ;
#60664 = EDGE_LOOP ( 'NONE', ( #61247, #85562, #54445, #60329, #15036 ) ) ;
#60665 = CARTESIAN_POINT ( 'NONE',  ( 4.972909066023143865, -46.53482677768356979, 42.62007988880538534 ) ) ;
#60666 = CARTESIAN_POINT ( 'NONE',  ( 5.082755093536325930, -23.46875000204838457, -5.082755093536325042 ) ) ;
#60667 = CARTESIAN_POINT ( 'NONE',  ( -103.1324900820093262, -57.63586870064128931, 202.7914362107620434 ) ) ;
#60668 = ORIENTED_EDGE ( 'NONE', *, *, #1301, .F. ) ;
#60669 = VECTOR ( 'NONE', #22004, 1000.000000000000000 ) ;
#60670 = MECHANICAL_DESIGN_GEOMETRIC_PRESENTATION_REPRESENTATION (  '', ( #95071 ), #3758 ) ;
#60671 = CARTESIAN_POINT ( 'NONE',  ( 102.8080410108812544, -37.84829216994245371, 172.5350295752351713 ) ) ;
#60672 = CARTESIAN_POINT ( 'NONE',  ( -43.02621584241282449, 434.6128289108255558, 16.97888786059002086 ) ) ;
#60673 = TOROIDAL_SURFACE ( 'NONE', #55463, 11.00000000000000000, 1.000000000000000000 ) ;
#60674 = CYLINDRICAL_SURFACE ( 'NONE', #62031, 60.00000000000000000 ) ;
#60675 = CARTESIAN_POINT ( 'NONE',  ( -3.313708498984765161, -20.65625000409677270, 7.999999999999998224 ) ) ;
#60676 = CARTESIAN_POINT ( 'NONE',  ( -45.18794255447445352, -28.36039750011541827, 40.27443962283176404 ) ) ;
#60677 = DIRECTION ( 'NONE',  ( 0.000000000000000000, 1.000000000000000000, -0.000000000000000000 ) ) ;
#60678 = LINE ( 'NONE', #45023, #12065 ) ;
#60679 = B_SPLINE_CURVE_WITH_KNOTS ( 'NONE', 3,
 ( #72812, #64742, #88496, #106238, #71754, #64229, #73340, #32398, #48539, #97101, #97618, #23242, #81430, #65270, #104663, #96588, #23784, #6490 ),
 .UNSPECIFIED., .F., .F.,
 ( 4, 2, 2, 2, 2, 2, 2, 2, 4 ),
 ( 0.5000000000000000000, 0.5625000000000000000, 0.6250000000000000000, 0.6875000000000000000, 0.7500000000000000000, 0.8125000000000000000, 0.8750000000000000000, 0.9375000000000000000, 1.000000000000000000 ),
 .UNSPECIFIED. ) ;
#60680 = CARTESIAN_POINT ( 'NONE',  ( 32.20054824794733861, 485.9557913861509633, 4.953638954094006230 ) ) ;
#60681 = DIRECTION ( 'NONE',  ( 1.000000000000000000, 0.000000000000000000, 0.000000000000000000 ) ) ;
#60682 = CARTESIAN_POINT ( 'NONE',  ( 32.99999999999998579, 463.5362553048591963, 6.739467187734351938 ) ) ;
#60683 = ORIENTED_EDGE ( 'NONE', *, *, #28665, .F. ) ;
#60684 = CARTESIAN_POINT ( 'NONE',  ( -5.036565248985447774, -51.83812713192594401, 40.06353886212085769 ) ) ;
#60685 = CARTESIAN_POINT ( 'NONE',  ( 11.07494621800369039, -4.984107567658546678, -12.57739282099218592 ) ) ;
#60686 = DIRECTION ( 'NONE',  ( 0.000000000000000000, 0.000000000000000000, 1.000000000000000000 ) ) ;
#60687 = CARTESIAN_POINT ( 'NONE',  ( -86.33424672516723319, -30.00000000000000000, 180.6259601542327857 ) ) ;
#60688 = EDGE_CURVE ( 'NONE', #47738, #79305, #5391, .T. ) ;
#60689 = EDGE_LOOP ( 'NONE', ( #20670, #55193, #105823, #69374, #68850 ) ) ;
#60690 = DIRECTION ( 'NONE',  ( 0.000000000000000000, 1.000000000000000000, 0.000000000000000000 ) ) ;
#60691 = CARTESIAN_POINT ( 'NONE',  ( 81.46498296581839327, -57.51694840548930188, 200.1052016080623162 ) ) ;
#60692 = DIRECTION ( 'NONE',  ( -1.000000000000000000, -1.224606353822377258E-16, -0.000000000000000000 ) ) ;
#60693 = ADVANCED_FACE ( 'NONE', ( #14510 ), #80312, .T. ) ;
#60694 = EDGE_CURVE ( 'NONE', #99927, #95837, #52978, .T. ) ;
#60695 = CARTESIAN_POINT ( 'NONE',  ( 58.29968221944096740, -37.09312005238718513, -34.56216655994825970 ) ) ;
#60696 = CARTESIAN_POINT ( 'NONE',  ( -16.14328335387691027, 20.70972091797312231, -4.174903250177856684 ) ) ;
#60697 = CARTESIAN_POINT ( 'NONE',  ( 18.71538461538461462, 4.172000000000003261, 0.000000000000000000 ) ) ;
#60698 = CARTESIAN_POINT ( 'NONE',  ( -71.35988770730575936, -60.00000000000000711, 149.7293370354783804 ) ) ;
#60699 = CARTESIAN_POINT ( 'NONE',  ( -31.23718509250011621, 439.6127102907155404, 23.21745058978948251 ) ) ;
#60700 = EDGE_CURVE ( 'NONE', #19012, #90464, #16121, .T. ) ;
#60701 = CARTESIAN_POINT ( 'NONE',  ( 51.78317192862468943, 48.00000000000000000, 39.73656039225600978 ) ) ;
#60702 = CARTESIAN_POINT ( 'NONE',  ( -86.75334951847432308, -24.36967792699222102, 185.3770496680724875 ) ) ;
#60703 = ORIENTED_EDGE ( 'NONE', *, *, #62678, .T. ) ;
#60704 = CARTESIAN_POINT ( 'NONE',  ( 22.33349330513380693, -4.000000000000000000, 4.898587196589415787E-16 ) ) ;
#60705 = CARTESIAN_POINT ( 'NONE',  ( -1.013597693207653139, -49.92101462973083414, 32.20981906455752153 ) ) ;
#60706 = EDGE_CURVE ( 'NONE', #57621, #73170, #73826, .T. ) ;
#60707 = CARTESIAN_POINT ( 'NONE',  ( -6.417056615203631686, 41.92969948368747168, -59.44199727782134346 ) ) ;
#60708 = AXIS2_PLACEMENT_3D ( 'NONE', #83190, #74563, #99350 ) ;
#60709 = CARTESIAN_POINT ( 'NONE',  ( -2.100696513098593066, -49.85179523580853100, 102.1543767095519968 ) ) ;
#60710 = CARTESIAN_POINT ( 'NONE',  ( -24.29519218197498631, 295.4518972802553094, 2.065840140822523541 ) ) ;
#60711 = ORIENTED_EDGE ( 'NONE', *, *, #85026, .T. ) ;
#60712 = CARTESIAN_POINT ( 'NONE',  ( 3.673202536116901758E-15, 1.005902684993158047, 14.99698745252234566 ) ) ;
#60713 = CARTESIAN_POINT ( 'NONE',  ( 39.98830517851552457, 490.5859057859975110, 11.67971501230864995 ) ) ;
#60714 = CARTESIAN_POINT ( 'NONE',  ( 1.125484721681054401, 27.97705396987858961, 38.86472904274390316 ) ) ;
#60715 = CARTESIAN_POINT ( 'NONE',  ( -29.68315524077005207, 13.12249633091091816, -39.60535821593474282 ) ) ;
#60716 = AXIS2_PLACEMENT_3D ( 'NONE', #39134, #96308, #54747 ) ;
#60717 = CARTESIAN_POINT ( 'NONE',  ( 23.32842889633158379, 295.1981192840830772, -1.925701350189481076 ) ) ;
#60718 = CARTESIAN_POINT ( 'NONE',  ( 35.74363442581862671, 380.1068966271811860, 4.951945592532029927 ) ) ;
#60719 = CARTESIAN_POINT ( 'NONE',  ( 9.781676926622875357, 53.39490368674695731, -3.092698992276897041 ) ) ;
#60720 = B_SPLINE_CURVE_WITH_KNOTS ( 'NONE', 3,
 ( #6752, #8341, #89807, #98415, #15906, #216, #97346, #88743, #65528, #81678, #66051, #97884, #48785, #90328, #49320, #7800, #106500, #6208, #24567, #80105, #24039, #98928 ),
 .UNSPECIFIED., .F., .F.,
 ( 4, 2, 2, 2, 2, 2, 2, 2, 2, 2, 4 ),
 ( 0.003271557979369705584, 0.003775597685872196171, 0.004279637392374686759, 0.004783677098877177347, 0.005287716805379667068, 0.005791756511882157656, 0.006043776365133403383, 0.006295796218384648243, 0.006547816071635893104, 0.006799835924887137964, 0.007303875631389625950 ),
 .UNSPECIFIED. ) ;
#60721 = CARTESIAN_POINT ( 'NONE',  ( 90.15648792673195544, -30.00000000000007816, 30.33492934306279309 ) ) ;
#60722 = CARTESIAN_POINT ( 'NONE',  ( -79.97220600232276411, -49.91032667486920360, 158.2823762716815565 ) ) ;
#60723 = ORIENTED_EDGE ( 'NONE', *, *, #94232, .T. ) ;
#60724 = FACE_OUTER_BOUND ( 'NONE', #32483, .T. ) ;
#60725 =( NAMED_UNIT ( * ) SI_UNIT ( $, .STERADIAN. ) SOLID_ANGLE_UNIT ( ) );
#60726 = CARTESIAN_POINT ( 'NONE',  ( 30.00000000000000000, 450.0000000000002274, 8.202422573753707979 ) ) ;
#60727 = CARTESIAN_POINT ( 'NONE',  ( 42.33262710065869783, 332.4327577417291195, 7.108190472527923021 ) ) ;
#60728 = CARTESIAN_POINT ( 'NONE',  ( 33.73990888920651088, 486.9635397366919278, 1.197403147134062706 ) ) ;
#60729 = EDGE_LOOP ( 'NONE', ( #31093, #44562, #90764, #40903 ) ) ;
#60730 = CARTESIAN_POINT ( 'NONE',  ( -3.493042281569127550, 304.8518027749427119, -10.00000000028269120 ) ) ;
#60731 = CARTESIAN_POINT ( 'NONE',  ( 0.000000000000000000, 27.68727484027578356, 0.000000000000000000 ) ) ;
#60732 = CARTESIAN_POINT ( 'NONE',  ( -7.188101187500001821, -29.00000000204838813, -2.977408999572651371 ) ) ;
#60733 = EDGE_LOOP ( 'NONE', ( #29887, #80926, #1088, #58921, #67335 ) ) ;
#60734 = DIRECTION ( 'NONE',  ( -0.000000000000000000, 1.000000000000000000, -0.000000000000000000 ) ) ;
#60735 = AXIS2_PLACEMENT_3D ( 'NONE', #100044, #75773, #102173 ) ;
#60736 = CARTESIAN_POINT ( 'NONE',  ( -2.450541714948251126, 15.75132464342601146, 9.701712097384769251 ) ) ;
#60737 = CARTESIAN_POINT ( 'NONE',  ( 6.821510612526563655, 41.53001914900257674, -70.37925568709802349 ) ) ;
#60738 = CARTESIAN_POINT ( 'NONE',  ( 42.35263604940418958, 50.00000000000000000, 46.99568999590452734 ) ) ;
#60739 = CARTESIAN_POINT ( 'NONE',  ( -8.000000000000000000, -17.74999999999999645, -9.797174393178825657E-16 ) ) ;
#60740 =( GEOMETRIC_REPRESENTATION_CONTEXT ( 3 ) GLOBAL_UNCERTAINTY_ASSIGNED_CONTEXT ( ( #23003 ) ) GLOBAL_UNIT_ASSIGNED_CONTEXT ( ( #7295, #39170, #40736 ) ) REPRESENTATION_CONTEXT ( 'NONE', 'WORKASPACE' ) );
#60741 = DIRECTION ( 'NONE',  ( -1.000000000000000000, -1.224606353822377258E-16, -0.000000000000000000 ) ) ;
#60742 = ORIENTED_EDGE ( 'NONE', *, *, #13559, .T. ) ;
#60743 = CARTESIAN_POINT ( 'NONE',  ( 44.28326324223792909, -60.00000000000000000, -38.95962436850444988 ) ) ;
#60744 = VECTOR ( 'NONE', #722, 1000.000000000000000 ) ;
#60746 = CARTESIAN_POINT ( 'NONE',  ( 19.65438280374391056, -18.59146986454509332, 27.43996338408375379 ) ) ;
#60745 = CARTESIAN_POINT ( 'NONE',  ( -48.81109529425772564, -14.21045842199442788, 55.84243332122913017 ) ) ;
#60747 = CARTESIAN_POINT ( 'NONE',  ( 8.851860011917325868E-15, 43.22324503868515677, -36.14046114390016839 ) ) ;
#60748 = EDGE_CURVE ( 'NONE', #75902, #51548, #58126, .T. ) ;
#60749 = CARTESIAN_POINT ( 'NONE',  ( -33.68155633810341953, -22.16622110500054177, 31.32162176238002971 ) ) ;
#60750 = UNCERTAINTY_MEASURE_WITH_UNIT (LENGTH_MEASURE( 1.000000000000000082E-05 ), #102334, 'distance_accuracy_value', 'NONE');
#60751 = ORIENTED_EDGE ( 'NONE', *, *, #102647, .T. ) ;
#60752 = CYLINDRICAL_SURFACE ( 'NONE', #54314, 1.250000000000001110 ) ;
#60753 = CARTESIAN_POINT ( 'NONE',  ( 119.9999999999999858, 0.000000000000000000, -59.99999999999997158 ) ) ;
#60754 = CARTESIAN_POINT ( 'NONE',  ( -13.42019126081076941, -55.04352106308903103, 30.98765330636284077 ) ) ;
#60755 = CIRCLE ( 'NONE', #14206, 4.172000000000001485 ) ;
#60756 = CARTESIAN_POINT ( 'NONE',  ( 22.61650669486618526, -3.999999999999998224, 0.000000000000000000 ) ) ;
#60757 = CARTESIAN_POINT ( 'NONE',  ( 6.928203230275509661, -65.00000000000000000, -4.000000000000002665 ) ) ;
#60758 = CARTESIAN_POINT ( 'NONE',  ( -15.85122647056043732, 4.114663126769221968, 4.288211754900368433 ) ) ;
#60759 = ORIENTED_EDGE ( 'NONE', *, *, #101671, .T. ) ;
#60760 = CARTESIAN_POINT ( 'NONE',  ( -15.55441737893091947, 37.11602535008573511, -22.68899775139453823 ) ) ;
#60761 = VERTEX_POINT ( 'NONE', #49549 ) ;
#60762 = CARTESIAN_POINT ( 'NONE',  ( 98.06547367653239178, -30.00000000000002132, 190.4620094107865498 ) ) ;
#60763 = CARTESIAN_POINT ( 'NONE',  ( 32.37035071761208371, 40.78778520401346697, -63.10690315066334932 ) ) ;
#60764 = CARTESIAN_POINT ( 'NONE',  ( 74.56127108291157413, 6.975173280561618775E-15, 0.000000000000000000 ) ) ;
#60765 = CARTESIAN_POINT ( 'NONE',  ( 81.32474297617858383, -30.00000000000000355, -0.8629055029887053863 ) ) ;
#60766 = EDGE_CURVE ( 'NONE', #43629, #71682, #82989, .T. ) ;
#60767 = CARTESIAN_POINT ( 'NONE',  ( -32.13490731594677641, 427.1953081090705950, 24.83868860164863079 ) ) ;
#60768 = ORIENTED_EDGE ( 'NONE', *, *, #39167, .F. ) ;
#60769 = ORIENTED_EDGE ( 'NONE', *, *, #3202, .T. ) ;
#60770 = VERTEX_POINT ( 'NONE', #18282 ) ;
#60771 = CARTESIAN_POINT ( 'NONE',  ( -32.68851106860801536, 465.0799323318227607, 13.83425062237807879 ) ) ;
#60772 = DIRECTION ( 'NONE',  ( -0.5735764363510459374, -0.8191520442889919096, 0.000000000000000000 ) ) ;
#60773 = DIRECTION ( 'NONE',  ( -1.000000000000000000, -1.224606353822377258E-16, -0.000000000000000000 ) ) ;
#60774 = CARTESIAN_POINT ( 'NONE',  ( 35.53294979701562539, 439.9362927074972731, 24.32573494709669149 ) ) ;
#60775 = CARTESIAN_POINT ( 'NONE',  ( -17.71948856052742016, 43.32302192893173043, -4.750715123135393902 ) ) ;
#60776 = DIRECTION ( 'NONE',  ( -1.000000000000000000, -0.000000000000000000, -0.000000000000000000 ) ) ;
#60777 = ORIENTED_EDGE ( 'NONE', *, *, #49369, .T. ) ;
#60778 = CARTESIAN_POINT ( 'NONE',  ( -3.140974613990812792, 50.00000000000000000, -73.31232788067644890 ) ) ;
#60779 = EDGE_LOOP ( 'NONE', ( #105538, #76751, #98623 ) ) ;
#60780 = CARTESIAN_POINT ( 'NONE',  ( -4.905018583967750700, -62.97640014320320034, -3.459768807258292167 ) ) ;
#60781 = CARTESIAN_POINT ( 'NONE',  ( 75.83882639694283512, -38.36842668940455070, 177.1099218260232817 ) ) ;
#60782 = DIRECTION ( 'NONE',  ( 0.000000000000000000, -1.000000000000000000, 0.000000000000000000 ) ) ;
#60783 = CARTESIAN_POINT ( 'NONE',  ( 24.62657823539835178, 295.6185519456691395, 10.10170238537927823 ) ) ;
#60784 = AXIS2_PLACEMENT_3D ( 'NONE', #18291, #91112, #1526 ) ;
#60785 = ADVANCED_FACE ( 'NONE', ( #98626 ), #84053, .F. ) ;
#60786 = LINE ( 'NONE', #36536, #37278 ) ;
#60787 = AXIS2_PLACEMENT_3D ( 'NONE', #18089, #91960, #67165 ) ;
#60788 = VERTEX_POINT ( 'NONE', #17208 ) ;
#60789 = CARTESIAN_POINT ( 'NONE',  ( 28.88699125077532059, 13.70431814614561539, -39.88880000601603371 ) ) ;
#60790 = DIRECTION ( 'NONE',  ( 0.000000000000000000, -1.000000000000000000, 0.000000000000000000 ) ) ;
#60791 = TOROIDAL_SURFACE ( 'NONE', #52134, 5.999999999999994671, 1.000000000000000444 ) ;
#60792 = CARTESIAN_POINT ( 'NONE',  ( 34.42332229506718022, 302.2847767890208956, 3.633360753947871391 ) ) ;
#60793 = ORIENTED_EDGE ( 'NONE', *, *, #33886, .T. ) ;
#60795 = CARTESIAN_POINT ( 'NONE',  ( 7.986711519608433285, -88.97361903623433932, -0.5300249774147601789 ) ) ;
#60794 =( NAMED_UNIT ( * ) PLANE_ANGLE_UNIT ( ) SI_UNIT ( $, .RADIAN. ) );
#60796 =( LENGTH_UNIT ( ) NAMED_UNIT ( * ) SI_UNIT ( .MILLI., .METRE. ) );
#60797 = CARTESIAN_POINT ( 'NONE',  ( -32.81992448453860334, 465.7192846569213884, 11.17271167765305862 ) ) ;
#60798 = DIRECTION ( 'NONE',  ( -0.000000000000000000, -0.000000000000000000, -1.000000000000000000 ) ) ;
#60799 = CARTESIAN_POINT ( 'NONE',  ( -0.04050535873993734576, 7.919512791578242172, -6.573129608219096198 ) ) ;
#60800 = CARTESIAN_POINT ( 'NONE',  ( 86.01633990920335293, -53.81041820905097239, 191.9596364128520634 ) ) ;
#60801 = CARTESIAN_POINT ( 'NONE',  ( 94.84444444444443434, 1.023464760207051730E-14, 0.000000000000000000 ) ) ;
#60802 = CARTESIAN_POINT ( 'NONE',  ( -8.002549191621405100, 102.8991202088225521, 5.000000000000000888 ) ) ;
#60803 = VERTEX_POINT ( 'NONE', #67350 ) ;
#60804 = CARTESIAN_POINT ( 'NONE',  ( 22.43756508786705695, -57.67086147514856265, -43.66263415315633978 ) ) ;
#60805 = CARTESIAN_POINT ( 'NONE',  ( 4.338297905010414901, -15.54644901148979486, -35.15006977224143014 ) ) ;
#60806 = CARTESIAN_POINT ( 'NONE',  ( 27.33349330513380337, 4.000000000000003553, 0.000000000000000000 ) ) ;
#60807 = CARTESIAN_POINT ( 'NONE',  ( 16.58687548431174363, 34.28952745851042749, -24.30698433968624883 ) ) ;
#60808 = DIRECTION ( 'NONE',  ( 0.000000000000000000, -1.000000000000000000, 0.000000000000000000 ) ) ;
#60809 = TOROIDAL_SURFACE ( 'NONE', #52231, 8.331345277524542681, 0.6186547224754556096 ) ;
#60810 = CARTESIAN_POINT ( 'NONE',  ( -90.21070732519919488, -29.99999999999999645, 89.72569532995613883 ) ) ;
#60811 = STYLED_ITEM ( 'NONE', ( #60147 ), #101356 ) ;
#60812 = EDGE_CURVE ( 'NONE', #10153, #59923, #1516, .T. ) ;
#60813 = MECHANICAL_DESIGN_GEOMETRIC_PRESENTATION_REPRESENTATION (  '', ( #52162 ), #83112 ) ;
#60814 = DIRECTION ( 'NONE',  ( -0.8191520442889924647, 0.000000000000000000, -0.5735764363510451602 ) ) ;
#60815 = CARTESIAN_POINT ( 'NONE',  ( 28.02193915076392727, -57.67940780473148266, 44.29223288112500967 ) ) ;
#60817 = CARTESIAN_POINT ( 'NONE',  ( -30.00000000000000000, 0.000000000000000000, 0.000000000000000000 ) ) ;
#60816 = CARTESIAN_POINT ( 'NONE',  ( 34.84618260875170392, 489.9833681528626812, 11.97975507378813731 ) ) ;
#60818 = EDGE_CURVE ( 'NONE', #92082, #26910, #59998, .T. ) ;
#60819 = CARTESIAN_POINT ( 'NONE',  ( -16.18099529597535025, -23.36744278781230477, 27.97947390617177277 ) ) ;
#60820 = CARTESIAN_POINT ( 'NONE',  ( 41.71840012517787244, 489.3048647944241907, 10.52957302900621350 ) ) ;
#60821 = CARTESIAN_POINT ( 'NONE',  ( 43.47539511674882817, 487.0683156417112514, 3.561597533069202903 ) ) ;
#60822 = CARTESIAN_POINT ( 'NONE',  ( 24.91891126693706227, -20.04364040963082516, -33.01464637846507344 ) ) ;
#60823 = CARTESIAN_POINT ( 'NONE',  ( -25.12479025497365370, -46.43848000890793770, 32.95526142708619233 ) ) ;
#60824 = ORIENTED_EDGE ( 'NONE', *, *, #47901, .F. ) ;
#60825 = CARTESIAN_POINT ( 'NONE',  ( 40.08499133126954206, 485.6798096563408649, -4.492259481486891914 ) ) ;
#60826 = CARTESIAN_POINT ( 'NONE',  ( -9.165151389911679658, 105.2673515560711337, -4.000000000000001776 ) ) ;
#60827 = CARTESIAN_POINT ( 'NONE',  ( -21.32298952633117395, -39.47768505749013457, 31.13619358448382712 ) ) ;
#60828 = ADVANCED_FACE ( 'NONE', ( #16659 ), #74351, .F. ) ;
#60829 = ADVANCED_FACE ( 'NONE', ( #82456 ), #65119, .F. ) ;
#60831 = CARTESIAN_POINT ( 'NONE',  ( -40.55047790000728014, 438.3493795828572388, 22.65582424288032826 ) ) ;
#60830 = CARTESIAN_POINT ( 'NONE',  ( -0.3376690634117764933, 27.30884096673758776, 40.71517686674960856 ) ) ;
#60832 = ORIENTED_EDGE ( 'NONE', *, *, #15396, .F. ) ;
#60833 = EDGE_CURVE ( 'NONE', #53314, #8468, #43069, .T. ) ;
#60834 = CARTESIAN_POINT ( 'NONE',  ( 0.000000000000000000, 45.00000000000000711, 0.000000000000000000 ) ) ;
#60835 = ORIENTED_EDGE ( 'NONE', *, *, #21865, .T. ) ;
#60836 = CYLINDRICAL_SURFACE ( 'NONE', #89509, 4.000000000000000000 ) ;
#60837 = PLANE ( 'NONE',  #51164 ) ;
#60838 = CARTESIAN_POINT ( 'NONE',  ( -8.679094227360542035, -60.00000000000000000, -42.46732092095059130 ) ) ;
#60839 = VERTEX_POINT ( 'NONE', #100229 ) ;
#60840 = CYLINDRICAL_SURFACE ( 'NONE', #87716, 5.000000000000001776 ) ;
#60841 = CARTESIAN_POINT ( 'NONE',  ( 0.000000000000000000, 0.000000000000000000, 0.000000000000000000 ) ) ;
#60842 = CARTESIAN_POINT ( 'NONE',  ( 99.72099231572487099, -37.83690929057568297, 191.0453301431148248 ) ) ;
#60843 = VECTOR ( 'NONE', #75303, 1000.000000000000000 ) ;
#60845 = DIRECTION ( 'NONE',  ( -1.000000000000000000, -1.224606353822377258E-16, -0.000000000000000000 ) ) ;
#60844 = CARTESIAN_POINT ( 'NONE',  ( 0.000000000000000000, 0.000000000000000000, 0.000000000000000000 ) ) ;
#60846 = ORIENTED_EDGE ( 'NONE', *, *, #54001, .F. ) ;
#60847 = AXIS2_PLACEMENT_3D ( 'NONE', #56252, #39588, #21297 ) ;
#60848 = ORIENTED_EDGE ( 'NONE', *, *, #85871, .T. ) ;
#60849 = AXIS2_PLACEMENT_3D ( 'NONE', #75799, #69322, #76858 ) ;
#60850 = ORIENTED_EDGE ( 'NONE', *, *, #48109, .F. ) ;
#60851 = CARTESIAN_POINT ( 'NONE',  ( 24.60286054134615341, 307.0080087803624451, 10.42432472471663907 ) ) ;
#60852 = DIRECTION ( 'NONE',  ( -1.000000000000000000, -1.224606353822377258E-16, -0.000000000000000000 ) ) ;
#60853 = DIRECTION ( 'NONE',  ( 0.000000000000000000, -1.000000000000000000, 0.000000000000000000 ) ) ;
#60854 = VERTEX_POINT ( 'NONE', #74873 ) ;
#60855 = DIRECTION ( 'NONE',  ( 0.000000000000000000, -1.000000000000000000, 0.000000000000000000 ) ) ;
#60856 = CARTESIAN_POINT ( 'NONE',  ( -5.622681999521890184, 41.99823411347379931, -69.46127173319746362 ) ) ;
#60857 = CARTESIAN_POINT ( 'NONE',  ( 0.000000000000000000, 0.000000000000000000, -10.00000000000000178 ) ) ;
#60858 = CARTESIAN_POINT ( 'NONE',  ( -55.85966931448584916, -60.00000000001456613, -39.08074821196408521 ) ) ;
#60859 = CARTESIAN_POINT ( 'NONE',  ( 0.000000000000000000, 0.000000000000000000, 0.000000000000000000 ) ) ;
#60860 = CARTESIAN_POINT ( 'NONE',  ( 10.50000000000000178, -5.000000000000000000, -12.52300748975612166 ) ) ;
#60861 = FACE_OUTER_BOUND ( 'NONE', #34996, .T. ) ;
#60862 = VECTOR ( 'NONE', #100276, 1000.000000000000000 ) ;
#60863 = CARTESIAN_POINT ( 'NONE',  ( -87.19976908022060513, -14.21045842199435860, -12.72659765151139233 ) ) ;
#60864 = CARTESIAN_POINT ( 'NONE',  ( -8.238951567618261862, 51.66657054343616551, 3.999790829972674544 ) ) ;
#60865 = EDGE_CURVE ( 'NONE', #92963, #58313, #51325, .T. ) ;
#60866 = CARTESIAN_POINT ( 'NONE',  ( -49.15736080366974647, -29.13434467386025872, 46.07356561062454148 ) ) ;
#60867 = VERTEX_POINT ( 'NONE', #57102 ) ;
#60868 = LINE ( 'NONE', #69485, #78012 ) ;
#60869 = ORIENTED_EDGE ( 'NONE', *, *, #85737, .T. ) ;
#60870 = DIRECTION ( 'NONE',  ( 0.000000000000000000, 1.000000000000000000, 0.000000000000000000 ) ) ;
#60871 = CARTESIAN_POINT ( 'NONE',  ( -8.984970058492191214, 294.6717433611603383, -4.394086705153881667 ) ) ;
#60872 = DIRECTION ( 'NONE',  ( 0.000000000000000000, 0.000000000000000000, -1.000000000000000000 ) ) ;
#60873 = VERTEX_POINT ( 'NONE', #90016 ) ;
#60874 = CARTESIAN_POINT ( 'NONE',  ( 5.477578620271504661, 246.8349856098389239, -2.459398706554666525 ) ) ;
#60875 = ORIENTED_EDGE ( 'NONE', *, *, #50931, .F. ) ;
#60876 = CARTESIAN_POINT ( 'NONE',  ( 89.97112945879391077, -29.99999999997625721, -10.10510908212382475 ) ) ;
#60877 = LINE ( 'NONE', #93767, #81255 ) ;
#60878 = CARTESIAN_POINT ( 'NONE',  ( 3.604576940038719979, -48.95215848635503164, 104.3731177596920503 ) ) ;
#60879 = CARTESIAN_POINT ( 'NONE',  ( -4.669235002214947805, -14.10229584173631601, -8.329632653661956709 ) ) ;
#60880 = CARTESIAN_POINT ( 'NONE',  ( -33.52312678242540755, 18.64316884714407152, -19.32152200344674498 ) ) ;
#60881 = CARTESIAN_POINT ( 'NONE',  ( 87.73947420500191186, -29.99999999999999289, 186.1036665454039678 ) ) ;
#60882 = EDGE_CURVE ( 'NONE', #82447, #75804, #33398, .T. ) ;
#60883 = CARTESIAN_POINT ( 'NONE',  ( -1.249887675601815129, 36.80302773944718098, 28.34105814077533481 ) ) ;
#60884 = TOROIDAL_SURFACE ( 'NONE', #48830, 2.000000000000011102, 5.000000000000000000 ) ;
#60885 = ORIENTED_EDGE ( 'NONE', *, *, #26652, .T. ) ;
#60886 = ORIENTED_EDGE ( 'NONE', *, *, #83556, .T. ) ;
#60887 = CARTESIAN_POINT ( 'NONE',  ( 54.96666262631825361, -36.02821829405777976, 58.82418178195225522 ) ) ;
#60888 = CIRCLE ( 'NONE', #14344, 12.00000000000001066 ) ;
#60889 = CARTESIAN_POINT ( 'NONE',  ( 5.383907448094620740, 41.54392475608550939, -58.58678525159944428 ) ) ;
#60890 = CARTESIAN_POINT ( 'NONE',  ( 56.22793774957824553, 6.975173280561618775E-15, 0.000000000000000000 ) ) ;
#60891 = ORIENTED_EDGE ( 'NONE', *, *, #34766, .F. ) ;
#60892 = CARTESIAN_POINT ( 'NONE',  ( -85.46470094257063010, -38.35991919399719308, -22.41886950923507626 ) ) ;
#60893 = ORIENTED_EDGE ( 'NONE', *, *, #87761, .F. ) ;
#60894 = DIRECTION ( 'NONE',  ( 0.000000000000000000, 0.000000000000000000, -1.000000000000000000 ) ) ;
#60895 = CARTESIAN_POINT ( 'NONE',  ( 109.0199404443706612, -38.35645241016953833, 190.0871729485212143 ) ) ;
#60896 = CARTESIAN_POINT ( 'NONE',  ( 10.36345999819431896, 16.99173003315943831, 9.890529223011252924 ) ) ;
#60897 = CARTESIAN_POINT ( 'NONE',  ( 82.62163173485843970, -37.86093661847765901, 4.878488117475526131 ) ) ;
#60898 = CARTESIAN_POINT ( 'NONE',  ( 42.57386119057987628, 361.2124773204089934, 16.59441752729008357 ) ) ;
#60899 = CARTESIAN_POINT ( 'NONE',  ( -20.37278541768182905, 303.8378246129573199, -10.00297115033341910 ) ) ;
#60900 = CARTESIAN_POINT ( 'NONE',  ( 4.337283319710566687, -10.96666117361874093, -10.25672613774106345 ) ) ;
#60901 = B_SPLINE_CURVE_WITH_KNOTS ( 'NONE', 3,
 ( #60158, #94090, #84408, #93023 ),
 .UNSPECIFIED., .F., .F.,
 ( 4, 4 ),
 ( 0.000000000000000000, 1.000000000000000000 ),
 .UNSPECIFIED. ) ;
#60902 = EDGE_CURVE ( 'NONE', #288, #57839, #49129, .T. ) ;
#60903 = CARTESIAN_POINT ( 'NONE',  ( 6.172110426326448795, -1.395451528107565675, 6.499999999999999112 ) ) ;
#60904 =( BOUNDED_SURFACE ( )  B_SPLINE_SURFACE ( 3, 2, ( 
 ( #104420, #71000, #103893 ),
 ( #39708, #80668, #55841 ),
 ( #54800, #32148, #6789 ),
 ( #56381, #23007, #5215 ),
 ( #88782, #72060, #40219 ),
 ( #23539, #80144, #15410 ),
 ( #63997, #64512, #46206 ),
 ( #73089, #46723, #30037 ),
 ( #38145, #31110, #97922 ),
 ( #104969, #65025, #6244 ) ),
 .UNSPECIFIED., .F., .F., .F. ) 
 B_SPLINE_SURFACE_WITH_KNOTS ( ( 4, 2, 2, 2, 4 ),
 ( 3, 3 ),
 ( 0.009720546615277408931, 0.01966181957347580903, 0.02463245605257501081, 0.02711777429212460996, 0.02960309253167420912 ),
 ( 0.000000000000000000, 1.000000000000000000 ),
 .UNSPECIFIED. ) 
 GEOMETRIC_REPRESENTATION_ITEM ( )  RATIONAL_B_SPLINE_SURFACE ( (
 ( 1.000000000000000000, 0.7071067811865475727, 1.000000000000000000),
 ( 1.000000000000000000, 0.7071067811865475727, 1.000000000000000000),
 ( 1.000000000000000000, 0.7071032135351020820, 1.000000000000000000),
 ( 1.000000000000000000, 0.7071081509336487603, 1.000000000000000000),
 ( 1.000000000000000000, 0.7071048030563258369, 1.000000000000000000),
 ( 1.000000000000000000, 0.7071073475032796374, 1.000000000000000000),
 ( 1.000000000000000000, 0.7070920504567346221, 1.000000000000000000),
 ( 1.000000000000000000, 0.7070828650738152366, 1.000000000000000000),
 ( 1.000000000000000000, 0.7071010094004099855, 1.000000000000000000),
 ( 1.000000000000000000, 0.7071067811865505703, 1.000000000000000000) ) ) 
 REPRESENTATION_ITEM ( '' )  SURFACE ( )  );
#60905 = SURFACE_STYLE_USAGE ( .BOTH. , #36131 ) ;
#60906 = CARTESIAN_POINT ( 'NONE',  ( 8.830661707065113220, 133.7962572603239551, 5.000000000000614619 ) ) ;
#60907 = ORIENTED_EDGE ( 'NONE', *, *, #10578, .T. ) ;
#60908 = EDGE_CURVE ( 'NONE', #26579, #58946, #15714, .T. ) ;
#60909 = FACE_OUTER_BOUND ( 'NONE', #99332, .T. ) ;
#60910 = CARTESIAN_POINT ( 'NONE',  ( 7.113472013431289653, 40.00000000359433017, -71.00901315851923812 ) ) ;
#60911 = CARTESIAN_POINT ( 'NONE',  ( 0.000000000000000000, -50.00000000000000000, 45.00000000000000000 ) ) ;
#60913 = EDGE_CURVE ( 'NONE', #67484, #78737, #4083, .T. ) ;
#60912 = ORIENTED_EDGE ( 'NONE', *, *, #47847, .T. ) ;
#60914 = CARTESIAN_POINT ( 'NONE',  ( -18.99999999999999289, -4.000000000000000000, 25.00000000000000000 ) ) ;
#60915 = CARTESIAN_POINT ( 'NONE',  ( -36.39696100913531751, 309.1476423045306774, 13.34792222534698780 ) ) ;
#60916 = CARTESIAN_POINT ( 'NONE',  ( 3.337161262018383995E-15, 37.21016666119768246, 27.25000000000000000 ) ) ;
#60917 = CARTESIAN_POINT ( 'NONE',  ( 0.000000000000000000, 0.000000000000000000, 4.000000000000000000 ) ) ;
#60918 = CARTESIAN_POINT ( 'NONE',  ( -1.469576158976823947E-15, -23.37499999999999289, 8.000000000000000000 ) ) ;
#60919 = CARTESIAN_POINT ( 'NONE',  ( 1.154068430507904086, -12.55449340960651483, 32.19352746017464284 ) ) ;
#60920 = CARTESIAN_POINT ( 'NONE',  ( 98.31310517497099966, -5.000000000000000888, 6.123233995736779101E-16 ) ) ;
#60921 = ORIENTED_EDGE ( 'NONE', *, *, #91080, .F. ) ;
#60922 = CARTESIAN_POINT ( 'NONE',  ( 84.92621421947670513, -39.36226118941799967, 183.3512328336199744 ) ) ;
#60923 = DIRECTION ( 'NONE',  ( 0.000000000000000000, 1.000000000000000000, 0.000000000000000000 ) ) ;
#60924 = DIRECTION ( 'NONE',  ( 0.000000000000000000, -1.000000000000000000, 0.000000000000000000 ) ) ;
#60925 = ORIENTED_EDGE ( 'NONE', *, *, #47647, .T. ) ;
#60926 = VECTOR ( 'NONE', #10141, 1000.000000000000000 ) ;
#60927 = ADVANCED_FACE ( 'NONE', ( #68953 ), #104766, .T. ) ;
#60928 = CARTESIAN_POINT ( 'NONE',  ( -85.46379202683773713, -37.82125448877485496, 49.13329909993041156 ) ) ;
#60929 = CARTESIAN_POINT ( 'NONE',  ( -13.73780227957324129, -5.000000000000002665, -78.37846873786800472 ) ) ;
#60930 = CARTESIAN_POINT ( 'NONE',  ( 15.63139425945679228, 304.5550792278134509, 8.873930317195700468 ) ) ;
#60931 = CARTESIAN_POINT ( 'NONE',  ( 8.099999999999999645, -7.505553499465148271, 0.000000000000000000 ) ) ;
#60932 = AXIS2_PLACEMENT_3D ( 'NONE', #28629, #61513, #3792 ) ;
#60933 =( BOUNDED_SURFACE ( )  B_SPLINE_SURFACE ( 3, 2, ( 
 ( #2413, #68227, #8908 ),
 ( #83332, #66623, #84939 ),
 ( #100049, #101118, #60163 ),
 ( #76836, #27281, #93027 ) ),
 .UNSPECIFIED., .F., .F., .F. ) 
 B_SPLINE_SURFACE_WITH_KNOTS ( ( 4, 4 ),
 ( 3, 3 ),
 ( 2.810685711951421695E-15, 0.0002131933143105659131 ),
 ( 0.000000000000000000, 1.000000000000000000 ),
 .UNSPECIFIED. ) 
 GEOMETRIC_REPRESENTATION_ITEM ( )  RATIONAL_B_SPLINE_SURFACE ( (
 ( 1.000000000000000000, 0.8328393170029404491, 1.000000000000000000),
 ( 1.000000000000000000, 0.8339687546429958021, 1.000000000000000000),
 ( 1.000000000000000000, 0.8350496135189969804, 1.000000000000000000),
 ( 1.000000000000000000, 0.8360809698955812275, 1.000000000000000000) ) ) 
 REPRESENTATION_ITEM ( '' )  SURFACE ( )  );
#60934 = CARTESIAN_POINT ( 'NONE',  ( 29.99506149210614581, -60.00000000000000711, 43.03431844238033221 ) ) ;
#60935 = CARTESIAN_POINT ( 'NONE',  ( 27.15809507750037710, -30.51936720628422961, 39.13764639798584000 ) ) ;
#60936 = CARTESIAN_POINT ( 'NONE',  ( 1.993516955649224487, -0.1166279987392843664, 102.1895970170251644 ) ) ;
#60937 = CARTESIAN_POINT ( 'NONE',  ( 41.55968476715275273, -26.98253679743242017, 37.03168355540274348 ) ) ;
#60939 = CARTESIAN_POINT ( 'NONE',  ( -10.06321370107148816, 14.98786682347728672, 10.39688774717462039 ) ) ;
#60938 = CARTESIAN_POINT ( 'NONE',  ( -30.01214130291127802, -32.45876557533858175, 40.58130538435680990 ) ) ;
#60940 = CARTESIAN_POINT ( 'NONE',  ( 1.488823952408661500, 295.3362597639684850, -10.00085782936185730 ) ) ;
#60941 = CARTESIAN_POINT ( 'NONE',  ( 35.96492786661492858, 302.4488314805894902, -8.278427239160079054 ) ) ;
#60942 = DIRECTION ( 'NONE',  ( 0.000000000000000000, -1.000000000000000000, 0.000000000000000000 ) ) ;
#60943 = ORIENTED_EDGE ( 'NONE', *, *, #21486, .F. ) ;
#60944 = CARTESIAN_POINT ( 'NONE',  ( -6.624059643703564149, 294.7379298340728724, -10.02420444108935271 ) ) ;
#60945 = CARTESIAN_POINT ( 'NONE',  ( -17.49999999999997513, 51.99999999999981526, 59.56761335716019801 ) ) ;
#60946 = CIRCLE ( 'NONE', #74696, 8.000000000000000000 ) ;
#60947 = ORIENTED_EDGE ( 'NONE', *, *, #17733, .F. ) ;
#60948 = CARTESIAN_POINT ( 'NONE',  ( -11.48322309281289044, -1.563619715725306891, 20.53900286216184057 ) ) ;
#60949 = FACE_OUTER_BOUND ( 'NONE', #19699, .T. ) ;
#60950 = EDGE_CURVE ( 'NONE', #49860, #64798, #54285, .T. ) ;
#60951 = CARTESIAN_POINT ( 'NONE',  ( 0.000000000000000000, 0.000000000000000000, 0.000000000000000000 ) ) ;
#60952 = AXIS2_PLACEMENT_3D ( 'NONE', #38638, #12737, #55313 ) ;
#60953 = ADVANCED_FACE ( 'NONE', ( #18830 ), #94476, .F. ) ;
#60955 = CARTESIAN_POINT ( 'NONE',  ( 4.642985192297872210, -21.77036161962056937, -30.46305366977244944 ) ) ;
#60954 = FILL_AREA_STYLE_COLOUR ( '', #101802 ) ;
#60956 = PRESENTATION_LAYER_ASSIGNMENT (  '', '', ( #73001 ) ) ;
#60957 = ORIENTED_EDGE ( 'NONE', *, *, #83379, .F. ) ;
#60958 = CIRCLE ( 'NONE', #28266, 5.000000000000010658 ) ;
#60959 = CARTESIAN_POINT ( 'NONE',  ( 27.86763638067955640, 36.37524770582945877, 9.811230206501790008 ) ) ;
#60960 = CYLINDRICAL_SURFACE ( 'NONE', #16982, 8.000000000000000000 ) ;
#60961 = ORIENTED_EDGE ( 'NONE', *, *, #55410, .F. ) ;
#60962 = EDGE_CURVE ( 'NONE', #18921, #72570, #3142, .T. ) ;
#60963 = DIRECTION ( 'NONE',  ( 0.000000000000000000, -1.000000000000000000, 0.000000000000000000 ) ) ;
#60964 = CARTESIAN_POINT ( 'NONE',  ( -5.902962327514317487, 41.87327319969161010, -59.02279321040224147 ) ) ;
#60965 = CARTESIAN_POINT ( 'NONE',  ( -92.23009394491774060, -59.99999999999999289, 2.477879558583810038 ) ) ;
#60966 = ORIENTED_EDGE ( 'NONE', *, *, #6280, .F. ) ;
#60967 = CARTESIAN_POINT ( 'NONE',  ( -3.313708498984746065, -24.96874999999998934, 8.000000000000017764 ) ) ;
#60968 = DIRECTION ( 'NONE',  ( -1.000000000000000000, -0.000000000000000000, -0.000000000000000000 ) ) ;
#60969 = CARTESIAN_POINT ( 'NONE',  ( 0.000000000000000000, -14.49999999999999822, 0.000000000000000000 ) ) ;
#60970 = DIRECTION ( 'NONE',  ( -1.000000000000000000, -1.224606353822377258E-16, -0.000000000000000000 ) ) ;
#60972 = SURFACE_STYLE_FILL_AREA ( #100870 ) ;
#60971 = CARTESIAN_POINT ( 'NONE',  ( 0.000000000000000000, 0.000000000000000000, -6.123524522925831270 ) ) ;
#60973 = CARTESIAN_POINT ( 'NONE',  ( -81.51997760136781324, -49.94239916794347067, 172.6801288724093979 ) ) ;
#60974 = ORIENTED_EDGE ( 'NONE', *, *, #105179, .F. ) ;
#60975 = CARTESIAN_POINT ( 'NONE',  ( -8.521411446768031084, 0.000000000000000000, -14.76969908562668721 ) ) ;
#60976 = ORIENTED_EDGE ( 'NONE', *, *, #40478, .F. ) ;
#60977 = ORIENTED_EDGE ( 'NONE', *, *, #89658, .T. ) ;
#60978 = CARTESIAN_POINT ( 'NONE',  ( 9.117185603066571886, -4.332661967060696284, -15.39580070564444014 ) ) ;
#60979 = CARTESIAN_POINT ( 'NONE',  ( 10.28624191511809371, -1.200000000000000030E-05, -14.15779740156171584 ) ) ;
#60980 = SURFACE_STYLE_FILL_AREA ( #78720 ) ;
#60981 = VERTEX_POINT ( 'NONE', #52206 ) ;
#60982 = CIRCLE ( 'NONE', #48853, 4.000000000000001776 ) ;
#60983 = DIRECTION ( 'NONE',  ( -1.000000000000000000, -1.224606353822377258E-16, -0.000000000000000000 ) ) ;
#60984 = CARTESIAN_POINT ( 'NONE',  ( -94.73097995338159194, -57.65973493957909568, -7.453110678737913553 ) ) ;
#60985 = CARTESIAN_POINT ( 'NONE',  ( -4.472135954999578722, -65.00000000000000000, -4.000000000000002665 ) ) ;
#60986 = CARTESIAN_POINT ( 'NONE',  ( 21.08349330513380337, 4.898587196589405926E-16, -4.000000000000001776 ) ) ;
#60987 = CARTESIAN_POINT ( 'NONE',  ( -9.842984802582135373, 101.4093040952434563, 1.781981959250506842 ) ) ;
#60988 = DIRECTION ( 'NONE',  ( -1.000000000000000000, -0.000000000000000000, -0.000000000000000000 ) ) ;
#60989 = CARTESIAN_POINT ( 'NONE',  ( 4.582575694955843382, 15.00000000000000000, -9.999999999999998224 ) ) ;
#60990 = CARTESIAN_POINT ( 'NONE',  ( 108.2372837266210297, -59.99999999999997868, 115.4707114838127211 ) ) ;
#60991 = CARTESIAN_POINT ( 'NONE',  ( -102.9006728679688365, -30.00000000000001421, 197.6531887663732618 ) ) ;
#60992 = EDGE_CURVE ( 'NONE', #70408, #98268, #27457, .T. ) ;
#60993 = CARTESIAN_POINT ( 'NONE',  ( -55.56343265448107616, -22.15138794996349247, 54.53997454549021739 ) ) ;
#60994 = ORIENTED_EDGE ( 'NONE', *, *, #63933, .F. ) ;
#60995 = CARTESIAN_POINT ( 'NONE',  ( 37.56673239365870387, -1.200000000000000030E-05, 12.20617127780998956 ) ) ;
#60996 = ORIENTED_EDGE ( 'NONE', *, *, #24281, .F. ) ;
#60997 = CARTESIAN_POINT ( 'NONE',  ( -104.5556233096705938, -52.71023842945449189, 183.8341536945831081 ) ) ;
#60998 = DIRECTION ( 'NONE',  ( -0.000000000000000000, -1.000000000000000000, -0.000000000000000000 ) ) ;
#60999 = COLOUR_RGB ( '', 0.09019608, 0.27058824, 0.51372549) ;
#61000 = CARTESIAN_POINT ( 'NONE',  ( 3.313708498984762496, -18.96875000409677270, 7.999999999999998224 ) ) ;
#61001 = EDGE_CURVE ( 'NONE', #6808, #96464, #42719, .T. ) ;
#61002 = CARTESIAN_POINT ( 'NONE',  ( 15.47979971815697908, 42.57621410692647146, -89.21879381463644165 ) ) ;
#61003 = VERTEX_POINT ( 'NONE', #76481 ) ;
#61004 = CARTESIAN_POINT ( 'NONE',  ( 5.902907888931476776, -4.999999999999999112, -73.20788160635341058 ) ) ;
#61005 = CIRCLE ( 'NONE', #67916, 0.9999999999999854561 ) ;
#61006 = DIRECTION ( 'NONE',  ( 0.000000000000000000, 0.000000000000000000, -1.000000000000000000 ) ) ;
#61007 = CARTESIAN_POINT ( 'NONE',  ( 37.24617447230036049, 25.58981836295230750, -13.42464766883425931 ) ) ;
#61008 = CARTESIAN_POINT ( 'NONE',  ( 7.188101187499999156, -16.62500000204838457, 2.977408999572654924 ) ) ;
#61009 = CYLINDRICAL_SURFACE ( 'NONE', #46467, 4.000000000000000888 ) ;
#61010 = DIRECTION ( 'NONE',  ( 0.5735764363510491570, -0.8191520442889895781, 1.003171929053522035E-16 ) ) ;
#61011 = DIRECTION ( 'NONE',  ( 0.000000000000000000, 0.000000000000000000, -1.000000000000000000 ) ) ;
#61012 = CARTESIAN_POINT ( 'NONE',  ( -27.97565635352651015, 315.9216507687758053, 12.64980990155120999 ) ) ;
#61013 = DIRECTION ( 'NONE',  ( 0.000000000000000000, 0.000000000000000000, 1.000000000000000000 ) ) ;
#61014 = CARTESIAN_POINT ( 'NONE',  ( -8.466070237930688691, 27.19802938155146421, 0.000000000000000000 ) ) ;
#61015 = EDGE_CURVE ( 'NONE', #89525, #56748, #2590, .T. ) ;
#61016 = CARTESIAN_POINT ( 'NONE',  ( -15.56661972382054948, 46.04807679453923441, -6.063442319127702262 ) ) ;
#61017 = CARTESIAN_POINT ( 'NONE',  ( -31.20798807302101707, -25.60670629028073719, 31.04078863611647421 ) ) ;
#61018 = DIRECTION ( 'NONE',  ( -1.000000000000000000, -1.224606353822377258E-16, -0.000000000000000000 ) ) ;
#61019 = CARTESIAN_POINT ( 'NONE',  ( 48.04108913913790246, -39.52162123606319000, 47.68945014315683295 ) ) ;
#61020 = CARTESIAN_POINT ( 'NONE',  ( -32.65915130202685646, 487.2382554987376579, 8.056573295088265141 ) ) ;
#61021 = CARTESIAN_POINT ( 'NONE',  ( -7.550180524134852078, 88.00559247213188030, 2.651855549982491400 ) ) ;
#61022 = CARTESIAN_POINT ( 'NONE',  ( -85.61943167051258285, -38.66581993764706482, 198.8511778627555771 ) ) ;
#61023 = ORIENTED_EDGE ( 'NONE', *, *, #48976, .F. ) ;
#61025 = CARTESIAN_POINT ( 'NONE',  ( -28.08712643177169355, 36.49724380641310262, 8.016830452732861545 ) ) ;
#61024 = CARTESIAN_POINT ( 'NONE',  ( -16.11717644235027791, 21.56691778980941621, 2.165075456531270870 ) ) ;
#61026 = CARTESIAN_POINT ( 'NONE',  ( 13.03070029080557646, 4.293758741504203336, -7.331204502238938048 ) ) ;
#61027 = CARTESIAN_POINT ( 'NONE',  ( -19.30670087550686986, 49.86676902829839264, 61.31490456933869382 ) ) ;
#61028 = DIRECTION ( 'NONE',  ( 1.000000000000000000, 0.000000000000000000, -0.000000000000000000 ) ) ;
#61029 = CARTESIAN_POINT ( 'NONE',  ( 6.455413918329012013, 41.05104878809925850, -71.04266228314376974 ) ) ;
#61030 = CARTESIAN_POINT ( 'NONE',  ( -32.82257518192243140, 434.5279504693334616, 16.69869453570042239 ) ) ;
#61031 = LINE ( 'NONE', #59437, #63789 ) ;
#61032 = DIRECTION ( 'NONE',  ( 1.000000000000000000, 0.000000000000000000, 0.000000000000000000 ) ) ;
#61033 = CARTESIAN_POINT ( 'NONE',  ( 106.6542038942911148, -59.99999999999999289, 197.5365053951335312 ) ) ;
#61034 = COLOUR_RGB ( '', 0.09019608, 0.27058824, 0.51372549) ;
#61035 = CARTESIAN_POINT ( 'NONE',  ( -6.943482370013977167, -65.52848370260726085, 3.973876482044368164 ) ) ;
#61036 = ORIENTED_EDGE ( 'NONE', *, *, #87186, .T. ) ;
#61037 = EDGE_CURVE ( 'NONE', #30981, #80889, #32421, .T. ) ;
#61038 = CARTESIAN_POINT ( 'NONE',  ( 1.545731922506614175, -49.97157980004173083, 101.5782547351728624 ) ) ;
#61039 = COLOUR_RGB ( '', 0.31764706, 0.68627451, 0.89019608) ;
#61040 = CARTESIAN_POINT ( 'NONE',  ( -81.47582811281075976, -30.00000000000000711, -9.499132834538738024 ) ) ;
#61041 = ORIENTED_EDGE ( 'NONE', *, *, #34419, .T. ) ;
#61043 = CARTESIAN_POINT ( 'NONE',  ( 5.282975838324663442, 16.24034189271231909, -35.83174429344832390 ) ) ;
#61042 = CARTESIAN_POINT ( 'NONE',  ( -78.70717280597565946, -38.65874930792139708, 190.2476505887177325 ) ) ;
#61044 = FACE_OUTER_BOUND ( 'NONE', #92459, .T. ) ;
#61045 = CARTESIAN_POINT ( 'NONE',  ( 4.403473400622099021, 6.117907484625860093, 2.340352033263631048E-15 ) ) ;
#61046 = CARTESIAN_POINT ( 'NONE',  ( 4.651269564039822946, -4.999999999999991118, -15.66707428873065311 ) ) ;
#61047 = CARTESIAN_POINT ( 'NONE',  ( 2.977408999572651815, -13.81250000204838280, 7.188101187500000933 ) ) ;
#61048 = DIRECTION ( 'NONE',  ( 0.000000000000000000, -1.000000000000000000, 0.000000000000000000 ) ) ;
#61050 = ORIENTED_EDGE ( 'NONE', *, *, #92666, .T. ) ;
#61049 = LINE ( 'NONE', #78797, #83973 ) ;
#61051 = CARTESIAN_POINT ( 'NONE',  ( 84.11707923628694061, -32.48599780003080184, 169.3644224162934790 ) ) ;
#61052 = CARTESIAN_POINT ( 'NONE',  ( -46.00000000004283152, 462.0224066507940961, 5.460670579100258770 ) ) ;
#61053 = CARTESIAN_POINT ( 'NONE',  ( 6.815830331203684977, 1.210606185736183200E-13, -6.171384342982610072 ) ) ;
#61054 = ORIENTED_EDGE ( 'NONE', *, *, #90079, .T. ) ;
#61055 = CYLINDRICAL_SURFACE ( 'NONE', #104779, 5.000000000000002665 ) ;
#61056 = CARTESIAN_POINT ( 'NONE',  ( 28.86650669486618881, 1.474610560812782335E-15, 0.000000000000000000 ) ) ;
#61057 = CARTESIAN_POINT ( 'NONE',  ( 0.000000000000000000, -6.505213034913025026E-15, -10.00000000000000178 ) ) ;
#61058 = CARTESIAN_POINT ( 'NONE',  ( 61.11682663846713837, 6.975173280561618775E-15, 0.000000000000000000 ) ) ;
#61059 = CARTESIAN_POINT ( 'NONE',  ( -29.59409995734550236, 13.24979100942360688, -39.60535821593476413 ) ) ;
#61060 = CARTESIAN_POINT ( 'NONE',  ( 17.62488890706315914, 43.36868375057044744, 4.616903831776418166 ) ) ;
#61061 = CARTESIAN_POINT ( 'NONE',  ( 5.385673916453010968, -2.602085213965210642E-15, 15.34388420865771607 ) ) ;
#61062 = ORIENTED_EDGE ( 'NONE', *, *, #62847, .F. ) ;
#61063 = STYLED_ITEM ( 'NONE', ( #8444 ), #61803 ) ;
#61064 = FILL_AREA_STYLE ('',( #35752 ) ) ;
#61065 = CARTESIAN_POINT ( 'NONE',  ( -4.406980464011021503, 299.0165906089773671, 8.990614526116086580 ) ) ;
#61066 = CARTESIAN_POINT ( 'NONE',  ( -5.000000000000000000, -30.71019771943890575, -0.3346393655629185671 ) ) ;
#61067 = CARTESIAN_POINT ( 'NONE',  ( 0.000000000000000000, 23.58303312036771615, 0.000000000000000000 ) ) ;
#61068 = DIRECTION ( 'NONE',  ( 0.000000000000000000, 1.000000000000000000, -0.000000000000000000 ) ) ;
#61069 = AXIS2_PLACEMENT_3D ( 'NONE', #93671, #19823, #69921 ) ;
#61070 = CARTESIAN_POINT ( 'NONE',  ( -5.082755093536325042, -26.09375000204838813, -5.082755093536325930 ) ) ;
#61071 = CARTESIAN_POINT ( 'NONE',  ( 33.52307692307692122, 1.411358822780289120E-15, 0.000000000000000000 ) ) ;
#61072 = AXIS2_PLACEMENT_3D ( 'NONE', #39388, #14013, #49977 ) ;
#61073 = STYLED_ITEM ( 'NONE', ( #8130 ), #55270 ) ;
#61074 = CARTESIAN_POINT ( 'NONE',  ( 0.000000000000000000, 152.0000000000000000, 5.000000000000000000 ) ) ;
#61075 = CARTESIAN_POINT ( 'NONE',  ( 0.000000000000000000, -19.99999999999998934, 0.000000000000000000 ) ) ;
#61076 = CIRCLE ( 'NONE', #47263, 5.000000000000011546 ) ;
#61077 = ITEM_DEFINED_TRANSFORMATION ( 'NONE', 'NONE', #81700,  #10728 ) ;
#61078 = ORIENTED_EDGE ( 'NONE', *, *, #88829, .T. ) ;
#61079 = DIRECTION ( 'NONE',  ( 0.000000000000000000, -1.000000000000000000, 0.000000000000000000 ) ) ;
#61080 = CARTESIAN_POINT ( 'NONE',  ( -9.737904751879213450, 8.235624462056064132, 0.000000000000000000 ) ) ;
#61081 = DIRECTION ( 'NONE',  ( -0.5735764363510494901, -0.8191520442889894671, 0.000000000000000000 ) ) ;
#61082 = EDGE_CURVE ( 'NONE', #25507, #19124, #104896, .T. ) ;
#61083 = ORIENTED_EDGE ( 'NONE', *, *, #56058, .F. ) ;
#61084 = ORIENTED_EDGE ( 'NONE', *, *, #70339, .T. ) ;
#61085 = EDGE_CURVE ( 'NONE', #85509, #26511, #106442, .T. ) ;
#61086 =( BOUNDED_SURFACE ( )  B_SPLINE_SURFACE ( 2, 3, ( 
 ( #69622, #44279, #93890, #88455, #56043, #32358, #6980, #54993, #15605, #88978, #5918, #87924, #104622, #48495, #31817, #97573, #47439, #38844, #14004, #40418, #90032, #98122, #64701, #23203, #39898, #23739, #73298, #63114, #81390, #72772, #106194, #65230, #79815, #30227, #80332, #24270, #31301, #71708, #56590, #7500, #39380, #89512, #57118, #6445, #16138, #80870, #22678, #30772, #72258, #49026, #63658, #96546, #105678, #96015, #46913, #81923, #8043, #64188, #97057, #40954, #104088, #22142, #55515, #14531, #105159, #15077, #47962, #91642, #34502, #50102, #84611, #83007, #9630, #41480, #33960, #42539, #82477, #66830, #42010, #18848, #99721, #75442, #74893, #50611, #49569, #74368, #59813, #66289, #10695, #25890, #100776, #99173, #59278, #8578, #51153, #106739, #446, #65762, #100247, #33415, #91121, #25332, #17755, #92692, #98643, #1535, #51693, #58195, #92153, #26939, #83529, #24793, #17230, #67367, #75976, #9102, #977, #84071, #58747, #26412, #18298, #67888, #10171, #43087, #2071, #35023, #73845, #57647, #32888, #90567, #16678, #27478, #44152, #94843, #78103, #37155, #93766, #52224, #60355, #86753, #29595, #37693 ),
 ( #93230, #12299, #86227, #19392, #69493, #77041, #45227, #77583, #35559, #20988, #70557, #68433, #11226, #45743, #21494, #4754, #11761, #85135, #70019, #62465, #4221, #101845, #54330, #60876, #12823, #3158, #102379, #36102, #36627, #68972, #102918, #28007, #28531, #87273, #43609, #76501, #19923, #61950, #52765, #94303, #78620, #61411, #20466, #85685, #53821, #44696, #53308, #3701, #29085, #103444, #95356, #2610, #101326, #14408, #47320, #48379, #5802, #22566, #80216, #6863, #72136, #57001, #105045, #38725, #39788, #64588, #88335, #81274, #46800, #31186, #56468, #6321, #105561, #5291, #71592, #104498, #47842, #64071, #97459, #24156, #72663, #13351, #39261, #31700, #23616, #7386, #40300, #89398, #65106, #15492, #73173, #38212, #106078, #96946, #103963, #55404, #79162, #32227, #98003, #23079, #46278, #62997, #88859, #55917, #95893, #14948, #13883, #80748, #71073, #30107, #22019, #54874, #87804, #79693, #30646, #63534, #96431, #58068, #73718, #83411, #1952, #58623, #41360, #100657, #329, #26295, #98528, #41889, #106621, #82887, #32771, #17639, #65643, #8985, #67770, #26818, #89915, #49443, #1413, #74253, #33834, #59155 ),
 ( #74777, #16559, #24674, #857, #57527, #90993, #90448, #17103, #49979, #18172, #82352, #99047, #66707, #9509, #99589, #16022, #25765, #8459, #42422, #34377, #91523, #51033, #33293, #50499, #92038, #75315, #67249, #81797, #66164, #25214, #100128, #83946, #10058, #48902, #42966, #7923, #75858, #34905, #40827, #53706, #86638, #12176, #4639, #69900, #76919, #12702, #19281, #69378, #45108, #28408, #84490, #60239, #102798, #61282, #37570, #59691, #94726, #94177, #37032, #4104, #76376, #86106, #28959, #93650, #101202, #61830, #3030, #35437, #11101, #70435, #60762, #20872, #35980, #45631, #52107, #102259, #77987, #20343, #10583, #93107, #78506, #53189, #103330, #92570, #18721, #51575, #43499, #2487, #68308, #27360, #85017, #19798, #44027, #68851, #101727, #27895, #52634, #85566, #11642, #44572, #77462, #3573, #36510, #13234, #71471, #95243, #47722, #15365, #38608, #48250, #79047, #104927, #72015, #5166, #55280, #29991, #31067, #63420, #21375, #80621, #56336, #54213, #103846, #31583, #7262, #97337, #104371, #46159, #22961, #81151, #63944, #87683, #40173, #46672, #72537, #38095, #88209, #70955, #22440, #62877, #96831, #95768 ) ),
 .UNSPECIFIED., .F., .F., .T. ) 
 B_SPLINE_SURFACE_WITH_KNOTS ( ( 3, 3 ),
 ( 4, 2, 2, 2, 2, 2, 2, 2, 2, 2, 2, 2, 2, 2, 2, 2, 2, 2, 2, 2, 2, 2, 2, 2, 2, 2, 2, 2, 2, 2, 2, 2, 2, 2, 2, 2, 2, 2, 2, 2, 2, 2, 2, 2, 2, 2, 2, 2, 2, 2, 2, 2, 2, 2, 2, 2, 2, 2, 2, 2, 2, 2, 2, 2, 2, 2, 2, 2, 2, 2, 4 ),
 ( 0.000000000000000000, 1.000000000000000000 ),
 ( 0.000000000000000000, 0.002867805938563325763, 0.005735611877126651527, 0.007169514846408315059, 0.008603417815689977724, 0.01003732078497164039, 0.01075427226961247172, 0.01147122375425330305, 0.01182969949657371872, 0.01218817523889413612, 0.01290512672353496745, 0.01433902969281663012, 0.01577293266209829278, 0.01720683563137995545, 0.02007464156994328078, 0.02294244750850660611, 0.02867805938563326024, 0.03441367126275991090, 0.04588489501701321222, 0.06882734252551982179, 0.09176979003402642443, 0.1376546850510396436, 0.1605971325595462462, 0.1720683563137995475, 0.1835395800680528489, 0.1950108038223061779, 0.2007464156994328286, 0.2064820275765594793, 0.2093498335151228185, 0.2107837364844044603, 0.2122176394536861299, 0.2129345909383269508, 0.2136515424229677995, 0.2140100181652881961, 0.2141892560364483944, 0.2143684939076086204, 0.2144581128431887196, 0.2145029223109787830, 0.2145477317787688465, 0.2147269696499290448, 0.2149062075210892431, 0.2150854453922494414, 0.2158023968768902900, 0.2165193483615311110, 0.2172362998461719319, 0.2179532513308127806, 0.2193871543000944502, 0.2201041057847352711, 0.2208210572693761198, 0.2215380087540169407, 0.2222549602386577616, 0.2224341981098179599, 0.2226134359809781860, 0.2229719117232986103, 0.2236888632079394312, 0.2244058146925802522, 0.2251227661772211008, 0.2265566691465027427, 0.2294244750850660819, 0.2322922810236294211, 0.2351600869621927326, 0.2408956988393193832, 0.2466313107164460339, 0.2523669225935726845, 0.2638381463478259858, 0.2753093701020792872, 0.3211942651190924924, 0.3326654888733457938, 0.3441367126275990951, 0.3556079363818523964, 0.3670791601361056977 ),
 .UNSPECIFIED. ) 
 GEOMETRIC_REPRESENTATION_ITEM ( )  RATIONAL_B_SPLINE_SURFACE ( (
 ( 1.000000000000000000, 1.000000000000000000, 1.000000000000000000, 1.000000000000000000, 1.000000000000000000, 1.000000000000000000, 1.000000000000000000, 1.000000000000000000, 1.000000000000000000, 1.000000000000000000, 1.000000000000000000, 1.000000000000000000, 1.000000000000000000, 1.000000000000000000, 1.000000000000000000, 1.000000000000000000, 1.000000000000000000, 1.000000000000000000, 1.000000000000000000, 1.000000000000000000, 1.000000000000000000, 1.000000000000000000, 1.000000000000000000, 1.000000000000000000, 1.000000000000000000, 1.000000000000000000, 1.000000000000000000, 1.000000000000000000, 1.000000000000000000, 1.000000000000000000, 1.000000000000000000, 1.000000000000000000, 1.000000000000000000, 1.000000000000000000, 1.000000000000000000, 1.000000000000000000, 1.000000000000000000, 1.000000000000000000, 1.000000000000000000, 1.000000000000000000, 1.000000000000000000, 1.000000000000000000, 1.000000000000000000, 1.000000000000000000, 1.000000000000000000, 1.000000000000000000, 1.000000000000000000, 1.000000000000000000, 1.000000000000000000, 1.000000000000000000, 1.000000000000000000, 1.000000000000000000, 1.000000000000000000, 1.000000000000000000, 1.000000000000000000, 1.000000000000000000, 1.000000000000000000, 1.000000000000000000, 1.000000000000000000, 1.000000000000000000, 1.000000000000000000, 1.000000000000000000, 1.000000000000000000, 1.000000000000000000, 1.000000000000000000, 1.000000000000000000, 1.000000000000000000, 1.000000000000000000, 1.000000000000000000, 1.000000000000000000, 1.000000000000000000, 1.000000000000000000, 1.000000000000000000, 1.000000000000000000, 1.000000000000000000, 1.000000000000000000, 1.000000000000000000, 1.000000000000000000, 1.000000000000000000, 1.000000000000000000, 1.000000000000000000, 1.000000000000000000, 1.000000000000000000, 1.000000000000000000, 1.000000000000000000, 1.000000000000000000, 1.000000000000000000, 1.000000000000000000, 1.000000000000000000, 1.000000000000000000, 1.000000000000000000, 1.000000000000000000, 1.000000000000000000, 1.000000000000000000, 1.000000000000000000, 1.000000000000000000, 1.000000000000000000, 1.000000000000000000, 1.000000000000000000, 1.000000000000000000, 1.000000000000000000, 1.000000000000000000, 1.000000000000000000, 1.000000000000000000, 1.000000000000000000, 1.000000000000000000, 1.000000000000000000, 1.000000000000000000, 1.000000000000000000, 1.000000000000000000, 1.000000000000000000, 1.000000000000000000, 1.000000000000000000, 1.000000000000000000, 1.000000000000000000, 1.000000000000000000, 1.000000000000000000, 1.000000000000000000, 1.000000000000000000, 1.000000000000000000, 1.000000000000000000, 1.000000000000000000, 1.000000000000000000, 1.000000000000000000, 1.000000000000000000, 1.000000000000000000, 1.000000000000000000, 1.000000000000000000, 1.000000000000000000, 1.000000000000000000, 1.000000000000000000, 1.000000000000000000, 1.000000000000000000, 1.000000000000000000, 1.000000000000000000, 1.000000000000000000, 1.000000000000000000, 1.000000000000000000, 1.000000000000000000, 1.000000000000000000, 1.000000000000000000, 1.000000000000000000),
 ( 1.857142857142858317, 1.857142857142858317, 1.857142857142858317, 1.857142857142858317, 1.857142857142858317, 1.857142857142858317, 1.857142857142858317, 1.857142857142858317, 1.857142857142858317, 1.857142857142858317, 1.857142857142858317, 1.857142857142858317, 1.857142857142858317, 1.857142857142858317, 1.857142857142858317, 1.857142857142858317, 1.857142857142858317, 1.857142857142858317, 1.857142857142858317, 1.857142857142858317, 1.857142857142858317, 1.857142857142858317, 1.857142857142858317, 1.857142857142858317, 1.857142857142858317, 1.857142857142858317, 1.857142857142858317, 1.857142857142858317, 1.857142857142858317, 1.857142857142858317, 1.857142857142858317, 1.857142857142858317, 1.857142857142858317, 1.857142857142858317, 1.857142857142858317, 1.857142857142858317, 1.857142857142858317, 1.857142857142858317, 1.857142857142858317, 1.857142857142858317, 1.857142857142858317, 1.857142857142858317, 1.857142857142858317, 1.857142857142858317, 1.857142857142858317, 1.857142857142858317, 1.857142857142858317, 1.857142857142858317, 1.857142857142858317, 1.857142857142858317, 1.857142857142858317, 1.857142857142858317, 1.857142857142858317, 1.857142857142858317, 1.857142857142858317, 1.857142857142858317, 1.857142857142858317, 1.857142857142858317, 1.857142857142858317, 1.857142857142858317, 1.857142857142858317, 1.857142857142858317, 1.857142857142858317, 1.857142857142858317, 1.857142857142858317, 1.857142857142858317, 1.857142857142858317, 1.857142857142858317, 1.857142857142858317, 1.857142857142858317, 1.857142857142858317, 1.857142857142858317, 1.857142857142858317, 1.857142857142858317, 1.857142857142858317, 1.857142857142858317, 1.857142857142858317, 1.857142857142858317, 1.857142857142858317, 1.857142857142858317, 1.857142857142858317, 1.857142857142858317, 1.857142857142858317, 1.857142857142858317, 1.857142857142858317, 1.857142857142858317, 1.857142857142858317, 1.857142857142858317, 1.857142857142858317, 1.857142857142858317, 1.857142857142858317, 1.857142857142858317, 1.857142857142858317, 1.857142857142858317, 1.857142857142858317, 1.857142857142858317, 1.857142857142858317, 1.857142857142858317, 1.857142857142858317, 1.857142857142858317, 1.857142857142858317, 1.857142857142858317, 1.857142857142858317, 1.857142857142858317, 1.857142857142858317, 1.857142857142858317, 1.857142857142858317, 1.857142857142858317, 1.857142857142858317, 1.857142857142858317, 1.857142857142858317, 1.857142857142858317, 1.857142857142858317, 1.857142857142858317, 1.857142857142858317, 1.857142857142858317, 1.857142857142858317, 1.857142857142858317, 1.857142857142858317, 1.857142857142858317, 1.857142857142858317, 1.857142857142858317, 1.857142857142858317, 1.857142857142858317, 1.857142857142858317, 1.857142857142858317, 1.857142857142858317, 1.857142857142858317, 1.857142857142858317, 1.857142857142858317, 1.857142857142858317, 1.857142857142858317, 1.857142857142858317, 1.857142857142858317, 1.857142857142858317, 1.857142857142858317, 1.857142857142858317, 1.857142857142858317, 1.857142857142858317, 1.857142857142858317, 1.857142857142858317, 1.857142857142858317),
 ( 1.000000000000000000, 1.000000000000000000, 1.000000000000000000, 1.000000000000000000, 1.000000000000000000, 1.000000000000000000, 1.000000000000000000, 1.000000000000000000, 1.000000000000000000, 1.000000000000000000, 1.000000000000000000, 1.000000000000000000, 1.000000000000000000, 1.000000000000000000, 1.000000000000000000, 1.000000000000000000, 1.000000000000000000, 1.000000000000000000, 1.000000000000000000, 1.000000000000000000, 1.000000000000000000, 1.000000000000000000, 1.000000000000000000, 1.000000000000000000, 1.000000000000000000, 1.000000000000000000, 1.000000000000000000, 1.000000000000000000, 1.000000000000000000, 1.000000000000000000, 1.000000000000000000, 1.000000000000000000, 1.000000000000000000, 1.000000000000000000, 1.000000000000000000, 1.000000000000000000, 1.000000000000000000, 1.000000000000000000, 1.000000000000000000, 1.000000000000000000, 1.000000000000000000, 1.000000000000000000, 1.000000000000000000, 1.000000000000000000, 1.000000000000000000, 1.000000000000000000, 1.000000000000000000, 1.000000000000000000, 1.000000000000000000, 1.000000000000000000, 1.000000000000000000, 1.000000000000000000, 1.000000000000000000, 1.000000000000000000, 1.000000000000000000, 1.000000000000000000, 1.000000000000000000, 1.000000000000000000, 1.000000000000000000, 1.000000000000000000, 1.000000000000000000, 1.000000000000000000, 1.000000000000000000, 1.000000000000000000, 1.000000000000000000, 1.000000000000000000, 1.000000000000000000, 1.000000000000000000, 1.000000000000000000, 1.000000000000000000, 1.000000000000000000, 1.000000000000000000, 1.000000000000000000, 1.000000000000000000, 1.000000000000000000, 1.000000000000000000, 1.000000000000000000, 1.000000000000000000, 1.000000000000000000, 1.000000000000000000, 1.000000000000000000, 1.000000000000000000, 1.000000000000000000, 1.000000000000000000, 1.000000000000000000, 1.000000000000000000, 1.000000000000000000, 1.000000000000000000, 1.000000000000000000, 1.000000000000000000, 1.000000000000000000, 1.000000000000000000, 1.000000000000000000, 1.000000000000000000, 1.000000000000000000, 1.000000000000000000, 1.000000000000000000, 1.000000000000000000, 1.000000000000000000, 1.000000000000000000, 1.000000000000000000, 1.000000000000000000, 1.000000000000000000, 1.000000000000000000, 1.000000000000000000, 1.000000000000000000, 1.000000000000000000, 1.000000000000000000, 1.000000000000000000, 1.000000000000000000, 1.000000000000000000, 1.000000000000000000, 1.000000000000000000, 1.000000000000000000, 1.000000000000000000, 1.000000000000000000, 1.000000000000000000, 1.000000000000000000, 1.000000000000000000, 1.000000000000000000, 1.000000000000000000, 1.000000000000000000, 1.000000000000000000, 1.000000000000000000, 1.000000000000000000, 1.000000000000000000, 1.000000000000000000, 1.000000000000000000, 1.000000000000000000, 1.000000000000000000, 1.000000000000000000, 1.000000000000000000, 1.000000000000000000, 1.000000000000000000, 1.000000000000000000, 1.000000000000000000, 1.000000000000000000, 1.000000000000000000, 1.000000000000000000, 1.000000000000000000, 1.000000000000000000, 1.000000000000000000) ) ) 
 REPRESENTATION_ITEM ( '' )  SURFACE ( )  );
#61087 = CARTESIAN_POINT ( 'NONE',  ( 33.51592517449224573, 434.0196043323697381, 13.78155809957686628 ) ) ;
#61088 = CARTESIAN_POINT ( 'NONE',  ( 9.843039827103241990, 101.4091649749166635, -1.781495459429543793 ) ) ;
#61089 = CARTESIAN_POINT ( 'NONE',  ( -16.75187969033532553, 37.11970326878314808, 21.80698433968612093 ) ) ;
#61090 = UNCERTAINTY_MEASURE_WITH_UNIT (LENGTH_MEASURE( 1.000000000000000082E-05 ), #24212, 'distance_accuracy_value', 'NONE');
#61091 = CARTESIAN_POINT ( 'NONE',  ( -108.5714035732085136, -60.00000000000000000, 194.5812896598510520 ) ) ;
#61092 = CARTESIAN_POINT ( 'NONE',  ( 71.63333333333333997, 6.915964383211875250E-15, 0.000000000000000000 ) ) ;
#61093 = CARTESIAN_POINT ( 'NONE',  ( 0.000000000000000000, 304.8518027762758038, -9.000000000000005329 ) ) ;
#61094 = SURFACE_STYLE_USAGE ( .BOTH. , #102064 ) ;
#61095 = CARTESIAN_POINT ( 'NONE',  ( -84.89423566776963526, -35.82611643478423957, 180.4073639259765969 ) ) ;
#61096 = SURFACE_SIDE_STYLE ('',( #60576 ) ) ;
#61097 = AXIS2_PLACEMENT_3D ( 'NONE', #87457, #101505, #45406 ) ;
#61098 = ORIENTED_EDGE ( 'NONE', *, *, #97820, .F. ) ;
#61099 = CARTESIAN_POINT ( 'NONE',  ( -9.658640570150691218, 45.55801956750498505, -15.25085205539905076 ) ) ;
#61100 = ADVANCED_FACE ( 'NONE', ( #16399 ), #32618, .T. ) ;
#61101 = CARTESIAN_POINT ( 'NONE',  ( 1.000000000000000000, -15.98920185053503928, -10.19345919381780519 ) ) ;
#61102 = MECHANICAL_DESIGN_GEOMETRIC_PRESENTATION_REPRESENTATION (  '', ( #21319 ), #91883 ) ;
#61103 = CARTESIAN_POINT ( 'NONE',  ( -84.36863145535683373, -45.27031347337740641, -2.914881809220207121 ) ) ;
#61104 = DIRECTION ( 'NONE',  ( 0.000000000000000000, 1.000000000000000000, 0.000000000000000000 ) ) ;
#61105 = CARTESIAN_POINT ( 'NONE',  ( -3.346174626192466306, 120.6797456782134503, -4.999999999999999112 ) ) ;
#61106 = CARTESIAN_POINT ( 'NONE',  ( 7.849089830965373160, 70.34685271985473776, -2.456708681988599773E-12 ) ) ;
#61107 = CARTESIAN_POINT ( 'NONE',  ( 0.000000000000000000, 4.898587196589412829E-16, -4.000000000000000000 ) ) ;
#61108 = DIRECTION ( 'NONE',  ( -1.224646799147353207E-16, 1.000000000000000000, 0.000000000000000000 ) ) ;
#61109 = CARTESIAN_POINT ( 'NONE',  ( 73.11766847789152735, -30.00000000000003197, 143.8471250665463117 ) ) ;
#61110 = CARTESIAN_POINT ( 'NONE',  ( -86.58264346576902426, -59.99999999999995737, -26.28034805200384838 ) ) ;
#61111 = CARTESIAN_POINT ( 'NONE',  ( -74.53378729071185660, -46.43775938986178176, 123.7974631154742866 ) ) ;
#61112 = ORIENTED_EDGE ( 'NONE', *, *, #12229, .F. ) ;
#61113 = CARTESIAN_POINT ( 'NONE',  ( 106.4941418293696387, -60.00000000000010658, 201.1229827202191984 ) ) ;
#61114 = CARTESIAN_POINT ( 'NONE',  ( 31.45106920060756295, 40.83882431089578091, 56.96264530398576653 ) ) ;
#61115 = CARTESIAN_POINT ( 'NONE',  ( 2.936182742934462817E-09, -59.99999999999998579, 41.99999999999666755 ) ) ;
#61116 = ORIENTED_EDGE ( 'NONE', *, *, #67802, .F. ) ;
#61117 = DIRECTION ( 'NONE',  ( 1.000000000000000000, -0.000000000000000000, -0.000000000000000000 ) ) ;
#61118 = CARTESIAN_POINT ( 'NONE',  ( 2.977408999572652260, -27.31250000204838457, 7.188101187500000044 ) ) ;
#61119 = CARTESIAN_POINT ( 'NONE',  ( -1.220180779666396820, 27.63012542767911839, -39.81491781757780757 ) ) ;
#61120 = ORIENTED_EDGE ( 'NONE', *, *, #30719, .F. ) ;
#61121 = CARTESIAN_POINT ( 'NONE',  ( 10.28624191511809371, -1.200000000000000030E-05, -12.90779740156171407 ) ) ;
#61122 = ORIENTED_EDGE ( 'NONE', *, *, #27418, .T. ) ;
#61123 = DIRECTION ( 'NONE',  ( 0.000000000000000000, 0.000000000000000000, 1.000000000000000000 ) ) ;
#61124 = DIRECTION ( 'NONE',  ( 0.000000000000000000, 0.000000000000000000, 1.000000000000000000 ) ) ;
#61125 = CARTESIAN_POINT ( 'NONE',  ( -92.35142332109028018, -60.00000000000000000, 24.83174829623999713 ) ) ;
#61126 = CARTESIAN_POINT ( 'NONE',  ( -8.559508646656389885, 53.96349637827586321, -1.531152949374502859 ) ) ;
#61127 = CARTESIAN_POINT ( 'NONE',  ( 7.188101187500001821, -32.93750000204839523, -2.977408999572650483 ) ) ;
#61128 = LINE ( 'NONE', #91887, #86065 ) ;
#61129 = SURFACE_STYLE_FILL_AREA ( #20181 ) ;
#61130 = SURFACE_SIDE_STYLE ('',( #34755 ) ) ;
#61131 = PRESENTATION_STYLE_ASSIGNMENT (( #8307 ) ) ;
#61132 = CARTESIAN_POINT ( 'NONE',  ( -6.943926999490793506, 105.5330099262614709, -3.973092371898548691 ) ) ;
#61133 = ADVANCED_FACE ( 'NONE', ( #105930 ), #105416, .F. ) ;
#61134 = CARTESIAN_POINT ( 'NONE',  ( 38.22195112133615424, 437.6732586221723409, 4.643349236001768965 ) ) ;
#61135 = VECTOR ( 'NONE', #37167, 1000.000000000000000 ) ;
#61136 = ORIENTED_EDGE ( 'NONE', *, *, #16169, .F. ) ;
#61137 = CARTESIAN_POINT ( 'NONE',  ( 4.464768147782852026, -1.996984918325857006, 102.6740199126133888 ) ) ;
#61139 = CARTESIAN_POINT ( 'NONE',  ( 32.20288135873296653, -22.14765632207181056, 30.75472695888904440 ) ) ;
#61138 = CARTESIAN_POINT ( 'NONE',  ( 34.64166250171371786, 490.4813561613897832, 11.60003975507683194 ) ) ;
#61140 =( LENGTH_UNIT ( ) NAMED_UNIT ( * ) SI_UNIT ( .MILLI., .METRE. ) );
#61141 = ORIENTED_EDGE ( 'NONE', *, *, #93974, .F. ) ;
#61142 = CARTESIAN_POINT ( 'NONE',  ( 37.69506754384874370, 484.8919167041208880, -3.620297613832784478 ) ) ;
#61143 = AXIS2_PLACEMENT_3D ( 'NONE', #75549, #51261, #84184 ) ;
#61145 = CARTESIAN_POINT ( 'NONE',  ( 6.757705285491359071, 41.35007050631321590, -70.67351639401239538 ) ) ;
#61144 = CARTESIAN_POINT ( 'NONE',  ( 27.99999999999999645, 0.000000000000000000, 15.00000000000000000 ) ) ;
#61146 = DIRECTION ( 'NONE',  ( 1.000000000000000000, 0.000000000000000000, 0.000000000000000000 ) ) ;
#61147 = AXIS2_PLACEMENT_3D ( 'NONE', #47313, #89907, #65098 ) ;
#61148 =( GEOMETRIC_REPRESENTATION_CONTEXT ( 3 ) GLOBAL_UNCERTAINTY_ASSIGNED_CONTEXT ( ( #12507 ) ) GLOBAL_UNIT_ASSIGNED_CONTEXT ( ( #70906, #29939, #104321 ) ) REPRESENTATION_CONTEXT ( 'NONE', 'WORKASPACE' ) );
#61149 = FACE_OUTER_BOUND ( 'NONE', #78619, .T. ) ;
#61150 = CARTESIAN_POINT ( 'NONE',  ( 16.65484354297773351, 1.340359594676612611E-15, 0.000000000000000000 ) ) ;
#61151 = AXIS2_PLACEMENT_3D ( 'NONE', #79026, #14807, #105940 ) ;
#61152 = DIRECTION ( 'NONE',  ( -1.000000000000000000, -1.224606353822377258E-16, -0.000000000000000000 ) ) ;
#61153 = CARTESIAN_POINT ( 'NONE',  ( -35.05476482818383488, 463.5208552852804473, 19.69826870375476346 ) ) ;
#61154 = ORIENTED_EDGE ( 'NONE', *, *, #82945, .T. ) ;
#61155 = CARTESIAN_POINT ( 'NONE',  ( 92.05911407252800416, -59.99999999999999289, 5.082830299684662378 ) ) ;
#61156 = CARTESIAN_POINT ( 'NONE',  ( -10.28624191511829977, 46.12099395432375104, -12.90779740156156841 ) ) ;
#61157 = AXIS2_PLACEMENT_3D ( 'NONE', #90569, #25334, #99175 ) ;
#61158 = CARTESIAN_POINT ( 'NONE',  ( -35.58239268463962190, 364.8620502323183246, 3.031411369397770450 ) ) ;
#61159 = CIRCLE ( 'NONE', #40422, 3.309500000000001663 ) ;
#61160 = CARTESIAN_POINT ( 'NONE',  ( -5.211028242775610053, 40.56334570827803532, -70.92280011129018646 ) ) ;
#61161 = FACE_BOUND ( 'NONE', #4858, .T. ) ;
#61162 = EDGE_LOOP ( 'NONE', ( #90203, #4798, #43994, #90962, #49450 ) ) ;
#61163 = EDGE_CURVE ( 'NONE', #3777, #74726, #30731, .T. ) ;
#61164 = CARTESIAN_POINT ( 'NONE',  ( -99.88742157809630839, -30.00000000021226398, 95.80496660798954167 ) ) ;
#61165 = ORIENTED_EDGE ( 'NONE', *, *, #79527, .F. ) ;
#61166 = DIRECTION ( 'NONE',  ( -1.000000000000000000, -1.224606353822377258E-16, -0.000000000000000000 ) ) ;
#61167 =( LENGTH_UNIT ( ) NAMED_UNIT ( * ) SI_UNIT ( .MILLI., .METRE. ) );
#61168 = LINE ( 'NONE', #46561, #83261 ) ;
#61169 = CARTESIAN_POINT ( 'NONE',  ( 14.88719829190570465, 23.11045037498492505, 0.5284321866356167519 ) ) ;
#61170 = CARTESIAN_POINT ( 'NONE',  ( 86.12633428247868039, -60.22439185339658252, -13.73171497637067517 ) ) ;
#61171 = CARTESIAN_POINT ( 'NONE',  ( 2.977408999572651815, -28.81250000204838457, 7.188101187500000933 ) ) ;
#61172 = FACE_OUTER_BOUND ( 'NONE', #31276, .T. ) ;
#61173 = CARTESIAN_POINT ( 'NONE',  ( 72.95844571965780290, -52.66120096372748804, -23.75233168814477480 ) ) ;
#61174 = VERTEX_POINT ( 'NONE', #15870 ) ;
#61176 = EDGE_CURVE ( 'NONE', #71690, #67548, #34193, .T. ) ;
#61175 = DIRECTION ( 'NONE',  ( -1.224646799147353454E-16, 0.000000000000000000, -1.000000000000000000 ) ) ;
#61177 = ORIENTED_EDGE ( 'NONE', *, *, #43518, .F. ) ;
#61178 = CARTESIAN_POINT ( 'NONE',  ( 66.00571552735603120, -4.000000000000000888, 4.898587196589422689E-16 ) ) ;
#61179 = FILL_AREA_STYLE ('',( #102151 ) ) ;
#61180 = ORIENTED_EDGE ( 'NONE', *, *, #25660, .T. ) ;
#61181 = CARTESIAN_POINT ( 'NONE',  ( 82.19117875687653907, -22.15571452471658986, 140.5442402927623675 ) ) ;
#61182 = VERTEX_POINT ( 'NONE', #98892 ) ;
#61183 = EDGE_CURVE ( 'NONE', #96838, #20, #14799, .T. ) ;
#61184 = CARTESIAN_POINT ( 'NONE',  ( 5.701904463861252381, -50.89740538927692626, 39.78701112839326015 ) ) ;
#61185 = CARTESIAN_POINT ( 'NONE',  ( 2.977408999572652260, -20.93750000204839168, 7.188101187500000044 ) ) ;
#61186 = AXIS2_PLACEMENT_3D ( 'NONE', #65556, #66082, #54379 ) ;
#61187 = CARTESIAN_POINT ( 'NONE',  ( -108.6808209725780330, -57.66364365951052662, 198.1525503354515081 ) ) ;
#61188 = CARTESIAN_POINT ( 'NONE',  ( 6.815964470353729432, -1.383691465877838755, -6.173460172893358688 ) ) ;
#61189 = ORIENTED_EDGE ( 'NONE', *, *, #19549, .F. ) ;
#61190 = FILL_AREA_STYLE ('',( #102163 ) ) ;
#61191 = CARTESIAN_POINT ( 'NONE',  ( -4.658465013329193383, -11.32363879673093621, 3.783534922165391112 ) ) ;
#61192 = CARTESIAN_POINT ( 'NONE',  ( 31.36650669486618881, 1.474610560812782335E-15, 0.000000000000000000 ) ) ;
#61193 = DIRECTION ( 'NONE',  ( -1.000000000000000000, -1.224606353822377258E-16, -0.000000000000000000 ) ) ;
#61194 = CARTESIAN_POINT ( 'NONE',  ( 3.313708498984762052, -16.90625000409676915, -8.000000000000000000 ) ) ;
#61195 = CARTESIAN_POINT ( 'NONE',  ( -45.20342746193760775, -28.36574318593202548, 40.29076024120101351 ) ) ;
#61196 = CARTESIAN_POINT ( 'NONE',  ( -36.80389671760433146, 25.99784339350267004, 11.20190813230474802 ) ) ;
#61197 = CARTESIAN_POINT ( 'NONE',  ( -33.00000000000000000, 488.8442721620238558, 4.433647275927475206 ) ) ;
#61198 = CARTESIAN_POINT ( 'NONE',  ( -37.20098947015251412, 438.1443347308166381, 4.012567541568420992 ) ) ;
#61199 = CARTESIAN_POINT ( 'NONE',  ( 19.29515645702225868, -5.000000000000000888, 6.123233995736769241E-16 ) ) ;
#61200 = AXIS2_PLACEMENT_3D ( 'NONE', #45680, #61882, #103896 ) ;
#61201 = APPLICATION_PROTOCOL_DEFINITION ( 'draft international standard', 'automotive_design', 1998, #93438 ) ;
#61202 = CARTESIAN_POINT ( 'NONE',  ( -0.08034007072829510432, -30.00000000000001066, -7.793135878010705397 ) ) ;
#61203 = ORIENTED_EDGE ( 'NONE', *, *, #4360, .F. ) ;
#61204 = CARTESIAN_POINT ( 'NONE',  ( -4.173972032418419076, -48.44822883994723384, 43.43505066642690338 ) ) ;
#61205 = CARTESIAN_POINT ( 'NONE',  ( 11.05388719230748684, -4.985422414517793221, -12.57711417799305664 ) ) ;
#61206 = DIRECTION ( 'NONE',  ( 0.000000000000000000, -1.000000000000000000, 0.000000000000000000 ) ) ;
#61207 = CARTESIAN_POINT ( 'NONE',  ( -62.55951166628249638, -29.54618481767612082, -24.05121344435046637 ) ) ;
#61208 = CARTESIAN_POINT ( 'NONE',  ( -84.71380100379134603, -29.99999999999998934, 167.6049798258065664 ) ) ;
#61209 = EDGE_CURVE ( 'NONE', #28024, #41772, #90832, .T. ) ;
#61210 = MECHANICAL_DESIGN_GEOMETRIC_PRESENTATION_REPRESENTATION (  '', ( #2587 ), #28504 ) ;
#61211 = ORIENTED_EDGE ( 'NONE', *, *, #18230, .T. ) ;
#61212 = FACE_OUTER_BOUND ( 'NONE', #39145, .T. ) ;
#61213 = CARTESIAN_POINT ( 'NONE',  ( 77.74182763612704150, -57.51479071948315180, 196.2079078470394222 ) ) ;
#61214 = CARTESIAN_POINT ( 'NONE',  ( 2.617478843592802473, 48.00000000000000711, -94.73972676668314818 ) ) ;
#61215 = EDGE_CURVE ( 'NONE', #33315, #86317, #20945, .T. ) ;
#61216 = ADVANCED_FACE ( 'NONE', ( #15339 ), #15220, .T. ) ;
#61217 = CARTESIAN_POINT ( 'NONE',  ( 47.01191233711254824, -34.86740698265760585, -36.61028653586306092 ) ) ;
#61218 = CARTESIAN_POINT ( 'NONE',  ( 7.500000000000007105, -4.999999999999999112, -52.94236561372729000 ) ) ;
#61219 = DIRECTION ( 'NONE',  ( 0.000000000000000000, -1.000000000000000000, 0.000000000000000000 ) ) ;
#61220 = CARTESIAN_POINT ( 'NONE',  ( -72.03623563651683526, -59.99999999999999289, 154.5482511779330537 ) ) ;
#61221 = AXIS2_PLACEMENT_3D ( 'NONE', #15357, #97331, #7784 ) ;
#61222 = STYLED_ITEM ( 'NONE', ( #96900 ), #35149 ) ;
#61223 = FACE_OUTER_BOUND ( 'NONE', #97200, .T. ) ;
#61224 = FILL_AREA_STYLE_COLOUR ( '', #73196 ) ;
#61225 = CARTESIAN_POINT ( 'NONE',  ( -84.53966279108223603, -53.82414633558762773, 189.9397737380796229 ) ) ;
#61226 = ORIENTED_EDGE ( 'NONE', *, *, #5398, .F. ) ;
#61227 = DIRECTION ( 'NONE',  ( 0.000000000000000000, -0.6543614439331889576, -0.7561819230143446147 ) ) ;
#61228 = CARTESIAN_POINT ( 'NONE',  ( -3.010010578735510478, -32.51265499686979155, 29.30374655122669836 ) ) ;
#61229 = CARTESIAN_POINT ( 'NONE',  ( -6.275176166263391586, 41.94081489990061584, -59.38054223964236655 ) ) ;
#61230 = CARTESIAN_POINT ( 'NONE',  ( 6.644028492724100232, 3.901260126080569712, 6.757180751913672623 ) ) ;
#61231 =( BOUNDED_SURFACE ( )  B_SPLINE_SURFACE ( 3, 2, ( 
 ( #44905, #20129, #102051 ),
 ( #69702, #60038, #19062 ),
 ( #60562, #43293, #84816 ),
 ( #51903, #95051, #69181 ) ),
 .UNSPECIFIED., .F., .F., .F. ) 
 B_SPLINE_SURFACE_WITH_KNOTS ( ( 4, 4 ),
 ( 3, 3 ),
 ( 0.01840331564793163538, 0.04646555858147861234 ),
 ( 0.000000000000000000, 1.000000000000000000 ),
 .UNSPECIFIED. ) 
 GEOMETRIC_REPRESENTATION_ITEM ( )  RATIONAL_B_SPLINE_SURFACE ( (
 ( 1.000000000000000000, 0.8381405999065927315, 1.000000000000000000),
 ( 1.000000000000000000, 0.8381408041605379333, 1.000000000000000000),
 ( 1.000000000000000000, 0.8381407647121852378, 1.000000000000000000),
 ( 1.000000000000000000, 0.8381405645739014032, 1.000000000000000000) ) ) 
 REPRESENTATION_ITEM ( '' )  SURFACE ( )  );
#61232 = FILL_AREA_STYLE ('',( #19222 ) ) ;
#61233 = ORIENTED_EDGE ( 'NONE', *, *, #24029, .F. ) ;
#61234 = EDGE_CURVE ( 'NONE', #104748, #17654, #89221, .T. ) ;
#61235 = CARTESIAN_POINT ( 'NONE',  ( 0.000000000000000000, 0.000000000000000000, -2.868028571428571372 ) ) ;
#61236 = DIRECTION ( 'NONE',  ( 1.000000000000000000, 1.224606353822377258E-16, 0.000000000000000000 ) ) ;
#61237 = DIRECTION ( 'NONE',  ( 0.000000000000000000, -1.000000000000000000, 0.000000000000000000 ) ) ;
#61238 = CARTESIAN_POINT ( 'NONE',  ( -30.64306277920947963, 7.829637822906565958, -41.65859565436478107 ) ) ;
#61239 = ORIENTED_EDGE ( 'NONE', *, *, #45173, .T. ) ;
#61240 = CARTESIAN_POINT ( 'NONE',  ( 23.32831762434326706, 303.3951354536446274, -9.883407546016623968 ) ) ;
#61241 = CARTESIAN_POINT ( 'NONE',  ( 45.29905483467455696, 497.0732240353902398, -8.041250874568902418 ) ) ;
#61242 = EDGE_CURVE ( 'NONE', #102596, #15986, #56482, .T. ) ;
#61243 = CARTESIAN_POINT ( 'NONE',  ( 24.56594385547430903, -4.285714285713612348, -6.601913983211183279 ) ) ;
#61244 = CARTESIAN_POINT ( 'NONE',  ( 9.502088046852136927, 53.42926094969260475, -3.606443582442682150 ) ) ;
#61245 = CARTESIAN_POINT ( 'NONE',  ( 91.01367250360885919, -30.00000000000005684, 38.60059757395459457 ) ) ;
#61246 = CARTESIAN_POINT ( 'NONE',  ( -78.92021213579246819, -56.84825361667137145, 159.0990771215834343 ) ) ;
#61247 = ORIENTED_EDGE ( 'NONE', *, *, #77286, .F. ) ;
#61248 = CARTESIAN_POINT ( 'NONE',  ( 8.099999999999999645, 7.505553499465140277, 0.000000000000000000 ) ) ;
#61249 = CARTESIAN_POINT ( 'NONE',  ( 0.000000000000000000, 0.000000000000000000, -7.259124522925831435 ) ) ;
#61250 = CARTESIAN_POINT ( 'NONE',  ( 37.14872619403364240, -57.69633467219071576, 51.57620306562363055 ) ) ;
#61251 = DIRECTION ( 'NONE',  ( -0.5882352941176471894, 0.000000000000000000, -0.8086898285216187476 ) ) ;
#61252 = CARTESIAN_POINT ( 'NONE',  ( 42.96915577533521713, 322.5831792346974680, -3.261277637034701637 ) ) ;
#61253 = CARTESIAN_POINT ( 'NONE',  ( 38.88026172477386666, 468.9844931099165706, 0.4637734290235665524 ) ) ;
#61254 = VERTEX_POINT ( 'NONE', #27735 ) ;
#61255 = CARTESIAN_POINT ( 'NONE',  ( 4.271854802331145784, 54.28677085485544040, -6.536858402226804365 ) ) ;
#61256 = CARTESIAN_POINT ( 'NONE',  ( 31.01615627852296342, 439.2622192783163086, 22.57221946846627958 ) ) ;
#61257 = CARTESIAN_POINT ( 'NONE',  ( 5.082755093536324154, -25.34375000204838813, 5.082755093536326818 ) ) ;
#61258 = ORIENTED_EDGE ( 'NONE', *, *, #48755, .T. ) ;
#61259 = CIRCLE ( 'NONE', #16430, 4.000000000000007105 ) ;
#61260 = CARTESIAN_POINT ( 'NONE',  ( 1.510421413154731551, 15.23810023151366977, 9.910377230549928029 ) ) ;
#61261 = CARTESIAN_POINT ( 'NONE',  ( 4.999060825136298014, 41.75164249415627182, -70.37937598343344803 ) ) ;
#61262 = CARTESIAN_POINT ( 'NONE',  ( -39.04923757934999884, 49.99999999997997691, 52.30342408740197158 ) ) ;
#61263 = CARTESIAN_POINT ( 'NONE',  ( -3.313708498984726969, -17.46874999999999645, 8.000000000000039080 ) ) ;
#61264 = CARTESIAN_POINT ( 'NONE',  ( 91.09088295274877112, -2.002967142162725287E-29, 5.000000000000011546 ) ) ;
#61265 = EDGE_LOOP ( 'NONE', ( #63926, #33957, #62475, #106434 ) ) ;
#61266 = CARTESIAN_POINT ( 'NONE',  ( 92.36673650245116107, -59.99999999999998579, 0.5857224784561708697 ) ) ;
#61268 = CARTESIAN_POINT ( 'NONE',  ( 20.33158520735264219, -46.43450536202994527, 32.18516374921409806 ) ) ;
#61267 = CARTESIAN_POINT ( 'NONE',  ( -41.69391581180516937, -30.00000000000004974, 49.76410629065788527 ) ) ;
#61269 = CARTESIAN_POINT ( 'NONE',  ( 88.26372640434641426, 34.25047185182970111, -44.13186320217318581 ) ) ;
#61270 = EDGE_CURVE ( 'NONE', #35302, #90326, #70290, .T. ) ;
#61271 = CARTESIAN_POINT ( 'NONE',  ( -37.55439227784096090, -29.13175677663839025, 34.71063202183116658 ) ) ;
#61272 = UNCERTAINTY_MEASURE_WITH_UNIT (LENGTH_MEASURE( 1.000000000000000082E-05 ), #14401, 'distance_accuracy_value', 'NONE');
#61273 = EDGE_LOOP ( 'NONE', ( #9152, #70523, #73767, #83501 ) ) ;
#61274 = CARTESIAN_POINT ( 'NONE',  ( 33.89250494191496443, 463.6575930728431558, 6.993601543837897339 ) ) ;
#61275 = CARTESIAN_POINT ( 'NONE',  ( -13.98736753405778543, -57.97328548197708642, 27.64795516495958339 ) ) ;
#61276 = DIRECTION ( 'NONE',  ( 0.000000000000000000, 0.000000000000000000, 1.000000000000000000 ) ) ;
#61277 = FACE_OUTER_BOUND ( 'NONE', #84240, .T. ) ;
#61278 = CARTESIAN_POINT ( 'NONE',  ( -14.29190075645470870, 6.456385560659953171, 7.561819230136401337 ) ) ;
#61279 = EDGE_LOOP ( 'NONE', ( #41728, #95567 ) ) ;
#61280 = CARTESIAN_POINT ( 'NONE',  ( -71.70444520824810297, -38.32814726721150578, 143.9842855213637733 ) ) ;
#61281 = CARTESIAN_POINT ( 'NONE',  ( 43.27291153936506873, 435.9049899631326070, 8.045225097063040565 ) ) ;
#61282 = CARTESIAN_POINT ( 'NONE',  ( 100.9278572184871479, -29.99999999999998224, 179.0295527065578938 ) ) ;
#61283 = CARTESIAN_POINT ( 'NONE',  ( 21.09715123528542691, 6.123233995736770227E-16, -5.000000000000002665 ) ) ;
#61284 = CARTESIAN_POINT ( 'NONE',  ( 2.450449656239129581, 15.75130202679986269, 9.701736001019305888 ) ) ;
#61285 = CARTESIAN_POINT ( 'NONE',  ( 81.52379479105302096, -30.00000000000000355, -3.957376937645873394 ) ) ;
#61286 = CARTESIAN_POINT ( 'NONE',  ( -4.681380154937277993, -50.73787295680603648, 103.7259032015044795 ) ) ;
#61287 = ORIENTED_EDGE ( 'NONE', *, *, #42155, .T. ) ;
#61288 = ADVANCED_FACE ( 'NONE', ( #58460 ), #84860, .T. ) ;
#61289 = STYLED_ITEM ( 'NONE', ( #55950 ), #63551 ) ;
#61290 = EDGE_CURVE ( 'NONE', #53379, #14336, #26515, .T. ) ;
#61291 = ORIENTED_EDGE ( 'NONE', *, *, #104624, .T. ) ;
#61292 = B_SPLINE_CURVE_WITH_KNOTS ( 'NONE', 3,
 ( #95484, #5926, #22691, #55526, #88466, #14540, #47449, #17765, #90579, #98652, #40429, #7510 ),
 .UNSPECIFIED., .F., .F.,
 ( 4, 2, 2, 2, 2, 4 ),
 ( 4.384643301807188419E-15, 0.001900005895290834707, 0.003800011790577284467, 0.005700017685863734661, 0.006650020633506964311, 0.007600023581150194829 ),
 .UNSPECIFIED. ) ;
#61293 = ORIENTED_EDGE ( 'NONE', *, *, #73401, .T. ) ;
#61294 = DIRECTION ( 'NONE',  ( 0.000000000000000000, -1.000000000000000000, 0.000000000000000000 ) ) ;
#61295 = CARTESIAN_POINT ( 'NONE',  ( 22.54429042550015083, 43.83586977107353988, -79.50672479082321331 ) ) ;
#61296 = CARTESIAN_POINT ( 'NONE',  ( 0.000000000000000000, 0.000000000000000000, 8.000000000000000000 ) ) ;
#61297 = CARTESIAN_POINT ( 'NONE',  ( -43.66706706802315807, 409.2729596023213503, 16.12745813032958608 ) ) ;
#61298 = DIRECTION ( 'NONE',  ( 8.673617379884035472E-16, 1.000000000000000000, -4.449471833015289037E-16 ) ) ;
#61299 = CARTESIAN_POINT ( 'NONE',  ( -7.619701877737479201, -88.17442159532768642, -2.447562251315979598 ) ) ;
#61300 = EDGE_CURVE ( 'NONE', #62246, #47334, #75695, .T. ) ;
#61301 = CARTESIAN_POINT ( 'NONE',  ( 0.000000000000000000, 17.85270131633358304, -10.00000000000000178 ) ) ;
#61302 = VERTEX_POINT ( 'NONE', #34750 ) ;
#61304 = EDGE_CURVE ( 'NONE', #82447, #11977, #7511, .T. ) ;
#61303 = CARTESIAN_POINT ( 'NONE',  ( 11.99999999999999467, 50.00000000000000000, -83.42920367501479006 ) ) ;
#61305 = ORIENTED_EDGE ( 'NONE', *, *, #11543, .F. ) ;
#61306 = CARTESIAN_POINT ( 'NONE',  ( -4.496882872040832702, -64.46211334510377355, 3.972797206970399397 ) ) ;
#61307 = CARTESIAN_POINT ( 'NONE',  ( 60.41163985755903099, -38.34247882570736721, 97.70464050350065577 ) ) ;
#61308 = CARTESIAN_POINT ( 'NONE',  ( 31.55246551994505921, 436.6870800834244051, 19.28475619652349593 ) ) ;
#61309 = CIRCLE ( 'NONE', #83670, 1.000000000000000000 ) ;
#61310 = COLOUR_RGB ( '', 0.40784314, 0.44705882, 0.49803922) ;
#61311 = CARTESIAN_POINT ( 'NONE',  ( 22.25695985037653202, 303.2606861724426608, 10.02485155946911810 ) ) ;
#61312 = CIRCLE ( 'NONE', #75047, 1.000000000000000222 ) ;
#61313 = AXIS2_PLACEMENT_3D ( 'NONE', #56692, #1089, #34063 ) ;
#61314 = CARTESIAN_POINT ( 'NONE',  ( 6.683837171061805194, -3.955946848495972556, -6.851900933636989599 ) ) ;
#61315 = CARTESIAN_POINT ( 'NONE',  ( 60.83498899738820853, -46.43599129440129047, 77.79182497454313250 ) ) ;
#61316 = VECTOR ( 'NONE', #39634, 1000.000000000000000 ) ;
#61317 = ORIENTED_EDGE ( 'NONE', *, *, #25954, .T. ) ;
#61318 = ADVANCED_FACE ( 'NONE', ( #17483 ), #50621, .T. ) ;
#61319 = CARTESIAN_POINT ( 'NONE',  ( -9.999999999999992895, -3.000000000000002665, -86.30899693899574743 ) ) ;
#61320 = VECTOR ( 'NONE', #23396, 1000.000000000000114 ) ;
#61321 = CARTESIAN_POINT ( 'NONE',  ( -8.000000000000000000, 0.000000000000000000, -3.725171428571429022 ) ) ;
#61322 = CARTESIAN_POINT ( 'NONE',  ( 0.000000000000000000, -100.0000000000000000, 0.000000000000000000 ) ) ;
#61323 = CARTESIAN_POINT ( 'NONE',  ( 3.454253436624935336, -0.8414180287960453253, 103.7259032015043232 ) ) ;
#61324 = ORIENTED_EDGE ( 'NONE', *, *, #25006, .T. ) ;
#61326 = CARTESIAN_POINT ( 'NONE',  ( 6.928203230275508773, -85.26479267253573369, 4.000000000000000888 ) ) ;
#61325 = FILL_AREA_STYLE_COLOUR ( '', #48685 ) ;
#61327 = CARTESIAN_POINT ( 'NONE',  ( 27.61650669486618881, 4.000000000000003553, 4.898587196589414801E-16 ) ) ;
#61328 = DIRECTION ( 'NONE',  ( 0.5735764363510466035, -0.8191520442889914655, 1.003171929053524500E-16 ) ) ;
#61329 = FILL_AREA_STYLE_COLOUR ( '', #104166 ) ;
#61330 =( LENGTH_UNIT ( ) NAMED_UNIT ( * ) SI_UNIT ( .MILLI., .METRE. ) );
#61331 = CARTESIAN_POINT ( 'NONE',  ( 2.422472278927138994E-15, -0.1944580884125578779, 19.78098730681987405 ) ) ;
#61332 = CARTESIAN_POINT ( 'NONE',  ( 44.46823338009918558, 1.482358050883964840E-15, 0.000000000000000000 ) ) ;
#61333 = CARTESIAN_POINT ( 'NONE',  ( 85.67780798737555870, -46.54417124946874651, 188.9740981328812381 ) ) ;
#61334 = CARTESIAN_POINT ( 'NONE',  ( 60.63333333333333286, -3.309500000000000774, 4.475777889183797681E-16 ) ) ;
#61335 = CARTESIAN_POINT ( 'NONE',  ( -7.844366129632167173, 79.51894426619178091, 5.000000000000000000 ) ) ;
#61336 = ORIENTED_EDGE ( 'NONE', *, *, #25782, .F. ) ;
#61337 = CARTESIAN_POINT ( 'NONE',  ( 75.76386167821715389, -57.67120288045602194, -32.30820643211533394 ) ) ;
#61338 = FACE_OUTER_BOUND ( 'NONE', #43061, .T. ) ;
#61339 = CARTESIAN_POINT ( 'NONE',  ( 4.999999999999995559, -4.000000000000000000, 42.58845726811989607 ) ) ;
#61340 = CARTESIAN_POINT ( 'NONE',  ( 30.00000000000000000, 461.8887775513396150, 11.55279652844105698 ) ) ;
#61341 = CIRCLE ( 'NONE', #52688, 5.000000000000001776 ) ;
#61342 = CARTESIAN_POINT ( 'NONE',  ( -86.30897805172713788, -29.99999999999998934, 66.16620683248447676 ) ) ;
#61343 = EDGE_CURVE ( 'NONE', #96186, #74990, #38855, .T. ) ;
#61344 = DIRECTION ( 'NONE',  ( 0.000000000000000000, 0.000000000000000000, 1.000000000000000000 ) ) ;
#61345 = CARTESIAN_POINT ( 'NONE',  ( 27.84462555168287778, -57.67905924191398270, 44.21611220939174558 ) ) ;
#61346 = CARTESIAN_POINT ( 'NONE',  ( 9.327072865849737937, 44.07210225711265394, 13.35182660753846129 ) ) ;
#61347 = EDGE_CURVE ( 'NONE', #3694, #100024, #40247, .T. ) ;
#61348 = DIRECTION ( 'NONE',  ( 0.000000000000000000, 0.000000000000000000, 1.000000000000000000 ) ) ;
#61349 = DIRECTION ( 'NONE',  ( -0.5735764363510494901, -0.8191520442889894671, 0.000000000000000000 ) ) ;
#61350 = CARTESIAN_POINT ( 'NONE',  ( -17.49999999999998224, 50.00000000000000000, 63.60712894880522583 ) ) ;
#61351 = CARTESIAN_POINT ( 'NONE',  ( 6.738141070036321345, -4.358126490543069664, -16.85492060642626200 ) ) ;
#61352 = DIRECTION ( 'NONE',  ( 0.000000000000000000, 0.000000000000000000, -1.000000000000000000 ) ) ;
#61353 = CARTESIAN_POINT ( 'NONE',  ( 24.22617517784814112, -19.82454084975979924, -33.12017639804538760 ) ) ;
#61354 = ADVANCED_FACE ( 'NONE', ( #37939 ), #44406, .T. ) ;
#61355 =( NAMED_UNIT ( * ) PLANE_ANGLE_UNIT ( ) SI_UNIT ( $, .RADIAN. ) );
#61356 = AXIS2_PLACEMENT_3D ( 'NONE', #103405, #78586, #14907 ) ;
#61357 = CARTESIAN_POINT ( 'NONE',  ( -24.01064210916210229, -49.91863376122307727, 33.32460945998198554 ) ) ;
#61358 = ORIENTED_EDGE ( 'NONE', *, *, #21094, .T. ) ;
#61359 = CARTESIAN_POINT ( 'NONE',  ( 39.65839090363501640, 485.8593493675161312, -5.004208577436686234 ) ) ;
#61360 =( NAMED_UNIT ( * ) SI_UNIT ( $, .STERADIAN. ) SOLID_ANGLE_UNIT ( ) );
#61361 = CARTESIAN_POINT ( 'NONE',  ( -17.15213637186141682, -60.36485515943083158, 34.22168534330848644 ) ) ;
#61363 = CARTESIAN_POINT ( 'NONE',  ( 1.250111974717941443, 36.68751764429408979, -28.65871480211785993 ) ) ;
#61362 = CARTESIAN_POINT ( 'NONE',  ( -0.3379557265678910793, 28.19330765266871452, 38.28504178355841248 ) ) ;
#61364 = AXIS2_PLACEMENT_3D ( 'NONE', #1984, #69407, #92597 ) ;
#61365 = ORIENTED_EDGE ( 'NONE', *, *, #72563, .T. ) ;
#61366 = ORIENTED_EDGE ( 'NONE', *, *, #79381, .T. ) ;
#61367 = EDGE_CURVE ( 'NONE', #23591, #66369, #90227, .T. ) ;
#61368 = CARTESIAN_POINT ( 'NONE',  ( 16.05785784214672773, 4.775831776474238843, 3.710403933782422836 ) ) ;
#61369 = AXIS2_PLACEMENT_3D ( 'NONE', #90930, #58565, #66107 ) ;
#61370 = CARTESIAN_POINT ( 'NONE',  ( 28.09999999999999787, -3.309499999999999886, 0.000000000000000000 ) ) ;
#61371 = ORIENTED_EDGE ( 'NONE', *, *, #12871, .T. ) ;
#61372 = CYLINDRICAL_SURFACE ( 'NONE', #36082, 1.250000000000000222 ) ;
#61373 = CARTESIAN_POINT ( 'NONE',  ( 3.122594241960849448, 50.00000000000000711, -96.69514296590838853 ) ) ;
#61374 = COLOUR_RGB ( '', 0.09019608, 0.27058824, 0.51372549) ;
#61375 = CARTESIAN_POINT ( 'NONE',  ( 100.7139165092765722, -45.27943385528230635, 191.7620851108205500 ) ) ;
#61376 = CIRCLE ( 'NONE', #13065, 7.999999999999994671 ) ;
#61378 = DIRECTION ( 'NONE',  ( -0.000000000000000000, 1.000000000000000000, 0.000000000000000000 ) ) ;
#61377 = CARTESIAN_POINT ( 'NONE',  ( -13.50000000000000000, 3.304540750553650152, -0.2220019300505651771 ) ) ;
#61379 = EDGE_CURVE ( 'NONE', #90844, #34259, #54056, .T. ) ;
#61380 = ORIENTED_EDGE ( 'NONE', *, *, #32550, .T. ) ;
#61381 = CIRCLE ( 'NONE', #52731, 1.000000000000000888 ) ;
#61382 = ORIENTED_EDGE ( 'NONE', *, *, #72780, .T. ) ;
#61383 = VECTOR ( 'NONE', #67965, 1000.000000000000000 ) ;
#61384 = VERTEX_POINT ( 'NONE', #78349 ) ;
#61385 = CARTESIAN_POINT ( 'NONE',  ( 22.84363777014927877, 305.5774054537097868, 9.094444372195162885 ) ) ;
#61386 = DIRECTION ( 'NONE',  ( -1.000000000000000000, -1.224606353822377258E-16, -0.000000000000000000 ) ) ;
#61387 = ORIENTED_EDGE ( 'NONE', *, *, #76092, .T. ) ;
#61388 = FACE_OUTER_BOUND ( 'NONE', #62265, .T. ) ;
#61389 = CARTESIAN_POINT ( 'NONE',  ( -6.675188372276874560, 41.63185016722236043, -70.36443417157406088 ) ) ;
#61390 = CARTESIAN_POINT ( 'NONE',  ( -36.42379736945513002, -59.99999999996140332, -42.51792151884048110 ) ) ;
#61391 = CARTESIAN_POINT ( 'NONE',  ( 6.928203230275509661, -65.00000000000000000, -4.000000000000002665 ) ) ;
#61392 = CONICAL_SURFACE ( 'NONE', #97532, 5.000000000000000000, 0.9599310885968913576 ) ;
#61393 = CARTESIAN_POINT ( 'NONE',  ( 79.82864494832747937, -60.00000000000971312, -30.74386842393604979 ) ) ;
#61394 = CARTESIAN_POINT ( 'NONE',  ( -43.55333112596419909, 465.2342844084849389, 9.238213423004411951 ) ) ;
#61395 = CARTESIAN_POINT ( 'NONE',  ( -6.744834067507015085, 41.44195096935217748, -58.57194677540513794 ) ) ;
#61397 = CARTESIAN_POINT ( 'NONE',  ( 4.101671097088348539, -53.39668839384628996, 32.78132364643582974 ) ) ;
#61396 = CARTESIAN_POINT ( 'NONE',  ( -92.03818768401583839, -29.99999999999997513, 46.84875813697714619 ) ) ;
#61398 = DIRECTION ( 'NONE',  ( 0.000000000000000000, 1.000000000000000000, 0.000000000000000000 ) ) ;
#61399 = CARTESIAN_POINT ( 'NONE',  ( -48.17921737381070102, -18.76214205199974927, 41.56990939206856694 ) ) ;
#61400 = ORIENTED_EDGE ( 'NONE', *, *, #87955, .T. ) ;
#61401 = CARTESIAN_POINT ( 'NONE',  ( 2.679328824289926914, -70.32470627744208969, 13.25646130353394803 ) ) ;
#61402 = PRODUCT_DEFINITION_SHAPE ( 'NONE', 'NONE',  #95727 ) ;
#61403 = ORIENTED_EDGE ( 'NONE', *, *, #88665, .F. ) ;
#61404 = CARTESIAN_POINT ( 'NONE',  ( 64.78349330513380266, 6.975173280561618775E-15, 0.000000000000000000 ) ) ;
#61405 = DIRECTION ( 'NONE',  ( 0.000000000000000000, 0.000000000000000000, 1.000000000000000000 ) ) ;
#61406 = CARTESIAN_POINT ( 'NONE',  ( 5.980543423763066357, -6.029035924989237571, -0.5500789318242828019 ) ) ;
#61408 = VERTEX_POINT ( 'NONE', #20175 ) ;
#61407 = AXIS2_PLACEMENT_3D ( 'NONE', #71535, #95307, #70502 ) ;
#61409 = CARTESIAN_POINT ( 'NONE',  ( 5.191144708981711986, 247.3596991447872142, 3.015512395308856952 ) ) ;
#61410 = VERTEX_POINT ( 'NONE', #103173 ) ;
#61411 = CARTESIAN_POINT ( 'NONE',  ( 97.39383678230348096, -30.00000000010727064, 81.91721032156783622 ) ) ;
#61412 =( NAMED_UNIT ( * ) PLANE_ANGLE_UNIT ( ) SI_UNIT ( $, .RADIAN. ) );
#61413 = CARTESIAN_POINT ( 'NONE',  ( 3.626288723285761240, -48.95575889185589347, 104.3502830461769406 ) ) ;
#61414 = CARTESIAN_POINT ( 'NONE',  ( 6.786616689952412074, 41.72678941544184994, -59.11526159199856068 ) ) ;
#61415 = CIRCLE ( 'NONE', #25241, 4.000000000000007105 ) ;
#61416 = CARTESIAN_POINT ( 'NONE',  ( -23.57730434129643626, 18.64316884713158728, -30.67950393661452679 ) ) ;
#61417 = CARTESIAN_POINT ( 'NONE',  ( 100.4873323852713867, -29.99999999999999645, 182.9215336627512443 ) ) ;
#61418 = CARTESIAN_POINT ( 'NONE',  ( 28.58349330513380337, -3.851859888774471706E-31, 4.000000000000001776 ) ) ;
#61419 = ORIENTED_EDGE ( 'NONE', *, *, #9276, .F. ) ;
#61420 = ADVANCED_FACE ( 'NONE', ( #79415 ), #53025, .T. ) ;
#61421 = ORIENTED_EDGE ( 'NONE', *, *, #102133, .T. ) ;
#61422 = ORIENTED_EDGE ( 'NONE', *, *, #69143, .F. ) ;
#61423 = CARTESIAN_POINT ( 'NONE',  ( 53.62448839840453729, -56.84308160174793301, 64.25510811246175535 ) ) ;
#61424 = CARTESIAN_POINT ( 'NONE',  ( 6.372521186659901637, 41.41795280492296172, -58.45320835100594081 ) ) ;
#61425 = CARTESIAN_POINT ( 'NONE',  ( 66.26095113931063452, 4.898587196589294500E-16, -4.000000000000007105 ) ) ;
#61426 = EDGE_CURVE ( 'NONE', #44463, #45750, #66117, .T. ) ;
#61427 = ORIENTED_EDGE ( 'NONE', *, *, #10621, .F. ) ;
#61429 = EDGE_CURVE ( 'NONE', #83574, #38530, #78759, .T. ) ;
#61428 = CARTESIAN_POINT ( 'NONE',  ( -90.31811283708992732, -38.40091087090596034, -15.13224940126931983 ) ) ;
#61430 = ORIENTED_EDGE ( 'NONE', *, *, #40870, .F. ) ;
#61431 = CARTESIAN_POINT ( 'NONE',  ( 99.81073769260291328, -38.46674976063415841, 200.5728603240891914 ) ) ;
#61432 = CARTESIAN_POINT ( 'NONE',  ( 12.60473757244623094, 22.93756007865150437, 5.608979574771352894 ) ) ;
#61433 = CARTESIAN_POINT ( 'NONE',  ( 83.93392681204029770, -45.28697172910836599, 3.738167347945261731 ) ) ;
#61434 = CARTESIAN_POINT ( 'NONE',  ( 42.78153023264098209, 391.2922209041898327, 19.62706161876795363 ) ) ;
#61435 = CARTESIAN_POINT ( 'NONE',  ( 5.939725004867027813, -11.78992312938688336, -9.289959103331071333 ) ) ;
#61436 = AXIS2_PLACEMENT_3D ( 'NONE', #87600, #54663, #104287 ) ;
#61437 = CARTESIAN_POINT ( 'NONE',  ( -24.47194732006304108, 25.31483624829911960, -32.07842946029033016 ) ) ;
#61438 = VECTOR ( 'NONE', #73746, 1000.000000000000000 ) ;
#61439 = EDGE_CURVE ( 'NONE', #87682, #48784, #55640, .T. ) ;
#61440 = CARTESIAN_POINT ( 'NONE',  ( -43.80952869898561630, 434.9438303799926189, 12.65470026211868237 ) ) ;
#61441 = CARTESIAN_POINT ( 'NONE',  ( 8.020869781892258743, 104.2554943876434805, 5.000000000002456702 ) ) ;
#61442 = VERTEX_POINT ( 'NONE', #81507 ) ;
#61443 = CIRCLE ( 'NONE', #75185, 5.000000000000001776 ) ;
#61444 = DIRECTION ( 'NONE',  ( 0.000000000000000000, 0.000000000000000000, 1.000000000000000000 ) ) ;
#61445 = CARTESIAN_POINT ( 'NONE',  ( -33.00795325653169243, 439.3958174160654835, 23.82489859418955191 ) ) ;
#61446 = ORIENTED_EDGE ( 'NONE', *, *, #76985, .T. ) ;
#61447 = CARTESIAN_POINT ( 'NONE',  ( -5.290067270632282437, 54.20842449845790867, 6.031152949371105798 ) ) ;
#61448 = CARTESIAN_POINT ( 'NONE',  ( -28.40381499265910392, 310.0606719538530456, 11.65298042467015449 ) ) ;
#61449 = CARTESIAN_POINT ( 'NONE',  ( 20.00000000000001066, -4.000000000000000000, -1.500000000000001332 ) ) ;
#61450 = SURFACE_SIDE_STYLE ('',( #102959 ) ) ;
#61451 = CARTESIAN_POINT ( 'NONE',  ( 7.999999999999998224, -20.09374999999999289, 3.313708498984766493 ) ) ;
#61452 = CARTESIAN_POINT ( 'NONE',  ( 8.212513060757594019, -15.78310966187656028, 34.62353203711420946 ) ) ;
#61453 = PRODUCT_DEFINITION_SHAPE ( 'NONE', 'NONE',  #106805 ) ;
#61454 = AXIS2_PLACEMENT_3D ( 'NONE', #3987, #78923, #71355 ) ;
#61455 = CONICAL_SURFACE ( 'NONE', #14911, 3.309500000000001663, 0.9599310885968770357 ) ;
#61456 = COLOUR_RGB ( '', 0.08235294, 0.09019608, 0.10196078) ;
#61457 = DIRECTION ( 'NONE',  ( 1.000000000000000000, 0.000000000000000000, 0.000000000000000000 ) ) ;
#61458 = CIRCLE ( 'NONE', #56246, 4.172000000000001485 ) ;
#61459 = ORIENTED_EDGE ( 'NONE', *, *, #81840, .T. ) ;
#61460 = CARTESIAN_POINT ( 'NONE',  ( 85.41283022940925207, -32.17522569109155484, 180.5326087057368056 ) ) ;
#61461 = CARTESIAN_POINT ( 'NONE',  ( 0.000000000000000000, 47.00000000000000000, 0.000000000000000000 ) ) ;
#61462 = DIRECTION ( 'NONE',  ( 0.000000000000000000, 0.000000000000000000, 1.000000000000000000 ) ) ;
#61463 = ORIENTED_EDGE ( 'NONE', *, *, #18821, .F. ) ;
#61464 = CARTESIAN_POINT ( 'NONE',  ( -88.90359386438426270, -60.15364184676742099, 46.79264400712646221 ) ) ;
#61465 = CIRCLE ( 'NONE', #75210, 3.309500000000001663 ) ;
#61466 = DIRECTION ( 'NONE',  ( -1.000000000000000000, -1.224606353822377258E-16, -0.000000000000000000 ) ) ;
#61467 = CARTESIAN_POINT ( 'NONE',  ( 4.766030446259729381, -5.000000000000002665, -97.32770387339404294 ) ) ;
#61468 = LINE ( 'NONE', #377, #81693 ) ;
#61469 = AXIS2_PLACEMENT_3D ( 'NONE', #6144, #71411, #29929 ) ;
#61470 = SURFACE_SIDE_STYLE ('',( #11279 ) ) ;
#61471 = CARTESIAN_POINT ( 'NONE',  ( 27.85340566596032374, -60.00000000000001421, 42.07270389097206476 ) ) ;
#61472 = CARTESIAN_POINT ( 'NONE',  ( 15.28118917856605563, -22.84720680763436818, 35.97391546425213704 ) ) ;
#61473 = CARTESIAN_POINT ( 'NONE',  ( 46.91226987233839907, -28.92226484961306809, 42.23736541826801982 ) ) ;
#61475 = CARTESIAN_POINT ( 'NONE',  ( -12.68805576174265504, 23.09990985348045456, 5.374855948767180536 ) ) ;
#61474 = CARTESIAN_POINT ( 'NONE',  ( 89.06666666666666288, -4.171999999999998820, 5.616230220889773285E-16 ) ) ;
#61476 = EDGE_CURVE ( 'NONE', #34409, #60770, #60982, .T. ) ;
#61477 = CARTESIAN_POINT ( 'NONE',  ( 4.240736524178923439, 300.6921934601160729, -10.01075408398112643 ) ) ;
#61478 = CARTESIAN_POINT ( 'NONE',  ( 45.43339346675878687, 430.7348383325900727, 7.234598910837349628 ) ) ;
#61479 = CARTESIAN_POINT ( 'NONE',  ( 38.04621267582680133, 308.1715813180469468, 1.136581563559742269 ) ) ;
#61480 = DIRECTION ( 'NONE',  ( 1.000000000000000000, 1.224606353822377258E-16, 0.000000000000000000 ) ) ;
#61481 = DIRECTION ( 'NONE',  ( 0.000000000000000000, 0.000000000000000000, 1.000000000000000000 ) ) ;
#61482 = ORIENTED_EDGE ( 'NONE', *, *, #26457, .T. ) ;
#61483 = CARTESIAN_POINT ( 'NONE',  ( -6.763850406535977022, 294.7356673863635592, 9.912314076180619438 ) ) ;
#61484 = CIRCLE ( 'NONE', #42512, 12.00000000000001066 ) ;
#61485 = B_SPLINE_CURVE_WITH_KNOTS ( 'NONE', 3,
 ( #57024, #23637, #6891, #8484, #33861, #90474 ),
 .UNSPECIFIED., .F., .F.,
 ( 4, 2, 4 ),
 ( 2.380733003139562229E-07, 0.001898835937927376583, 0.003797433802554438936 ),
 .UNSPECIFIED. ) ;
#61486 = DIRECTION ( 'NONE',  ( -1.000000000000000000, -1.224606353822377258E-16, -0.000000000000000000 ) ) ;
#61487 = VERTEX_POINT ( 'NONE', #106321 ) ;
#61488 = CARTESIAN_POINT ( 'NONE',  ( -11.81863854137958647, -1.931387118382052570, 20.62778170009254808 ) ) ;
#61489 = CARTESIAN_POINT ( 'NONE',  ( 0.000000000000000000, 3.500000000000000000, 0.000000000000000000 ) ) ;
#61490 = PRESENTATION_LAYER_ASSIGNMENT (  '', '', ( #80396 ) ) ;
#61491 = CARTESIAN_POINT ( 'NONE',  ( 4.472135954999578722, -65.00000000000000000, -4.000000000000002665 ) ) ;
#61492 = EDGE_CURVE ( 'NONE', #76319, #77337, #56716, .T. ) ;
#61494 = CARTESIAN_POINT ( 'NONE',  ( -6.199981704917457925, -21.77037438476674325, -30.42741826779913694 ) ) ;
#61493 = CARTESIAN_POINT ( 'NONE',  ( 9.999945253488261798, 253.9998631337052757, -0.2662901834231035103 ) ) ;
#61495 = VERTEX_POINT ( 'NONE', #24404 ) ;
#61496 = CYLINDRICAL_SURFACE ( 'NONE', #73888, 5.000000000000000888 ) ;
#61497 = CARTESIAN_POINT ( 'NONE',  ( 4.678819457397886517, 143.9212778189118467, 5.000000000000000000 ) ) ;
#61498 = ORIENTED_EDGE ( 'NONE', *, *, #7883, .T. ) ;
#61499 = CARTESIAN_POINT ( 'NONE',  ( 0.01372220897661678186, 5.309964801958117597, -3.802871176606132053 ) ) ;
#61500 = CARTESIAN_POINT ( 'NONE',  ( 34.83349330513379982, 1.593028355512270567E-15, 0.000000000000000000 ) ) ;
#61501 = CARTESIAN_POINT ( 'NONE',  ( -94.42521480436519710, -60.00000000000000000, 44.71142204259329844 ) ) ;
#61502 = ORIENTED_EDGE ( 'NONE', *, *, #60017, .T. ) ;
#61503 = LINE ( 'NONE', #86840, #74675 ) ;
#61504 = DIRECTION ( 'NONE',  ( 1.000000000000000000, 1.224606353822377258E-16, 0.000000000000000000 ) ) ;
#61505 = CARTESIAN_POINT ( 'NONE',  ( 16.46332378338231095, 294.5649011048989792, 1.876034907501067828 ) ) ;
#61506 = VECTOR ( 'NONE', #68645, 1000.000000000000000 ) ;
#61507 = PRESENTATION_STYLE_ASSIGNMENT (( #28626 ) ) ;
#61509 = ADVANCED_FACE ( 'NONE', ( #63781 ), #105286, .T. ) ;
#61508 = B_SPLINE_CURVE_WITH_KNOTS ( 'NONE', 3,
 ( #44981, #102668, #77864, #1821, #104785 ),
 .UNSPECIFIED., .F., .F.,
 ( 4, 1, 4 ),
 ( 6.258780363497294494E-20, 0.003752776749732572668, 0.007505553499465145335 ),
 .UNSPECIFIED. ) ;
#61510 = CARTESIAN_POINT ( 'NONE',  ( -83.37195354553843174, -36.00313111294963875, 167.8019081912905790 ) ) ;
#61511 = AXIS2_PLACEMENT_3D ( 'NONE', #95660, #78406, #5575 ) ;
#61512 = ORIENTED_EDGE ( 'NONE', *, *, #35352, .T. ) ;
#61513 = DIRECTION ( 'NONE',  ( -1.000000000000000000, -1.224606353822377258E-16, -0.000000000000000000 ) ) ;
#61514 = ORIENTED_EDGE ( 'NONE', *, *, #105270, .T. ) ;
#61515 = VERTEX_POINT ( 'NONE', #7628 ) ;
#61516 = CARTESIAN_POINT ( 'NONE',  ( 3.631902923573203879, -4.332661967060489339, 17.83376356531591611 ) ) ;
#61517 = PRESENTATION_STYLE_ASSIGNMENT (( #13983 ) ) ;
#61518 = FACE_OUTER_BOUND ( 'NONE', #80764, .T. ) ;
#61519 = ORIENTED_EDGE ( 'NONE', *, *, #17969, .T. ) ;
#61520 = CARTESIAN_POINT ( 'NONE',  ( 33.86650669486618881, 0.000000000000000000, 4.000000000000000888 ) ) ;
#61521 = DIRECTION ( 'NONE',  ( 0.000000000000000000, 0.000000000000000000, -1.000000000000000000 ) ) ;
#61522 = CARTESIAN_POINT ( 'NONE',  ( -93.58432581829866592, -57.65368546899212987, -15.63533335066522767 ) ) ;
#61523 = CARTESIAN_POINT ( 'NONE',  ( 7.344133061198930612, -12.44494392680577555, 3.176267128233872583 ) ) ;
#61524 = CARTESIAN_POINT ( 'NONE',  ( 44.11327388758677870, 464.4313852428367682, 9.822198357555455672 ) ) ;
#61525 = AXIS2_PLACEMENT_3D ( 'NONE', #69976, #29044, #4715 ) ;
#61526 = CARTESIAN_POINT ( 'NONE',  ( -10.00004721872059754, 100.9998819531884919, -0.2617599822266485909 ) ) ;
#61527 = AXIS2_PLACEMENT_3D ( 'NONE', #28773, #29297, #61652 ) ;
#61528 = CARTESIAN_POINT ( 'NONE',  ( 3.409011323176964758, 15.24615751665866981, -9.403185743875123848 ) ) ;
#61529 = CARTESIAN_POINT ( 'NONE',  ( 69.60540008574220394, -30.00000000000001421, -29.89027719438221453 ) ) ;
#61530 = CARTESIAN_POINT ( 'NONE',  ( -76.70274796309844589, -29.99999999999996447, 172.7051753936532066 ) ) ;
#61531 = CARTESIAN_POINT ( 'NONE',  ( -54.96692882686725312, -36.03106141262587414, 58.82583099766474533 ) ) ;
#61532 = ORIENTED_EDGE ( 'NONE', *, *, #45301, .T. ) ;
#61533 = SURFACE_STYLE_USAGE ( .BOTH. , #54986 ) ;
#61534 = CONICAL_SURFACE ( 'NONE', #46048, 4.000000000000001776, 0.9599310885968808105 ) ;
#61536 = ORIENTED_EDGE ( 'NONE', *, *, #36390, .T. ) ;
#61535 = CIRCLE ( 'NONE', #95937, 8.500000000000000000 ) ;
#61537 = CARTESIAN_POINT ( 'NONE',  ( -100.9568756953421342, -52.73574583597550713, 193.4176276002172585 ) ) ;
#61539 = CIRCLE ( 'NONE', #83910, 3.999999999999999112 ) ;
#61538 = CARTESIAN_POINT ( 'NONE',  ( 102.2191329667627713, -37.99999999999999289, 182.8622780301718365 ) ) ;
#61540 = CARTESIAN_POINT ( 'NONE',  ( -6.399272939559234707, 51.30530844324656670, 7.881311681917864576 ) ) ;
#61541 = ORIENTED_EDGE ( 'NONE', *, *, #30556, .T. ) ;
#61542 = CARTESIAN_POINT ( 'NONE',  ( 4.852941176470592310, -2.999999999999999112, -70.80672828634229177 ) ) ;
#61543 = CARTESIAN_POINT ( 'NONE',  ( 5.082755093536324154, -15.21875000204838457, 5.082755093536326818 ) ) ;
#61544 = CARTESIAN_POINT ( 'NONE',  ( 0.000000000000000000, 0.000000000000000000, -7.381345277524544279 ) ) ;
#61545 = AXIS2_PLACEMENT_3D ( 'NONE', #104181, #78318, #62171 ) ;
#61546 = DIRECTION ( 'NONE',  ( 0.000000000000000000, -1.000000000000000000, 0.000000000000000000 ) ) ;
#61547 =( BOUNDED_SURFACE ( )  B_SPLINE_SURFACE ( 3, 2, ( 
 ( #25711, #25158, #32717 ),
 ( #8404, #6814, #106026 ),
 ( #98473, #65055, #80692 ),
 ( #273, #65586, #66652 ),
 ( #106567, #15972, #33241 ),
 ( #24626, #7335, #98994 ) ),
 .UNSPECIFIED., .F., .F., .F. ) 
 B_SPLINE_SURFACE_WITH_KNOTS ( ( 4, 2, 4 ),
 ( 3, 3 ),
 ( 0.003190620565844237266, 0.007281897438794509257, 0.01137317431174478082 ),
 ( 0.000000000000000000, 1.000000000000000000 ),
 .UNSPECIFIED. ) 
 GEOMETRIC_REPRESENTATION_ITEM ( )  RATIONAL_B_SPLINE_SURFACE ( (
 ( 1.000000000000000000, 0.8047731410850398337, 1.000000000000000000),
 ( 1.000000000000000000, 0.8125552299156226788, 1.000000000000000000),
 ( 1.000000000000000000, 0.8191520442889870246, 1.000000000000000000),
 ( 1.000000000000000000, 0.8191520442889870246, 1.000000000000000000),
 ( 1.000000000000000000, 0.8125552299156239000, 1.000000000000000000),
 ( 1.000000000000000000, 0.8047731410850399447, 1.000000000000000000) ) ) 
 REPRESENTATION_ITEM ( '' )  SURFACE ( )  );
#61548 = FILL_AREA_STYLE_COLOUR ( '', #41276 ) ;
#61549 = CARTESIAN_POINT ( 'NONE',  ( 65.93937847753362291, -29.99999999999999645, 82.94257298685835167 ) ) ;
#61550 = CARTESIAN_POINT ( 'NONE',  ( 22.42417502586373246, 305.3961751430792333, 10.05444931189341773 ) ) ;
#61551 = CARTESIAN_POINT ( 'NONE',  ( -9.960428250040571641, 43.33465522821285987, -15.36733472782074550 ) ) ;
#61552 = CARTESIAN_POINT ( 'NONE',  ( 13.50000000000000533, -7.794228634059982674, -11.79422863405993382 ) ) ;
#61553 = CARTESIAN_POINT ( 'NONE',  ( -7.500000000000007105, 42.86855997971688481, -62.45407030448338048 ) ) ;
#61554 = CARTESIAN_POINT ( 'NONE',  ( -28.85079751128344938, -32.53587765291774758, 31.52101463460818564 ) ) ;
#61555 = CARTESIAN_POINT ( 'NONE',  ( 47.02088286195116495, -36.06800221881119484, 45.21478074418502757 ) ) ;
#61556 = CARTESIAN_POINT ( 'NONE',  ( 4.898587196589412829E-16, -13.62499999999999112, -8.000000000000000000 ) ) ;
#61557 = CARTESIAN_POINT ( 'NONE',  ( -0.6447495452450531239, 46.14900100259577442, 16.41618316663220511 ) ) ;
#61558 = CARTESIAN_POINT ( 'NONE',  ( -85.92922987661015100, -38.64615708810908501, 199.0210877423697866 ) ) ;
#61559 = AXIS2_PLACEMENT_3D ( 'NONE', #80494, #72930, #100277 ) ;
#61560 = VERTEX_POINT ( 'NONE', #32488 ) ;
#61561 = CARTESIAN_POINT ( 'NONE',  ( -9.500000000000000000, -5.000000000000000000, -20.99851272547259384 ) ) ;
#61562 =( NAMED_UNIT ( * ) SI_UNIT ( $, .STERADIAN. ) SOLID_ANGLE_UNIT ( ) );
#61563 = CARTESIAN_POINT ( 'NONE',  ( -48.02835407290533709, 11.61227450977237119, -14.35535821593460248 ) ) ;
#61564 = SURFACE_STYLE_USAGE ( .BOTH. , #79310 ) ;
#61565 = CARTESIAN_POINT ( 'NONE',  ( 6.195804100829465533, 41.59435685053998810, -70.65487364791137281 ) ) ;
#61566 = CARTESIAN_POINT ( 'NONE',  ( 5.656854249492380582, -26.00000000409677270, -5.656854249492379694 ) ) ;
#61567 = CARTESIAN_POINT ( 'NONE',  ( 5.656854249492380582, -17.00000000409676915, -5.656854249492379694 ) ) ;
#61568 = DIRECTION ( 'NONE',  ( 1.150791560227848544E-16, -0.3420201433256727652, 0.9396926207859068736 ) ) ;
#61569 = VECTOR ( 'NONE', #36754, 1000.000000000000000 ) ;
#61570 = CARTESIAN_POINT ( 'NONE',  ( 112.1703215029695286, -59.99999999999999289, 168.8166208195475519 ) ) ;
#61571 = VECTOR ( 'NONE', #4769, 1000.000000000000000 ) ;
#61572 = EDGE_CURVE ( 'NONE', #49420, #89178, #90226, .T. ) ;
#61573 = CARTESIAN_POINT ( 'NONE',  ( -7.150053860865846822, -66.78265453913975591, 3.590189269391292903 ) ) ;
#61574 = ORIENTED_EDGE ( 'NONE', *, *, #63299, .F. ) ;
#61575 = EDGE_CURVE ( 'NONE', #68507, #40311, #100582, .T. ) ;
#61576 = CARTESIAN_POINT ( 'NONE',  ( 3.677584134044423969, -48.98458100588077713, 104.5297932675492376 ) ) ;
#61577 = CARTESIAN_POINT ( 'NONE',  ( -81.44309280902999149, -30.00000000000002132, 29.19263923180426445 ) ) ;
#61578 = ORIENTED_EDGE ( 'NONE', *, *, #40871, .F. ) ;
#61580 = CARTESIAN_POINT ( 'NONE',  ( 5.221682558027961107, 7.016321058000157151, -27.48376762107660554 ) ) ;
#61579 = FILL_AREA_STYLE ('',( #104946 ) ) ;
#61581 = CARTESIAN_POINT ( 'NONE',  ( 12.47891400660274464, -3.648257510622830768, -13.58339488149144003 ) ) ;
#61582 = CARTESIAN_POINT ( 'NONE',  ( -7.791781413346525298, -2.999999999999999556, 2.093983074874242956 ) ) ;
#61583 = CARTESIAN_POINT ( 'NONE',  ( 39.83065760000189215, 436.5763539059782374, 5.509783410166992468 ) ) ;
#61584 = CARTESIAN_POINT ( 'NONE',  ( 4.401442555609581635E-16, -16.15625000204838457, -7.188101187500000044 ) ) ;
#61585 = CARTESIAN_POINT ( 'NONE',  ( 1.570796324976846403, -5.000000000000002665, -97.00000000000000000 ) ) ;
#61586 = B_SPLINE_CURVE_WITH_KNOTS ( 'NONE', 3,
 ( #97067, #63123, #31315, #88986, #64198, #23213, #22149, #4888, #54458, #13485, #56051, #88465, #15085, #55000, #53946, #87410, #96555, #5925, #38853, #14539, #104631, #30780 ),
 .UNSPECIFIED., .F., .F.,
 ( 4, 2, 2, 2, 2, 2, 2, 2, 2, 2, 4 ),
 ( 0.006473714219450311426, 0.006725523206561636463, 0.006977332193672962368, 0.007480950167895608974, 0.007984568142118255579, 0.008488186116340902185, 0.009495422064786186722, 0.009747231051897509158, 0.009999040039008831593, 0.01025084902612015403, 0.01050265801323147646 ),
 .UNSPECIFIED. ) ;
#61587 = DIRECTION ( 'NONE',  ( 0.000000000000000000, 0.000000000000000000, 1.000000000000000000 ) ) ;
#61589 = ORIENTED_EDGE ( 'NONE', *, *, #61426, .F. ) ;
#61588 = CARTESIAN_POINT ( 'NONE',  ( -7.500000000000006217, 39.99999999999999289, -62.89165061481655528 ) ) ;
#61590 = CARTESIAN_POINT ( 'NONE',  ( 85.65051399455167314, -18.54895490038211747, 161.4844583081507778 ) ) ;
#61591 = CARTESIAN_POINT ( 'NONE',  ( -43.90320859248178209, 462.7132367860276076, 5.469326048303289056 ) ) ;
#61592 = AXIS2_PLACEMENT_3D ( 'NONE', #49206, #48671, #71905 ) ;
#61593 = FACE_OUTER_BOUND ( 'NONE', #58118, .T. ) ;
#61594 = VERTEX_POINT ( 'NONE', #76090 ) ;
#61595 = CARTESIAN_POINT ( 'NONE',  ( 15.11650669486618881, 1.474610560812782335E-15, 0.000000000000000000 ) ) ;
#61596 = CARTESIAN_POINT ( 'NONE',  ( 17.83057459411148926, 34.57788205794057035, 22.40555159655071549 ) ) ;
#61597 = CARTESIAN_POINT ( 'NONE',  ( 0.000000000000000000, 48.00000000000000000, 0.000000000000000000 ) ) ;
#61598 = CYLINDRICAL_SURFACE ( 'NONE', #57122, 1.250000000000000222 ) ;
#61599 = DIRECTION ( 'NONE',  ( 0.000000000000000000, 0.000000000000000000, 1.000000000000000000 ) ) ;
#61600 = CARTESIAN_POINT ( 'NONE',  ( 1.248765323091368673, 16.16828180304352358, 50.36968963469745830 ) ) ;
#61601 = B_SPLINE_CURVE_WITH_KNOTS ( 'NONE', 3,
 ( #58198, #67891, #9105, #75978, #34505, #83531, #67370, #2075 ),
 .UNSPECIFIED., .F., .F.,
 ( 4, 2, 2, 4 ),
 ( 0.007886720825438852528, 0.009850969036564048015, 0.01181521724768924524, 0.01574371366993963101 ),
 .UNSPECIFIED. ) ;
#61602 = CARTESIAN_POINT ( 'NONE',  ( 8.928123070943627226, -1.462223317312293158, 15.49551036417120109 ) ) ;
#61603 = ORIENTED_EDGE ( 'NONE', *, *, #99371, .T. ) ;
#61604 =( NAMED_UNIT ( * ) PLANE_ANGLE_UNIT ( ) SI_UNIT ( $, .RADIAN. ) );
#61605 = AXIS2_PLACEMENT_3D ( 'NONE', #83367, #93606, #11596 ) ;
#61606 = CIRCLE ( 'NONE', #89064, 3.309500000000001663 ) ;
#61607 = CARTESIAN_POINT ( 'NONE',  ( -76.65309938956929159, -30.00000000000000355, -16.89940168842986878 ) ) ;
#61608 = CARTESIAN_POINT ( 'NONE',  ( -5.000000000000000000, -49.64217499592842131, 7.481703942370503846 ) ) ;
#61609 = CARTESIAN_POINT ( 'NONE',  ( -10.00000000000000355, 105.0000000000000000, 4.000000000000001776 ) ) ;
#61611 = FACE_OUTER_BOUND ( 'NONE', #1878, .T. ) ;
#61610 = CYLINDRICAL_SURFACE ( 'NONE', #13799, 4.000000000000000000 ) ;
#61612 = ADVANCED_FACE ( 'NONE', ( #75566 ), #100368, .T. ) ;
#61613 = CARTESIAN_POINT ( 'NONE',  ( 4.401442555609581635E-16, -26.28125000204838813, -7.188101187500000044 ) ) ;
#61614 = VECTOR ( 'NONE', #103104, 1000.000000000000000 ) ;
#61615 = STYLED_ITEM ( 'NONE', ( #1345 ), #58526 ) ;
#61616 = CARTESIAN_POINT ( 'NONE',  ( 13.28162482383687859, 294.5489039831744549, -10.06438307193624304 ) ) ;
#61617 = VECTOR ( 'NONE', #76230, 1000.000000000000000 ) ;
#61618 = LINE ( 'NONE', #85338, #55168 ) ;
#61619 = DIRECTION ( 'NONE',  ( 0.2259255479511208531, 0.3692254281733069465, 0.9014600545632757145 ) ) ;
#61620 = ITEM_DEFINED_TRANSFORMATION ( 'NONE', 'NONE', #21470,  #10728 ) ;
#61621 = ORIENTED_EDGE ( 'NONE', *, *, #53627, .F. ) ;
#61622 = DIRECTION ( 'NONE',  ( -1.000000000000000000, -0.000000000000000000, -0.000000000000000000 ) ) ;
#61623 = CARTESIAN_POINT ( 'NONE',  ( 7.500000000000000000, 1.572594658376116339, -7.069792055233641292 ) ) ;
#61624 = CARTESIAN_POINT ( 'NONE',  ( -7.883628181806170865, 62.00818940277061841, 0.000000000000000000 ) ) ;
#61625 = ADVANCED_FACE ( 'NONE', ( #28123 ), #35685, .F. ) ;
#61626 = CARTESIAN_POINT ( 'NONE',  ( 94.84444444444443434, -4.171999999999998820, 0.000000000000000000 ) ) ;
#61627 = EDGE_LOOP ( 'NONE', ( #55403, #57717, #3962, #5258 ) ) ;
#61628 = AXIS2_PLACEMENT_3D ( 'NONE', #63736, #96618, #22755 ) ;
#61629 = CARTESIAN_POINT ( 'NONE',  ( -1.469576158976823947E-15, -17.37499999999999289, 8.000000000000000000 ) ) ;
#61630 = CARTESIAN_POINT ( 'NONE',  ( -2.040829700809986047, 50.00000000000000000, -98.00000000000000000 ) ) ;
#61631 = ORIENTED_EDGE ( 'NONE', *, *, #91727, .T. ) ;
#61632 = CARTESIAN_POINT ( 'NONE',  ( -27.26583764555563150, 34.42251079669566138, 10.05698433968616357 ) ) ;
#61633 = CARTESIAN_POINT ( 'NONE',  ( -0.9999999999999943379, -1.409462824231155764E-15, 101.0455488498966758 ) ) ;
#61634 = AXIS2_PLACEMENT_3D ( 'NONE', #33681, #51426, #50885 ) ;
#61635 = CARTESIAN_POINT ( 'NONE',  ( 9.380871178326117388, 102.9888362020167563, 3.467392232194208557 ) ) ;
#61636 = CARTESIAN_POINT ( 'NONE',  ( -17.53682258900660074, 36.29665952923689076, 24.04445569364172286 ) ) ;
#61637 = CARTESIAN_POINT ( 'NONE',  ( -106.1374248126797539, -60.00000000000000000, 198.1280823682561447 ) ) ;
#61638 =( LENGTH_UNIT ( ) NAMED_UNIT ( * ) SI_UNIT ( .MILLI., .METRE. ) );
#61639 = DIRECTION ( 'NONE',  ( 0.000000000000000000, 0.000000000000000000, -1.000000000000000000 ) ) ;
#61640 = CARTESIAN_POINT ( 'NONE',  ( 6.274480239423446903, 53.84149731873487355, -6.494774485913110240 ) ) ;
#61641 = CARTESIAN_POINT ( 'NONE',  ( 17.08002596387369110, 34.90866943516432030, -21.84018144932510808 ) ) ;
#61642 = MECHANICAL_DESIGN_GEOMETRIC_PRESENTATION_REPRESENTATION (  '', ( #92636 ), #52995 ) ;
#61643 = EDGE_CURVE ( 'NONE', #41445, #40039, #97137, .T. ) ;
#61644 = CARTESIAN_POINT ( 'NONE',  ( -84.04979895421557501, -42.98303161459435984, 182.1087557225411899 ) ) ;
#61645 = CARTESIAN_POINT ( 'NONE',  ( 39.45041558553427308, 41.98133502302429321, -56.26464531454707441 ) ) ;
#61646 = AXIS2_PLACEMENT_3D ( 'NONE', #24899, #26517, #66941 ) ;
#61647 = VERTEX_POINT ( 'NONE', #20043 ) ;
#61648 = CARTESIAN_POINT ( 'NONE',  ( -9.034470188793504164, 46.02977034662631439, -14.11149907944951920 ) ) ;
#61649 = ADVANCED_FACE ( 'NONE', ( #52345 ), #2366, .F. ) ;
#61650 = PRESENTATION_STYLE_ASSIGNMENT (( #28771 ) ) ;
#61651 = CARTESIAN_POINT ( 'NONE',  ( -86.94550892133041486, -60.17282562918532562, -3.944479883897415995 ) ) ;
#61652 = DIRECTION ( 'NONE',  ( 0.000000000000000000, -1.000000000000000000, 0.000000000000000000 ) ) ;
#61653 = CARTESIAN_POINT ( 'NONE',  ( -3.227719910292865091, 36.27072058310572089, -5.000000000000000000 ) ) ;
#61654 = CARTESIAN_POINT ( 'NONE',  ( 8.224453817208788209, 115.5406540063851679, 0.000000000000000000 ) ) ;
#61655 = DIRECTION ( 'NONE',  ( 0.000000000000000000, -1.000000000000000000, 0.000000000000000000 ) ) ;
#61656 = CARTESIAN_POINT ( 'NONE',  ( -29.83308852624522345, 41.99999999999999289, 51.76085035109112198 ) ) ;
#61657 = EDGE_CURVE ( 'NONE', #89196, #5935, #68467, .T. ) ;
#61658 = CIRCLE ( 'NONE', #9964, 5.000000000000002665 ) ;
#61659 = CARTESIAN_POINT ( 'NONE',  ( 70.80389978121282013, -30.00000000000000711, 131.5992258684728995 ) ) ;
#61660 = CARTESIAN_POINT ( 'NONE',  ( 0.000000000000000000, 61.50000000000000000, -6.999999999999992895 ) ) ;
#61661 = CARTESIAN_POINT ( 'NONE',  ( -87.76943268072510307, -14.21045842199432307, -6.547605000374890238 ) ) ;
#61662 = CARTESIAN_POINT ( 'NONE',  ( -64.69100649186263752, -29.05538772269134284, 79.90073128498799804 ) ) ;
#61663 = VERTEX_POINT ( 'NONE', #19511 ) ;
#61664 = CARTESIAN_POINT ( 'NONE',  ( 100.3457197225335733, -14.21045842199427511, 196.5350150060856720 ) ) ;
#61665 = CARTESIAN_POINT ( 'NONE',  ( 55.21742879405702098, 39.42598490589298876, 34.80677065731995867 ) ) ;
#61666 = CARTESIAN_POINT ( 'NONE',  ( 35.13867974785705428, -59.99999999999999289, 49.78873796555570408 ) ) ;
#61667 = EDGE_CURVE ( 'NONE', #58869, #54340, #3815, .T. ) ;
#61668 = VERTEX_POINT ( 'NONE', #68010 ) ;
#61669 = CARTESIAN_POINT ( 'NONE',  ( -33.78656477175679385, 463.8460037826917528, 7.347243016405096583 ) ) ;
#61670 = CARTESIAN_POINT ( 'NONE',  ( 5.082755093536325930, -28.34375000204838813, -5.082755093536325042 ) ) ;
#61671 = CARTESIAN_POINT ( 'NONE',  ( -5.725989721596478788, -6.423228887435400658, 1.809923354557177344 ) ) ;
#61672 = ORIENTED_EDGE ( 'NONE', *, *, #37648, .T. ) ;
#61674 = DIRECTION ( 'NONE',  ( -0.000000000000000000, -1.000000000000000000, -0.000000000000000000 ) ) ;
#61673 = TOROIDAL_SURFACE ( 'NONE', #90905, 7.025805963803935406, 3.000000000000000000 ) ;
#61675 = EDGE_LOOP ( 'NONE', ( #6245, #51810, #104634, #85453 ) ) ;
#61676 = DIRECTION ( 'NONE',  ( 0.000000000000000000, 0.000000000000000000, 1.000000000000000000 ) ) ;
#61677 = ADVANCED_FACE ( 'NONE', ( #1662 ), #59405, .T. ) ;
#61678 =( NAMED_UNIT ( * ) PLANE_ANGLE_UNIT ( ) SI_UNIT ( $, .RADIAN. ) );
#61679 = CARTESIAN_POINT ( 'NONE',  ( -88.36461763089066324, -60.00000000000001421, -21.16661413833238825 ) ) ;
#61680 = CARTESIAN_POINT ( 'NONE',  ( 0.000000000000000000, 38.67090180175566871, 0.000000000000000000 ) ) ;
#61681 = CARTESIAN_POINT ( 'NONE',  ( 2.977408999572650927, -9.875000002048386349, -7.188101187500001821 ) ) ;
#61682 = CARTESIAN_POINT ( 'NONE',  ( 32.11956073034194503, 486.1307440743741495, 5.366431738779005478 ) ) ;
#61683 = CARTESIAN_POINT ( 'NONE',  ( -1.544427540536530316E-15, -4.285714285714290916, 25.22241582816893057 ) ) ;
#61684 = FACE_OUTER_BOUND ( 'NONE', #92920, .T. ) ;
#61685 = CARTESIAN_POINT ( 'NONE',  ( -6.043427762771305112, 50.00000000000000000, -74.51456333905269958 ) ) ;
#61686 = CARTESIAN_POINT ( 'NONE',  ( -7.986539162393897939, 108.9732717105745223, -0.5321833565149903800 ) ) ;
#61687 = CARTESIAN_POINT ( 'NONE',  ( -8.000000000000000000, 0.000000000000000000, -7.424942857142857733 ) ) ;
#61688 = EDGE_LOOP ( 'NONE', ( #87922, #40687, #5148, #75201 ) ) ;
#61689 = CARTESIAN_POINT ( 'NONE',  ( -28.08715220167751170, 18.64284798593048365, 26.23039857545936826 ) ) ;
#61690 = AXIS2_PLACEMENT_3D ( 'NONE', #87380, #105661, #79268 ) ;
#61692 = CARTESIAN_POINT ( 'NONE',  ( 34.28021199336672709, -32.56668617693117795, 33.60777154440098968 ) ) ;
#61691 = CARTESIAN_POINT ( 'NONE',  ( 34.12349128637462314, 490.8027302422241291, 11.84948222508890403 ) ) ;
#61693 = CARTESIAN_POINT ( 'NONE',  ( -25.22241582816893413, -4.285714285714287364, -3.301606509427108982 ) ) ;
#61694 = ORIENTED_EDGE ( 'NONE', *, *, #48848, .T. ) ;
#61695 = DIRECTION ( 'NONE',  ( 0.000000000000000000, 0.000000000000000000, 1.000000000000000000 ) ) ;
#61696 = AXIS2_PLACEMENT_3D ( 'NONE', #98604, #16635, #39468 ) ;
#61697 = DIRECTION ( 'NONE',  ( -1.000000000000000000, -1.224606353822377258E-16, -0.000000000000000000 ) ) ;
#61698 = CARTESIAN_POINT ( 'NONE',  ( -44.15895461026264712, 485.1651389999502157, 0.5848183293849077424 ) ) ;
#61699 = AXIS2_PLACEMENT_3D ( 'NONE', #88213, #32649, #48253 ) ;
#61700 = SURFACE_SIDE_STYLE ('',( #102120 ) ) ;
#61701 = FACE_OUTER_BOUND ( 'NONE', #29486, .T. ) ;
#61702 = DIRECTION ( 'NONE',  ( -1.000000000000000000, -1.224606353822377258E-16, -0.000000000000000000 ) ) ;
#61703 = CARTESIAN_POINT ( 'NONE',  ( -7.500000000000000000, 4.330127018922188320, -7.422398894150033399 ) ) ;
#61704 = ORIENTED_EDGE ( 'NONE', *, *, #70250, .F. ) ;
#61705 = CARTESIAN_POINT ( 'NONE',  ( 92.01607953741286394, -60.00000000000001421, 18.77391487596767661 ) ) ;
#61706 = CARTESIAN_POINT ( 'NONE',  ( 5.000000000000000000, -63.32102160712415895, 12.61250543006184088 ) ) ;
#61707 = SURFACE_STYLE_FILL_AREA ( #93525 ) ;
#61708 = CARTESIAN_POINT ( 'NONE',  ( -5.231947880461875755, 41.12212895974708715, -70.85062085811149757 ) ) ;
#61709 = CARTESIAN_POINT ( 'NONE',  ( -11.69375096826101768, 11.66688986588565591, -9.917519730966944280 ) ) ;
#61710 = ORIENTED_EDGE ( 'NONE', *, *, #20351, .F. ) ;
#61711 = EDGE_CURVE ( 'NONE', #16669, #27639, #24804, .T. ) ;
#61712 = CIRCLE ( 'NONE', #15160, 4.000000000000001776 ) ;
#61713 = CARTESIAN_POINT ( 'NONE',  ( -102.9438915830126291, -29.99999999999873879, 197.5134625135077613 ) ) ;
#61714 = EDGE_LOOP ( 'NONE', ( #81560, #96443, #85500, #11925, #15020, #37668, #49684 ) ) ;
#61715 = CARTESIAN_POINT ( 'NONE',  ( 45.11650669486618881, 1.474610560812782335E-15, 0.000000000000000000 ) ) ;
#61716 = CARTESIAN_POINT ( 'NONE',  ( 2.212097561415784952, -14.31130214556283065, -12.46447053051439724 ) ) ;
#61717 = DIRECTION ( 'NONE',  ( 0.000000000000000000, -1.000000000000000000, 0.000000000000000000 ) ) ;
#61718 = CARTESIAN_POINT ( 'NONE',  ( 15.74152552778519443, 22.22013712430071308, 3.418714015814440454 ) ) ;
#61719 = CARTESIAN_POINT ( 'NONE',  ( 84.90240974134064800, -60.18835296399971213, -16.21870115458467865 ) ) ;
#61720 = CARTESIAN_POINT ( 'NONE',  ( -2.977408999572654480, -33.50000000204838813, 7.188101187499999156 ) ) ;
#61722 = EDGE_CURVE ( 'NONE', #98362, #79927, #43714, .T. ) ;
#61721 = DIRECTION ( 'NONE',  ( -1.000000000000000000, -0.000000000000000000, -0.000000000000000000 ) ) ;
#61723 = CARTESIAN_POINT ( 'NONE',  ( 9.267538580112169910, 46.19448214903180627, -13.41394971794144020 ) ) ;
#61724 = ORIENTED_EDGE ( 'NONE', *, *, #99929, .F. ) ;
#61725 = CARTESIAN_POINT ( 'NONE',  ( -24.22231588719698436, -19.79037096225153647, -33.14000009352793086 ) ) ;
#61726 = AXIS2_PLACEMENT_3D ( 'NONE', #6462, #14546, #53954 ) ;
#61728 = ORIENTED_EDGE ( 'NONE', *, *, #85366, .T. ) ;
#61727 = FILL_AREA_STYLE_COLOUR ( '', #47692 ) ;
#61729 = CARTESIAN_POINT ( 'NONE',  ( 79.06124460869463633, -53.37162188482365366, 155.5587481820264202 ) ) ;
#61730 = ORIENTED_EDGE ( 'NONE', *, *, #15801, .F. ) ;
#61731 = CARTESIAN_POINT ( 'NONE',  ( 1.529791816479536326, -49.97354766897922218, 44.88943603909616087 ) ) ;
#61732 = CARTESIAN_POINT ( 'NONE',  ( -5.082755093536326818, -16.71875000204838813, 5.082755093536325042 ) ) ;
#61733 = CARTESIAN_POINT ( 'NONE',  ( -105.2191501062491881, -57.64508961356604999, 201.5420537206667291 ) ) ;
#61734 = EDGE_CURVE ( 'NONE', #89859, #69966, #19598, .T. ) ;
#61735 = ORIENTED_EDGE ( 'NONE', *, *, #67655, .T. ) ;
#61736 = CIRCLE ( 'NONE', #78857, 0.5999999999999980904 ) ;
#61737 = CARTESIAN_POINT ( 'NONE',  ( 3.168307535684220966, 39.18401492176337797, 5.000000000000000888 ) ) ;
#61738 = CARTESIAN_POINT ( 'NONE',  ( 6.784953749580444615, 41.67963532863181797, -59.00226812211813154 ) ) ;
#61739 = CARTESIAN_POINT ( 'NONE',  ( 0.000000000000000000, -78.00000000000000000, 41.00000000000000000 ) ) ;
#61740 = EDGE_CURVE ( 'NONE', #37996, #22095, #96737, .T. ) ;
#61741 = CARTESIAN_POINT ( 'NONE',  ( 3.313708498984762052, -19.90625000409677270, -8.000000000000000000 ) ) ;
#61742 = CARTESIAN_POINT ( 'NONE',  ( 0.000000000000000000, -78.00000000000000000, 27.00000000000000000 ) ) ;
#61743 = CARTESIAN_POINT ( 'NONE',  ( 9.435590127032934760, 15.92795519102023860, 3.316968746324335804 ) ) ;
#61744 = DIRECTION ( 'NONE',  ( 0.000000000000000000, -1.000000000000000000, 0.000000000000000000 ) ) ;
#61745 = CARTESIAN_POINT ( 'NONE',  ( 5.327003236163648126, 25.27808877631457207, -43.98407828350998727 ) ) ;
#61746 = CARTESIAN_POINT ( 'NONE',  ( 5.126327086984646897, 52.11936742043627646, 6.031152949374359196 ) ) ;
#61747 =( NAMED_UNIT ( * ) PLANE_ANGLE_UNIT ( ) SI_UNIT ( $, .RADIAN. ) );
#61748 = CARTESIAN_POINT ( 'NONE',  ( 33.83651168703158163, 463.7543666047810120, 7.167145050618551672 ) ) ;
#61749 = ORIENTED_EDGE ( 'NONE', *, *, #86814, .T. ) ;
#61750 = CARTESIAN_POINT ( 'NONE',  ( -4.332563242637840872, -48.31029031541129370, 40.50631733802364209 ) ) ;
#61751 = CARTESIAN_POINT ( 'NONE',  ( -89.99999999999997158, -60.00000000000000000, 196.0238439516549818 ) ) ;
#61752 = CARTESIAN_POINT ( 'NONE',  ( 0.000000000000000000, 3.999999999999996447, 0.000000000000000000 ) ) ;
#61753 = CARTESIAN_POINT ( 'NONE',  ( 14.52379002078253301, -19.49130720279776696, -37.81483145485863417 ) ) ;
#61754 = CARTESIAN_POINT ( 'NONE',  ( -81.60074597489959558, -29.99999999999999289, 143.5170916637224252 ) ) ;
#61755 = EDGE_CURVE ( 'NONE', #96036, #61182, #78208, .T. ) ;
#61756 = CARTESIAN_POINT ( 'NONE',  ( 7.500000000000007105, 42.00000000000000711, -58.69229087761227959 ) ) ;
#61757 = ORIENTED_EDGE ( 'NONE', *, *, #9891, .F. ) ;
#61758 = PRESENTATION_LAYER_ASSIGNMENT (  '', '', ( #94474 ) ) ;
#61759 = CARTESIAN_POINT ( 'NONE',  ( -26.34368984043107531, 37.12851728967876852, -7.801921120626483130 ) ) ;
#61760 = VECTOR ( 'NONE', #48746, 1000.000000000000000 ) ;
#61761 = CARTESIAN_POINT ( 'NONE',  ( 75.28700688039084810, -57.56648276822033949, 191.4465710134679739 ) ) ;
#61762 = CIRCLE ( 'NONE', #30733, 62.00000000000000000 ) ;
#61763 = CARTESIAN_POINT ( 'NONE',  ( 5.036189803708993828, 48.00000000000000711, -93.73786388354255905 ) ) ;
#61764 = AXIS2_PLACEMENT_3D ( 'NONE', #50135, #3188, #43642 ) ;
#61765 = DIRECTION ( 'NONE',  ( 0.000000000000000000, 0.000000000000000000, 1.000000000000000000 ) ) ;
#61766 = CARTESIAN_POINT ( 'NONE',  ( 7.500000000000001776, -3.000000000000000000, -36.97043916959991350 ) ) ;
#61767 = LINE ( 'NONE', #93583, #46049 ) ;
#61768 = CARTESIAN_POINT ( 'NONE',  ( -61.04408880086688782, -60.00000000000000711, 104.0053245555540258 ) ) ;
#61769 = CARTESIAN_POINT ( 'NONE',  ( -2.075968632160785088, 6.306992450857870303, -6.056431503346635381 ) ) ;
#61770 = DIRECTION ( 'NONE',  ( 0.000000000000000000, 0.000000000000000000, -1.000000000000000000 ) ) ;
#61771 = CARTESIAN_POINT ( 'NONE',  ( 57.09426686933954898, 50.00000000000000000, -27.25041924768392576 ) ) ;
#61772 = CARTESIAN_POINT ( 'NONE',  ( -84.69478162058261717, -53.83175173781702938, 190.2051053124634166 ) ) ;
#61773 = ORIENTED_EDGE ( 'NONE', *, *, #34811, .T. ) ;
#61774 = CARTESIAN_POINT ( 'NONE',  ( 35.45196906070734855, 373.3971792367692615, 5.126420406680051833 ) ) ;
#61775 = CARTESIAN_POINT ( 'NONE',  ( -2.969389021251942484, -18.58608251166780079, 26.98300677151931382 ) ) ;
#61776 = CARTESIAN_POINT ( 'NONE',  ( -6.700949174070592207, 41.88761787213280741, -59.59787320614237416 ) ) ;
#61777 = CARTESIAN_POINT ( 'NONE',  ( 34.34679764914265121, 491.0133751866268312, 12.01297952733224150 ) ) ;
#61778 = PRESENTATION_STYLE_ASSIGNMENT (( #10530 ) ) ;
#61779 = EDGE_CURVE ( 'NONE', #68633, #13798, #9358, .T. ) ;
#61780 = DIRECTION ( 'NONE',  ( -1.000000000000000000, 0.000000000000000000, 0.000000000000000000 ) ) ;
#61781 = CARTESIAN_POINT ( 'NONE',  ( 39.36919468843574066, 490.3664410044918895, 11.50853341535465368 ) ) ;
#61782 = PRESENTATION_LAYER_ASSIGNMENT (  '', '', ( #1447 ) ) ;
#61783 = CARTESIAN_POINT ( 'NONE',  ( 97.15356149169568312, 1.016364837396684119E-14, 0.000000000000000000 ) ) ;
#61784 = CARTESIAN_POINT ( 'NONE',  ( 44.19066549755432760, 435.2576907183105845, 14.58870676253211762 ) ) ;
#61785 = EDGE_LOOP ( 'NONE', ( #60141, #17249 ) ) ;
#61786 = CARTESIAN_POINT ( 'NONE',  ( 17.75966234059601234, 50.00000000000002132, 62.25802333796747945 ) ) ;
#61787 = CARTESIAN_POINT ( 'NONE',  ( 14.11595029532508860, 2.410436752314647713, 5.024000119269133258 ) ) ;
#61788 = ADVANCED_FACE ( 'NONE', ( #10567 ), #42949, .T. ) ;
#61789 = CARTESIAN_POINT ( 'NONE',  ( -17.78317311657527000, -3.867350551647862515E-12, 13.66642973271121342 ) ) ;
#61790 = CIRCLE ( 'NONE', #25859, 7.000000000000000000 ) ;
#61791 = DIRECTION ( 'NONE',  ( 0.000000000000000000, -1.000000000000000000, 0.000000000000000000 ) ) ;
#61792 = CARTESIAN_POINT ( 'NONE',  ( 105.9102621261374253, -29.99999999999996803, 132.9887338302407898 ) ) ;
#61793 = CARTESIAN_POINT ( 'NONE',  ( -80.32583173421626555, -25.62118807212741345, 133.8900160517275708 ) ) ;
#61794 = ORIENTED_EDGE ( 'NONE', *, *, #74327, .F. ) ;
#61795 = DIRECTION ( 'NONE',  ( 0.000000000000000000, -1.000000000000000000, 0.000000000000000000 ) ) ;
#61796 = CARTESIAN_POINT ( 'NONE',  ( 0.000000000000000000, 60.00000000000000000, -23.66666666666665719 ) ) ;
#61797 = APPLICATION_CONTEXT ( 'automotive_design' ) ;
#61798 = CARTESIAN_POINT ( 'NONE',  ( 42.33349330513380693, 4.898587196589405926E-16, -4.000000000000001776 ) ) ;
#61799 = CARTESIAN_POINT ( 'NONE',  ( 45.37874805213238716, 369.5478906911545778, 5.965867277830504634 ) ) ;
#61800 = CARTESIAN_POINT ( 'NONE',  ( 34.73928765630499527, 485.6865374000855127, -2.860106678717950324 ) ) ;
#61801 = ORIENTED_EDGE ( 'NONE', *, *, #50642, .F. ) ;
#61802 = CARTESIAN_POINT ( 'NONE',  ( -20.24579557674103469, 304.8297271373346575, -10.00469232190998525 ) ) ;
#61803 = ADVANCED_FACE ( 'NONE', ( #51016 ), #74429, .T. ) ;
#61804 = CARTESIAN_POINT ( 'NONE',  ( 31.61511976764354870, 439.3933909026691822, 23.34297217120054313 ) ) ;
#61805 = CARTESIAN_POINT ( 'NONE',  ( 7.188101187500000044, -23.65625000204838457, 0.000000000000000000 ) ) ;
#61806 = VERTEX_POINT ( 'NONE', #20329 ) ;
#61807 = DIRECTION ( 'NONE',  ( 0.000000000000000000, -1.000000000000000000, 0.000000000000000000 ) ) ;
#61808 = CARTESIAN_POINT ( 'NONE',  ( -3.313708498984726969, -23.46874999999999289, 8.000000000000039080 ) ) ;
#61809 = CARTESIAN_POINT ( 'NONE',  ( 5.687763635532137485, 41.86978750169822661, -70.29636349754139246 ) ) ;
#61810 = CARTESIAN_POINT ( 'NONE',  ( -16.96051095573446332, 45.50173602991597477, -6.619600894237387401 ) ) ;
#61811 = CARTESIAN_POINT ( 'NONE',  ( 28.09999999999999787, -3.309499999999999886, 0.000000000000000000 ) ) ;
#61813 = CARTESIAN_POINT ( 'NONE',  ( 10.28624191511840458, -1.200000000000000030E-05, 14.15779740156149025 ) ) ;
#61812 =( GEOMETRIC_REPRESENTATION_CONTEXT ( 3 ) GLOBAL_UNCERTAINTY_ASSIGNED_CONTEXT ( ( #9477 ) ) GLOBAL_UNIT_ASSIGNED_CONTEXT ( ( #50185, #73381, #1617 ) ) REPRESENTATION_CONTEXT ( 'NONE', 'WORKASPACE' ) );
#61814 = ORIENTED_EDGE ( 'NONE', *, *, #103526, .T. ) ;
#61815 = CARTESIAN_POINT ( 'NONE',  ( 92.64087237572343270, -60.00000000000000000, -9.951826560658968646 ) ) ;
#61817 = CARTESIAN_POINT ( 'NONE',  ( 25.00472155834508925, -42.95520012000800847, 32.33701874286857247 ) ) ;
#61816 = CARTESIAN_POINT ( 'NONE',  ( -62.45630560627096628, -29.99999999999992184, 99.43668923270982418 ) ) ;
#61818 = CARTESIAN_POINT ( 'NONE',  ( 50.10796912846466000, 53.37899725327127953, 25.05398456423234776 ) ) ;
#61819 = ORIENTED_EDGE ( 'NONE', *, *, #49109, .F. ) ;
#61820 = CARTESIAN_POINT ( 'NONE',  ( -39.00554263752280093, -36.06017026425686822, 37.16608606929241887 ) ) ;
#61821 = ORIENTED_EDGE ( 'NONE', *, *, #60626, .T. ) ;
#61822 = CARTESIAN_POINT ( 'NONE',  ( 34.63382419943125257, 462.0010168197948701, 4.189557279629578801 ) ) ;
#61823 = CARTESIAN_POINT ( 'NONE',  ( 6.677362058809300116, -11.98847278904868396, 9.465251842568012108 ) ) ;
#61824 = CARTESIAN_POINT ( 'NONE',  ( -0.1687275065231993998, 52.17923068443690937, -7.749999999999973355 ) ) ;
#61825 = CARTESIAN_POINT ( 'NONE',  ( 7.801339272325197527, -61.41268528040300367, -1.788609912539670166 ) ) ;
#61826 = PRESENTATION_STYLE_ASSIGNMENT (( #28954 ) ) ;
#61827 = ORIENTED_EDGE ( 'NONE', *, *, #86669, .T. ) ;
#61828 = CARTESIAN_POINT ( 'NONE',  ( -75.06642738654252867, -38.33958646326993147, 170.1756141881156168 ) ) ;
#61829 = AXIS2_PLACEMENT_3D ( 'NONE', #104297, #63871, #5612 ) ;
#61830 = CARTESIAN_POINT ( 'NONE',  ( 98.39163834582095092, -29.99999999999995737, 190.0198514090498634 ) ) ;
#61831 = CARTESIAN_POINT ( 'NONE',  ( 42.00322489364931755, 39.55629383142768773, -50.29209334003609655 ) ) ;
#61832 = CARTESIAN_POINT ( 'NONE',  ( -5.649205854336970312, -81.54645467188484531, -2.034449005107560549 ) ) ;
#61833 = CARTESIAN_POINT ( 'NONE',  ( 80.72524915699251835, -30.00000000000000711, -12.58409207385285988 ) ) ;
#61834 = DIRECTION ( 'NONE',  ( -0.000000000000000000, -1.000000000000000000, -0.000000000000000000 ) ) ;
#61835 = ORIENTED_EDGE ( 'NONE', *, *, #93699, .F. ) ;
#61836 = ADVANCED_FACE ( 'NONE', ( #53174 ), #102782, .F. ) ;
#61837 = ORIENTED_EDGE ( 'NONE', *, *, #91279, .F. ) ;
#61838 = ORIENTED_EDGE ( 'NONE', *, *, #81115, .T. ) ;
#61839 = LINE ( 'NONE', #37581, #3851 ) ;
#61840 = DIRECTION ( 'NONE',  ( 1.096832036894112098E-16, -0.000000000000000000, 1.000000000000000000 ) ) ;
#61841 = CARTESIAN_POINT ( 'NONE',  ( 31.84999999999999787, -3.309499999999999886, 0.000000000000000000 ) ) ;
#61842 = CARTESIAN_POINT ( 'NONE',  ( -7.986452802927061612, -88.97309757691890297, 0.5332468218996310183 ) ) ;
#61844 = EDGE_CURVE ( 'NONE', #14520, #27731, #48932, .T. ) ;
#61843 = CARTESIAN_POINT ( 'NONE',  ( 39.08667504540952109, 49.99999999999999289, -56.76470588249685534 ) ) ;
#61845 = ORIENTED_EDGE ( 'NONE', *, *, #36312, .F. ) ;
#61846 = CARTESIAN_POINT ( 'NONE',  ( -9.999999999999996447, 48.00000000000000000, -83.69100306252323662 ) ) ;
#61847 = ORIENTED_EDGE ( 'NONE', *, *, #85230, .T. ) ;
#61848 = CARTESIAN_POINT ( 'NONE',  ( -5.981118819178459667, -61.02816543819941586, 0.5452870891823673460 ) ) ;
#61849 = CARTESIAN_POINT ( 'NONE',  ( 55.26095113931063452, 6.856755485862130937E-15, 0.000000000000000000 ) ) ;
#61850 = DIRECTION ( 'NONE',  ( -1.000000000000000000, -1.224606353822377258E-16, -0.000000000000000000 ) ) ;
#61851 = CARTESIAN_POINT ( 'NONE',  ( 23.85675658565387991, 303.8681536343033258, 10.15842353693015809 ) ) ;
#61852 = STYLED_ITEM ( 'NONE', ( #53372 ), #39853 ) ;
#61853 = EDGE_CURVE ( 'NONE', #37488, #73687, #48931, .T. ) ;
#61854 = DIRECTION ( 'NONE',  ( 0.000000000000000000, -1.000000000000000000, 0.000000000000000000 ) ) ;
#61855 = CARTESIAN_POINT ( 'NONE',  ( 62.71390290029641079, -60.33891165955828484, 90.28853715842232930 ) ) ;
#61856 = ORIENTED_EDGE ( 'NONE', *, *, #53240, .T. ) ;
#61857 = CARTESIAN_POINT ( 'NONE',  ( 0.000000000000000000, -8.673617379884035472E-16, -17.01589776168603407 ) ) ;
#61858 = CARTESIAN_POINT ( 'NONE',  ( -54.69861804585598719, -36.50581144510210407, -35.32386462939300031 ) ) ;
#61859 = LINE ( 'NONE', #5197, #64413 ) ;
#61860 = CARTESIAN_POINT ( 'NONE',  ( -9.804047713996713043, 51.27631422876505951, 2.925016539151283013 ) ) ;
#61861 = EDGE_CURVE ( 'NONE', #21060, #89753, #57553, .T. ) ;
#61862 = B_SPLINE_CURVE_WITH_KNOTS ( 'NONE', 3,
 ( #67589, #42227, #84295, #75658 ),
 .UNSPECIFIED., .F., .F.,
 ( 4, 4 ),
 ( 0.000000000000000000, 1.000000000000000000 ),
 .UNSPECIFIED. ) ;
#61863 = EDGE_LOOP ( 'NONE', ( #91744, #83642, #86075, #42381 ) ) ;
#61864 = CARTESIAN_POINT ( 'NONE',  ( 24.34999999999999787, 1.533819458162526451E-15, 0.000000000000000000 ) ) ;
#61865 = CARTESIAN_POINT ( 'NONE',  ( 0.000000000000000000, 1.502314598737161398E-15, 6.499999999999999112 ) ) ;
#61866 = CARTESIAN_POINT ( 'NONE',  ( 0.9999999999999961142, -4.000000000000000000, 27.00000000000000000 ) ) ;
#61867 = VECTOR ( 'NONE', #24208, 1000.000000000000000 ) ;
#61868 = CIRCLE ( 'NONE', #20555, 4.000000000000007105 ) ;
#61869 = CARTESIAN_POINT ( 'NONE',  ( 18.00000000000000355, 12.99999999999999467, 9.500000000000000000 ) ) ;
#61870 = AXIS2_PLACEMENT_3D ( 'NONE', #43948, #19721, #61206 ) ;
#61871 = DIRECTION ( 'NONE',  ( 0.7071067811865456854, 0.000000000000000000, -0.7071067811865493491 ) ) ;
#61872 = CARTESIAN_POINT ( 'NONE',  ( 4.444974277458376477, 4.939246403833576160, -5.720331885005371930 ) ) ;
#61873 = CARTESIAN_POINT ( 'NONE',  ( 84.90064340091288386, -57.46992232430159930, 192.0070107122053003 ) ) ;
#61874 = PRESENTATION_LAYER_ASSIGNMENT (  '', '', ( #96353 ) ) ;
#61875 = DIRECTION ( 'NONE',  ( 0.000000000000000000, 1.000000000000000000, 0.000000000000000000 ) ) ;
#61876 = CONICAL_SURFACE ( 'NONE', #80777, 4.000000000000001776, 0.9599310885968774798 ) ;
#61877 = CARTESIAN_POINT ( 'NONE',  ( -9.692620405224255720, 8.443756516856183225, 0.000000000000000000 ) ) ;
#61878 = ORIENTED_EDGE ( 'NONE', *, *, #57291, .F. ) ;
#61879 = CARTESIAN_POINT ( 'NONE',  ( -14.43785825815714752, -17.02022128621486274, -34.43806907934169459 ) ) ;
#61880 = DIRECTION ( 'NONE',  ( -0.5735764363510494901, -0.8191520442889894671, 0.000000000000000000 ) ) ;
#61881 = CARTESIAN_POINT ( 'NONE',  ( 16.75187969033515145, 34.99134772383131775, -21.80698433968624528 ) ) ;
#61882 = DIRECTION ( 'NONE',  ( 0.000000000000000000, 1.000000000000000000, 0.000000000000000000 ) ) ;
#61883 =( BOUNDED_SURFACE ( )  B_SPLINE_SURFACE ( 3, 2, ( 
 ( #17634, #50494, #10579 ),
 ( #67765, #34900, #86101 ),
 ( #100652, #53702, #94172 ),
 ( #26812, #43494, #20869 ),
 ( #20337, #59686, #51570 ),
 ( #68303, #76371, #101722 ) ),
 .UNSPECIFIED., .F., .F., .F. ) 
 B_SPLINE_SURFACE_WITH_KNOTS ( ( 4, 2, 4 ),
 ( 3, 3 ),
 ( 0.003199762745115999809, 0.007302762474435751071, 0.01140576220375550190 ),
 ( 0.000000000000000000, 1.000000000000000000 ),
 .UNSPECIFIED. ) 
 GEOMETRIC_REPRESENTATION_ITEM ( )  RATIONAL_B_SPLINE_SURFACE ( (
 ( 1.000000000000000000, 0.8047731410850422762, 1.000000000000000000),
 ( 1.000000000000000000, 0.8125552299159720659, 1.000000000000000000),
 ( 1.000000000000000000, 0.8191520442885290576, 1.000000000000000000),
 ( 1.000000000000000000, 0.8191520442894507648, 1.000000000000000000),
 ( 1.000000000000000000, 0.8125552299152799529, 1.000000000000000000),
 ( 1.000000000000000000, 0.8047731410850428313, 1.000000000000000000) ) ) 
 REPRESENTATION_ITEM ( '' )  SURFACE ( )  );
#61884 = CARTESIAN_POINT ( 'NONE',  ( -100.9715102229217365, -30.00000000000000711, 178.1047487978037509 ) ) ;
#61885 = PRESENTATION_LAYER_ASSIGNMENT (  '', '', ( #37730 ) ) ;
#61886 = CARTESIAN_POINT ( 'NONE',  ( -5.000000000000000888, 6.123233995736767268E-16, -25.03750572909317285 ) ) ;
#61887 = CARTESIAN_POINT ( 'NONE',  ( 32.18356949007781509, -57.68957018251984437, 46.69086977585512699 ) ) ;
#61888 = CIRCLE ( 'NONE', #70491, 5.000000000000011546 ) ;
#61889 = CARTESIAN_POINT ( 'NONE',  ( 13.53904809976053691, 7.592565540055561613, -8.416763124031669818 ) ) ;
#61890 = FILL_AREA_STYLE_COLOUR ( '', #60999 ) ;
#61891 = CARTESIAN_POINT ( 'NONE',  ( -18.00109036083110681, 50.00000000000000711, 61.88627459926749452 ) ) ;
#61892 =( NAMED_UNIT ( * ) PLANE_ANGLE_UNIT ( ) SI_UNIT ( $, .RADIAN. ) );
#61893 = COLOUR_RGB ( '', 0.09019608, 0.27058824, 0.51372549) ;
#61894 = CARTESIAN_POINT ( 'NONE',  ( 11.76221606908526240, -16.54900257170227107, -34.66273767363278324 ) ) ;
#61895 = AXIS2_PLACEMENT_3D ( 'NONE', #100458, #18506, #85345 ) ;
#61896 =( NAMED_UNIT ( * ) SI_UNIT ( $, .STERADIAN. ) SOLID_ANGLE_UNIT ( ) );
#61897 =( LENGTH_UNIT ( ) NAMED_UNIT ( * ) SI_UNIT ( .MILLI., .METRE. ) );
#61898 = ORIENTED_EDGE ( 'NONE', *, *, #83668, .F. ) ;
#61899 = CARTESIAN_POINT ( 'NONE',  ( 40.83852310120747120, 485.7816305618702586, -4.779469532616784200 ) ) ;
#61900 = CARTESIAN_POINT ( 'NONE',  ( -9.220915120640581719, 106.0445488643208165, -3.870126578504840431 ) ) ;
#61901 = CARTESIAN_POINT ( 'NONE',  ( -21.23094043253502150, -35.99698555973125735, 30.53890210230313329 ) ) ;
#61903 = DIRECTION ( 'NONE',  ( 0.000000000000000000, 0.000000000000000000, 1.000000000000000000 ) ) ;
#61902 = CARTESIAN_POINT ( 'NONE',  ( -86.13135164208073036, -59.99999999999992895, -13.61769622756565035 ) ) ;
#61904 = EDGE_CURVE ( 'NONE', #65856, #85904, #9015, .T. ) ;
#61905 = ORIENTED_EDGE ( 'NONE', *, *, #60748, .T. ) ;
#61906 = EDGE_CURVE ( 'NONE', #33490, #2579, #102390, .T. ) ;
#61907 = FILL_AREA_STYLE ('',( #95847 ) ) ;
#61908 = ORIENTED_EDGE ( 'NONE', *, *, #11015, .F. ) ;
#61909 = CARTESIAN_POINT ( 'NONE',  ( 42.89416850988997254, 486.3091028892278587, 6.394136786127195826 ) ) ;
#61910 = EDGE_CURVE ( 'NONE', #59854, #73607, #57917, .T. ) ;
#61911 = EDGE_CURVE ( 'NONE', #80767, #12476, #101682, .T. ) ;
#61912 = CARTESIAN_POINT ( 'NONE',  ( 16.03050524006189548, 4.255071776846901521, -2.702720838580708662 ) ) ;
#61913 = FACE_OUTER_BOUND ( 'NONE', #93070, .T. ) ;
#61914 = ORIENTED_EDGE ( 'NONE', *, *, #53034, .T. ) ;
#61915 = CYLINDRICAL_SURFACE ( 'NONE', #98011, 4.000000000000000000 ) ;
#61916 = PRESENTATION_STYLE_ASSIGNMENT (( #102345 ) ) ;
#61917 = AXIS2_PLACEMENT_3D ( 'NONE', #66916, #32970, #15688 ) ;
#61918 = CARTESIAN_POINT ( 'NONE',  ( 101.5338889927411827, -45.28223279133771229, 190.3009016725240770 ) ) ;
#61919 = CIRCLE ( 'NONE', #99764, 5.000000000000002665 ) ;
#61921 = DIRECTION ( 'NONE',  ( 0.000000000000000000, 0.7310552682428690385, 0.6823182503600110360 ) ) ;
#61920 = SURFACE_STYLE_USAGE ( .BOTH. , #95324 ) ;
#61922 = ORIENTED_EDGE ( 'NONE', *, *, #70359, .F. ) ;
#61923 = EDGE_CURVE ( 'NONE', #85977, #69148, #82381, .T. ) ;
#61924 = ORIENTED_EDGE ( 'NONE', *, *, #6030, .F. ) ;
#61925 = EDGE_LOOP ( 'NONE', ( #83107, #54595, #52595, #101616 ) ) ;
#61926 = CARTESIAN_POINT ( 'NONE',  ( 26.90838114744199672, 308.9771128992503577, 11.14144682951946308 ) ) ;
#61927 = DIRECTION ( 'NONE',  ( 0.000000000000000000, -1.000000000000000000, 0.000000000000000000 ) ) ;
#61928 =( LENGTH_UNIT ( ) NAMED_UNIT ( * ) SI_UNIT ( .MILLI., .METRE. ) );
#61929 = ORIENTED_EDGE ( 'NONE', *, *, #103217, .T. ) ;
#61930 = SURFACE_STYLE_FILL_AREA ( #55896 ) ;
#61931 = CARTESIAN_POINT ( 'NONE',  ( -6.996268133785214616, 41.79455485337270204, -69.25931873534777594 ) ) ;
#61932 = VECTOR ( 'NONE', #13192, 1000.000000000000000 ) ;
#61933 = CARTESIAN_POINT ( 'NONE',  ( -97.06981497546472326, -60.00000000003904432, 46.90335524957238533 ) ) ;
#61934 = FACE_BOUND ( 'NONE', #55767, .T. ) ;
#61935 = CARTESIAN_POINT ( 'NONE',  ( 11.36546102070421149, -60.00000000000001421, 39.66528621601015914 ) ) ;
#61936 = CARTESIAN_POINT ( 'NONE',  ( -15.35350627405965085, -5.000000000000000000, -5.840883397579456293 ) ) ;
#61937 = CARTESIAN_POINT ( 'NONE',  ( -5.660418747924874872, 41.80469015519229714, -58.87109497794652668 ) ) ;
#61939 = CARTESIAN_POINT ( 'NONE',  ( 12.48886139173590593, -46.43473308940932753, 31.68645849438150819 ) ) ;
#61938 = CARTESIAN_POINT ( 'NONE',  ( -90.94649322911389788, -14.21045842199428222, 57.96573475225447680 ) ) ;
#61940 = DIRECTION ( 'NONE',  ( -1.000000000000000000, -1.224606353822377258E-16, -0.000000000000000000 ) ) ;
#61941 = CARTESIAN_POINT ( 'NONE',  ( -48.29725705757057597, -46.44452024506328058, 50.22719862630319909 ) ) ;
#61942 = CARTESIAN_POINT ( 'NONE',  ( 1.408267258621023643, -70.62266515023254954, 13.06855514134478469 ) ) ;
#61943 = ORIENTED_EDGE ( 'NONE', *, *, #34908, .T. ) ;
#61944 = DIRECTION ( 'NONE',  ( 0.000000000000000000, -1.000000000000000000, 0.000000000000000000 ) ) ;
#61945 = CARTESIAN_POINT ( 'NONE',  ( 17.08493112194837238, 36.32471929476455585, 24.27338705487281700 ) ) ;
#61946 = CARTESIAN_POINT ( 'NONE',  ( 6.222803527742077456, 4.089662073612390536, 6.499999999999997335 ) ) ;
#61947 = ORIENTED_EDGE ( 'NONE', *, *, #32719, .F. ) ;
#61948 = CARTESIAN_POINT ( 'NONE',  ( -5.330204762053584844, -8.150230459544712147, 13.71357708370459072 ) ) ;
#61949 = EDGE_LOOP ( 'NONE', ( #44143, #66306, #2507, #86203, #105489, #11075 ) ) ;
#61950 = CARTESIAN_POINT ( 'NONE',  ( 89.93526870310212473, -30.00000000001337241, 29.02783687399049128 ) ) ;
#61951 = CARTESIAN_POINT ( 'NONE',  ( 4.284822031654949015, -48.90716638558772900, 104.4267991316944943 ) ) ;
#61952 = CARTESIAN_POINT ( 'NONE',  ( 6.676660777536701730, 41.76849096538412454, -59.12256610131672119 ) ) ;
#61953 = CARTESIAN_POINT ( 'NONE',  ( 59.23741894013591036, 42.00000000000000711, 7.754160006506985781 ) ) ;
#61954 = CARTESIAN_POINT ( 'NONE',  ( 100.6243693333776434, -30.00000000000000355, 160.8148924688006218 ) ) ;
#61955 = B_SPLINE_SURFACE_WITH_KNOTS ( 'NONE', 1, 3, ( 
 ( #25019, #57874, #24504, #16913, #82154, #89205, #90799, #31525, #81605, #57338, #73523, #96771, #105385, #8267, #65457, #8801, #6678, #90260, #56815, #39606, #105897, #48718, #80558, #64925, #32047, #64406, #41180, #15305 ),
 ( #97809, #98350, #23975, #71953, #89740, #97279, #147, #104858, #40116, #22901, #23431, #15835, #55738, #7732, #88672, #14762, #56268, #48191, #81094, #72991, #19072, #52440, #68102, #41709, #42765, #101002, #92907, #35785 ) ),
 .UNSPECIFIED., .F., .F., .F.,
 ( 2, 2 ),
 ( 4, 2, 2, 2, 2, 2, 2, 2, 2, 2, 2, 2, 2, 4 ),
 ( 0.000000000000000000, 1.000000000000000000 ),
 ( 0.08901491201581737678, 0.1032490540155679704, 0.1174831960153185778, 0.1317173380150691853, 0.1459514800148197788, 0.1744197640143299588, 0.2028880480138401388, 0.2598246160128514504, 0.3167611840118632616, 0.4306343200098861623, 0.5445074560079088410, 0.6583805920059359051, 0.7722537280039543095, 1.000000000000000000 ),
 .UNSPECIFIED. ) ;
#61956 = CARTESIAN_POINT ( 'NONE',  ( -0.6416578798349835688, 36.36110222310433215, 29.57590615574903836 ) ) ;
#61957 = VERTEX_POINT ( 'NONE', #2875 ) ;
#61958 = EDGE_CURVE ( 'NONE', #105946, #54290, #14508, .T. ) ;
#61959 = AXIS2_PLACEMENT_3D ( 'NONE', #101372, #18348, #85183 ) ;
#61960 = VERTEX_POINT ( 'NONE', #18570 ) ;
#61961 = ORIENTED_EDGE ( 'NONE', *, *, #95841, .T. ) ;
#61962 = CARTESIAN_POINT ( 'NONE',  ( 54.78051204086806791, -29.09201784496401544, 55.71616249050997993 ) ) ;
#61963 = CARTESIAN_POINT ( 'NONE',  ( -43.91156819296970326, 435.5051061888428308, 9.836736652448470508 ) ) ;
#61964 = DIRECTION ( 'NONE',  ( 0.000000000000000000, -1.000000000000000000, 0.000000000000000000 ) ) ;
#61965 = ADVANCED_FACE ( 'NONE', ( #19661 ), #85481, .T. ) ;
#61966 = EDGE_CURVE ( 'NONE', #99028, #102372, #7581, .T. ) ;
#61967 = VERTEX_POINT ( 'NONE', #58892 ) ;
#61968 = CARTESIAN_POINT ( 'NONE',  ( -16.01236936003244438, 3.722446712627851984, 0.6596918664871591620 ) ) ;
#61969 = CIRCLE ( 'NONE', #18866, 7.000000000000000000 ) ;
#61970 = ORIENTED_EDGE ( 'NONE', *, *, #36163, .F. ) ;
#61971 = FACE_OUTER_BOUND ( 'NONE', #93199, .T. ) ;
#61972 = CARTESIAN_POINT ( 'NONE',  ( 94.04204770716727069, -38.49239426584006907, 201.1939902864932037 ) ) ;
#61973 = CARTESIAN_POINT ( 'NONE',  ( 11.01232928683251977, 16.91647149312766274, 9.208423644124117402 ) ) ;
#61974 = CARTESIAN_POINT ( 'NONE',  ( 86.12722738054240779, -60.13654648131097247, 11.25971878457827913 ) ) ;
#61975 = LINE ( 'NONE', #76658, #27060 ) ;
#61976 = CARTESIAN_POINT ( 'NONE',  ( 0.7145311798163208605, 4.618802153517005848, 7.999999999999996447 ) ) ;
#61977 = CARTESIAN_POINT ( 'NONE',  ( -43.54152071279120406, 464.9591243512669507, 12.86066780445021962 ) ) ;
#61978 = CIRCLE ( 'NONE', #63655, 3.309500000000007880 ) ;
#61979 = LINE ( 'NONE', #104521, #74022 ) ;
#61980 = CARTESIAN_POINT ( 'NONE',  ( -39.69617136735454466, 460.2157148251831700, 2.207451131567688574 ) ) ;
#61981 = CARTESIAN_POINT ( 'NONE',  ( 3.454253436624935336, -0.8414180287960453253, 103.7259032015043232 ) ) ;
#61982 = ORIENTED_EDGE ( 'NONE', *, *, #8406, .T. ) ;
#61983 = CARTESIAN_POINT ( 'NONE',  ( 5.000000000000000000, 6.123233995736766282E-16, -0.02540000000000007530 ) ) ;
#61984 = EDGE_CURVE ( 'NONE', #4725, #2640, #79972, .T. ) ;
#61985 = CARTESIAN_POINT ( 'NONE',  ( 15.97269242673970702, 37.21081289561244176, -22.07591361862218449 ) ) ;
#61986 = CARTESIAN_POINT ( 'NONE',  ( -25.89112870477232065, 37.21026264049879018, 8.497328228240501602 ) ) ;
#61987 = ORIENTED_EDGE ( 'NONE', *, *, #99234, .F. ) ;
#61988 = DIRECTION ( 'NONE',  ( 0.000000000000000000, 0.000000000000000000, 1.000000000000000000 ) ) ;
#61989 = CARTESIAN_POINT ( 'NONE',  ( -36.82997274950742650, 306.6632309731772352, 4.707311215296837048 ) ) ;
#61990 = DIRECTION ( 'NONE',  ( -1.000000000000000000, -1.224606353822377258E-16, -0.000000000000000000 ) ) ;
#61991 = CARTESIAN_POINT ( 'NONE',  ( 42.40769230769231513, 1.411358822780289120E-15, 0.000000000000000000 ) ) ;
#61992 = CARTESIAN_POINT ( 'NONE',  ( -8.000000000000000000, -20.84374999999999645, -3.313708498984762496 ) ) ;
#61993 = CARTESIAN_POINT ( 'NONE',  ( 38.43315959910751189, -27.95011100668220649, 45.39859000375419384 ) ) ;
#61994 = TOROIDAL_SURFACE ( 'NONE', #72272, 7.999999999999998224, 2.000000000000000000 ) ;
#61995 = EDGE_CURVE ( 'NONE', #70854, #32906, #93773, .T. ) ;
#61996 = DIRECTION ( 'NONE',  ( 0.000000000000000000, 0.000000000000000000, -1.000000000000000000 ) ) ;
#61997 = ORIENTED_EDGE ( 'NONE', *, *, #41133, .F. ) ;
#61998 = CARTESIAN_POINT ( 'NONE',  ( 84.10550226404134833, -46.55871237661660444, 184.9821644560045399 ) ) ;
#61999 = ADVANCED_FACE ( 'NONE', ( #106340 ), #91262, .T. ) ;
#62000 = CARTESIAN_POINT ( 'NONE',  ( -38.76877242246048638, 27.37289375180844431, 11.85340545765227382 ) ) ;
#62001 = FACE_OUTER_BOUND ( 'NONE', #31530, .T. ) ;
#62002 = ORIENTED_EDGE ( 'NONE', *, *, #24537, .F. ) ;
#62003 = CARTESIAN_POINT ( 'NONE',  ( -96.00081068786835203, -45.26563211955492960, 106.3251220198503120 ) ) ;
#62004 = DIRECTION ( 'NONE',  ( -1.000000000000000000, -1.224606353822377258E-16, -0.000000000000000000 ) ) ;
#62005 = CARTESIAN_POINT ( 'NONE',  ( -10.50942704840529629, -5.000000000000002665, -93.01494055617339995 ) ) ;
#62006 = CARTESIAN_POINT ( 'NONE',  ( 69.18888888888888289, 6.915964383211875250E-15, 0.000000000000000000 ) ) ;
#62007 = COLOUR_RGB ( '', 0.66274510, 0.83137255, 0.94901961) ;
#62008 = CARTESIAN_POINT ( 'NONE',  ( 7.878783547692759903, -19.41176153434803098, 35.22918882278415964 ) ) ;
#62009 = CARTESIAN_POINT ( 'NONE',  ( 2.678351059745755602, -0.3580534592355345547, 103.0656783881315306 ) ) ;
#62010 = CARTESIAN_POINT ( 'NONE',  ( 39.78494456460381912, -26.23335630279444786, 35.82506221462753615 ) ) ;
#62013 = CARTESIAN_POINT ( 'NONE',  ( -10.76371368059873390, 15.73337048095761403, 9.625036908677250480 ) ) ;
#62012 = CONICAL_SURFACE ( 'NONE', #12002, 34.51297463494397988, 1.221730476396026610 ) ;
#62011 = CARTESIAN_POINT ( 'NONE',  ( -2.500000000000002220, 0.000000000000000000, 0.000000000000000000 ) ) ;
#62014 = CARTESIAN_POINT ( 'NONE',  ( 9.148737761749414332, 294.6669993733608521, -4.042064116745931024 ) ) ;
#62015 = CARTESIAN_POINT ( 'NONE',  ( -16.02654702170687528, 43.95888759761753306, -4.317547509937734951 ) ) ;
#62016 = CARTESIAN_POINT ( 'NONE',  ( 43.63596364813231787, 421.7880994604767011, 15.67549955746410184 ) ) ;
#62017 = CARTESIAN_POINT ( 'NONE',  ( 31.14131030317610538, -5.000000000000000000, 6.123233995736768255E-16 ) ) ;
#62018 = CARTESIAN_POINT ( 'NONE',  ( 6.585468679846623985, 7.640532685286893333, 0.2337908078075577600 ) ) ;
#62019 = AXIS2_PLACEMENT_3D ( 'NONE', #61150, #332, #58072 ) ;
#62020 = ORIENTED_EDGE ( 'NONE', *, *, #27433, .F. ) ;
#62021 = CARTESIAN_POINT ( 'NONE',  ( 16.36650669486618881, 1.474610560812782335E-15, 0.000000000000000000 ) ) ;
#62022 = EDGE_LOOP ( 'NONE', ( #55914, #87815, #69043, #34765 ) ) ;
#62023 = CARTESIAN_POINT ( 'NONE',  ( -11.60195201528633291, -1.681760983426669576, 20.57261808643857037 ) ) ;
#62024 =( NAMED_UNIT ( * ) SI_UNIT ( $, .STERADIAN. ) SOLID_ANGLE_UNIT ( ) );
#62025 = DIRECTION ( 'NONE',  ( 1.000000000000000000, 1.224606353822377258E-16, 0.000000000000000000 ) ) ;
#62026 = CONICAL_SURFACE ( 'NONE', #48199, 7.500000000000000888, 0.8594454914424817238 ) ;
#62028 = CARTESIAN_POINT ( 'NONE',  ( -1.543626744577732079, -21.77031562861895608, -30.51802372251457385 ) ) ;
#62027 = CARTESIAN_POINT ( 'NONE',  ( 9.536842176398169002, 252.6423536988397416, 3.014135744008177742 ) ) ;
#62029 = ADVANCED_FACE ( 'NONE', ( #64842 ), #23178, .T. ) ;
#62030 = VERTEX_POINT ( 'NONE', #81522 ) ;
#62031 = AXIS2_PLACEMENT_3D ( 'NONE', #19180, #19708, #12608 ) ;
#62032 = DIRECTION ( 'NONE',  ( -1.000000000000000000, -1.224606353822377258E-16, -0.000000000000000000 ) ) ;
#62033 = CARTESIAN_POINT ( 'NONE',  ( -41.44325370401499953, 477.1517044324976951, -1.084963556091905534 ) ) ;
#62034 = EDGE_LOOP ( 'NONE', ( #101284, #72419, #89065, #44712 ) ) ;
#62035 = ADVANCED_FACE ( 'NONE', ( #33036 ), #105759, .T. ) ;
#62036 = ADVANCED_FACE ( 'NONE', ( #66979 ), #50757, .T. ) ;
#62037 = CARTESIAN_POINT ( 'NONE',  ( 6.289692432696983637, 6.589071317541204564, 2.245373559999253033 ) ) ;
#62038 = AXIS2_PLACEMENT_3D ( 'NONE', #79039, #55275, #48244 ) ;
#62039 = DIRECTION ( 'NONE',  ( -0.000000000000000000, -1.000000000000000000, -0.000000000000000000 ) ) ;
#62040 = CARTESIAN_POINT ( 'NONE',  ( -91.98068305807049683, -59.99999999999997868, 6.624129181415079337 ) ) ;
#62041 = EDGE_LOOP ( 'NONE', ( #34516, #77016, #93695, #84919 ) ) ;
#62042 = CARTESIAN_POINT ( 'NONE',  ( 14.34999999999999787, 1.533819458162526451E-15, 0.000000000000000000 ) ) ;
#62043 = CARTESIAN_POINT ( 'NONE',  ( -1.469576158976823947E-15, -11.37499999999999289, 8.000000000000000000 ) ) ;
#62044 = DIRECTION ( 'NONE',  ( -0.000000000000000000, -1.000000000000000000, -0.000000000000000000 ) ) ;
#62045 = CARTESIAN_POINT ( 'NONE',  ( -9.221346651730838673, 28.95165979931662292, -3.869102247876034184 ) ) ;
#62047 = CARTESIAN_POINT ( 'NONE',  ( 6.400000000000000355, -4.618802153517009401, -8.000000000000001776 ) ) ;
#62046 = CARTESIAN_POINT ( 'NONE',  ( 44.11327388758692081, 464.4313852428372797, 9.822198357557351045 ) ) ;
#62048 = EDGE_CURVE ( 'NONE', #101426, #98362, #26601, .T. ) ;
#62049 = CIRCLE ( 'NONE', #36196, 5.000000000000000000 ) ;
#62050 = CARTESIAN_POINT ( 'NONE',  ( -81.95665186865053897, -46.45865666940190408, 171.2074146399188237 ) ) ;
#62051 = ORIENTED_EDGE ( 'NONE', *, *, #84869, .F. ) ;
#62052 = CARTESIAN_POINT ( 'NONE',  ( -10.38447319517632295, -0.000000000000000000, -13.52495681779584302 ) ) ;
#62053 = ADVANCED_FACE ( 'NONE', ( #32503 ), #57793, .F. ) ;
#62054 = ORIENTED_EDGE ( 'NONE', *, *, #84517, .F. ) ;
#62055 = EDGE_CURVE ( 'NONE', #51964, #26612, #675, .T. ) ;
#62056 = ORIENTED_EDGE ( 'NONE', *, *, #95539, .F. ) ;
#62057 = CARTESIAN_POINT ( 'NONE',  ( 7.012902693339095883, -4.999999999998556710, 16.13291991228437894 ) ) ;
#62058 = CARTESIAN_POINT ( 'NONE',  ( -4.999999999999922728, -12.25926108426836514, 9.485372419963017165 ) ) ;
#62059 = ORIENTED_EDGE ( 'NONE', *, *, #58806, .F. ) ;
#62060 = CARTESIAN_POINT ( 'NONE',  ( -4.088397730506703845E-15, 46.03420836107012093, 33.38430095398285147 ) ) ;
#62061 = DIRECTION ( 'NONE',  ( -1.000000000000000000, -0.000000000000000000, -0.000000000000000000 ) ) ;
#62062 = CARTESIAN_POINT ( 'NONE',  ( -99.13865059541491576, -57.67127950436278638, 63.61738387431689290 ) ) ;
#62063 = CARTESIAN_POINT ( 'NONE',  ( 7.414580834929598296, -12.64656280281483092, 3.010264818013835608 ) ) ;
#62064 = FACE_OUTER_BOUND ( 'NONE', #56467, .T. ) ;
#62065 = CARTESIAN_POINT ( 'NONE',  ( 22.33349330513380693, 1.593028355512270962E-15, 0.000000000000000000 ) ) ;
#62066 = SURFACE_STYLE_USAGE ( .BOTH. , #87386 ) ;
#62067 = FILL_AREA_STYLE ('',( #12404 ) ) ;
#62068 = CIRCLE ( 'NONE', #15526, 9.999999999999994671 ) ;
#62069 = CARTESIAN_POINT ( 'NONE',  ( 60.74900604410193239, -14.21045842199440301, -29.98664384297035213 ) ) ;
#62070 = CARTESIAN_POINT ( 'NONE',  ( -59.93215762506982713, -30.00000000000009592, 91.51900601851320971 ) ) ;
#62071 = CARTESIAN_POINT ( 'NONE',  ( -56.07191290525906879, -49.91320329917822107, 67.05920270483053969 ) ) ;
#62072 = EDGE_LOOP ( 'NONE', ( #69396, #31941 ) ) ;
#62073 = FILL_AREA_STYLE_COLOUR ( '', #48717 ) ;
#62074 = ORIENTED_EDGE ( 'NONE', *, *, #36837, .T. ) ;
#62075 = CARTESIAN_POINT ( 'NONE',  ( -101.2319481900598106, -52.72902908576037362, 193.1221610425403412 ) ) ;
#62076 = CARTESIAN_POINT ( 'NONE',  ( -30.25727950662331978, 17.21737621059155643, -39.73669541984511966 ) ) ;
#62077 = ORIENTED_EDGE ( 'NONE', *, *, #59096, .T. ) ;
#62078 = CARTESIAN_POINT ( 'NONE',  ( 18.99451835574970815, 49.48953773287491487, 61.92607718230669178 ) ) ;
#62079 = CYLINDRICAL_SURFACE ( 'NONE', #100143, 8.000000000000000000 ) ;
#62080 = CARTESIAN_POINT ( 'NONE',  ( 7.188101187500001821, -14.93750000204838457, -2.977408999572650483 ) ) ;
#62081 = CARTESIAN_POINT ( 'NONE',  ( -3.631499270081283814, -68.18321798808027268, 13.10122733214759982 ) ) ;
#62082 = DIRECTION ( 'NONE',  ( 0.000000000000000000, 0.000000000000000000, 1.000000000000000000 ) ) ;
#62083 = FACE_OUTER_BOUND ( 'NONE', #13746, .T. ) ;
#62084 = CARTESIAN_POINT ( 'NONE',  ( 69.72280996538995623, -30.00000000000000711, 94.43922800780518401 ) ) ;
#62085 = DIRECTION ( 'NONE',  ( -1.000000000000000000, -0.000000000000000000, -0.000000000000000000 ) ) ;
#62086 = DIRECTION ( 'NONE',  ( -1.000000000000000000, -1.224606353822377258E-16, -0.000000000000000000 ) ) ;
#62087 = UNCERTAINTY_MEASURE_WITH_UNIT (LENGTH_MEASURE( 1.000000000000000082E-05 ), #66155, 'distance_accuracy_value', 'NONE');
#62088 = CARTESIAN_POINT ( 'NONE',  ( -29.32136198015045281, -56.86423622103713882, 35.94540326096643668 ) ) ;
#62089 = VECTOR ( 'NONE', #6456, 1000.000000000000000 ) ;
#62090 = VERTEX_POINT ( 'NONE', #40562 ) ;
#62091 = CARTESIAN_POINT ( 'NONE',  ( 47.74913715125470048, -29.14591046249990924, 44.14729050338506511 ) ) ;
#62092 = DIRECTION ( 'NONE',  ( 1.000000000000000000, 0.000000000000000000, 0.000000000000000000 ) ) ;
#62093 = CARTESIAN_POINT ( 'NONE',  ( -6.705159343100833169, 16.46048476709899688, -2.022944797798715388 ) ) ;
#62094 = AXIS2_PLACEMENT_3D ( 'NONE', #98975, #8917, #65037 ) ;
#62095 = ADVANCED_FACE ( 'NONE', ( #41630 ), #73445, .T. ) ;
#62096 = CARTESIAN_POINT ( 'NONE',  ( -87.23646927575083510, -38.58587952222158179, 199.6458570365388141 ) ) ;
#62097 = EDGE_LOOP ( 'NONE', ( #44163, #40470, #96459, #23171, #22855 ) ) ;
#62098 = CARTESIAN_POINT ( 'NONE',  ( 91.43959331831491966, -38.37791452498228040, -4.964256820052830754 ) ) ;
#62099 = FILL_AREA_STYLE_COLOUR ( '', #45530 ) ;
#62100 = CARTESIAN_POINT ( 'NONE',  ( -18.91772294158991130, 48.18297239048385450, 62.18609455207817405 ) ) ;
#62101 = CARTESIAN_POINT ( 'NONE',  ( 34.35000000000000142, 3.309500000000003439, 0.000000000000000000 ) ) ;
#62102 = CARTESIAN_POINT ( 'NONE',  ( 6.309251617458595085, 40.00000000335901973, -71.19739464403906481 ) ) ;
#62103 = CARTESIAN_POINT ( 'NONE',  ( -33.05281441019222655, 434.2935209264010723, 15.73787673445679225 ) ) ;
#62104 = CYLINDRICAL_SURFACE ( 'NONE', #55209, 1.250000000000001110 ) ;
#62105 = CARTESIAN_POINT ( 'NONE',  ( 12.49999999999999822, -4.999999999999999112, -8.595933841506987250 ) ) ;
#62106 = EDGE_CURVE ( 'NONE', #18346, #24961, #19530, .T. ) ;
#62107 = CARTESIAN_POINT ( 'NONE',  ( 111.2609372169454502, -60.00000000000000711, 185.9044869507005160 ) ) ;
#62108 = VECTOR ( 'NONE', #4650, 1000.000000000000000 ) ;
#62109 = CARTESIAN_POINT ( 'NONE',  ( -6.928203230275505220, -65.26526156932587241, 4.000000000000002665 ) ) ;
#62110 = CIRCLE ( 'NONE', #15561, 4.000000000000000888 ) ;
#62111 = ADVANCED_FACE ( 'NONE', ( #77187 ), #64596, .T. ) ;
#62112 = ORIENTED_EDGE ( 'NONE', *, *, #34757, .T. ) ;
#62113 = CARTESIAN_POINT ( 'NONE',  ( 85.59800593614014019, 5.000000000000002665, 6.123233995736756422E-16 ) ) ;
#62114 = CARTESIAN_POINT ( 'NONE',  ( -13.50000000000000178, -5.228219631169437775, -12.46710323223871164 ) ) ;
#62115 = ORIENTED_EDGE ( 'NONE', *, *, #30006, .T. ) ;
#62116 = COLOUR_RGB ( '', 0.08235294, 0.09019608, 0.10196078) ;
#62118 = FACE_OUTER_BOUND ( 'NONE', #22573, .T. ) ;
#62117 = CARTESIAN_POINT ( 'NONE',  ( -108.9786437150107332, -38.35638155208228994, 190.2319024447106699 ) ) ;
#62119 = CARTESIAN_POINT ( 'NONE',  ( 20.00100000000000122, 12.99999999999999289, -4.000000000000000000 ) ) ;
#62120 = CARTESIAN_POINT ( 'NONE',  ( 43.49620567743568245, 471.8615734360752754, 7.936790638082919180 ) ) ;
#62121 = SURFACE_STYLE_USAGE ( .BOTH. , #37855 ) ;
#62122 = CARTESIAN_POINT ( 'NONE',  ( 2.977408999572650927, -14.75000000204838457, -7.188101187500001821 ) ) ;
#62123 = CARTESIAN_POINT ( 'NONE',  ( 0.000000000000000000, -5.000000000000002665, -75.00000000000001421 ) ) ;
#62124 = AXIS2_PLACEMENT_3D ( 'NONE', #55664, #5032, #39532 ) ;
#62125 = CARTESIAN_POINT ( 'NONE',  ( -42.69811214730272297, 434.9611672192513652, 18.34625614733208820 ) ) ;
#62127 = ORIENTED_EDGE ( 'NONE', *, *, #9543, .F. ) ;
#62126 = CARTESIAN_POINT ( 'NONE',  ( 6.683837171061803417, -3.955946848495962787, 6.851900933636989599 ) ) ;
#62128 = CARTESIAN_POINT ( 'NONE',  ( 83.79296793638981455, -35.97364189524810740, 171.8120904271870018 ) ) ;
#62129 = EDGE_CURVE ( 'NONE', #45319, #68633, #55925, .T. ) ;
#62130 = CARTESIAN_POINT ( 'NONE',  ( 3.400000000000000355, 0.000000000000000000, -8.000000000000000000 ) ) ;
#62131 = CARTESIAN_POINT ( 'NONE',  ( 5.698650001973516233, -4.592339236403583769, -6.344532336093709368 ) ) ;
#62132 = ORIENTED_EDGE ( 'NONE', *, *, #72946, .T. ) ;
#62133 = CARTESIAN_POINT ( 'NONE',  ( -23.07924577400106969, 303.3257072796955072, -9.898399575382260451 ) ) ;
#62134 = CARTESIAN_POINT ( 'NONE',  ( -47.36344235967359850, 18.16811379743644395, 14.54383657267810825 ) ) ;
#62135 = CARTESIAN_POINT ( 'NONE',  ( 2.688402820137708371, 5.953403407568484518, -0.01956314070068211619 ) ) ;
#62136 = DIRECTION ( 'NONE',  ( 0.000000000000000000, 0.000000000000000000, -1.000000000000000000 ) ) ;
#62137 = CARTESIAN_POINT ( 'NONE',  ( 14.11571568429345369, 5.211159435664226791, 3.514002131771331250 ) ) ;
#62138 = CARTESIAN_POINT ( 'NONE',  ( -4.250000000000000000, 5.204748896376250699E-16, -7.657127082228716297 ) ) ;
#62139 = VERTEX_POINT ( 'NONE', #67510 ) ;
#62140 =( LENGTH_UNIT ( ) NAMED_UNIT ( * ) SI_UNIT ( .MILLI., .METRE. ) );
#62141 = CARTESIAN_POINT ( 'NONE',  ( -76.69088380834561747, -29.99999999999999645, -16.87249134269979578 ) ) ;
#62142 = CIRCLE ( 'NONE', #8661, 5.000000000000001776 ) ;
#62143 = CARTESIAN_POINT ( 'NONE',  ( 6.231493956936414058, 147.8264543773111654, 0.000000000000000000 ) ) ;
#62144 = FACE_OUTER_BOUND ( 'NONE', #70157, .T. ) ;
#62145 = CARTESIAN_POINT ( 'NONE',  ( -14.21470604016367290, 4.169147088453041050, -4.752692181068058908 ) ) ;
#62146 = AXIS2_PLACEMENT_3D ( 'NONE', #30666, #55936, #31204 ) ;
#62147 = PRODUCT_RELATED_PRODUCT_CATEGORY ( 'part', '', ( #27484 ) ) ;
#62148 = CARTESIAN_POINT ( 'NONE',  ( 7.188101187499999156, -17.75000000204838457, 2.977408999572654924 ) ) ;
#62149 = CARTESIAN_POINT ( 'NONE',  ( 15.60168599250222243, 302.5584640164269103, -10.06235166778797208 ) ) ;
#62150 = DIRECTION ( 'NONE',  ( 0.000000000000000000, 0.000000000000000000, 1.000000000000000000 ) ) ;
#62151 = ORIENTED_EDGE ( 'NONE', *, *, #26086, .T. ) ;
#62152 = CARTESIAN_POINT ( 'NONE',  ( -37.26717676828223347, 490.8904373082769439, 12.42641029562198618 ) ) ;
#62153 = CARTESIAN_POINT ( 'NONE',  ( 7.922798488042200660, -4.627419312545549168, -8.057411459260043429 ) ) ;
#62154 = CARTESIAN_POINT ( 'NONE',  ( -9.590509843993705985, 9.008796699721322909, 0.000000000000000000 ) ) ;
#62155 = CARTESIAN_POINT ( 'NONE',  ( -4.852941176470592310, -2.999999999999999112, -70.80672828634229177 ) ) ;
#62156 = CARTESIAN_POINT ( 'NONE',  ( -15.45234973294482117, 2.833591715794670396, 2.076776216679724119 ) ) ;
#62157 = AXIS2_PLACEMENT_3D ( 'NONE', #14415, #46806, #38216 ) ;
#62158 = VERTEX_POINT ( 'NONE', #28143 ) ;
#62159 = CARTESIAN_POINT ( 'NONE',  ( 64.29999999999999716, -3.309500000000000774, 4.475777889183797681E-16 ) ) ;
#62160 = VECTOR ( 'NONE', #24552, 1000.000000000000000 ) ;
#62161 = CARTESIAN_POINT ( 'NONE',  ( 10.74465425721583856, 48.00000000000000000, -95.72854256505367232 ) ) ;
#62162 = ORIENTED_EDGE ( 'NONE', *, *, #80456, .T. ) ;
#62163 = EDGE_CURVE ( 'NONE', #2998, #83001, #28354, .T. ) ;
#62164 =( LENGTH_UNIT ( ) NAMED_UNIT ( * ) SI_UNIT ( .MILLI., .METRE. ) );
#62165 = CARTESIAN_POINT ( 'NONE',  ( 0.000000000000000000, 4.898587196589412829E-16, -4.000000000000000000 ) ) ;
#62166 = CARTESIAN_POINT ( 'NONE',  ( 6.786616689952412074, 41.72678941544184994, -59.11526159199856068 ) ) ;
#62167 = UNCERTAINTY_MEASURE_WITH_UNIT (LENGTH_MEASURE( 1.000000000000000082E-05 ), #43860, 'distance_accuracy_value', 'NONE');
#62168 = CARTESIAN_POINT ( 'NONE',  ( -108.5578913194906931, -60.00000000000000711, 194.6075768431653330 ) ) ;
#62169 = CARTESIAN_POINT ( 'NONE',  ( 5.799999999999999822, 9.237604307034018802, 0.000000000000000000 ) ) ;
#62170 = DIRECTION ( 'NONE',  ( 1.000000000000000000, 0.000000000000000000, 0.000000000000000000 ) ) ;
#62171 = DIRECTION ( 'NONE',  ( 0.000000000000000000, 0.000000000000000000, 1.000000000000000000 ) ) ;
#62172 = CARTESIAN_POINT ( 'NONE',  ( 17.76463732149834129, 34.19216742441107471, -23.79440628143193592 ) ) ;
#62173 = CARTESIAN_POINT ( 'NONE',  ( -83.57352743474167767, -42.98438523098171515, 179.4517796046237095 ) ) ;
#62174 = CARTESIAN_POINT ( 'NONE',  ( 16.52731600354976393, 43.98685737190850631, -87.77869701378344303 ) ) ;
#62175 = VECTOR ( 'NONE', #77211, 1000.000000000000000 ) ;
#62176 = EDGE_CURVE ( 'NONE', #42837, #50100, #18726, .T. ) ;
#62177 =( BOUNDED_CURVE ( )  B_SPLINE_CURVE ( 2, ( #36315, #69182, #20130, #85903, #52982, #44906, #14089, #104171, #38410 ),
 .UNSPECIFIED., .F., .F. ) 
 B_SPLINE_CURVE_WITH_KNOTS ( ( 3, 2, 2, 2, 3 ),
 ( 0.4558823529411765163, 0.4632352941176471339, 0.4705882352941177516, 0.4779411764705883692, 0.4852941176470589313 ),
 .UNSPECIFIED. ) 
 CURVE ( )  GEOMETRIC_REPRESENTATION_ITEM ( )  RATIONAL_B_SPLINE_CURVE ( ( 0.9999999999999994449, 0.9238795325112872936, 1.000000000000000000, 0.9238795325112867385, 1.000000000000000000, 0.9238795325112867385, 1.000000000000000000, 0.9238795325112856283, 1.000000000000001110 ) ) 
 REPRESENTATION_ITEM ( '' )  );
#62178 = ORIENTED_EDGE ( 'NONE', *, *, #71799, .T. ) ;
#62179 = PLANE ( 'NONE',  #69926 ) ;
#62180 = ADVANCED_FACE ( 'NONE', ( #53448 ), #19369, .F. ) ;
#62181 = CARTESIAN_POINT ( 'NONE',  ( 1.000000000000000000, -69.59657292934913642, 12.76848391599222765 ) ) ;
#62182 = CARTESIAN_POINT ( 'NONE',  ( -86.18221325923798304, -60.14546413765744859, 16.47069715629995557 ) ) ;
#62183 = CONICAL_SURFACE ( 'NONE', #63873, 3.309500000000007880, 0.9599310885968770357 ) ;
#62184 = DIRECTION ( 'NONE',  ( -1.000000000000000000, -1.224606353822377258E-16, -0.000000000000000000 ) ) ;
#62185 =( NAMED_UNIT ( * ) PLANE_ANGLE_UNIT ( ) SI_UNIT ( $, .RADIAN. ) );
#62186 = CARTESIAN_POINT ( 'NONE',  ( 9.300358455351362963, 140.6343319111669246, -4.999999999999999112 ) ) ;
#62187 = CARTESIAN_POINT ( 'NONE',  ( -4.555094537983155334, -5.243183837310271045, -6.208110906918266281 ) ) ;
#62188 = CARTESIAN_POINT ( 'NONE',  ( 10.04205104294044482, 18.64316884711816513, -37.36680950588930727 ) ) ;
#62189 = VECTOR ( 'NONE', #92129, 1000.000000000000000 ) ;
#62190 = CARTESIAN_POINT ( 'NONE',  ( 102.0109750195309175, -30.00000000000007816, 198.2012210982776708 ) ) ;
#62191 = CARTESIAN_POINT ( 'NONE',  ( -5.404594501095028576E-15, 34.25047185182970111, 44.13186320217320713 ) ) ;
#62192 = VECTOR ( 'NONE', #84654, 1000.000000000000341 ) ;
#62193 = CARTESIAN_POINT ( 'NONE',  ( -98.75680450758818552, -14.21045842199431064, 105.0421542466116023 ) ) ;
#62194 = CARTESIAN_POINT ( 'NONE',  ( -64.12976986942591395, -32.53224925924665456, 80.08508429969118936 ) ) ;
#62195 = EDGE_LOOP ( 'NONE', ( #30286, #86656, #69790, #92998, #37663, #24095 ) ) ;
#62196 = CARTESIAN_POINT ( 'NONE',  ( 91.59609553898350498, -30.00000000000011013, 199.7677339052814602 ) ) ;
#62197 = CARTESIAN_POINT ( 'NONE',  ( -59.26337206958330484, 39.42463816063593640, 26.86447829808549059 ) ) ;
#62198 = CARTESIAN_POINT ( 'NONE',  ( 46.36952623917631655, -60.00000000001961098, 69.16733414759707443 ) ) ;
#62199 = VERTEX_POINT ( 'NONE', #43229 ) ;
#62200 = CARTESIAN_POINT ( 'NONE',  ( -32.89395609998138070, 463.7240567052280653, 7.148062722717972051 ) ) ;
#62201 = EDGE_CURVE ( 'NONE', #9931, #42028, #76114, .T. ) ;
#62202 = CARTESIAN_POINT ( 'NONE',  ( -7.188101187500000933, -21.87500000204838813, -2.977408999572651371 ) ) ;
#62203 =( NAMED_UNIT ( * ) SI_UNIT ( $, .STERADIAN. ) SOLID_ANGLE_UNIT ( ) );
#62204 = ORIENTED_EDGE ( 'NONE', *, *, #23416, .F. ) ;
#62205 = CARTESIAN_POINT ( 'NONE',  ( -8.000000000000000000, -26.93750000409677625, -9.797174393178825657E-16 ) ) ;
#62206 = EDGE_LOOP ( 'NONE', ( #47792, #91756, #72106, #46435, #59045, #13440 ) ) ;
#62207 = CARTESIAN_POINT ( 'NONE',  ( 4.999999999999995559, -4.000000000000003553, 40.07669683062201926 ) ) ;
#62208 = CARTESIAN_POINT ( 'NONE',  ( -39.64792090968533245, 485.8593029974498450, -5.004078333543798607 ) ) ;
#62209 = CARTESIAN_POINT ( 'NONE',  ( -82.63119616871206574, -59.99999999999995737, -26.28467615004301194 ) ) ;
#62210 = CARTESIAN_POINT ( 'NONE',  ( 36.68484412175028808, 425.7526927197205282, 5.533094624903789338 ) ) ;
#62211 = CARTESIAN_POINT ( 'NONE',  ( -2.977408999572650039, -34.06250000204839523, -7.188101187500001821 ) ) ;
#62212 = CARTESIAN_POINT ( 'NONE',  ( 32.86259851300478374, 485.9239370913665539, 5.440925357812795404 ) ) ;
#62213 = CARTESIAN_POINT ( 'NONE',  ( 1.650803255657546709, -4.285714285714293581, 25.22241582816891636 ) ) ;
#62214 = SURFACE_SIDE_STYLE ('',( #22281 ) ) ;
#62215 = DIRECTION ( 'NONE',  ( -1.224646799147349509E-16, 0.000000000000000000, -1.000000000000000000 ) ) ;
#62216 = CARTESIAN_POINT ( 'NONE',  ( -8.000086790516061086, 109.0001735810600678, 0.2639471549312831233 ) ) ;
#62217 = CARTESIAN_POINT ( 'NONE',  ( 38.10433946279106010, 437.2340514686391089, 4.662695304591946588 ) ) ;
#62218 = LINE ( 'NONE', #2474, #101710 ) ;
#62219 = ORIENTED_EDGE ( 'NONE', *, *, #92025, .F. ) ;
#62220 = LINE ( 'NONE', #5021, #22983 ) ;
#62221 = CARTESIAN_POINT ( 'NONE',  ( -34.14642055599488657, 464.2253822571460091, 6.054698699017524888 ) ) ;
#62222 = CARTESIAN_POINT ( 'NONE',  ( 35.05802874304034589, -46.42926842311833013, 36.68586914177578961 ) ) ;
#62223 = AXIS2_PLACEMENT_3D ( 'NONE', #94697, #28381, #28930 ) ;
#62224 = CARTESIAN_POINT ( 'NONE',  ( 68.70539558375507738, 6.856755485862130937E-15, 0.000000000000000000 ) ) ;
#62225 = ORIENTED_EDGE ( 'NONE', *, *, #32310, .T. ) ;
#62226 = CARTESIAN_POINT ( 'NONE',  ( 6.123233995736763324E-16, 48.00000000000000000, -75.00000000000001421 ) ) ;
#62227 = ADVANCED_FACE ( 'NONE', ( #3838 ), #50776, .T. ) ;
#62228 = CIRCLE ( 'NONE', #98368, 5.000000000000002665 ) ;
#62230 = CARTESIAN_POINT ( 'NONE',  ( -5.500000000000007105, 42.00000000000000000, -62.89165061492693809 ) ) ;
#62229 = CARTESIAN_POINT ( 'NONE',  ( 4.998455113691382401, -5.000000000000000000, -15.56475508679018027 ) ) ;
#62231 = FACE_OUTER_BOUND ( 'NONE', #96523, .T. ) ;
#62232 = DIRECTION ( 'NONE',  ( -1.000000000000000000, -1.224606353822377258E-16, -0.000000000000000000 ) ) ;
#62233 = DIRECTION ( 'NONE',  ( 1.000000000000000000, 0.000000000000000000, 0.000000000000000000 ) ) ;
#62234 =( NAMED_UNIT ( * ) SI_UNIT ( $, .STERADIAN. ) SOLID_ANGLE_UNIT ( ) );
#62235 = DIRECTION ( 'NONE',  ( 1.000000000000000000, 0.000000000000000000, 0.000000000000000000 ) ) ;
#62236 = FILL_AREA_STYLE ('',( #101061 ) ) ;
#62237 = ORIENTED_EDGE ( 'NONE', *, *, #44622, .T. ) ;
#62238 = CARTESIAN_POINT ( 'NONE',  ( 92.58558766009146268, -60.00000000000001421, -2.558238702422552802 ) ) ;
#62239 =( NAMED_UNIT ( * ) SI_UNIT ( $, .STERADIAN. ) SOLID_ANGLE_UNIT ( ) );
#62240 = CARTESIAN_POINT ( 'NONE',  ( -7.284483346386982916E-16, -0.6346842323187733559, 6.500000000000000000 ) ) ;
#62241 = CARTESIAN_POINT ( 'NONE',  ( -6.422423974165688776, 41.30029428932490987, -70.89074254924834406 ) ) ;
#62242 = CARTESIAN_POINT ( 'NONE',  ( 16.14595037822613932, 12.99999999999999289, 0.000000000000000000 ) ) ;
#62243 = ORIENTED_EDGE ( 'NONE', *, *, #8535, .T. ) ;
#62244 = AXIS2_PLACEMENT_3D ( 'NONE', #8464, #14954, #33302 ) ;
#62245 = CARTESIAN_POINT ( 'NONE',  ( -90.93883295786046972, -30.00000000000355271, 199.4788298540976257 ) ) ;
#62246 = VERTEX_POINT ( 'NONE', #35704 ) ;
#62247 = CARTESIAN_POINT ( 'NONE',  ( 26.11923076923076792, 1.411358822780289120E-15, 0.000000000000000000 ) ) ;
#62248 = CYLINDRICAL_SURFACE ( 'NONE', #86761, 4.000000000000000888 ) ;
#62249 = CARTESIAN_POINT ( 'NONE',  ( 83.69130407765804591, -52.73017012645138379, -15.75844283506252097 ) ) ;
#62250 = CARTESIAN_POINT ( 'NONE',  ( 7.188101187499999156, -31.62500000204838813, 2.977408999572654924 ) ) ;
#62251 = FACE_OUTER_BOUND ( 'NONE', #52854, .T. ) ;
#62252 = CARTESIAN_POINT ( 'NONE',  ( -16.45446808530939009, 304.5657599011952925, 8.876165325073888113 ) ) ;
#62253 = SURFACE_STYLE_USAGE ( .BOTH. , #29884 ) ;
#62254 = VERTEX_POINT ( 'NONE', #68582 ) ;
#62256 = ORIENTED_EDGE ( 'NONE', *, *, #68601, .F. ) ;
#62255 = CARTESIAN_POINT ( 'NONE',  ( 36.36650669486618881, -3.851859888774471706E-31, 4.000000000000000888 ) ) ;
#62257 = CARTESIAN_POINT ( 'NONE',  ( 80.74191332831607326, -25.62223386318168039, 135.9007221451898033 ) ) ;
#62258 = ADVANCED_FACE ( 'NONE', ( #69111 ), #74870, .T. ) ;
#62259 = ORIENTED_EDGE ( 'NONE', *, *, #90112, .T. ) ;
#62260 = PRESENTATION_LAYER_ASSIGNMENT (  '', '', ( #19247 ) ) ;
#62261 = CARTESIAN_POINT ( 'NONE',  ( -12.50000000000001066, 39.72486035274638283, -64.91592812567742499 ) ) ;
#62262 = CARTESIAN_POINT ( 'NONE',  ( 4.401442555609581635E-16, -17.28125000204838813, -7.188101187500000044 ) ) ;
#62263 = CARTESIAN_POINT ( 'NONE',  ( -109.9801870187163644, -57.66844046886203756, 196.1568551196091903 ) ) ;
#62264 = EDGE_CURVE ( 'NONE', #50990, #25464, #62605, .T. ) ;
#62265 = EDGE_LOOP ( 'NONE', ( #74092, #80987, #69133, #28082, #35016 ) ) ;
#62266 = PRESENTATION_LAYER_ASSIGNMENT (  '', '', ( #69108 ) ) ;
#62268 = CARTESIAN_POINT ( 'NONE',  ( 6.123233995736763324E-16, 48.00000000000000000, -95.00000000000000000 ) ) ;
#62267 = VECTOR ( 'NONE', #52082, 1000.000000000000000 ) ;
#62269 = CARTESIAN_POINT ( 'NONE',  ( 6.866539600944548738, 41.67963879285974116, -59.06571970116536363 ) ) ;
#62270 = CARTESIAN_POINT ( 'NONE',  ( 49.13304414347678772, 12.95525746345893481, -16.19504546972810033 ) ) ;
#62271 = CARTESIAN_POINT ( 'NONE',  ( -5.656854249492381470, -17.75000000409676915, 5.656854249492379694 ) ) ;
#62272 = CARTESIAN_POINT ( 'NONE',  ( -49.65412818270985440, -29.62131271632045326, 46.06396428430316803 ) ) ;
#62273 = DIRECTION ( 'NONE',  ( -0.000000000000000000, 0.3548932414479616382, 0.9349068334195439478 ) ) ;
#62274 = CARTESIAN_POINT ( 'NONE',  ( -9.176855344542985904, 85.52960426977412567, -3.973472207155925862 ) ) ;
#62275 = CARTESIAN_POINT ( 'NONE',  ( 4.044781357444436232, 51.90680650645019512, 7.474578379459966726 ) ) ;
#62276 = ADVANCED_FACE ( 'NONE', ( #5932 ), #88681, .F. ) ;
#62277 = CARTESIAN_POINT ( 'NONE',  ( 38.74267013308406860, 27.39035684269769888, 11.77443177698138221 ) ) ;
#62278 = ORIENTED_EDGE ( 'NONE', *, *, #15787, .F. ) ;
#62279 = DIRECTION ( 'NONE',  ( -1.000000000000000000, 0.000000000000000000, 0.000000000000000000 ) ) ;
#62280 = DIRECTION ( 'NONE',  ( 0.000000000000000000, 0.000000000000000000, 1.000000000000000000 ) ) ;
#62281 = CARTESIAN_POINT ( 'NONE',  ( -53.91796304099374026, -29.20809689804048759, -34.29182838456584648 ) ) ;
#62282 = CARTESIAN_POINT ( 'NONE',  ( -84.24486252583190549, -29.99999999999999645, 163.2080965712097509 ) ) ;
#62283 = CARTESIAN_POINT ( 'NONE',  ( 7.500000000000007994, 40.00000000000000000, -72.67206406577979294 ) ) ;
#62284 = VERTEX_POINT ( 'NONE', #30243 ) ;
#62285 = CARTESIAN_POINT ( 'NONE',  ( -26.01163681415079765, 37.20415886906720715, -8.178344558965836342 ) ) ;
#62286 = CARTESIAN_POINT ( 'NONE',  ( 83.72989002924066426, -57.54382900384099031, 201.5987905778323181 ) ) ;
#62287 = CARTESIAN_POINT ( 'NONE',  ( 68.05335443350816149, -60.22836387010958958, -27.16755064673009201 ) ) ;
#62288 = CARTESIAN_POINT ( 'NONE',  ( -6.781345014477443200, -3.590342129888875355, -6.122077150241855392 ) ) ;
#62289 = AXIS2_PLACEMENT_3D ( 'NONE', #41255, #74668, #49873 ) ;
#62290 = CARTESIAN_POINT ( 'NONE',  ( -14.37785056367358116, 21.52979621148618250, 5.240284069518001964 ) ) ;
#62291 = DIRECTION ( 'NONE',  ( -0.5735764363510494901, -0.8191520442889894671, 0.000000000000000000 ) ) ;
#62292 = CARTESIAN_POINT ( 'NONE',  ( -65.19869439566309666, -59.99999999999999289, 119.1295691880435896 ) ) ;
#62293 = CARTESIAN_POINT ( 'NONE',  ( -4.000000000000000888, 4.898587196589413815E-16, 3.469446951953614189E-15 ) ) ;
#62294 = CARTESIAN_POINT ( 'NONE',  ( 0.000000000000000000, 0.000000000000000000, 0.000000000000000000 ) ) ;
#62295 = CARTESIAN_POINT ( 'NONE',  ( 60.66923414622826982, 50.00000000000000000, 17.93278245653309710 ) ) ;
#62296 = CARTESIAN_POINT ( 'NONE',  ( -86.28001627044659472, -24.64161911929981130, 181.9982194805413656 ) ) ;
#62297 = ORIENTED_EDGE ( 'NONE', *, *, #84920, .F. ) ;
#62298 = CARTESIAN_POINT ( 'NONE',  ( 33.07871186279389519, 322.7520366298887211, -5.621988175703525492 ) ) ;
#62299 = CARTESIAN_POINT ( 'NONE',  ( -11.82165952410163356, 294.5900423753296309, -10.05563889079273387 ) ) ;
#62300 = CARTESIAN_POINT ( 'NONE',  ( -7.109733192396789470, 41.69026681596732686, -59.69141549319190432 ) ) ;
#62301 = CARTESIAN_POINT ( 'NONE',  ( 12.45393346519260724, -3.927217745179178099, -76.72514752459306919 ) ) ;
#62302 = EDGE_CURVE ( 'NONE', #49340, #81388, #784, .T. ) ;
#62303 = CARTESIAN_POINT ( 'NONE',  ( -27.08705420553263821, 306.3021870952275094, -9.457589952739034800 ) ) ;
#62304 = DIRECTION ( 'NONE',  ( 0.000000000000000000, 1.000000000000000000, 0.000000000000000000 ) ) ;
#62305 = CARTESIAN_POINT ( 'NONE',  ( 74.56127108291157413, -1.232595164407830946E-29, 4.000000000000007105 ) ) ;
#62306 = LINE ( 'NONE', #81107, #13808 ) ;
#62307 = ORIENTED_EDGE ( 'NONE', *, *, #57784, .F. ) ;
#62308 = SURFACE_STYLE_FILL_AREA ( #103285 ) ;
#62309 = ADVANCED_FACE ( 'NONE', ( #88994 ), #31881, .F. ) ;
#62310 = CARTESIAN_POINT ( 'NONE',  ( 10.98741596925694353, 19.21026732195910824, 8.912652956011438476 ) ) ;
#62311 = CARTESIAN_POINT ( 'NONE',  ( 86.89874827037927218, -29.99999999999997868, -18.81865104787653920 ) ) ;
#62312 = CARTESIAN_POINT ( 'NONE',  ( -80.67225572899188535, -22.15189889752034702, 132.4868695557189540 ) ) ;
#62313 = ORIENTED_EDGE ( 'NONE', *, *, #72729, .T. ) ;
#62314 = FACE_OUTER_BOUND ( 'NONE', #13510, .T. ) ;
#62315 = CARTESIAN_POINT ( 'NONE',  ( 43.00000000000000000, 438.4646224975062978, 9.895601460515774050 ) ) ;
#62316 = CARTESIAN_POINT ( 'NONE',  ( 65.36663488618646056, -57.67974036715745001, 127.4738114322918392 ) ) ;
#62317 =( NAMED_UNIT ( * ) PLANE_ANGLE_UNIT ( ) SI_UNIT ( $, .RADIAN. ) );
#62318 = CARTESIAN_POINT ( 'NONE',  ( 44.12118527028935944, 333.2930620178879622, -0.6804749548666318981 ) ) ;
#62319 = CARTESIAN_POINT ( 'NONE',  ( 44.26701432269690883, 464.1304138491097433, 8.787925729982960732 ) ) ;
#62320 = VERTEX_POINT ( 'NONE', #96031 ) ;
#62321 = FACE_OUTER_BOUND ( 'NONE', #104505, .T. ) ;
#62322 = AXIS2_PLACEMENT_3D ( 'NONE', #66372, #42094, #31907 ) ;
#62323 = CARTESIAN_POINT ( 'NONE',  ( 42.33349330513380693, 1.593028355512270567E-15, 0.000000000000000000 ) ) ;
#62324 = CARTESIAN_POINT ( 'NONE',  ( -7.188101187500001821, -26.00000000204838457, -2.977408999572651371 ) ) ;
#62325 = CIRCLE ( 'NONE', #101944, 1.999999999999998224 ) ;
#62326 = DIRECTION ( 'NONE',  ( -0.000000000000000000, -0.000000000000000000, -1.000000000000000000 ) ) ;
#62327 = CARTESIAN_POINT ( 'NONE',  ( 5.754767977403508539, 41.95837094234298092, -69.99685021967000864 ) ) ;
#62328 = EDGE_CURVE ( 'NONE', #49522, #79906, #79826, .T. ) ;
#62329 = DIRECTION ( 'NONE',  ( -1.224646799147351482E-16, 0.000000000000000000, -1.000000000000000000 ) ) ;
#62330 = CARTESIAN_POINT ( 'NONE',  ( 1.337681583493947279, -5.478209635665768573, -13.97306298562694060 ) ) ;
#62331 = CARTESIAN_POINT ( 'NONE',  ( 42.10086803841213765, 435.6552064019005570, 19.95582312411065828 ) ) ;
#62332 = VERTEX_POINT ( 'NONE', #104636 ) ;
#62333 = CARTESIAN_POINT ( 'NONE',  ( 6.750000000000017764, 11.69134295108991317, -13.00000000000000000 ) ) ;
#62334 = CIRCLE ( 'NONE', #88192, 56.85174851683467523 ) ;
#62336 = CARTESIAN_POINT ( 'NONE',  ( 24.52113603086038296, -29.04043804430480691, 29.86937766656776816 ) ) ;
#62335 = CARTESIAN_POINT ( 'NONE',  ( -45.38252603333997826, -14.21045842199430354, 49.92404905378138125 ) ) ;
#62337 = CARTESIAN_POINT ( 'NONE',  ( 50.10796912846467421, 53.37899725327127953, -25.05398456423232645 ) ) ;
#62338 = EDGE_LOOP ( 'NONE', ( #44606, #89890, #75586, #47524, #75272, #64555 ) ) ;
#62339 = VECTOR ( 'NONE', #49352, 1000.000000000000341 ) ;
#62340 = ADVANCED_FACE ( 'NONE', ( #14545 ), #22157, .T. ) ;
#62341 = UNCERTAINTY_MEASURE_WITH_UNIT (LENGTH_MEASURE( 1.000000000000000082E-05 ), #97403, 'distance_accuracy_value', 'NONE');
#62342 = VERTEX_POINT ( 'NONE', #38347 ) ;
#62343 = PRODUCT_DEFINITION_SHAPE ( 'NONE', 'NONE',  #106808 ) ;
#62344 = CARTESIAN_POINT ( 'NONE',  ( 72.06187821828702056, -37.99999999999999289, -21.47593870486667811 ) ) ;
#62345 = CARTESIAN_POINT ( 'NONE',  ( 14.54015256618498242, 142.2617268803927288, 0.000000000000000000 ) ) ;
#62346 = CYLINDRICAL_SURFACE ( 'NONE', #75910, 5.000000000000002665 ) ;
#62347 = CARTESIAN_POINT ( 'NONE',  ( 13.28402714419663155, 1.403786919265707089, 14.93563726026576788 ) ) ;
#62348 = DIRECTION ( 'NONE',  ( 0.000000000000000000, -1.000000000000000000, 0.000000000000000000 ) ) ;
#62349 = ORIENTED_EDGE ( 'NONE', *, *, #75294, .T. ) ;
#62351 = EDGE_CURVE ( 'NONE', #55752, #86888, #33489, .T. ) ;
#62350 = B_SPLINE_CURVE_WITH_KNOTS ( 'NONE', 3,
 ( #39915, #994, #49041, #40434, #81938, #99735, #32903, #57661, #91656, #462, #50117, #82492, #33431, #65245, #64717, #89530, #33973, #73313, #99185, #23757, #25348, #48513 ),
 .UNSPECIFIED., .F., .F.,
 ( 4, 2, 2, 2, 2, 2, 2, 2, 2, 2, 4 ),
 ( 0.003600184084728503923, 0.004103037208643595807, 0.004605890332558686823, 0.004857316894516234065, 0.005108743456473779573, 0.005611596580388875793, 0.005863023142346423904, 0.006114449704303972014, 0.006617302828219070836, 0.007120155952134168791, 0.007623009076049266745 ),
 .UNSPECIFIED. ) ;
#62352 = CARTESIAN_POINT ( 'NONE',  ( 17.50000000000002132, 46.94999999999998153, 64.09953197957062798 ) ) ;
#62353 = CARTESIAN_POINT ( 'NONE',  ( 21.97248774489993295, 25.82615788719429872, -32.15153141218966226 ) ) ;
#62354 = CARTESIAN_POINT ( 'NONE',  ( -11.28474606562284777, 20.02052538581057917, -8.415621975122691723 ) ) ;
#62355 = CARTESIAN_POINT ( 'NONE',  ( -0.000000000000000000, 58.72416816948006613, -16.91618513671782509 ) ) ;
#62356 = CARTESIAN_POINT ( 'NONE',  ( 81.28015307217464169, -29.99999999999999645, -0.2274418294518818218 ) ) ;
#62357 = DIRECTION ( 'NONE',  ( 1.000000000000000000, 0.000000000000000000, 0.000000000000000000 ) ) ;
#62358 = ADVANCED_FACE ( 'NONE', ( #96562 ), #42173, .T. ) ;
#62359 = ORIENTED_EDGE ( 'NONE', *, *, #68214, .T. ) ;
#62360 = AXIS2_PLACEMENT_3D ( 'NONE', #4990, #71302, #47018 ) ;
#62361 = ORIENTED_EDGE ( 'NONE', *, *, #66599, .F. ) ;
#62362 = ORIENTED_EDGE ( 'NONE', *, *, #38683, .T. ) ;
#62363 = CARTESIAN_POINT ( 'NONE',  ( 19.34999999999999787, 1.533819458162526451E-15, 0.000000000000000000 ) ) ;
#62364 = SURFACE_STYLE_USAGE ( .BOTH. , #77473 ) ;
#62365 = DIRECTION ( 'NONE',  ( 0.000000000000000000, 0.000000000000000000, -1.000000000000000000 ) ) ;
#62366 = MECHANICAL_DESIGN_GEOMETRIC_PRESENTATION_REPRESENTATION (  '', ( #89896 ), #84749 ) ;
#62367 = CARTESIAN_POINT ( 'NONE',  ( -37.71361324390009884, 391.6894161628994198, 6.182277153786067458 ) ) ;
#62368 = DIRECTION ( 'NONE',  ( -1.000000000000000000, 8.673617379884035472E-16, 0.000000000000000000 ) ) ;
#62369 = CARTESIAN_POINT ( 'NONE',  ( -7.002641335706725201, -86.05087262680831373, 3.868676264653294172 ) ) ;
#62370 = LINE ( 'NONE', #21392, #98335 ) ;
#62371 = ORIENTED_EDGE ( 'NONE', *, *, #47973, .F. ) ;
#62372 = CARTESIAN_POINT ( 'NONE',  ( -9.739726766104087829, 48.00000000000000000, -87.61747884499078509 ) ) ;
#62373 = VECTOR ( 'NONE', #33232, 1000.000000000000000 ) ;
#62374 = ORIENTED_EDGE ( 'NONE', *, *, #46957, .F. ) ;
#62375 = CARTESIAN_POINT ( 'NONE',  ( -4.813668318631093790, -63.20486770173315705, 3.583991016754781267 ) ) ;
#62376 = LINE ( 'NONE', #85588, #15978 ) ;
#62377 = CARTESIAN_POINT ( 'NONE',  ( -41.32135724059589421, 485.4908763545977877, -3.838542627834635734 ) ) ;
#62378 = DIRECTION ( 'NONE',  ( 0.000000000000000000, 0.000000000000000000, 1.000000000000000000 ) ) ;
#62379 = CARTESIAN_POINT ( 'NONE',  ( 63.78764792876993539, -32.53022072251602026, 79.11273379103411685 ) ) ;
#62380 = ORIENTED_EDGE ( 'NONE', *, *, #66206, .T. ) ;
#62381 = CARTESIAN_POINT ( 'NONE',  ( -7.150000000000001243, 41.64999999999999147, -68.91429205801802027 ) ) ;
#62382 = CARTESIAN_POINT ( 'NONE',  ( -62.68570420933652798, -37.65611969153471961, -33.47651594426432808 ) ) ;
#62383 = CARTESIAN_POINT ( 'NONE',  ( -5.835236874069059887, 11.94353909508101985, -3.867049007331976540 ) ) ;
#62384 = DIRECTION ( 'NONE',  ( -0.8191520442889884679, 1.003171929053520679E-16, 0.5735764363510508224 ) ) ;
#62385 = EDGE_CURVE ( 'NONE', #96664, #21098, #66913, .T. ) ;
#62386 = ORIENTED_EDGE ( 'NONE', *, *, #23812, .F. ) ;
#62387 = CARTESIAN_POINT ( 'NONE',  ( 0.000000000000000000, 4.898587196589412829E-16, -4.000000000000000000 ) ) ;
#62388 = CARTESIAN_POINT ( 'NONE',  ( 42.88690404153408764, 465.8389234275369972, 12.02232841035013422 ) ) ;
#62389 = FACE_OUTER_BOUND ( 'NONE', #92017, .T. ) ;
#62390 = CARTESIAN_POINT ( 'NONE',  ( 0.000000000000000000, 0.000000000000000000, 0.000000000000000000 ) ) ;
#62391 = DIRECTION ( 'NONE',  ( -0.2270551762890244685, 0.1092888915761295876, 0.9677302749725364972 ) ) ;
#62392 = CARTESIAN_POINT ( 'NONE',  ( 85.78379958766628022, -57.44889651991635304, 192.9311378948322329 ) ) ;
#62393 = CARTESIAN_POINT ( 'NONE',  ( 44.17139329880469489, 463.1540488235348789, 6.319274787421930384 ) ) ;
#62394 = CARTESIAN_POINT ( 'NONE',  ( -9.880470759316240859, 7.740809967772715794, 0.000000000000000000 ) ) ;
#62395 = DIRECTION ( 'NONE',  ( 1.000000000000000000, 0.000000000000000000, 1.160749806054361473E-16 ) ) ;
#62396 = TOROIDAL_SURFACE ( 'NONE', #81296, 12.00000000000003908, 1.000000000000000000 ) ;
#62397 = CARTESIAN_POINT ( 'NONE',  ( 17.33349330513380337, 1.593028355512270567E-15, 0.000000000000000000 ) ) ;
#62398 = CARTESIAN_POINT ( 'NONE',  ( 13.59360248487383771, -51.99192117344531994, 23.64795065864135637 ) ) ;
#62399 = DIRECTION ( 'NONE',  ( -0.000000000000000000, -1.000000000000000000, -0.000000000000000000 ) ) ;
#62400 =( GEOMETRIC_REPRESENTATION_CONTEXT ( 3 ) GLOBAL_UNCERTAINTY_ASSIGNED_CONTEXT ( ( #82921 ) ) GLOBAL_UNIT_ASSIGNED_CONTEXT ( ( #8237, #17415, #58389 ) ) REPRESENTATION_CONTEXT ( 'NONE', 'WORKASPACE' ) );
#62401 = CARTESIAN_POINT ( 'NONE',  ( -100.7581804555464373, -30.00000000000000355, 180.7064422284077807 ) ) ;
#62402 = LINE ( 'NONE', #28466, #96819 ) ;
#62403 = MECHANICAL_DESIGN_GEOMETRIC_PRESENTATION_REPRESENTATION (  '', ( #67560 ), #105496 ) ;
#62404 = CARTESIAN_POINT ( 'NONE',  ( 13.25658586220136925, -57.67136151655925147, 41.68871071852922228 ) ) ;
#62406 = CARTESIAN_POINT ( 'NONE',  ( 43.99295543328099711, 464.6035880628708128, 10.45302038925775179 ) ) ;
#62405 = CARTESIAN_POINT ( 'NONE',  ( 10.28624191511840458, 43.99263840937192782, 12.90779740156148847 ) ) ;
#62407 = CONICAL_SURFACE ( 'NONE', #2087, 4.000000000000001776, 0.9599310885968774798 ) ;
#62408 = PRESENTATION_STYLE_ASSIGNMENT (( #23021 ) ) ;
#62409 = CARTESIAN_POINT ( 'NONE',  ( -17.51905876331014511, 50.00000000000000711, 63.23049753801218742 ) ) ;
#62410 = CARTESIAN_POINT ( 'NONE',  ( -9.910377230549258343, 15.23810023151367155, 1.510421413154401371 ) ) ;
#62411 = CARTESIAN_POINT ( 'NONE',  ( 46.00000000000000000, 486.5369520448867888, 4.408549137149760710 ) ) ;
#62412 = SURFACE_SIDE_STYLE ('',( #62940 ) ) ;
#62413 = DIRECTION ( 'NONE',  ( 0.000000000000000000, -0.000000000000000000, 1.000000000000000000 ) ) ;
#62414 = CARTESIAN_POINT ( 'NONE',  ( -87.46061870122996140, -42.74219916028555843, 190.5714494835581831 ) ) ;
#62415 = EDGE_LOOP ( 'NONE', ( #38956, #21910, #98517, #17645 ) ) ;
#62416 = CARTESIAN_POINT ( 'NONE',  ( 39.23335254075882261, 485.6839217479536046, -4.505383133704073728 ) ) ;
#62417 = DIRECTION ( 'NONE',  ( 0.000000000000000000, 0.000000000000000000, 1.000000000000000000 ) ) ;
#62418 = CARTESIAN_POINT ( 'NONE',  ( -12.57806496835559962, -53.40254179854935046, 32.85052738830435004 ) ) ;
#62420 = CARTESIAN_POINT ( 'NONE',  ( -41.61208469664205722, 437.6914194411011181, 21.78364932966315237 ) ) ;
#62419 = CARTESIAN_POINT ( 'NONE',  ( -106.0619102637862312, -59.99999999999999289, 161.5357636300732338 ) ) ;
#62421 = EDGE_CURVE ( 'NONE', #65506, #73382, #37065, .T. ) ;
#62422 = EDGE_LOOP ( 'NONE', ( #57746, #106246, #2854, #35405 ) ) ;
#62423 = MECHANICAL_DESIGN_GEOMETRIC_PRESENTATION_REPRESENTATION (  '', ( #2104 ), #57220 ) ;
#62424 = CARTESIAN_POINT ( 'NONE',  ( 15.82318872385482145, 4.444012391124124939, -4.874853782843320715 ) ) ;
#62425 = CARTESIAN_POINT ( 'NONE',  ( -13.32558116180121921, 42.77601834456852714, -92.18035469403051252 ) ) ;
#62426 = EDGE_CURVE ( 'NONE', #8963, #84380, #2718, .T. ) ;
#62427 = AXIS2_PLACEMENT_3D ( 'NONE', #33114, #82696, #65979 ) ;
#62428 = CARTESIAN_POINT ( 'NONE',  ( 15.92744018389458915, 3.245174460793482041, -1.809927857062401557 ) ) ;
#62429 = CARTESIAN_POINT ( 'NONE',  ( -43.29658055318886767, 324.1952503670673877, -2.852919881210743913 ) ) ;
#62430 = ORIENTED_EDGE ( 'NONE', *, *, #54812, .T. ) ;
#62431 = CARTESIAN_POINT ( 'NONE',  ( 32.42250183443744760, 438.8720138150355297, 23.74901013937720506 ) ) ;
#62432 = CARTESIAN_POINT ( 'NONE',  ( 44.83349330513380693, -4.000000000000000000, 4.898587196589415787E-16 ) ) ;
#62434 =( NAMED_UNIT ( * ) SI_UNIT ( $, .STERADIAN. ) SOLID_ANGLE_UNIT ( ) );
#62433 = FILL_AREA_STYLE ('',( #29051 ) ) ;
#62435 = CARTESIAN_POINT ( 'NONE',  ( 84.15356149169568312, 1.016364837396684119E-14, 0.000000000000000000 ) ) ;
#62436 = ORIENTED_EDGE ( 'NONE', *, *, #594, .T. ) ;
#62437 = ORIENTED_EDGE ( 'NONE', *, *, #70072, .T. ) ;
#62438 = CARTESIAN_POINT ( 'NONE',  ( -30.59165872538332209, 327.9687303963079330, 15.85230159117361914 ) ) ;
#62439 = ORIENTED_EDGE ( 'NONE', *, *, #49470, .F. ) ;
#62440 = FACE_OUTER_BOUND ( 'NONE', #20639, .T. ) ;
#62441 = DIRECTION ( 'NONE',  ( -1.000000000000000000, 0.000000000000000000, 0.000000000000000000 ) ) ;
#62442 = CARTESIAN_POINT ( 'NONE',  ( 20.59999999999999787, 1.533819458162526451E-15, 0.000000000000000000 ) ) ;
#62443 = ORIENTED_EDGE ( 'NONE', *, *, #76970, .F. ) ;
#62444 = ADVANCED_FACE ( 'NONE', ( #83023 ), #15272, .T. ) ;
#62445 = CARTESIAN_POINT ( 'NONE',  ( -4.205882352941185509, -5.000000000000002665, -72.69916451482998809 ) ) ;
#62446 = CARTESIAN_POINT ( 'NONE',  ( -6.057904167604424295, 41.61856606222242050, -70.65344123333893833 ) ) ;
#62447 = CARTESIAN_POINT ( 'NONE',  ( -89.26291111005475898, -59.99999999997328359, 204.3060666321922270 ) ) ;
#62448 = CARTESIAN_POINT ( 'NONE',  ( 9.999999999999996447, 15.00000000000000000, -10.00000000000000000 ) ) ;
#62449 = CARTESIAN_POINT ( 'NONE',  ( 71.98594699884088755, -60.00000000001919176, -34.35552695216333063 ) ) ;
#62450 = CARTESIAN_POINT ( 'NONE',  ( -3.302423421000036718, -5.000000000000001776, 16.08808873516354510 ) ) ;
#62451 = CARTESIAN_POINT ( 'NONE',  ( -5.663714540180169621, 41.53602265354958689, -58.55436150342320190 ) ) ;
#62453 = CARTESIAN_POINT ( 'NONE',  ( 10.37487025158898568, -49.91581432402574592, 32.22216560970060328 ) ) ;
#62452 = CARTESIAN_POINT ( 'NONE',  ( -99.06514666684596193, -59.99999999999997158, 60.62150588740050949 ) ) ;
#62454 = CARTESIAN_POINT ( 'NONE',  ( 0.000000000000000000, 0.000000000000000000, 0.000000000000000000 ) ) ;
#62455 = CARTESIAN_POINT ( 'NONE',  ( -49.01032723201429064, -39.52037656706556135, 49.15628037481865675 ) ) ;
#62456 = CARTESIAN_POINT ( 'NONE',  ( 5.146599240078983506, -67.41437153544924854, 13.97902347505284837 ) ) ;
#62457 = ORIENTED_EDGE ( 'NONE', *, *, #94030, .T. ) ;
#62458 = CARTESIAN_POINT ( 'NONE',  ( 0.9493808841748633265, 12.66946710488672068, -49.67524744289797667 ) ) ;
#62459 = VECTOR ( 'NONE', #1237, 1000.000000000000000 ) ;
#62460 = SURFACE_SIDE_STYLE ('',( #30639 ) ) ;
#62461 = CARTESIAN_POINT ( 'NONE',  ( 5.856349485908422636, 1.359279156792593701, 6.499999999999999112 ) ) ;
#62462 = ORIENTED_EDGE ( 'NONE', *, *, #54066, .F. ) ;
#62463 = CARTESIAN_POINT ( 'NONE',  ( -5.846241857870205116, -7.705620505147201094, 13.78798924724435615 ) ) ;
#62464 = ORIENTED_EDGE ( 'NONE', *, *, #50800, .F. ) ;
#62465 = CARTESIAN_POINT ( 'NONE',  ( 89.20714034186237029, -30.00000000001022116, -14.16964046280356015 ) ) ;
#62466 = FACE_OUTER_BOUND ( 'NONE', #73055, .T. ) ;
#62467 = CIRCLE ( 'NONE', #34929, 4.000000000000001776 ) ;
#62468 = CARTESIAN_POINT ( 'NONE',  ( -3.158708192431145090, -10.09041393549569499, -11.69019864734867831 ) ) ;
#62469 = CARTESIAN_POINT ( 'NONE',  ( -51.76085035125569789, 42.00000000008225953, 29.83308852628617203 ) ) ;
#62470 = CARTESIAN_POINT ( 'NONE',  ( 95.97260220087535743, -30.00000000000000000, 191.2893859301274802 ) ) ;
#62471 = TOROIDAL_SURFACE ( 'NONE', #46971, 11.18527996897366528, 1.000000000000000000 ) ;
#62472 = DIRECTION ( 'NONE',  ( 0.3893994694821809044, 0.000000000000000000, 0.9210689730780189377 ) ) ;
#62473 = B_SPLINE_CURVE_WITH_KNOTS ( 'NONE', 3,
 ( #79474, #88111, #79997, #14191, #5584, #38509, #30418, #39032, #71914, #22865, #39570, #82116, #2254, #34682, #110, #83711, #9818, #41147, #9287, #49758 ),
 .UNSPECIFIED., .F., .F.,
 ( 4, 2, 2, 2, 2, 2, 2, 2, 2, 4 ),
 ( 0.007119059105098823372, 0.007623191790411408715, 0.008127324475723994926, 0.008379390818380284128, 0.008631457161036575065, 0.009135589846349155205, 0.009639722531661735344, 0.01014385521697431722, 0.01064798790228689736, 0.01115212058759947750 ),
 .UNSPECIFIED. ) ;
#62474 = ORIENTED_EDGE ( 'NONE', *, *, #51829, .F. ) ;
#62475 = ORIENTED_EDGE ( 'NONE', *, *, #65205, .F. ) ;
#62476 = ORIENTED_EDGE ( 'NONE', *, *, #93433, .T. ) ;
#62477 = CARTESIAN_POINT ( 'NONE',  ( 53.90771391880598884, -60.31426852269981254, 66.32011985641655372 ) ) ;
#62478 = CARTESIAN_POINT ( 'NONE',  ( -46.00000000000000000, 436.1583201866848754, 9.603910868008647128 ) ) ;
#62479 = PRESENTATION_LAYER_ASSIGNMENT (  '', '', ( #102109 ) ) ;
#62480 = LINE ( 'NONE', #13364, #85815 ) ;
#62481 = ORIENTED_EDGE ( 'NONE', *, *, #48723, .T. ) ;
#62482 = DIRECTION ( 'NONE',  ( 0.000000000000000000, -1.000000000000000000, 0.000000000000000000 ) ) ;
#62483 = ORIENTED_EDGE ( 'NONE', *, *, #48194, .T. ) ;
#62484 = CARTESIAN_POINT ( 'NONE',  ( -3.601501433546143538E-16, 15.58845726811991206, -13.00000000000000000 ) ) ;
#62485 = CARTESIAN_POINT ( 'NONE',  ( 93.35170594872228378, -38.49489428715083505, 201.1561598503145376 ) ) ;
#62486 = CARTESIAN_POINT ( 'NONE',  ( 11.68473590324837730, 18.93084228341375663, 8.064254821439817533 ) ) ;
#62487 = CARTESIAN_POINT ( 'NONE',  ( 82.55926974371887184, -37.86161494215052414, 6.154721773108606797 ) ) ;
#62488 = CARTESIAN_POINT ( 'NONE',  ( 2.503857664561936320E-16, -8.660254037844401509, -10.00000000000000000 ) ) ;
#62489 = CARTESIAN_POINT ( 'NONE',  ( 42.47229554058168333, 355.2072415732512241, 15.63453588980991427 ) ) ;
#62490 = DIRECTION ( 'NONE',  ( 0.9727555100395927079, 0.000000000000000000, 0.2318333834623737266 ) ) ;
#62491 = CYLINDRICAL_SURFACE ( 'NONE', #37885, 8.000000000000000000 ) ;
#62492 = CARTESIAN_POINT ( 'NONE',  ( 0.000000000000000000, 0.000000000000000000, 65.00000000000000000 ) ) ;
#62493 = DIRECTION ( 'NONE',  ( -0.000000000000000000, -0.000000000000000000, -1.000000000000000000 ) ) ;
#62495 = ORIENTED_EDGE ( 'NONE', *, *, #77774, .F. ) ;
#62494 =( BOUNDED_SURFACE ( )  B_SPLINE_SURFACE ( 3, 2, ( 
 ( #75421, #32867, #90548 ),
 ( #98624, #34481, #97555 ),
 ( #91097, #49003, #15587 ),
 ( #56567, #24252, #50080 ) ),
 .UNSPECIFIED., .F., .F., .F. ) 
 B_SPLINE_SURFACE_WITH_KNOTS ( ( 4, 4 ),
 ( 3, 3 ),
 ( -9.540979117872439019E-18, 0.001771883439666498226 ),
 ( 0.000000000000000000, 1.000000000000000000 ),
 .UNSPECIFIED. ) 
 GEOMETRIC_REPRESENTATION_ITEM ( )  RATIONAL_B_SPLINE_SURFACE ( (
 ( 1.000000000000000000, 0.7699558187665761499, 1.000000000000000000),
 ( 1.000000000000000000, 0.7661160612247130963, 1.000000000000000000),
 ( 1.000000000000000000, 0.7602452393654992591, 1.000000000000000000),
 ( 1.000000000000000000, 0.7533433155455192543, 1.000000000000000000) ) ) 
 REPRESENTATION_ITEM ( '' )  SURFACE ( )  );
#62496 = AXIS2_PLACEMENT_3D ( 'NONE', #41936, #74297, #903 ) ;
#62497 = FACE_OUTER_BOUND ( 'NONE', #80833, .T. ) ;
#62498 = ADVANCED_FACE ( 'NONE', ( #77594 ), #24959, .T. ) ;
#62499 = CARTESIAN_POINT ( 'NONE',  ( 16.00313525666932435, 43.99315673427333451, -88.49932639890887742 ) ) ;
#62500 = COLOUR_RGB ( '', 0.66274510, 0.83137255, 0.94901961) ;
#62501 = CARTESIAN_POINT ( 'NONE',  ( -4.678819457397884740, 143.9212778189118467, 5.000000000000000000 ) ) ;
#62502 = ORIENTED_EDGE ( 'NONE', *, *, #11228, .F. ) ;
#62503 = EDGE_CURVE ( 'NONE', #34393, #91694, #101338, .T. ) ;
#62504 = CARTESIAN_POINT ( 'NONE',  ( -21.14842190820295187, 304.9658827179694072, -8.975750559732306399 ) ) ;
#62505 = CARTESIAN_POINT ( 'NONE',  ( -29.32492077227583493, 297.8361219291210773, 10.59529383611387132 ) ) ;
#62506 = CARTESIAN_POINT ( 'NONE',  ( 0.000000000000000000, 152.0000000000000000, 5.000000000000000000 ) ) ;
#62507 = DIRECTION ( 'NONE',  ( 0.000000000000000000, -1.000000000000000000, 0.000000000000000000 ) ) ;
#62508 = CARTESIAN_POINT ( 'NONE',  ( 3.313708498984762052, -22.71875000000000355, -8.000000000000000000 ) ) ;
#62509 = VECTOR ( 'NONE', #5704, 999.9999999999998863 ) ;
#62510 = CARTESIAN_POINT ( 'NONE',  ( -28.35997571216497803, -31.34280435441244705, 39.68179292875564101 ) ) ;
#62511 = EDGE_CURVE ( 'NONE', #50065, #30636, #40396, .T. ) ;
#62512 = DIRECTION ( 'NONE',  ( -0.000000000000000000, -1.000000000000000000, -0.000000000000000000 ) ) ;
#62513 = AXIS2_PLACEMENT_3D ( 'NONE', #52518, #37980, #3986 ) ;
#62514 = ORIENTED_EDGE ( 'NONE', *, *, #31386, .T. ) ;
#62515 = CARTESIAN_POINT ( 'NONE',  ( 84.23774194945092120, -42.97611175225988234, 182.9332601167417067 ) ) ;
#62516 = CARTESIAN_POINT ( 'NONE',  ( -38.81495481606859244, 27.33043566563091176, 12.09930584269103804 ) ) ;
#62517 = ORIENTED_EDGE ( 'NONE', *, *, #42692, .F. ) ;
#62518 = CARTESIAN_POINT ( 'NONE',  ( 94.19143966283073155, -57.67257289481475624, 22.55042990271367032 ) ) ;
#62519 = ADVANCED_FACE ( 'NONE', ( #28018 ), #104037, .T. ) ;
#62520 = CARTESIAN_POINT ( 'NONE',  ( 0.000000000000000000, -30.00000000000000000, 0.000000000000000000 ) ) ;
#62521 = CARTESIAN_POINT ( 'NONE',  ( -9.290012601901949552, -5.000000000000002665, -75.85638632170552853 ) ) ;
#62522 = DIRECTION ( 'NONE',  ( -0.000000000000000000, -0.000000000000000000, -1.000000000000000000 ) ) ;
#62523 = SURFACE_STYLE_FILL_AREA ( #63046 ) ;
#62524 = DIRECTION ( 'NONE',  ( 0.07722429248628930043, 0.000000000000000000, 0.9970137454669278920 ) ) ;
#62525 = CARTESIAN_POINT ( 'NONE',  ( 8.106211149174814778, -19.49056414931506609, 35.24334571562989282 ) ) ;
#62526 =( LENGTH_UNIT ( ) NAMED_UNIT ( * ) SI_UNIT ( .MILLI., .METRE. ) );
#62527 = CARTESIAN_POINT ( 'NONE',  ( 45.42450008630215308, -28.44167713921813601, 40.52586451359788811 ) ) ;
#62529 = CARTESIAN_POINT ( 'NONE',  ( -14.09102575900082321, 20.97624040389351663, 6.037758616000266088 ) ) ;
#62528 = CARTESIAN_POINT ( 'NONE',  ( 3.616665348617805752E-21, 26.07813853931757464, -38.25000000000000000 ) ) ;
#62530 = CARTESIAN_POINT ( 'NONE',  ( 42.36735105587926142, 487.4262793962163300, 8.281278960740705131 ) ) ;
#62531 = CARTESIAN_POINT ( 'NONE',  ( -15.43026448159015729, 44.08566165821367377, -5.095151619626889783 ) ) ;
#62532 = CARTESIAN_POINT ( 'NONE',  ( 39.44851073818434628, 312.5366107982540598, 2.232686811542719862 ) ) ;
#62533 = CARTESIAN_POINT ( 'NONE',  ( 28.09999999999999787, -3.309499999999999886, 4.475777889183790779E-16 ) ) ;
#62534 = DIRECTION ( 'NONE',  ( -1.000000000000000000, -1.224606353822377258E-16, -0.000000000000000000 ) ) ;
#62535 = AXIS2_PLACEMENT_3D ( 'NONE', #85070, #86683, #12754 ) ;
#62536 = VERTEX_POINT ( 'NONE', #72148 ) ;
#62537 = CARTESIAN_POINT ( 'NONE',  ( -9.803567740517793894, -0.5665513748614124934, 19.98103188536380870 ) ) ;
#62538 = CARTESIAN_POINT ( 'NONE',  ( 0.08224679563971193375, 6.145890662064649845, -5.355005115540897975 ) ) ;
#62539 = MECHANICAL_DESIGN_GEOMETRIC_PRESENTATION_REPRESENTATION (  '', ( #45297 ), #40122 ) ;
#62541 = CARTESIAN_POINT ( 'NONE',  ( -0.001430412024211547310, -34.58958055692348665, -32.65458004663561553 ) ) ;
#62540 =( NAMED_UNIT ( * ) SI_UNIT ( $, .STERADIAN. ) SOLID_ANGLE_UNIT ( ) );
#62542 = EDGE_CURVE ( 'NONE', #94111, #4931, #67968, .T. ) ;
#62543 = ORIENTED_EDGE ( 'NONE', *, *, #100053, .T. ) ;
#62544 = CARTESIAN_POINT ( 'NONE',  ( 0.3306966981844232656, 8.469326210127494647, -7.349897473154332062 ) ) ;
#62545 = DIRECTION ( 'NONE',  ( 1.000000000000000000, 1.224606353822377258E-16, 0.000000000000000000 ) ) ;
#62547 = EDGE_LOOP ( 'NONE', ( #76063, #105216, #106298, #82777 ) ) ;
#62546 =( GEOMETRIC_REPRESENTATION_CONTEXT ( 3 ) GLOBAL_UNCERTAINTY_ASSIGNED_CONTEXT ( ( #92418 ) ) GLOBAL_UNIT_ASSIGNED_CONTEXT ( ( #46940, #79840, #38872 ) ) REPRESENTATION_CONTEXT ( 'NONE', 'WORKASPACE' ) );
#62548 = EDGE_CURVE ( 'NONE', #94131, #81142, #102465, .T. ) ;
#62549 = CARTESIAN_POINT ( 'NONE',  ( 0.000000000000000000, 6.123233995736770227E-16, -5.000000000000002665 ) ) ;
#62550 = CARTESIAN_POINT ( 'NONE',  ( 0.000000000000000000, 0.000000000000000000, 0.000000000000000000 ) ) ;
#62551 = CARTESIAN_POINT ( 'NONE',  ( -92.39013394304011229, -59.99999999999999289, 0.2848972956623299080 ) ) ;
#62552 = EDGE_LOOP ( 'NONE', ( #22742, #37297 ) ) ;
#62553 = DIRECTION ( 'NONE',  ( 0.000000000000000000, -1.000000000000000000, 0.000000000000000000 ) ) ;
#62554 = CARTESIAN_POINT ( 'NONE',  ( 61.85555555555556140, -3.309500000000000774, 0.000000000000000000 ) ) ;
#62555 = CARTESIAN_POINT ( 'NONE',  ( -9.176803346051508825, 29.47052844202562483, 3.973598758023531019 ) ) ;
#62557 = CYLINDRICAL_SURFACE ( 'NONE', #56398, 4.000000000000000000 ) ;
#62556 = DIRECTION ( 'NONE',  ( 1.000000000000000000, 1.224606353822377258E-16, 0.000000000000000000 ) ) ;
#62558 = CARTESIAN_POINT ( 'NONE',  ( -84.34656395696856634, -29.01820936530794626, 165.8801275300401983 ) ) ;
#62559 = VERTEX_POINT ( 'NONE', #22029 ) ;
#62560 = DIRECTION ( 'NONE',  ( -1.000000000000000000, -1.224606353822377258E-16, -0.000000000000000000 ) ) ;
#62561 = ORIENTED_EDGE ( 'NONE', *, *, #72882, .T. ) ;
#62562 = ORIENTED_EDGE ( 'NONE', *, *, #34970, .F. ) ;
#62563 = CARTESIAN_POINT ( 'NONE',  ( 31.12255221142792294, 439.8596962522411786, 23.32261708534639411 ) ) ;
#62564 = AXIS2_PLACEMENT_3D ( 'NONE', #41771, #67656, #33176 ) ;
#62565 = CARTESIAN_POINT ( 'NONE',  ( -1.411247199636991373E-12, 7.746009256445978153, -51.75000000000450484 ) ) ;
#62566 =( LENGTH_UNIT ( ) NAMED_UNIT ( * ) SI_UNIT ( .MILLI., .METRE. ) );
#62567 = ORIENTED_EDGE ( 'NONE', *, *, #38555, .F. ) ;
#62568 = EDGE_CURVE ( 'NONE', #86482, #27869, #94854, .T. ) ;
#62569 =( GEOMETRIC_REPRESENTATION_CONTEXT ( 3 ) GLOBAL_UNCERTAINTY_ASSIGNED_CONTEXT ( ( #84798 ) ) GLOBAL_UNIT_ASSIGNED_CONTEXT ( ( #28863, #21284, #37475 ) ) REPRESENTATION_CONTEXT ( 'NONE', 'WORKASPACE' ) );
#62570 = SURFACE_SIDE_STYLE ('',( #47420 ) ) ;
#62571 = DIRECTION ( 'NONE',  ( 0.000000000000000000, 1.000000000000000000, 0.000000000000000000 ) ) ;
#62572 = CARTESIAN_POINT ( 'NONE',  ( -91.26204144827082132, -57.66323380191850845, -20.53964676755072105 ) ) ;
#62573 = CARTESIAN_POINT ( 'NONE',  ( -10.00233396054510493, 294.6427044336463723, 0.2481344758280235319 ) ) ;
#62574 = DIRECTION ( 'NONE',  ( 0.000000000000000000, 1.000000000000000000, 0.000000000000000000 ) ) ;
#62575 = CIRCLE ( 'NONE', #76331, 5.000000000000000000 ) ;
#62576 = CARTESIAN_POINT ( 'NONE',  ( -9.253500431420432548, 103.7022845008229126, 3.792688295761953210 ) ) ;
#62577 = DIRECTION ( 'NONE',  ( -0.5735764363510461594, 0.8191520442889916875, 1.003171929053524870E-16 ) ) ;
#62578 = DIRECTION ( 'NONE',  ( 1.000000000000000000, 0.000000000000000000, -0.000000000000000000 ) ) ;
#62579 = CARTESIAN_POINT ( 'NONE',  ( 92.19440588371723777, -59.99999999999994316, -19.86251273113072102 ) ) ;
#62580 = EDGE_CURVE ( 'NONE', #84193, #87634, #95904, .T. ) ;
#62581 = CARTESIAN_POINT ( 'NONE',  ( -67.91869938964059372, -14.21045842199436571, 108.3284777829519214 ) ) ;
#62582 = CARTESIAN_POINT ( 'NONE',  ( -53.76999817631660505, -53.37993369322897763, 63.18917586708445810 ) ) ;
#62583 = ORIENTED_EDGE ( 'NONE', *, *, #40677, .T. ) ;
#62584 = DIRECTION ( 'NONE',  ( 0.000000000000000000, 0.000000000000000000, 1.000000000000000000 ) ) ;
#62585 = ORIENTED_EDGE ( 'NONE', *, *, #861, .T. ) ;
#62586 = CARTESIAN_POINT ( 'NONE',  ( -102.5341287361919171, -60.18785315653154555, 193.5342851667064679 ) ) ;
#62587 = EDGE_CURVE ( 'NONE', #34113, #73538, #80227, .T. ) ;
#62588 = CARTESIAN_POINT ( 'NONE',  ( -1.012490096689796948, 51.43211407868803775, 9.751042324627787750 ) ) ;
#62589 = ORIENTED_EDGE ( 'NONE', *, *, #84381, .T. ) ;
#62590 = CARTESIAN_POINT ( 'NONE',  ( 19.24691749296559351, 49.81725912942741985, 61.46328798589317444 ) ) ;
#62591 =( NAMED_UNIT ( * ) SI_UNIT ( $, .STERADIAN. ) SOLID_ANGLE_UNIT ( ) );
#62592 = DIRECTION ( 'NONE',  ( 0.8191520442889881348, 0.000000000000000000, 0.5735764363510513775 ) ) ;
#62593 = CARTESIAN_POINT ( 'NONE',  ( -2.977408999572654480, -12.50000000204838990, 7.188101187499999156 ) ) ;
#62594 = DIRECTION ( 'NONE',  ( 0.2517716543986374678, 0.000000000000000000, 0.9677866676294797355 ) ) ;
#62595 =( LENGTH_UNIT ( ) NAMED_UNIT ( * ) SI_UNIT ( .MILLI., .METRE. ) );
#62596 = CARTESIAN_POINT ( 'NONE',  ( 7.211357414135265209, -82.98853460065558352, 3.467230644691329466 ) ) ;
#62597 = CARTESIAN_POINT ( 'NONE',  ( 62.29946635938797783, -30.00000000000000000, 72.81714634848326284 ) ) ;
#62598 = CARTESIAN_POINT ( 'NONE',  ( -7.850999800289822694, 69.61084308864499803, -0.000000000000000000 ) ) ;
#62599 = CARTESIAN_POINT ( 'NONE',  ( 4.391938347788338248, -48.86119740214457607, 104.3926446507460923 ) ) ;
#62600 = DIRECTION ( 'NONE',  ( -1.000000000000000000, -1.224606353822377258E-16, -0.000000000000000000 ) ) ;
#62601 = CARTESIAN_POINT ( 'NONE',  ( -27.93204256690871645, -25.58061032913567701, 30.03670486279004237 ) ) ;
#62602 = VERTEX_POINT ( 'NONE', #37705 ) ;
#62603 = EDGE_LOOP ( 'NONE', ( #2986, #85612, #76279, #87888 ) ) ;
#62604 = CARTESIAN_POINT ( 'NONE',  ( 48.13035336012885779, -60.27851473694221340, 54.32458513865176286 ) ) ;
#62605 = LINE ( 'NONE', #23218, #62824 ) ;
#62606 = CARTESIAN_POINT ( 'NONE',  ( -5.744562646538028616, 12.99999999999999289, -4.000000000000000000 ) ) ;
#62607 = EDGE_CURVE ( 'NONE', #7097, #15625, #54342, .T. ) ;
#62608 = CARTESIAN_POINT ( 'NONE',  ( -110.8957197956460163, -38.35621571426651144, 177.5099108999381485 ) ) ;
#62609 = EDGE_LOOP ( 'NONE', ( #91418, #23172, #91896, #82074, #31362, #45777 ) ) ;
#62610 = CARTESIAN_POINT ( 'NONE',  ( 91.32895771670399654, -38.39937082712951621, -10.08704785443199192 ) ) ;
#62611 = CARTESIAN_POINT ( 'NONE',  ( 13.72095418692558511, 3.072081172788998504, -6.016902580136559209 ) ) ;
#62612 = DIRECTION ( 'NONE',  ( -1.000000000000000000, -1.224606353822377258E-16, -0.000000000000000000 ) ) ;
#62613 = CARTESIAN_POINT ( 'NONE',  ( 26.08349330513380337, 4.000000000000003553, 0.000000000000000000 ) ) ;
#62614 = SURFACE_STYLE_USAGE ( .BOTH. , #70700 ) ;
#62615 = CARTESIAN_POINT ( 'NONE',  ( 6.478079979052916215, 41.41225025427277728, -70.77206711466079980 ) ) ;
#62616 = CARTESIAN_POINT ( 'NONE',  ( -32.13673779510316564, 435.4387075916259846, 16.27397328763151663 ) ) ;
#62617 = CARTESIAN_POINT ( 'NONE',  ( 21.36650669486618881, 1.474610560812782335E-15, 0.000000000000000000 ) ) ;
#62618 = CARTESIAN_POINT ( 'NONE',  ( 12.50000000000000711, -4.999999999999999112, -78.42624373368740009 ) ) ;
#62619 = CARTESIAN_POINT ( 'NONE',  ( 89.19650734279991866, -59.99999999999997868, 201.7715613159374186 ) ) ;
#62620 = VECTOR ( 'NONE', #24998, 1000.000000000000114 ) ;
#62621 = AXIS2_PLACEMENT_3D ( 'NONE', #2166, #10271, #58845 ) ;
#62622 = CYLINDRICAL_SURFACE ( 'NONE', #78512, 1.250000000000001110 ) ;
#62623 = ORIENTED_EDGE ( 'NONE', *, *, #46210, .F. ) ;
#62624 = CARTESIAN_POINT ( 'NONE',  ( -32.65872443253056190, 299.8117513331611690, -0.8913389630357930749 ) ) ;
#62625 = CARTESIAN_POINT ( 'NONE',  ( 7.151597709147945459, 31.78929265052214603, 3.587174531012141454 ) ) ;
#62626 = EDGE_CURVE ( 'NONE', #52893, #61806, #12831, .T. ) ;
#62627 = CARTESIAN_POINT ( 'NONE',  ( -7.986468734911285949, 26.02686320276919929, 0.5341897780976145871 ) ) ;
#62628 = ORIENTED_EDGE ( 'NONE', *, *, #64374, .T. ) ;
#62630 = CARTESIAN_POINT ( 'NONE',  ( 5.222004380948645164, 7.054286485517851979, -27.51823936837747198 ) ) ;
#62629 = CARTESIAN_POINT ( 'NONE',  ( -106.2913668757043268, -38.35584237662276763, 125.9193867242538403 ) ) ;
#62631 = CARTESIAN_POINT ( 'NONE',  ( 1.469576158976823947E-15, -78.00000000000000000, 15.00000000000000000 ) ) ;
#62632 = DIRECTION ( 'NONE',  ( 0.000000000000000000, -1.000000000000000000, 0.000000000000000000 ) ) ;
#62633 = PRESENTATION_LAYER_ASSIGNMENT (  '', '', ( #7459 ) ) ;
#62634 = CARTESIAN_POINT ( 'NONE',  ( -2.977408999572650039, -14.56250000204838457, -7.188101187500001821 ) ) ;
#62635 = CARTESIAN_POINT ( 'NONE',  ( 5.036189802310915731, -3.000000000000002665, -93.73786388412167980 ) ) ;
#62636 = EDGE_CURVE ( 'NONE', #42319, #88074, #12835, .T. ) ;
#62637 = EDGE_CURVE ( 'NONE', #67806, #70575, #31045, .T. ) ;
#62638 = B_SPLINE_CURVE_WITH_KNOTS ( 'NONE', 3,
 ( #120, #26604, #1184, #643, #98834, #66482, #89710, #24479, #24991, #57314, #17953, #57844, #67565, #34155, #25541, #83199, #58400, #48690, #8242, #33090 ),
 .UNSPECIFIED., .F., .F.,
 ( 4, 2, 2, 2, 2, 2, 2, 2, 2, 4 ),
 ( 0.003302071085094845405, 0.003806141473758820667, 0.004058176668090805045, 0.004310211862422788989, 0.005318352639750726502, 0.005822423028414703064, 0.006074458222746694815, 0.006326493417078686565, 0.006830563805742671801, 0.007334634194406657905 ),
 .UNSPECIFIED. ) ;
#62639 = DIRECTION ( 'NONE',  ( -0.5735764363510494901, -0.8191520442889894671, 0.000000000000000000 ) ) ;
#62640 = EDGE_LOOP ( 'NONE', ( #6458, #65796, #103022, #6217, #9424 ) ) ;
#62641 = CARTESIAN_POINT ( 'NONE',  ( 83.47724775591717616, -35.99455235840694911, 168.8079037484727962 ) ) ;
#62642 = EDGE_CURVE ( 'NONE', #42350, #94131, #46288, .T. ) ;
#62643 = B_SPLINE_CURVE_WITH_KNOTS ( 'NONE', 3,
 ( #30670, #87827, #91982, #60187, #67719, #76322, #60709, #41835, #43446, #93591, #2435, #83889 ),
 .UNSPECIFIED., .F., .F.,
 ( 4, 2, 2, 2, 2, 4 ),
 ( -4.799938976750792050E-05, 0.0004199937929076860850, 0.0008879869755828801109, 0.001823973340933268163, 0.002759959706283656323, 0.003695946071634044483 ),
 .UNSPECIFIED. ) ;
#62644 = CARTESIAN_POINT ( 'NONE',  ( 9.046046032567931050, 14.47514906270266977, -5.777789833161669899E-31 ) ) ;
#62645 = CARTESIAN_POINT ( 'NONE',  ( -35.57915322819296478, 439.9237900209715804, 24.31413808603394955 ) ) ;
#62646 = ORIENTED_EDGE ( 'NONE', *, *, #100665, .F. ) ;
#62647 = CARTESIAN_POINT ( 'NONE',  ( -32.49199191497101680, 312.4199643528780825, -7.743724379035653804 ) ) ;
#62648 = CIRCLE ( 'NONE', #41980, 4.000000000000007105 ) ;
#62649 = ADVANCED_FACE ( 'NONE', ( #70570 ), #49002, .T. ) ;
#62650 = DIRECTION ( 'NONE',  ( -1.000000000000000000, -1.224606353822377258E-16, -0.000000000000000000 ) ) ;
#62651 = SURFACE_SIDE_STYLE ('',( #102571 ) ) ;
#62652 =( NAMED_UNIT ( * ) PLANE_ANGLE_UNIT ( ) SI_UNIT ( $, .RADIAN. ) );
#62653 = DIRECTION ( 'NONE',  ( 0.000000000000000000, -1.000000000000000000, 0.000000000000000000 ) ) ;
#62655 = CARTESIAN_POINT ( 'NONE',  ( 1.128130203593064484, 301.8985493317087503, 9.936162350049338343 ) ) ;
#62654 = AXIS2_PLACEMENT_3D ( 'NONE', #77876, #69785, #3454 ) ;
#62656 = ORIENTED_EDGE ( 'NONE', *, *, #21037, .T. ) ;
#62657 = STYLED_ITEM ( 'NONE', ( #94499 ), #88554 ) ;
#62658 = PRESENTATION_STYLE_ASSIGNMENT (( #70732 ) ) ;
#62659 =( GEOMETRIC_REPRESENTATION_CONTEXT ( 3 ) GLOBAL_UNCERTAINTY_ASSIGNED_CONTEXT ( ( #1718 ) ) GLOBAL_UNIT_ASSIGNED_CONTEXT ( ( #26069, #58380, #8230 ) ) REPRESENTATION_CONTEXT ( 'NONE', 'WORKASPACE' ) );
#62660 = CARTESIAN_POINT ( 'NONE',  ( -78.94292291836882214, -30.00000000000000711, -15.09795832904019264 ) ) ;
#62662 = CARTESIAN_POINT ( 'NONE',  ( -1.000000000000000000, -56.64697988393488259, 6.234486214427730211 ) ) ;
#62661 = SHAPE_REPRESENTATION ( 'hex bolt gradeab_iso_ISO 4014 - M10 x 100 x 26-S', ( #10728 ), #79871 ) ;
#62663 = DIRECTION ( 'NONE',  ( 0.4999999999999996669, 0.000000000000000000, -0.8660254037844390407 ) ) ;
#62664 = CARTESIAN_POINT ( 'NONE',  ( 35.00384615384614762, 1.411358822780289120E-15, 0.000000000000000000 ) ) ;
#62665 = CARTESIAN_POINT ( 'NONE',  ( -5.082755093536326818, -16.71875000204838813, 5.082755093536325042 ) ) ;
#62666 = DIRECTION ( 'NONE',  ( -0.000000000000000000, -0.000000000000000000, 1.000000000000000000 ) ) ;
#62667 = CONTEXT_DEPENDENT_SHAPE_REPRESENTATION ( #87296, #62343 ) ;
#62668 = ORIENTED_EDGE ( 'NONE', *, *, #56279, .T. ) ;
#62669 = DIRECTION ( 'NONE',  ( 0.000000000000000000, 0.000000000000000000, 1.000000000000000000 ) ) ;
#62670 = LINE ( 'NONE', #71789, #46141 ) ;
#62671 = CARTESIAN_POINT ( 'NONE',  ( -8.240610721200784639, 35.73638292219641244, 0.000000000000000000 ) ) ;
#62672 = CARTESIAN_POINT ( 'NONE',  ( -7.141975279401744814, -2.999999999999884537, -70.98863559355044117 ) ) ;
#62673 = CARTESIAN_POINT ( 'NONE',  ( 0.000000000000000000, 0.000000000000000000, -9.974599999999998801 ) ) ;
#62674 = VECTOR ( 'NONE', #51276, 1000.000000000000000 ) ;
#62675 = ORIENTED_EDGE ( 'NONE', *, *, #11209, .T. ) ;
#62676 = DIRECTION ( 'NONE',  ( -1.000000000000000000, 0.000000000000000000, 0.000000000000000000 ) ) ;
#62677 = ORIENTED_EDGE ( 'NONE', *, *, #37179, .F. ) ;
#62678 = EDGE_CURVE ( 'NONE', #20574, #17114, #80039, .T. ) ;
#62679 = DIRECTION ( 'NONE',  ( -0.5735764363510510444, -0.8191520442889883569, 0.000000000000000000 ) ) ;
#62680 = CARTESIAN_POINT ( 'NONE',  ( -3.303250429860502102, -0.7130296830186633184, 103.9470740044716024 ) ) ;
#62681 = CARTESIAN_POINT ( 'NONE',  ( -17.39534200550415122, 36.29816465214055654, 24.14189926133820308 ) ) ;
#62682 = CARTESIAN_POINT ( 'NONE',  ( -109.7084241075396704, -60.00000000000000711, 141.1604396081787627 ) ) ;
#62683 = CARTESIAN_POINT ( 'NONE',  ( 0.000000000000000000, 0.000000000000000000, -8.125150395352576993 ) ) ;
#62684 = VECTOR ( 'NONE', #62679, 1000.000000000000000 ) ;
#62685 = CARTESIAN_POINT ( 'NONE',  ( 0.1306530452038090484, -7.903938623646867612, -2.309976723937607446 ) ) ;
#62686 = DIRECTION ( 'NONE',  ( 1.000000000000000000, 1.224606353822377258E-16, 0.000000000000000000 ) ) ;
#62687 = CARTESIAN_POINT ( 'NONE',  ( 18.00625151213652586, 34.31693948171063369, -23.17957379143527419 ) ) ;
#62688 = CARTESIAN_POINT ( 'NONE',  ( -86.37231359403887154, -18.01014218771245723, 173.0452270788669580 ) ) ;
#62689 = DIRECTION ( 'NONE',  ( 0.000000000000000000, -1.000000000000000000, 0.000000000000000000 ) ) ;
#62690 = AXIS2_PLACEMENT_3D ( 'NONE', #18415, #75011, #44271 ) ;
#62691 = ORIENTED_EDGE ( 'NONE', *, *, #96365, .F. ) ;
#62693 = ADVANCED_FACE ( 'NONE', ( #12312 ), #8274, .F. ) ;
#62692 = CARTESIAN_POINT ( 'NONE',  ( 46.00000000000000000, 450.0000000000002274, 13.20242257375370976 ) ) ;
#62694 = CARTESIAN_POINT ( 'NONE',  ( -33.21102376836597614, 438.9613914113129454, 23.92328486949907074 ) ) ;
#62695 = CARTESIAN_POINT ( 'NONE',  ( -86.14699410518059608, -60.14324746009915401, 13.86886434169398186 ) ) ;
#62696 = CARTESIAN_POINT ( 'NONE',  ( 9.833493305133805151, -4.000000000000000000, 4.898587196589415787E-16 ) ) ;
#62697 = CARTESIAN_POINT ( 'NONE',  ( -3.426421942082409799, 123.5896999595963166, -4.999999999999999112 ) ) ;
#62698 = CARTESIAN_POINT ( 'NONE',  ( 3.591870599023079258, 128.3878650910794192, -5.000000000000000000 ) ) ;
#62699 = DIRECTION ( 'NONE',  ( 0.000000000000000000, 1.000000000000000000, 0.000000000000000000 ) ) ;
#62700 = CARTESIAN_POINT ( 'NONE',  ( -7.754160006593189713, 42.00000000000000711, 59.23741894013591036 ) ) ;
#62701 = CARTESIAN_POINT ( 'NONE',  ( 103.2152402541460248, -59.99999999999995026, 203.2731761476304655 ) ) ;
#62702 = EDGE_CURVE ( 'NONE', #89611, #42044, #68256, .T. ) ;
#62703 = CARTESIAN_POINT ( 'NONE',  ( -99.06514666684596193, -59.99999999999997158, 60.62150588740050949 ) ) ;
#62704 = CARTESIAN_POINT ( 'NONE',  ( -65.47023038585730603, -22.10278188241376895, 78.54803145069421078 ) ) ;
#62705 = ORIENTED_EDGE ( 'NONE', *, *, #57290, .T. ) ;
#62706 = CARTESIAN_POINT ( 'NONE',  ( -60.44716248555326388, 39.42448426419966268, 24.08435288277104291 ) ) ;
#62707 = CARTESIAN_POINT ( 'NONE',  ( 95.58593148621761770, -60.00000000000116529, 204.9903296923171467 ) ) ;
#62708 = ORIENTED_EDGE ( 'NONE', *, *, #94444, .F. ) ;
#62709 = CARTESIAN_POINT ( 'NONE',  ( 13.38090213880806800, -54.26185238422452528, 31.11721482942555994 ) ) ;
#62710 = CARTESIAN_POINT ( 'NONE',  ( 7.188101187500000044, -19.53125000204838457, 0.000000000000000000 ) ) ;
#62711 = EDGE_CURVE ( 'NONE', #51711, #14152, #57013, .T. ) ;
#62712 = CARTESIAN_POINT ( 'NONE',  ( -32.15310320217076878, 439.7024266304582625, 23.94087012106557211 ) ) ;
#62713 = ORIENTED_EDGE ( 'NONE', *, *, #1262, .F. ) ;
#62714 = CARTESIAN_POINT ( 'NONE',  ( 3.352941176470589646, -48.79941684889505638, 104.5794940929807524 ) ) ;
#62715 = ORIENTED_EDGE ( 'NONE', *, *, #47769, .F. ) ;
#62716 = DIRECTION ( 'NONE',  ( 1.000000000000000000, -0.000000000000000000, -0.000000000000000000 ) ) ;
#62717 = DIRECTION ( 'NONE',  ( -0.7071067811865314745, 0.000000000000000000, 0.7071067811865635599 ) ) ;
#62718 = CARTESIAN_POINT ( 'NONE',  ( -92.33664849472602043, -60.00000000000000000, 0.9840071046490757034 ) ) ;
#62719 = CARTESIAN_POINT ( 'NONE',  ( 36.70734217215343165, 381.5765345362427752, 5.207851135035667767 ) ) ;
#62720 = CARTESIAN_POINT ( 'NONE',  ( 4.401442555609581635E-16, -9.781250002048384573, -7.188101187500000044 ) ) ;
#62721 = CARTESIAN_POINT ( 'NONE',  ( 32.15166163075745942, 486.0589784586658197, 5.199393881399715589 ) ) ;
#62722 = CIRCLE ( 'NONE', #24852, 5.000000000000000000 ) ;
#62723 = DIRECTION ( 'NONE',  ( -0.000000000000000000, -0.000000000000000000, -1.000000000000000000 ) ) ;
#62724 = CARTESIAN_POINT ( 'NONE',  ( 2.500000000000000444, -30.00000000000000000, 14.79019945774903810 ) ) ;
#62725 = CARTESIAN_POINT ( 'NONE',  ( 9.999999999999994671, 48.00000000000000000, -83.69100306252322241 ) ) ;
#62726 = CYLINDRICAL_SURFACE ( 'NONE', #79985, 4.000000000000000000 ) ;
#62727 = CARTESIAN_POINT ( 'NONE',  ( -39.43902656928035100, 312.5010541801748900, 2.223703621048137347 ) ) ;
#62728 = CARTESIAN_POINT ( 'NONE',  ( 23.44736835841093026, 303.4251214680779185, -9.876957852573138297 ) ) ;
#62729 = MECHANICAL_DESIGN_GEOMETRIC_PRESENTATION_REPRESENTATION (  '', ( #52387 ), #17924 ) ;
#62730 = ORIENTED_EDGE ( 'NONE', *, *, #79054, .F. ) ;
#62731 = CARTESIAN_POINT ( 'NONE',  ( -8.875886419521037851, 53.84819952152465561, -1.561592776398766258 ) ) ;
#62732 = CARTESIAN_POINT ( 'NONE',  ( -15.33144028279955329, 43.81371552016283033, -89.42275431741276748 ) ) ;
#62733 = CARTESIAN_POINT ( 'NONE',  ( 33.72764780035902277, -49.89708627978800592, 36.63738911784905383 ) ) ;
#62734 = CARTESIAN_POINT ( 'NONE',  ( 17.78317311658683408, 9.642355526980000143E-13, 13.66642973271509831 ) ) ;
#62735 = ORIENTED_EDGE ( 'NONE', *, *, #100383, .T. ) ;
#62736 = CARTESIAN_POINT ( 'NONE',  ( 6.222742520105470021, -3.584500230190543313, 6.791463481567636684 ) ) ;
#62737 = ORIENTED_EDGE ( 'NONE', *, *, #44810, .T. ) ;
#62739 = CARTESIAN_POINT ( 'NONE',  ( -5.500000000000007994, 42.00000000000000000, -68.91429205818155879 ) ) ;
#62738 = DIRECTION ( 'NONE',  ( 1.000000000000000000, 0.000000000000000000, 0.000000000000000000 ) ) ;
#62740 = CARTESIAN_POINT ( 'NONE',  ( 11.89131030317610183, 1.482358050883964840E-15, 0.000000000000000000 ) ) ;
#62741 = CARTESIAN_POINT ( 'NONE',  ( -4.852941176470594975, 11.33333333333377269, -70.80672828634229177 ) ) ;
#62742 =( NAMED_UNIT ( * ) PLANE_ANGLE_UNIT ( ) SI_UNIT ( $, .RADIAN. ) );
#62743 = SURFACE_SIDE_STYLE ('',( #54085 ) ) ;
#62744 = CARTESIAN_POINT ( 'NONE',  ( -49.22356967707574427, 12.91018829711988225, -15.97913688296349832 ) ) ;
#62745 = CARTESIAN_POINT ( 'NONE',  ( -4.969492168108461172, -46.56556601679959329, 42.62409117991908403 ) ) ;
#62746 = VERTEX_POINT ( 'NONE', #64600 ) ;
#62747 = CARTESIAN_POINT ( 'NONE',  ( 91.87505181909152441, -60.00000000000001421, 10.10118637906101213 ) ) ;
#62748 = B_SPLINE_CURVE_WITH_KNOTS ( 'NONE', 3,
 ( #25477, #34101, #99852, #26026, #1676, #34635, #28666, #21113, #53440, #12953, #37285, #5415, #96023, #44286, #93900, #11357, #22148, #95481, #61551, #45358, #13483, #45873 ),
 .UNSPECIFIED., .F., .F.,
 ( 4, 2, 2, 2, 2, 2, 2, 2, 2, 2, 4 ),
 ( 0.003044036087729489436, 0.003548461684534129183, 0.003800674482936449924, 0.004052887281338770666, 0.004557312878143412148, 0.005061738474948054498, 0.005566164071752695980, 0.006070589668557337462, 0.006575015265361978944, 0.006827228063764296216, 0.007079440862166612621 ),
 .UNSPECIFIED. ) ;
#62749 = PRESENTATION_STYLE_ASSIGNMENT (( #65784 ) ) ;
#62750 = CARTESIAN_POINT ( 'NONE',  ( -1.829579891623863134E-15, 10.71892156097790583, -14.93965356295127478 ) ) ;
#62751 = DIRECTION ( 'NONE',  ( -1.000000000000000000, -1.224606353822377258E-16, -0.000000000000000000 ) ) ;
#62752 = CARTESIAN_POINT ( 'NONE',  ( -12.02519846569306239, 10.60060048072689298, -9.714517618948729449 ) ) ;
#62753 = VERTEX_POINT ( 'NONE', #57538 ) ;
#62754 = CARTESIAN_POINT ( 'NONE',  ( -82.30107582774267883, -30.00000000000000000, 147.8409899216399310 ) ) ;
#62755 = ORIENTED_EDGE ( 'NONE', *, *, #59341, .F. ) ;
#62756 = EDGE_CURVE ( 'NONE', #44079, #106075, #29697, .T. ) ;
#62757 = FACE_OUTER_BOUND ( 'NONE', #32051, .T. ) ;
#62758 = CARTESIAN_POINT ( 'NONE',  ( -7.036764705882381676, 40.00000000007575807, -71.06385277390852195 ) ) ;
#62759 = LINE ( 'NONE', #85989, #88430 ) ;
#62760 = CARTESIAN_POINT ( 'NONE',  ( 15.77973964953668862, 22.60063761606701149, -1.998938598334726757 ) ) ;
#62761 = DIRECTION ( 'NONE',  ( 0.000000000000000000, 0.000000000000000000, 1.000000000000000000 ) ) ;
#62762 = CARTESIAN_POINT ( 'NONE',  ( -7.188101187500002709, -30.68750000204839168, 2.977408999572648707 ) ) ;
#62763 = CARTESIAN_POINT ( 'NONE',  ( 57.45015997180046696, 4.000000000000014211, 0.000000000000000000 ) ) ;
#62764 = CARTESIAN_POINT ( 'NONE',  ( 13.86650669486618881, 1.474610560812782335E-15, 0.000000000000000000 ) ) ;
#62765 = FACE_OUTER_BOUND ( 'NONE', #93057, .T. ) ;
#62766 = ADVANCED_FACE ( 'NONE', ( #65656 ), #63484, .T. ) ;
#62767 = ORIENTED_EDGE ( 'NONE', *, *, #58436, .T. ) ;
#62768 = ADVANCED_FACE ( 'NONE', ( #30936 ), #15240, .T. ) ;
#62769 = VECTOR ( 'NONE', #24053, 1000.000000000000114 ) ;
#62770 =( GEOMETRIC_REPRESENTATION_CONTEXT ( 3 ) GLOBAL_UNCERTAINTY_ASSIGNED_CONTEXT ( ( #94528 ) ) GLOBAL_UNIT_ASSIGNED_CONTEXT ( ( #73383, #32444, #65319 ) ) REPRESENTATION_CONTEXT ( 'NONE', 'WORKASPACE' ) );
#62772 = VERTEX_POINT ( 'NONE', #72929 ) ;
#62771 = DIRECTION ( 'NONE',  ( 0.000000000000000000, 0.000000000000000000, 1.000000000000000000 ) ) ;
#62773 = CARTESIAN_POINT ( 'NONE',  ( 76.55139626907627814, -60.31021925763745628, 145.8034420760990315 ) ) ;
#62774 = CYLINDRICAL_SURFACE ( 'NONE', #97044, 1.250000000000001110 ) ;
#62775 = ORIENTED_EDGE ( 'NONE', *, *, #99802, .T. ) ;
#62776 = LINE ( 'NONE', #5581, #72056 ) ;
#62777 = EDGE_CURVE ( 'NONE', #67401, #54018, #30114, .T. ) ;
#62778 = CARTESIAN_POINT ( 'NONE',  ( -2.977408999572650039, -18.68750000204838457, -7.188101187500000933 ) ) ;
#62779 = EDGE_CURVE ( 'NONE', #59786, #17325, #39979, .T. ) ;
#62780 = CARTESIAN_POINT ( 'NONE',  ( -91.62307993511501536, -57.61497437271354727, 204.2871689995596967 ) ) ;
#62781 = CARTESIAN_POINT ( 'NONE',  ( 10.11650669486618881, 1.474610560812782335E-15, 0.000000000000000000 ) ) ;
#62782 = ORIENTED_EDGE ( 'NONE', *, *, #40900, .F. ) ;
#62783 = DIRECTION ( 'NONE',  ( 0.000000000000000000, 0.000000000000000000, 1.000000000000000000 ) ) ;
#62784 = CARTESIAN_POINT ( 'NONE',  ( -9.948181520647858989, 81.13107197239621371, 1.049088206181491012 ) ) ;
#62785 = CARTESIAN_POINT ( 'NONE',  ( 43.86650669486618881, 1.474610560812782335E-15, 0.000000000000000000 ) ) ;
#62786 = CARTESIAN_POINT ( 'NONE',  ( 3.313708498984762052, -12.40625000409676915, -8.000000000000000000 ) ) ;
#62787 = CARTESIAN_POINT ( 'NONE',  ( 8.999999999999996447, -4.000000000000003553, 42.58845726811989607 ) ) ;
#62788 = CARTESIAN_POINT ( 'NONE',  ( -36.62603724863704713, 26.04072037792466787, 11.37877576920930167 ) ) ;
#62789 = CARTESIAN_POINT ( 'NONE',  ( -44.10862079528641999, 485.7176850333842708, 3.977867558419631244 ) ) ;
#62790 = CARTESIAN_POINT ( 'NONE',  ( 5.243676916559595114, 9.267627703000917094, -29.53296413887904848 ) ) ;
#62791 = FACE_OUTER_BOUND ( 'NONE', #51791, .T. ) ;
#62793 = AXIS2_PLACEMENT_3D ( 'NONE', #91575, #50029, #82935 ) ;
#62792 = DIRECTION ( 'NONE',  ( 0.9820818503191364179, -1.040834085586084257E-17, -0.1884548733085492089 ) ) ;
#62794 = CARTESIAN_POINT ( 'NONE',  ( -9.788305016933179559, -12.70835420169926167, 16.98816223485645693 ) ) ;
#62795 = ORIENTED_EDGE ( 'NONE', *, *, #64694, .F. ) ;
#62796 = CARTESIAN_POINT ( 'NONE',  ( -1.607819346471298427, -53.94600928665112605, 40.91329866885064348 ) ) ;
#62797 = CARTESIAN_POINT ( 'NONE',  ( 2.500000000000002665, -30.00000000000000000, -13.00000000000000000 ) ) ;
#62799 = CARTESIAN_POINT ( 'NONE',  ( -3.177804682974228800, 15.40991233412802330, -6.239222125484262804 ) ) ;
#62798 =( BOUNDED_SURFACE ( )  B_SPLINE_SURFACE ( 3, 2, ( 
 ( #84800, #68636, #1735 ),
 ( #67029, #27671, #51354 ),
 ( #83196, #9293, #50293 ),
 ( #2261, #17950, #10362 ),
 ( #1182, #50812, #43276 ),
 ( #34690, #83716, #9825 ),
 ( #76161, #63185, #62662 ),
 ( #61608, #96079, #14069 ),
 ( #4407, #29261, #46463 ),
 ( #79350, #45935, #22210 ),
 ( #78289, #5470, #13544 ),
 ( #61066, #53493, #4947 ),
 ( #55061, #30296, #38393 ),
 ( #104152, #46978, #87991 ),
 ( #70735, #79876, #78815 ),
 ( #87465, #102577, #52958 ) ),
 .UNSPECIFIED., .F., .F., .F. ) 
 B_SPLINE_SURFACE_WITH_KNOTS ( ( 4, 2, 2, 2, 2, 2, 2, 4 ),
 ( 3, 3 ),
 ( -3.089907223421224040E-05, 0.004354571166036939195, 0.008740041404308090955, 0.01751098188085039448, 0.02628192235739269800, 0.03505286283393500152, 0.05259474378701960162, 0.07013662474010420866 ),
 ( 0.000000000000000000, 1.000000000000000000 ),
 .UNSPECIFIED. ) 
 GEOMETRIC_REPRESENTATION_ITEM ( )  RATIONAL_B_SPLINE_SURFACE ( (
 ( 1.000000000000000000, 0.7071067811865475727, 1.000000000000000000),
 ( 1.000000000000000000, 0.7071067811865475727, 1.000000000000000000),
 ( 1.000000000000000000, 0.7071067811865475727, 1.000000000000000000),
 ( 1.000000000000000000, 0.7071067811865475727, 1.000000000000000000),
 ( 1.000000000000000000, 0.7071067811865479058, 1.000000000000000000),
 ( 1.000000000000000000, 0.7071067811865479058, 1.000000000000000000),
 ( 1.000000000000000000, 0.7071067811865475727, 1.000000000000000000),
 ( 1.000000000000000000, 0.7071067811865475727, 1.000000000000000000),
 ( 1.000000000000000000, 0.7071067811865475727, 1.000000000000000000),
 ( 1.000000000000000000, 0.7071067811865475727, 1.000000000000000000),
 ( 1.000000000000000000, 0.7071067811865475727, 1.000000000000000000),
 ( 1.000000000000000000, 0.7071067811865475727, 1.000000000000000000),
 ( 1.000000000000000000, 0.7071067811865475727, 1.000000000000000000),
 ( 1.000000000000000000, 0.7071067811865475727, 1.000000000000000000),
 ( 1.000000000000000000, 0.7071067811865475727, 1.000000000000000000),
 ( 1.000000000000000000, 0.7071067811865475727, 1.000000000000000000) ) ) 
 REPRESENTATION_ITEM ( '' )  SURFACE ( )  );
#62800 = VECTOR ( 'NONE', #42195, 1000.000000000000000 ) ;
#62801 = CARTESIAN_POINT ( 'NONE',  ( -64.65451142056612355, -30.13026884046936971, -31.58747142994624824 ) ) ;
#62802 = CARTESIAN_POINT ( 'NONE',  ( -84.24488595034571858, -30.00000000000000000, 163.2083109249410597 ) ) ;
#62803 = DIRECTION ( 'NONE',  ( 0.000000000000000000, -1.000000000000000000, 0.000000000000000000 ) ) ;
#62804 = AXIS2_PLACEMENT_3D ( 'NONE', #50419, #26738, #1325 ) ;
#62805 = VERTEX_POINT ( 'NONE', #22311 ) ;
#62806 = DIRECTION ( 'NONE',  ( 0.000000000000000000, 0.000000000000000000, 1.000000000000000000 ) ) ;
#62807 = CARTESIAN_POINT ( 'NONE',  ( 91.21542037083939647, -57.61349364694762443, 204.2098944395803812 ) ) ;
#62808 = CARTESIAN_POINT ( 'NONE',  ( 64.94639244015790780, -34.58951604102425392, -23.72275273821461994 ) ) ;
#62809 = ADVANCED_FACE ( 'NONE', ( #64346, #81025, #79446, #7142, #79968 ), #28439, .T. ) ;
#62810 = CARTESIAN_POINT ( 'NONE',  ( -2.055025722541617750, -6.319083845364160013, -5.720331885005381700 ) ) ;
#62811 = DIRECTION ( 'NONE',  ( -1.000000000000000000, 0.000000000000000000, 0.000000000000000000 ) ) ;
#62812 = CARTESIAN_POINT ( 'NONE',  ( -1.224646799147352665E-15, -3.000000000000002665, -75.00000000000001421 ) ) ;
#62813 = CARTESIAN_POINT ( 'NONE',  ( -50.51290784178923587, -59.99999999999999289, 73.09413085601065063 ) ) ;
#62814 = CARTESIAN_POINT ( 'NONE',  ( -0.8808064505792063681, 6.997019658119279839, -5.875704392892937555 ) ) ;
#62815 = FACE_OUTER_BOUND ( 'NONE', #47030, .T. ) ;
#62816 = CARTESIAN_POINT ( 'NONE',  ( -58.90678327790172375, 48.00000000000000000, -28.11551192219426909 ) ) ;
#62817 = CARTESIAN_POINT ( 'NONE',  ( -85.80693792311036816, -39.24834306964363861, 186.3877018209399523 ) ) ;
#62818 = VERTEX_POINT ( 'NONE', #89141 ) ;
#62819 = CARTESIAN_POINT ( 'NONE',  ( 32.60563673599508405, 321.1394446977577672, -5.024823039848338446 ) ) ;
#62820 = CARTESIAN_POINT ( 'NONE',  ( 0.000000000000000000, 304.8518027762758038, -9.000000000000005329 ) ) ;
#62821 = CARTESIAN_POINT ( 'NONE',  ( -6.570528617701141272, 41.93002611759227705, -59.71599440453709917 ) ) ;
#62823 = ADVANCED_FACE ( 'NONE', ( #56746 ), #69754, .T. ) ;
#62822 = CARTESIAN_POINT ( 'NONE',  ( 11.17909359582588102, -4.978490734258791406, -77.11252404932572801 ) ) ;
#62825 = CARTESIAN_POINT ( 'NONE',  ( -21.13173862753238907, 303.9465108651830292, -9.979862028335890756 ) ) ;
#62824 = VECTOR ( 'NONE', #97072, 1000.000000000000000 ) ;
#62826 = CARTESIAN_POINT ( 'NONE',  ( 40.62197427625243762, 488.7236279320703716, 10.90363067260340380 ) ) ;
#62827 = FACE_OUTER_BOUND ( 'NONE', #36875, .T. ) ;
#62828 = CARTESIAN_POINT ( 'NONE',  ( 0.000000000000000000, 0.000000000000000000, 0.000000000000000000 ) ) ;
#62829 = ORIENTED_EDGE ( 'NONE', *, *, #60309, .F. ) ;
#62830 = CARTESIAN_POINT ( 'NONE',  ( 18.48043600567737954, 50.00000000000001421, 61.28289380712539014 ) ) ;
#62831 = CARTESIAN_POINT ( 'NONE',  ( 10.35049317287506732, 16.92759726105998652, 9.911179642419414293 ) ) ;
#62832 = CARTESIAN_POINT ( 'NONE',  ( -12.70248734012553804, -4.285714285715715555, -22.03900363279001340 ) ) ;
#62833 = CARTESIAN_POINT ( 'NONE',  ( -32.95646543402900619, 485.7809766657131831, 5.067016726494650847 ) ) ;
#62834 = CARTESIAN_POINT ( 'NONE',  ( 95.18118770502717041, -60.00000000000013500, -7.509903379402337542 ) ) ;
#62835 = CARTESIAN_POINT ( 'NONE',  ( -79.65920824261152688, -36.03009231341933116, 140.1419517927330389 ) ) ;
#62836 = CIRCLE ( 'NONE', #16312, 7.500000000000000888 ) ;
#62837 = ORIENTED_EDGE ( 'NONE', *, *, #41694, .T. ) ;
#62838 = PLANE ( 'NONE',  #82617 ) ;
#62839 = CARTESIAN_POINT ( 'NONE',  ( -2.216488688100143101, -14.30876692738956812, -12.46553453015538793 ) ) ;
#62840 = CARTESIAN_POINT ( 'NONE',  ( 71.69458925131347371, -57.67877169993052178, 168.9530237613620045 ) ) ;
#62841 = CIRCLE ( 'NONE', #18035, 3.999999999999989786 ) ;
#62842 = MECHANICAL_DESIGN_GEOMETRIC_PRESENTATION_REPRESENTATION (  '', ( #31811 ), #7680 ) ;
#62843 = CARTESIAN_POINT ( 'NONE',  ( 0.000000000000000000, 0.000000000000000000, 4.000000000000000000 ) ) ;
#62844 = UNCERTAINTY_MEASURE_WITH_UNIT (LENGTH_MEASURE( 1.000000000000000082E-05 ), #21511, 'distance_accuracy_value', 'NONE');
#62845 = VECTOR ( 'NONE', #54197, 1000.000000000000000 ) ;
#62846 = CARTESIAN_POINT ( 'NONE',  ( 39.72561652656278852, 309.2274488375438750, -6.620765666067498501 ) ) ;
#62847 = EDGE_CURVE ( 'NONE', #28015, #41783, #93841, .T. ) ;
#62848 = CARTESIAN_POINT ( 'NONE',  ( -30.00000000000000000, 462.0217650461273706, 12.66663979487288572 ) ) ;
#62849 = VERTEX_POINT ( 'NONE', #89675 ) ;
#62850 = AXIS2_PLACEMENT_3D ( 'NONE', #26550, #28141, #44290 ) ;
#62851 = FILL_AREA_STYLE ('',( #54188 ) ) ;
#62852 = CARTESIAN_POINT ( 'NONE',  ( -15.67047892703677192, 36.78599904984204017, 23.70382416292481409 ) ) ;
#62853 = CARTESIAN_POINT ( 'NONE',  ( -7.188101187500001821, -24.50000000204839168, -2.977408999572651371 ) ) ;
#62854 = ORIENTED_EDGE ( 'NONE', *, *, #27391, .T. ) ;
#62855 = CARTESIAN_POINT ( 'NONE',  ( 79.82022815836235452, 5.000000000000023093, 6.123233995736781074E-16 ) ) ;
#62856 = CIRCLE ( 'NONE', #24982, 2.000000000000000000 ) ;
#62858 = EDGE_CURVE ( 'NONE', #4237, #42466, #12897, .T. ) ;
#62857 = CARTESIAN_POINT ( 'NONE',  ( 17.50000000000000711, 2.500000000000000444, 25.00000000000000000 ) ) ;
#62859 = DIRECTION ( 'NONE',  ( 0.000000000000000000, 0.000000000000000000, -1.000000000000000000 ) ) ;
#62860 = CARTESIAN_POINT ( 'NONE',  ( 25.90320363122974001, 37.12824114503998629, 9.160210970361452709 ) ) ;
#62861 = CYLINDRICAL_SURFACE ( 'NONE', #55858, 4.000000000000000888 ) ;
#62862 = CARTESIAN_POINT ( 'NONE',  ( 17.89663725870117972, 43.18032939976320250, -5.550406259236770445 ) ) ;
#62863 = ORIENTED_EDGE ( 'NONE', *, *, #104265, .T. ) ;
#62864 = CARTESIAN_POINT ( 'NONE',  ( -6.075724000949984216, 41.99394325426889196, -59.86320218788793568 ) ) ;
#62866 = CARTESIAN_POINT ( 'NONE',  ( 28.82484700973959946, -60.33570494953415420, 36.38165799802252565 ) ) ;
#62865 = CARTESIAN_POINT ( 'NONE',  ( -57.26243271903199172, -29.99999999999990763, 83.64903429017334702 ) ) ;
#62867 = CARTESIAN_POINT ( 'NONE',  ( 24.46403792248021603, 27.44444016472269610, -32.08006538382090156 ) ) ;
#62868 = VERTEX_POINT ( 'NONE', #5041 ) ;
#62869 = ORIENTED_EDGE ( 'NONE', *, *, #45015, .T. ) ;
#62870 = CARTESIAN_POINT ( 'NONE',  ( -25.05982991920904368, -4.285714285714295357, -3.301565691951521053 ) ) ;
#62871 = CARTESIAN_POINT ( 'NONE',  ( 0.000000000000000000, 0.000000000000000000, 0.000000000000000000 ) ) ;
#62872 = CARTESIAN_POINT ( 'NONE',  ( 7.500000000000006217, 39.99999999999942446, -59.88032989331673406 ) ) ;
#62873 = CARTESIAN_POINT ( 'NONE',  ( 1.637502573363885733E-19, 51.26930509877138320, -10.24999999999999822 ) ) ;
#62874 = CARTESIAN_POINT ( 'NONE',  ( -30.00000000000000000, 489.2902422664049027, 5.500203528953035104 ) ) ;
#62875 = CARTESIAN_POINT ( 'NONE',  ( 67.48317336153286305, -4.000000000000000000, 0.000000000000000000 ) ) ;
#62876 = ORIENTED_EDGE ( 'NONE', *, *, #68521, .T. ) ;
#62877 = CARTESIAN_POINT ( 'NONE',  ( 56.58891463576402003, -29.99999999999996447, 58.99988038729124185 ) ) ;
#62878 = CARTESIAN_POINT ( 'NONE',  ( -12.58912078539690960, 22.90675615147189959, -5.652532877199186068 ) ) ;
#62879 = EDGE_CURVE ( 'NONE', #70947, #93228, #37130, .T. ) ;
#62880 = LINE ( 'NONE', #88211, #22159 ) ;
#62881 = CARTESIAN_POINT ( 'NONE',  ( 81.02036043352956085, -30.00000000000001066, 3.658347682202609974 ) ) ;
#62882 = AXIS2_PLACEMENT_3D ( 'NONE', #82801, #74166, #87325 ) ;
#62883 = CARTESIAN_POINT ( 'NONE',  ( 69.92761780597730592, 4.898587196589294500E-16, -4.000000000000007105 ) ) ;
#62884 = ORIENTED_EDGE ( 'NONE', *, *, #5855, .F. ) ;
#62885 = AXIS2_PLACEMENT_3D ( 'NONE', #79224, #45283, #37210 ) ;
#62886 = ORIENTED_EDGE ( 'NONE', *, *, #43306, .F. ) ;
#62887 = ORIENTED_EDGE ( 'NONE', *, *, #94277, .T. ) ;
#62888 = DIRECTION ( 'NONE',  ( -1.000000000000000000, -1.224606353822377258E-16, -0.000000000000000000 ) ) ;
#62889 = CARTESIAN_POINT ( 'NONE',  ( 94.26467260280679739, -5.000000000000000000, 0.000000000000000000 ) ) ;
#62890 = CARTESIAN_POINT ( 'NONE',  ( 80.00000000000000000, -52.00000000000000000, -21.09707704303352926 ) ) ;
#62891 = CARTESIAN_POINT ( 'NONE',  ( -37.65606885761010147, 426.5576088575361950, 5.696479835041206030 ) ) ;
#62892 = CARTESIAN_POINT ( 'NONE',  ( -0.9330442100817423201, -70.05675763226157926, 13.03100537459360986 ) ) ;
#62893 = CARTESIAN_POINT ( 'NONE',  ( -45.99999999999999289, 485.7126260709432586, -0.7245019728194501685 ) ) ;
#62894 = CARTESIAN_POINT ( 'NONE',  ( 6.562974947121709590, -4.277474787035884241, 6.282829635893500964 ) ) ;
#62895 = VERTEX_POINT ( 'NONE', #40054 ) ;
#62896 = CARTESIAN_POINT ( 'NONE',  ( -1.308996937480702005, 48.00000000000000000, -75.00000000000001421 ) ) ;
#62897 = ORIENTED_EDGE ( 'NONE', *, *, #81900, .F. ) ;
#62898 = CARTESIAN_POINT ( 'NONE',  ( 16.36650669486618881, 1.474610560812782335E-15, 0.000000000000000000 ) ) ;
#62899 = CARTESIAN_POINT ( 'NONE',  ( 51.24056960644092840, -38.33573759255047975, 71.51432244761679158 ) ) ;
#62900 = CARTESIAN_POINT ( 'NONE',  ( -40.22629662632770930, 485.6695299957992233, -4.459425866590305709 ) ) ;
#62901 = CARTESIAN_POINT ( 'NONE',  ( -80.72588694485581584, -60.00000000000002132, 180.8123989976356825 ) ) ;
#62902 = CARTESIAN_POINT ( 'NONE',  ( 62.04802235831051149, -60.33937181082633572, 88.28494246272528301 ) ) ;
#62903 = VERTEX_POINT ( 'NONE', #63281 ) ;
#62904 = CARTESIAN_POINT ( 'NONE',  ( -0.01393140247697588312, -21.31702117966834109, -38.55283400289633278 ) ) ;
#62905 = EDGE_CURVE ( 'NONE', #74471, #2708, #48129, .T. ) ;
#62906 = CARTESIAN_POINT ( 'NONE',  ( -45.81007331173236707, -34.56545578652658435, -36.77482165736895325 ) ) ;
#62907 = DIRECTION ( 'NONE',  ( -1.000000000000000000, 0.000000000000000000, 0.000000000000000000 ) ) ;
#62908 = EDGE_CURVE ( 'NONE', #29102, #26216, #70835, .T. ) ;
#62909 = CARTESIAN_POINT ( 'NONE',  ( -8.559508646656370345, 51.83514083332403999, 1.531152949374564365 ) ) ;
#62910 = AXIS2_PLACEMENT_3D ( 'NONE', #92309, #42709, #58361 ) ;
#62911 = ORIENTED_EDGE ( 'NONE', *, *, #73074, .F. ) ;
#62912 = DIRECTION ( 'NONE',  ( 0.000000000000000000, 0.000000000000000000, -1.000000000000000000 ) ) ;
#62913 = CARTESIAN_POINT ( 'NONE',  ( -2.472961632485875860, -59.99999999999999289, -36.87415311768745596 ) ) ;
#62914 = COLOUR_RGB ( '', 0.31764706, 0.68627451, 0.89019608) ;
#62915 = EDGE_CURVE ( 'NONE', #65538, #45473, #97214, .T. ) ;
#62916 = CARTESIAN_POINT ( 'NONE',  ( 30.00000000000000000, 0.000000000000000000, -11.00000000000000000 ) ) ;
#62917 = AXIS2_PLACEMENT_3D ( 'NONE', #70641, #103535, #103016 ) ;
#62918 = CARTESIAN_POINT ( 'NONE',  ( -5.656854249492381470, -31.25000000409677270, 5.656854249492379694 ) ) ;
#62919 = VECTOR ( 'NONE', #39017, 1000.000000000000000 ) ;
#62920 = CARTESIAN_POINT ( 'NONE',  ( 1.098735407080511761, 7.248058225761106144, -6.326622577871084729 ) ) ;
#62921 = CARTESIAN_POINT ( 'NONE',  ( 86.73331853478092057, -42.79697935687362076, 189.5367378819176167 ) ) ;
#62922 = AXIS2_PLACEMENT_3D ( 'NONE', #102743, #68799, #18668 ) ;
#62923 = DIRECTION ( 'NONE',  ( 0.000000000000000000, -1.000000000000000000, 0.000000000000000000 ) ) ;
#62924 = CARTESIAN_POINT ( 'NONE',  ( -9.550648136318311998, 9.268430070310975211, 4.999999999999841904 ) ) ;
#62925 = FILL_AREA_STYLE_COLOUR ( '', #62007 ) ;
#62926 = FILL_AREA_STYLE ('',( #72583 ) ) ;
#62927 = ORIENTED_EDGE ( 'NONE', *, *, #103232, .F. ) ;
#62928 = CARTESIAN_POINT ( 'NONE',  ( 16.41907560254749399, 35.05515302546547218, -21.84033983347977070 ) ) ;
#62929 = CARTESIAN_POINT ( 'NONE',  ( 34.01866702109263230, 436.1375402535096555, 7.445741394046557105 ) ) ;
#62930 = PRESENTATION_LAYER_ASSIGNMENT (  '', '', ( #74972 ) ) ;
#62931 = CARTESIAN_POINT ( 'NONE',  ( -99.01130425066659768, -30.00000000000000355, 188.8065168094256592 ) ) ;
#62932 = CARTESIAN_POINT ( 'NONE',  ( 40.76111137871845358, -57.69046583023251173, 56.94201171814951579 ) ) ;
#62934 = DIRECTION ( 'NONE',  ( 0.000000000000000000, 1.000000000000000000, 0.000000000000000000 ) ) ;
#62933 = CARTESIAN_POINT ( 'NONE',  ( 10.41054107240687188, 1.482358050883964840E-15, 0.000000000000000000 ) ) ;
#62935 = ADVANCED_FACE ( 'NONE', ( #13640 ), #46554, .T. ) ;
#62936 = CARTESIAN_POINT ( 'NONE',  ( -16.52732684424164944, 43.98685724163156863, -87.77868211029608858 ) ) ;
#62937 = CARTESIAN_POINT ( 'NONE',  ( -19.17751609777260313, 50.00000000000000711, 60.34505262736215059 ) ) ;
#62938 = CARTESIAN_POINT ( 'NONE',  ( -41.46910480218704009, 484.7338956289818270, -3.418960549715579500 ) ) ;
#62939 = CARTESIAN_POINT ( 'NONE',  ( 0.000000000000000000, 24.35682532067546902, -46.94949242731048145 ) ) ;
#62940 = SURFACE_STYLE_FILL_AREA ( #13830 ) ;
#62941 = ORIENTED_EDGE ( 'NONE', *, *, #61290, .F. ) ;
#62942 = FILL_AREA_STYLE ('',( #93717 ) ) ;
#62943 = CARTESIAN_POINT ( 'NONE',  ( -1.232335077818826452, -49.99311995005906084, 101.3399051430503164 ) ) ;
#62944 = CARTESIAN_POINT ( 'NONE',  ( -12.22075746324277468, -25.54981014065818457, 28.19739034840224789 ) ) ;
#62945 = CIRCLE ( 'NONE', #99102, 5.000000000000002665 ) ;
#62948 = EDGE_CURVE ( 'NONE', #102596, #83184, #39004, .T. ) ;
#62947 = FACE_OUTER_BOUND ( 'NONE', #32801, .T. ) ;
#62946 = CARTESIAN_POINT ( 'NONE',  ( -105.5251249205886097, -60.00000000000000000, 154.7757544112112100 ) ) ;
#62949 = ORIENTED_EDGE ( 'NONE', *, *, #89452, .T. ) ;
#62950 = CARTESIAN_POINT ( 'NONE',  ( 26.16605992612153031, 35.04355381026522309, 7.977766528426338155 ) ) ;
#62951 = SURFACE_STYLE_USAGE ( .BOTH. , #69973 ) ;
#62952 = DIRECTION ( 'NONE',  ( 0.000000000000000000, -0.3488521823429531765, 0.9371777605526920851 ) ) ;
#62953 = CARTESIAN_POINT ( 'NONE',  ( 15.89812512823695378, 3.583431000102802244, -3.067165457272547968 ) ) ;
#62954 = CARTESIAN_POINT ( 'NONE',  ( 73.08871575436322132, -60.00000000000000000, 163.2694307510419094 ) ) ;
#62955 = CARTESIAN_POINT ( 'NONE',  ( -1.248908226501082908, 53.88132084694859003, -8.833326452425996678 ) ) ;
#62956 = ORIENTED_EDGE ( 'NONE', *, *, #13511, .T. ) ;
#62957 =( LENGTH_UNIT ( ) NAMED_UNIT ( * ) SI_UNIT ( .MILLI., .METRE. ) );
#62958 =( NAMED_UNIT ( * ) PLANE_ANGLE_UNIT ( ) SI_UNIT ( $, .RADIAN. ) );
#62959 = CARTESIAN_POINT ( 'NONE',  ( 3.757221660946452602, 132.6327945012824898, -5.000000000000000000 ) ) ;
#62960 = ADVANCED_FACE ( 'NONE', ( #88608 ), #93926, .T. ) ;
#62961 = CARTESIAN_POINT ( 'NONE',  ( -5.803898591548312780, -3.468598768277427524, 103.8893302396401879 ) ) ;
#62962 = VERTEX_POINT ( 'NONE', #84 ) ;
#62963 = VECTOR ( 'NONE', #62669, 1000.000000000000000 ) ;
#62964 = EDGE_LOOP ( 'NONE', ( #77731, #90688, #95596, #42864 ) ) ;
#62965 = CARTESIAN_POINT ( 'NONE',  ( -30.82828255813691953, 330.8479429521501629, 16.52448723566699584 ) ) ;
#62966 = ORIENTED_EDGE ( 'NONE', *, *, #92748, .T. ) ;
#62967 = EDGE_CURVE ( 'NONE', #49798, #31749, #15841, .T. ) ;
#62968 = CARTESIAN_POINT ( 'NONE',  ( -41.18667489362677969, 461.2717826764276197, 2.470602812283182015 ) ) ;
#62969 =( NAMED_UNIT ( * ) PLANE_ANGLE_UNIT ( ) SI_UNIT ( $, .RADIAN. ) );
#62970 = VERTEX_POINT ( 'NONE', #83687 ) ;
#62971 = MECHANICAL_DESIGN_GEOMETRIC_PRESENTATION_REPRESENTATION (  '', ( #87083 ), #100829 ) ;
#62972 = CARTESIAN_POINT ( 'NONE',  ( 4.852941176470595863, -3.000000000000002665, -70.80672828634229177 ) ) ;
#62973 = CARTESIAN_POINT ( 'NONE',  ( -6.195804093982627769, 41.59435685013754380, -70.65487364512668478 ) ) ;
#62974 = CARTESIAN_POINT ( 'NONE',  ( -100.2369946233466180, -59.99999999998519229, 204.3298598803837933 ) ) ;
#62975 = CARTESIAN_POINT ( 'NONE',  ( 6.332254158185369519, -2.698766916918251990, -6.500000000000001776 ) ) ;
#62976 = CARTESIAN_POINT ( 'NONE',  ( 55.50171542583959194, -60.00000000000000000, 86.69625062228917045 ) ) ;
#62977 = CARTESIAN_POINT ( 'NONE',  ( 37.06438722625302518, 5.000000000000003553, 0.000000000000000000 ) ) ;
#62978 = DIRECTION ( 'NONE',  ( 0.000000000000000000, -1.000000000000000000, 0.000000000000000000 ) ) ;
#62979 = TOROIDAL_SURFACE ( 'NONE', #76731, 11.00000000000000000, 1.000000000000000000 ) ;
#62981 = CARTESIAN_POINT ( 'NONE',  ( 12.62289470629085919, -56.87776700476601377, 33.43110291409266921 ) ) ;
#62980 = CARTESIAN_POINT ( 'NONE',  ( -102.0721909215208427, -14.21045842199424314, 125.2231725879975954 ) ) ;
#62982 = ADVANCED_FACE ( 'NONE', ( #50264 ), #18180, .T. ) ;
#62983 = DIRECTION ( 'NONE',  ( -0.000000000000000000, -0.000000000000000000, -1.000000000000000000 ) ) ;
#62984 = CARTESIAN_POINT ( 'NONE',  ( -48.95940874045572144, -42.98222722188957334, 50.18422616547311321 ) ) ;
#62985 = CARTESIAN_POINT ( 'NONE',  ( -6.786616733794231138, 41.72678875807561383, -59.11526074045958268 ) ) ;
#62986 = ORIENTED_EDGE ( 'NONE', *, *, #4946, .T. ) ;
#62987 = ADVANCED_FACE ( 'NONE', ( #99328 ), #29748, .T. ) ;
#62988 = CONICAL_SURFACE ( 'NONE', #102556, 3.309500000000001663, 0.9599310885968770357 ) ;
#62989 = CARTESIAN_POINT ( 'NONE',  ( 38.51502786939645517, 460.0233756673477501, 2.043034587343977027 ) ) ;
#62990 = AXIS2_PLACEMENT_3D ( 'NONE', #23305, #95066, #104187 ) ;
#62991 = DIRECTION ( 'NONE',  ( 1.000000000000000000, 0.000000000000000000, 0.000000000000000000 ) ) ;
#62992 = CARTESIAN_POINT ( 'NONE',  ( -5.290067270632269114, -1.200000000000000030E-05, -7.281152949374520844 ) ) ;
#62993 = EDGE_LOOP ( 'NONE', ( #50096, #69655, #36073, #78248, #41888 ) ) ;
#62994 = CARTESIAN_POINT ( 'NONE',  ( -8.016921032071788744, -5.439319868627221943, 14.17797645233462056 ) ) ;
#62995 = STYLED_ITEM ( 'NONE', ( #101992 ), #86700 ) ;
#62996 = ORIENTED_EDGE ( 'NONE', *, *, #3064, .T. ) ;
#62997 = CARTESIAN_POINT ( 'NONE',  ( 85.58605083099615740, -29.99999999999847944, 197.5044427888071823 ) ) ;
#62998 = LINE ( 'NONE', #14409, #9448 ) ;
#62999 = CARTESIAN_POINT ( 'NONE',  ( 6.338673411933466006, 41.81695763293575396, -59.02782193812689115 ) ) ;
#63000 = VECTOR ( 'NONE', #50292, 1000.000000000000000 ) ;
#63001 =( NAMED_UNIT ( * ) PLANE_ANGLE_UNIT ( ) SI_UNIT ( $, .RADIAN. ) );
#63002 = CARTESIAN_POINT ( 'NONE',  ( 97.25576257169278449, -30.00000000000000000, 190.9957396260108169 ) ) ;
#63003 = DIRECTION ( 'NONE',  ( 0.000000000000000000, 1.000000000000000000, -0.000000000000000000 ) ) ;
#63004 = VERTEX_POINT ( 'NONE', #9793 ) ;
#63005 = ORIENTED_EDGE ( 'NONE', *, *, #8807, .F. ) ;
#63006 = ORIENTED_EDGE ( 'NONE', *, *, #105521, .T. ) ;
#63007 = FACE_OUTER_BOUND ( 'NONE', #78173, .T. ) ;
#63008 = CARTESIAN_POINT ( 'NONE',  ( -46.00000000000000000, 436.1502960164518754, 10.01001013570486364 ) ) ;
#63009 = CARTESIAN_POINT ( 'NONE',  ( 6.624059643703564149, 294.7379298340728724, -10.02420444108935271 ) ) ;
#63010 = VERTEX_POINT ( 'NONE', #41648 ) ;
#63011 = CARTESIAN_POINT ( 'NONE',  ( -82.90940669858844103, -38.35712835889985683, -24.56897092220943080 ) ) ;
#63012 = EDGE_LOOP ( 'NONE', ( #43398, #68231, #76938, #81195, #38569 ) ) ;
#63013 = DIRECTION ( 'NONE',  ( 0.5735764363510466035, -0.8191520442889914655, 1.003171929053524500E-16 ) ) ;
#63014 = CARTESIAN_POINT ( 'NONE',  ( 105.2245759065473862, -38.38978177102808331, 197.2557521603409043 ) ) ;
#63015 = CARTESIAN_POINT ( 'NONE',  ( 13.39710689387089460, 7.823780487645683124, 8.560214244964429398 ) ) ;
#63016 = CARTESIAN_POINT ( 'NONE',  ( 86.30570207415318862, -60.13085251795755681, 5.317764354392895854 ) ) ;
#63017 = CARTESIAN_POINT ( 'NONE',  ( -52.56483885390523625, -79.93083296558610584, -38.23529411764706509 ) ) ;
#63018 = CARTESIAN_POINT ( 'NONE',  ( 32.85498697112881672, 354.4200440325224690, 21.54103032174089805 ) ) ;
#63019 = FACE_OUTER_BOUND ( 'NONE', #54345, .T. ) ;
#63020 = FACE_OUTER_BOUND ( 'NONE', #79931, .T. ) ;
#63021 = CONICAL_SURFACE ( 'NONE', #94046, 4.000000000000001776, 0.9599310885968808105 ) ;
#63022 = FACE_OUTER_BOUND ( 'NONE', #30876, .T. ) ;
#63023 = CARTESIAN_POINT ( 'NONE',  ( 0.000000000000000000, 0.000000000000000000, -6.235812796514431433 ) ) ;
#63024 = VERTEX_POINT ( 'NONE', #67529 ) ;
#63025 = EDGE_CURVE ( 'NONE', #60365, #22876, #95617, .T. ) ;
#63026 = SURFACE_SIDE_STYLE ('',( #4255 ) ) ;
#63027 = CARTESIAN_POINT ( 'NONE',  ( -35.61279199273527496, 462.7776672770684172, 4.031031541873562496 ) ) ;
#63028 = CARTESIAN_POINT ( 'NONE',  ( -26.35516898678989151, 36.89168544900753943, 9.819666744838436045 ) ) ;
#63029 = ORIENTED_EDGE ( 'NONE', *, *, #35342, .T. ) ;
#63030 = CARTESIAN_POINT ( 'NONE',  ( -35.44793164930461415, 372.9548512003073597, 5.074121509499998517 ) ) ;
#63031 = CARTESIAN_POINT ( 'NONE',  ( -32.72936687177245574, 300.2420673382501946, 3.148605481384946891 ) ) ;
#63032 = CARTESIAN_POINT ( 'NONE',  ( -3.510275272315380057, -48.85091879836223683, 104.5952116206504456 ) ) ;
#63033 = CARTESIAN_POINT ( 'NONE',  ( 3.313708498984762052, -12.21874999999999467, -8.000000000000000000 ) ) ;
#63034 = CARTESIAN_POINT ( 'NONE',  ( -44.64961496624998460, -29.90790381629714290, 54.34366819126163506 ) ) ;
#63035 = ADVANCED_FACE ( 'NONE', ( #65924 ), #87011, .T. ) ;
#63036 = CARTESIAN_POINT ( 'NONE',  ( -9.165151389911699198, 249.9999999999999432, 4.000000000000002665 ) ) ;
#63037 = VERTEX_POINT ( 'NONE', #24956 ) ;
#63038 = CARTESIAN_POINT ( 'NONE',  ( 85.33851620155638784, -39.31096730626728686, 184.9291323951870822 ) ) ;
#63039 = CARTESIAN_POINT ( 'NONE',  ( -48.98802391561670078, 7.953645742798949314, 16.40821160912093291 ) ) ;
#63040 = CIRCLE ( 'NONE', #13040, 5.000000000000002665 ) ;
#63041 = CARTESIAN_POINT ( 'NONE',  ( 23.58349330513380337, -7.703719777548943412E-31, 4.000000000000001776 ) ) ;
#63042 = ORIENTED_EDGE ( 'NONE', *, *, #55310, .F. ) ;
#63043 = CARTESIAN_POINT ( 'NONE',  ( 94.12096428010207205, -57.67269879928694820, 21.37994873513087057 ) ) ;
#63044 = DIRECTION ( 'NONE',  ( -1.000000000000000000, -1.224606353822377258E-16, -0.000000000000000000 ) ) ;
#63045 = CARTESIAN_POINT ( 'NONE',  ( -12.50000000000000355, -3.000000000000001776, -76.70872284621019332 ) ) ;
#63046 = FILL_AREA_STYLE ('',( #5853 ) ) ;
#63047 = ADVANCED_FACE ( 'NONE', ( #41118 ), #57275, .F. ) ;
#63048 = COLOUR_RGB ( '', 0.72549020, 0.75294118, 0.79215686) ;
#63049 = DIRECTION ( 'NONE',  ( 0.000000000000000000, -1.000000000000000000, 0.000000000000000000 ) ) ;
#63050 = CARTESIAN_POINT ( 'NONE',  ( 19.00000000000001421, -4.999999999999999112, -1.500000000000001332 ) ) ;
#63051 = CARTESIAN_POINT ( 'NONE',  ( 49.55824609672842485, -29.60162563601594599, 45.91477733028057173 ) ) ;
#63053 = CARTESIAN_POINT ( 'NONE',  ( -7.665950860465550857E-14, -1.200000000000000030E-05, -40.75000000000000000 ) ) ;
#63052 = SURFACE_STYLE_USAGE ( .BOTH. , #30167 ) ;
#63054 = EDGE_CURVE ( 'NONE', #1, #104211, #99098, .T. ) ;
#63055 = CARTESIAN_POINT ( 'NONE',  ( 8.019147853953672467, 302.4786514485326165, -10.03165473704643595 ) ) ;
#63056 = COLOUR_RGB ( '', 0.66274510, 0.83137255, 0.94901961) ;
#63057 = CARTESIAN_POINT ( 'NONE',  ( 4.699999999999999289, 0.000000000000000000, 0.000000000000000000 ) ) ;
#63058 = DIRECTION ( 'NONE',  ( 0.000000000000000000, -1.000000000000000000, 0.000000000000000000 ) ) ;
#63059 = CARTESIAN_POINT ( 'NONE',  ( -6.177150199754209758, 12.02207793746705455, -13.00000000000000888 ) ) ;
#63060 = AXIS2_PLACEMENT_3D ( 'NONE', #70699, #95498, #21641 ) ;
#63061 = COLOUR_RGB ( '', 0.72549020, 0.75294118, 0.79215686) ;
#63062 = AXIS2_PLACEMENT_3D ( 'NONE', #99401, #25585, #58444 ) ;
#63063 = CARTESIAN_POINT ( 'NONE',  ( -93.54323754964579507, -37.99999999999998579, 99.16270155519150364 ) ) ;
#63064 = PRODUCT_DEFINITION_SHAPE ( 'NONE', 'NONE',  #106795 ) ;
#63065 = ORIENTED_EDGE ( 'NONE', *, *, #74282, .T. ) ;
#63066 = CARTESIAN_POINT ( 'NONE',  ( -9.057198557144582551, -0.3318150627287249632, 19.72202478657212765 ) ) ;
#63067 = COLOUR_RGB ( '', 0.40784314, 0.44705882, 0.49803922) ;
#63068 = CARTESIAN_POINT ( 'NONE',  ( 5.647817967127100047, -61.54873593471205595, -2.038183545141173614 ) ) ;
#63071 = EDGE_CURVE ( 'NONE', #32259, #18153, #69825, .T. ) ;
#63070 = CARTESIAN_POINT ( 'NONE',  ( -34.70505231949518077, -34.58949826982289011, -30.29862454714900011 ) ) ;
#63069 = CARTESIAN_POINT ( 'NONE',  ( 1.227754105814700372E-15, 67.05096163904791240, 10.02537308446411402 ) ) ;
#63072 = EDGE_LOOP ( 'NONE', ( #43796, #3413 ) ) ;
#63073 = CARTESIAN_POINT ( 'NONE',  ( 7.777900015783949961, 4.169681370001524279, -7.928862157988302073 ) ) ;
#63074 = ORIENTED_EDGE ( 'NONE', *, *, #4634, .F. ) ;
#63075 = CARTESIAN_POINT ( 'NONE',  ( 0.000000000000000000, 47.77514352166374323, 0.000000000000000000 ) ) ;
#63076 = DIRECTION ( 'NONE',  ( 1.000000000000000000, -0.000000000000000000, -0.000000000000000000 ) ) ;
#63077 = CARTESIAN_POINT ( 'NONE',  ( -91.70092392707927331, -60.00000000000000711, -15.05504486430357325 ) ) ;
#63078 = VERTEX_POINT ( 'NONE', #10330 ) ;
#63079 = CARTESIAN_POINT ( 'NONE',  ( -8.245342207438692839, 41.99999999999999289, -58.66077168407692710 ) ) ;
#63080 = CARTESIAN_POINT ( 'NONE',  ( -9.380169522195149767, 15.95824666716552365, 3.484756791224360661 ) ) ;
#63081 = FACE_OUTER_BOUND ( 'NONE', #55822, .T. ) ;
#63083 = DIRECTION ( 'NONE',  ( 0.000000000000000000, 0.000000000000000000, 1.000000000000000000 ) ) ;
#63082 = LINE ( 'NONE', #37246, #21666 ) ;
#63084 = AXIS2_PLACEMENT_3D ( 'NONE', #4704, #21966, #103391 ) ;
#63085 = CARTESIAN_POINT ( 'NONE',  ( -83.69471021262442889, -29.06694036840339734, 159.7615962780223811 ) ) ;
#63086 = ORIENTED_EDGE ( 'NONE', *, *, #72149, .F. ) ;
#63087 = CARTESIAN_POINT ( 'NONE',  ( -16.14659623658557308, 0.000000000000000000, 5.483224646664452528 ) ) ;
#63088 = ORIENTED_EDGE ( 'NONE', *, *, #72763, .T. ) ;
#63089 = VECTOR ( 'NONE', #65490, 1000.000000000000000 ) ;
#63090 = ORIENTED_EDGE ( 'NONE', *, *, #66231, .T. ) ;
#63091 = CARTESIAN_POINT ( 'NONE',  ( 41.96713667498180911, 484.5369099524149874, -2.773154793583016531 ) ) ;
#63092 = EDGE_CURVE ( 'NONE', #39124, #33725, #45379, .T. ) ;
#63093 = CARTESIAN_POINT ( 'NONE',  ( 6.125000000000000000, -60.71953810597977252, 14.41094225130411033 ) ) ;
#63094 = ORIENTED_EDGE ( 'NONE', *, *, #41183, .T. ) ;
#63095 = FACE_OUTER_BOUND ( 'NONE', #78114, .T. ) ;
#63096 = CARTESIAN_POINT ( 'NONE',  ( 0.000000000000000000, 0.000000000000000000, 0.000000000000000000 ) ) ;
#63097 = CARTESIAN_POINT ( 'NONE',  ( -81.37675186042847031, -57.51598868027654987, 200.0426579070166895 ) ) ;
#63098 = CARTESIAN_POINT ( 'NONE',  ( 1.112434445721927290, -50.00000000000002132, 101.1533620683574952 ) ) ;
#63099 = CARTESIAN_POINT ( 'NONE',  ( 1.127757440534756794, 7.231345287187100013, -6.344532336093711145 ) ) ;
#63100 = CARTESIAN_POINT ( 'NONE',  ( -13.50929957260945535, -52.70262457293414826, 23.32445699588452470 ) ) ;
#63101 = DIRECTION ( 'NONE',  ( 0.000000000000000000, 1.224646799147353454E-16, 1.000000000000000000 ) ) ;
#63102 = CARTESIAN_POINT ( 'NONE',  ( 84.89432107329884047, -60.00000000000002132, -27.59204247542200505 ) ) ;
#63103 = EDGE_CURVE ( 'NONE', #83331, #31200, #43952, .T. ) ;
#63104 = CARTESIAN_POINT ( 'NONE',  ( -74.04808884210443409, -14.21045842199433018, 133.5060932470338741 ) ) ;
#63105 = CARTESIAN_POINT ( 'NONE',  ( -54.51511722965400253, -46.44099520825000127, 62.03887026768623514 ) ) ;
#63106 = VERTEX_POINT ( 'NONE', #84235 ) ;
#63107 = CARTESIAN_POINT ( 'NONE',  ( 42.57704743493908950, 486.1612337113410263, 7.852296464539637810 ) ) ;
#63108 = ORIENTED_EDGE ( 'NONE', *, *, #18140, .F. ) ;
#63109 = CARTESIAN_POINT ( 'NONE',  ( -99.29800454330434434, -37.79210113977332952, 191.5838778425412841 ) ) ;
#63110 = DIRECTION ( 'NONE',  ( -0.000000000000000000, 1.000000000000000000, -0.000000000000000000 ) ) ;
#63111 = VERTEX_POINT ( 'NONE', #2230 ) ;
#63112 = CARTESIAN_POINT ( 'NONE',  ( 18.92698369676902814, 49.06730440414835925, 62.10640571433232537 ) ) ;
#63113 = AXIS2_PLACEMENT_3D ( 'NONE', #38515, #31726, #64613 ) ;
#63114 = CARTESIAN_POINT ( 'NONE',  ( 91.46570115715213944, -38.37904828772288823, -5.692861098220960869 ) ) ;
#63115 = DIRECTION ( 'NONE',  ( -1.000000000000000000, -1.224606353822377258E-16, -0.000000000000000000 ) ) ;
#63116 = CARTESIAN_POINT ( 'NONE',  ( -7.188101187500001821, -9.875000002048386349, -2.977408999572651371 ) ) ;
#63117 = EDGE_CURVE ( 'NONE', #2494, #98655, #105987, .T. ) ;
#63118 = SURFACE_STYLE_FILL_AREA ( #89515 ) ;
#63119 = SURFACE_STYLE_USAGE ( .BOTH. , #53437 ) ;
#63120 = CARTESIAN_POINT ( 'NONE',  ( 32.22120753352783140, 464.6691781026584636, 10.60621122532586291 ) ) ;
#63121 =( BOUNDED_SURFACE ( )  B_SPLINE_SURFACE ( 3, 2, ( 
 ( #16820, #1126, #82611 ),
 ( #8715, #26025, #99850 ),
 ( #41622, #50238, #9237 ),
 ( #15746, #49159, #24929 ) ),
 .UNSPECIFIED., .F., .F., .F. ) 
 B_SPLINE_SURFACE_WITH_KNOTS ( ( 4, 4 ),
 ( 3, 3 ),
 ( -5.282232984349377602E-16, 0.0002932702099348026580 ),
 ( 0.000000000000000000, 1.000000000000000000 ),
 .UNSPECIFIED. ) 
 GEOMETRIC_REPRESENTATION_ITEM ( )  RATIONAL_B_SPLINE_SURFACE ( (
 ( 1.000000000000000000, 0.7964893136846440402, 1.000000000000000000),
 ( 1.000000000000000000, 0.7948324867097400492, 1.000000000000000000),
 ( 1.000000000000000000, 0.7930891386530558584, 1.000000000000000000),
 ( 1.000000000000000000, 0.7912633096140525568, 1.000000000000000000) ) ) 
 REPRESENTATION_ITEM ( '' )  SURFACE ( )  );
#63122 = CARTESIAN_POINT ( 'NONE',  ( -8.154214789436208477, 112.0280654573990802, -7.222237291452134449E-31 ) ) ;
#63123 = CARTESIAN_POINT ( 'NONE',  ( -0.08420089935654326285, 35.08181111624585213, 27.25000000000000355 ) ) ;
#63124 = CIRCLE ( 'NONE', #71498, 4.172000000000009479 ) ;
#63125 = DIRECTION ( 'NONE',  ( -0.000000000000000000, -0.000000000000000000, 1.000000000000000000 ) ) ;
#63126 = UNCERTAINTY_MEASURE_WITH_UNIT (LENGTH_MEASURE( 1.000000000000000082E-05 ), #1729, 'distance_accuracy_value', 'NONE');
#63127 = CARTESIAN_POINT ( 'NONE',  ( -27.18296926593496110, -36.00581825497734911, 31.66575979565292087 ) ) ;
#63128 = ORIENTED_EDGE ( 'NONE', *, *, #94713, .T. ) ;
#63129 = ORIENTED_EDGE ( 'NONE', *, *, #32887, .F. ) ;
#63130 = CARTESIAN_POINT ( 'NONE',  ( 47.66081387494537580, -46.44007846935294026, 49.24185928217620756 ) ) ;
#63131 = CONICAL_SURFACE ( 'NONE', #18340, 3.309500000000001663, 0.9599310885968770357 ) ;
#63132 = DIRECTION ( 'NONE',  ( 0.000000000000000000, 0.000000000000000000, 1.000000000000000000 ) ) ;
#63133 = CARTESIAN_POINT ( 'NONE',  ( 27.33349330513380337, 1.593028355512270567E-15, 0.000000000000000000 ) ) ;
#63134 = CARTESIAN_POINT ( 'NONE',  ( -110.8469737611757324, -38.35618416066114378, 166.6374178958760410 ) ) ;
#63135 = MECHANICAL_DESIGN_GEOMETRIC_PRESENTATION_REPRESENTATION (  '', ( #51021 ), #76906 ) ;
#63136 = ORIENTED_EDGE ( 'NONE', *, *, #30933, .T. ) ;
#63137 = CARTESIAN_POINT ( 'NONE',  ( 91.27230094422854734, -38.36276317364043109, -1.771946917198911731 ) ) ;
#63138 = CARTESIAN_POINT ( 'NONE',  ( 11.51042249250562399, 12.50642680738181944, -10.00378701082364152 ) ) ;
#63139 = CARTESIAN_POINT ( 'NONE',  ( 18.00000000000000355, 12.99999999999999289, 7.500000000000000000 ) ) ;
#63141 = CARTESIAN_POINT ( 'NONE',  ( 10.83537542021312383, 43.83140336798144432, 13.03201732437568161 ) ) ;
#63140 = AXIS2_PLACEMENT_3D ( 'NONE', #38620, #21387, #71483 ) ;
#63142 = CONICAL_SURFACE ( 'NONE', #26982, 5.000000000000001776, 0.9599310885968803664 ) ;
#63143 = DIRECTION ( 'NONE',  ( -0.000000000000000000, 1.000000000000000000, -0.000000000000000000 ) ) ;
#63144 = CARTESIAN_POINT ( 'NONE',  ( -32.48517913958589531, 435.0118361155008415, 18.08961438120518039 ) ) ;
#63145 = CARTESIAN_POINT ( 'NONE',  ( -36.66354163798878574, 432.5726246612500177, 4.913532023235378077 ) ) ;
#63146 = CARTESIAN_POINT ( 'NONE',  ( -31.31921715863741085, 437.4259532257088949, 20.46640379489214823 ) ) ;
#63147 = CARTESIAN_POINT ( 'NONE',  ( 12.50000000000000711, -3.000000000000000000, -80.60844091781802945 ) ) ;
#63148 = CARTESIAN_POINT ( 'NONE',  ( 81.71125754684067033, -59.99999999999998579, 197.8273229994767064 ) ) ;
#63149 = VECTOR ( 'NONE', #45469, 1000.000000000000000 ) ;
#63150 = CIRCLE ( 'NONE', #42494, 61.50000000000000000 ) ;
#63151 = DIRECTION ( 'NONE',  ( 0.000000000000000000, -1.000000000000000000, 0.000000000000000000 ) ) ;
#63152 = ORIENTED_EDGE ( 'NONE', *, *, #97789, .F. ) ;
#63153 = CARTESIAN_POINT ( 'NONE',  ( 58.43184352567574535, -49.90951488237450206, 72.98920087071743978 ) ) ;
#63154 = CARTESIAN_POINT ( 'NONE',  ( -34.81025666956482922, 301.2271517761568020, -8.565222899818694557 ) ) ;
#63155 = EDGE_CURVE ( 'NONE', #79845, #82202, #73181, .T. ) ;
#63156 = DIRECTION ( 'NONE',  ( -1.000000000000000000, -1.224606353822377258E-16, -0.000000000000000000 ) ) ;
#63157 = DIRECTION ( 'NONE',  ( 0.000000000000000000, -1.000000000000000000, 0.000000000000000000 ) ) ;
#63158 = ORIENTED_EDGE ( 'NONE', *, *, #37057, .T. ) ;
#63160 = DIRECTION ( 'NONE',  ( 0.000000000000000000, 0.000000000000000000, 1.000000000000000000 ) ) ;
#63159 = CARTESIAN_POINT ( 'NONE',  ( -106.9302167770077432, -38.36496539244966186, 194.9700385483175467 ) ) ;
#63161 = CARTESIAN_POINT ( 'NONE',  ( 19.83349330513380693, 1.593028355512270962E-15, 0.000000000000000000 ) ) ;
#63162 =( NAMED_UNIT ( * ) SI_UNIT ( $, .STERADIAN. ) SOLID_ANGLE_UNIT ( ) );
#63163 = CARTESIAN_POINT ( 'NONE',  ( -1.469576158976823947E-15, -30.87499999999999645, 8.000000000000000000 ) ) ;
#63164 = CARTESIAN_POINT ( 'NONE',  ( 1.308996937483426715, -3.000000000000002665, -75.00000000000001421 ) ) ;
#63165 = EDGE_CURVE ( 'NONE', #53206, #3401, #59987, .T. ) ;
#63166 = PRODUCT ( '8. Bar', '8. Bar', '', ( #88649 ) ) ;
#63167 = DIRECTION ( 'NONE',  ( -1.000000000000000000, -1.224606353822377258E-16, -0.000000000000000000 ) ) ;
#63169 = VERTEX_POINT ( 'NONE', #44853 ) ;
#63168 = CARTESIAN_POINT ( 'NONE',  ( 1.316107777606558615, 302.2275528426508799, 9.913267165427164684 ) ) ;
#63170 = CARTESIAN_POINT ( 'NONE',  ( 85.49456200365183633, -21.96913521486521859, 166.0344729825741581 ) ) ;
#63172 = VECTOR ( 'NONE', #97174, 1000.000000000000000 ) ;
#63171 = DIRECTION ( 'NONE',  ( -1.000000000000000000, -1.224606353822377258E-16, -0.000000000000000000 ) ) ;
#63173 = CARTESIAN_POINT ( 'NONE',  ( 36.47172676003749103, 28.20078810612359987, 11.58029744488031554 ) ) ;
#63174 = ORIENTED_EDGE ( 'NONE', *, *, #97770, .F. ) ;
#63175 = CARTESIAN_POINT ( 'NONE',  ( -23.44105230970441767, 303.4233223010897973, -9.877347747162149361 ) ) ;
#63176 = CARTESIAN_POINT ( 'NONE',  ( 4.903611268973771864, -4.999999999999984901, -16.52575844349507861 ) ) ;
#63177 = FACE_OUTER_BOUND ( 'NONE', #60079, .T. ) ;
#63178 = CYLINDRICAL_SURFACE ( 'NONE', #10698, 7.499999999992679633 ) ;
#63179 = CARTESIAN_POINT ( 'NONE',  ( -25.39209522342085279, 43.62729496076146063, -75.59164047554419597 ) ) ;
#63180 = AXIS2_PLACEMENT_3D ( 'NONE', #55915, #40298, #39786 ) ;
#63181 = CARTESIAN_POINT ( 'NONE',  ( -4.497472161260654744, 250.5422254662594241, -3.972129482042457749 ) ) ;
#63182 = EDGE_CURVE ( 'NONE', #28621, #102936, #19011, .T. ) ;
#63183 = ORIENTED_EDGE ( 'NONE', *, *, #73750, .F. ) ;
#63184 = CARTESIAN_POINT ( 'NONE',  ( -80.77589227446330256, -30.00000000000000000, 10.05485495590529688 ) ) ;
#63185 = CARTESIAN_POINT ( 'NONE',  ( -5.000000000000000888, -56.64697988390040706, 6.234486214504725510 ) ) ;
#63187 = ADVANCED_FACE ( 'NONE', ( #10851 ), #28692, .F. ) ;
#63186 = LINE ( 'NONE', #70736, #76921 ) ;
#63189 = CARTESIAN_POINT ( 'NONE',  ( -12.11070743667100480, 7.914088390801861550, -8.625134750327234201 ) ) ;
#63188 = CARTESIAN_POINT ( 'NONE',  ( -0.4504275197381015783, -18.03418682189721878, 35.00556608437873507 ) ) ;
#63190 = CARTESIAN_POINT ( 'NONE',  ( -1.320432766682874540E-15, -22.53125000204838457, 7.188101187500000044 ) ) ;
#63191 = CARTESIAN_POINT ( 'NONE',  ( 9.740083726526400199, 294.6493269980093714, -10.04303756037254658 ) ) ;
#63192 = DIRECTION ( 'NONE',  ( 0.000000000000000000, -1.000000000000000000, 0.000000000000000000 ) ) ;
#63193 = AXIS2_PLACEMENT_3D ( 'NONE', #91317, #41162, #24996 ) ;
#63194 = AXIS2_PLACEMENT_3D ( 'NONE', #46569, #36928, #45002 ) ;
#63195 = CONTEXT_DEPENDENT_SHAPE_REPRESENTATION ( #8036, #39125 ) ;
#63196 = ORIENTED_EDGE ( 'NONE', *, *, #3930, .F. ) ;
#63197 = DIRECTION ( 'NONE',  ( -1.000000000000000000, 0.000000000000000000, 0.000000000000000000 ) ) ;
#63198 = CARTESIAN_POINT ( 'NONE',  ( 30.00000000000000000, 500.0000000000002274, 0.000000000000000000 ) ) ;
#63199 = CARTESIAN_POINT ( 'NONE',  ( -9.545014793119364072, 9.306529264687913638, 0.000000000000000000 ) ) ;
#63200 = CARTESIAN_POINT ( 'NONE',  ( -7.500000000000003553, -2.999999999998154365, -69.80246343544763477 ) ) ;
#63201 = CARTESIAN_POINT ( 'NONE',  ( 69.67238219402268840, 4.898587196589294500E-16, -4.000000000000007105 ) ) ;
#63202 = EDGE_LOOP ( 'NONE', ( #79425, #59785 ) ) ;
#63203 = DIRECTION ( 'NONE',  ( -0.5735764363510461594, 0.8191520442889916875, 1.003171929053524870E-16 ) ) ;
#63204 = DIRECTION ( 'NONE',  ( 0.000000000000000000, 0.000000000000000000, 1.000000000000000000 ) ) ;
#63205 = STYLED_ITEM ( 'NONE', ( #27566 ), #25527 ) ;
#63206 = VECTOR ( 'NONE', #46625, 1000.000000000000000 ) ;
#63207 = ORIENTED_EDGE ( 'NONE', *, *, #65158, .T. ) ;
#63208 = DIRECTION ( 'NONE',  ( 0.000000000000000000, 0.000000000000000000, 1.000000000000000000 ) ) ;
#63209 = CARTESIAN_POINT ( 'NONE',  ( -3.870939636683478291, -1.214734195355908319, 104.2727580839184895 ) ) ;
#63210 = SURFACE_STYLE_USAGE ( .BOTH. , #6008 ) ;
#63211 = UNCERTAINTY_MEASURE_WITH_UNIT (LENGTH_MEASURE( 1.000000000000000082E-05 ), #27598, 'distance_accuracy_value', 'NONE');
#63212 = CARTESIAN_POINT ( 'NONE',  ( -112.2209848136311052, -60.00000000000000000, 174.8538164149834699 ) ) ;
#63213 = PRODUCT_DEFINITION_SHAPE ( 'NONE', 'NONE',  #106802 ) ;
#63214 = VECTOR ( 'NONE', #85304, 1000.000000000000000 ) ;
#63215 = MECHANICAL_DESIGN_GEOMETRIC_PRESENTATION_REPRESENTATION (  '', ( #66668 ), #75277 ) ;
#63216 = CIRCLE ( 'NONE', #16703, 3.309500000000001663 ) ;
#63217 = AXIS2_PLACEMENT_3D ( 'NONE', #34219, #15468, #58465 ) ;
#63218 = CARTESIAN_POINT ( 'NONE',  ( 16.91683273982978619, 34.22137765266874965, -24.30698433968624883 ) ) ;
#63219 = CARTESIAN_POINT ( 'NONE',  ( -83.54734737942287381, -50.12438367015052165, 185.4795622266105113 ) ) ;
#63220 = ORIENTED_EDGE ( 'NONE', *, *, #78794, .F. ) ;
#63221 = CARTESIAN_POINT ( 'NONE',  ( 41.97891391008103312, 41.63476235974957262, -52.78853482450573864 ) ) ;
#63222 = VECTOR ( 'NONE', #23581, 1000.000000000000000 ) ;
#63223 = ORIENTED_EDGE ( 'NONE', *, *, #70808, .T. ) ;
#63224 = CARTESIAN_POINT ( 'NONE',  ( 15.11650669486618881, -3.999999999999998224, 0.000000000000000000 ) ) ;
#63225 = ADVANCED_FACE ( 'NONE', ( #19547 ), #74955, .T. ) ;
#63226 = FILL_AREA_STYLE_COLOUR ( '', #105923 ) ;
#63227 = CARTESIAN_POINT ( 'NONE',  ( -86.75379648495294305, -60.15014714565931797, 26.71264858234389195 ) ) ;
#63228 = FACE_OUTER_BOUND ( 'NONE', #18552, .T. ) ;
#63229 = EDGE_CURVE ( 'NONE', #62332, #25738, #21569, .T. ) ;
#63230 = CARTESIAN_POINT ( 'NONE',  ( 7.955551520408266519, 53.39349112219676385, 2.456524630699382222E-12 ) ) ;
#63231 = FACE_OUTER_BOUND ( 'NONE', #48271, .T. ) ;
#63232 = CARTESIAN_POINT ( 'NONE',  ( -33.52312678239033517, 18.64316884709848665, 19.32152200342503079 ) ) ;
#63233 = CARTESIAN_POINT ( 'NONE',  ( 112.2652136917531465, -60.00000000000000000, 191.8488956690686962 ) ) ;
#63234 = EDGE_CURVE ( 'NONE', #21252, #33697, #65689, .T. ) ;
#63235 = CARTESIAN_POINT ( 'NONE',  ( -103.2297580319645220, -60.00000000000001421, 85.94764253490394879 ) ) ;
#63236 = CARTESIAN_POINT ( 'NONE',  ( -64.80909832733323128, -32.53232063311292421, 82.02485752868588520 ) ) ;
#63237 = ORIENTED_EDGE ( 'NONE', *, *, #35634, .F. ) ;
#63238 = CARTESIAN_POINT ( 'NONE',  ( -62.84968139608024273, 39.42568783935983134, -16.84587978088738325 ) ) ;
#63239 = CARTESIAN_POINT ( 'NONE',  ( 75.83101594479042262, -60.00000000000735412, 194.1828841934077730 ) ) ;
#63240 = ORIENTED_EDGE ( 'NONE', *, *, #64281, .T. ) ;
#63241 = CARTESIAN_POINT ( 'NONE',  ( 13.95403936970824965, -57.86992245155132508, 28.16216733762122004 ) ) ;
#63242 = CARTESIAN_POINT ( 'NONE',  ( -2.977408999572654480, -18.50000000204838457, 7.188101187499999156 ) ) ;
#63243 = CARTESIAN_POINT ( 'NONE',  ( 29.68315524077034340, 13.12249633091093415, 39.60535821593451544 ) ) ;
#63244 = ORIENTED_EDGE ( 'NONE', *, *, #20294, .T. ) ;
#63245 = AXIS2_PLACEMENT_3D ( 'NONE', #91246, #50227, #32482 ) ;
#63246 = CARTESIAN_POINT ( 'NONE',  ( -11.30587238908023195, 45.32085087904604848, 14.90049756856780228 ) ) ;
#63247 = EDGE_LOOP ( 'NONE', ( #63267, #40916, #105941, #82106, #41817 ) ) ;
#63248 = CARTESIAN_POINT ( 'NONE',  ( 0.000000000000000000, -30.00000000000000000, 0.000000000000000000 ) ) ;
#63249 = CARTESIAN_POINT ( 'NONE',  ( -38.47428897412184767, 485.7788508071988645, -4.770630528146724281 ) ) ;
#63250 = CARTESIAN_POINT ( 'NONE',  ( -2.798807412529719763, -60.00000000000002132, -42.63907750795410578 ) ) ;
#63251 = CARTESIAN_POINT ( 'NONE',  ( 36.64823341582350480, 437.5392299810053487, 4.281405873620231617 ) ) ;
#63252 = CARTESIAN_POINT ( 'NONE',  ( -7.188101187500001821, -24.87500000204838457, -2.977408999572651371 ) ) ;
#63253 = ADVANCED_FACE ( 'NONE', ( #5950 ), #70706, .T. ) ;
#63254 = DIRECTION ( 'NONE',  ( 0.5735764363510557073, -0.8191520442889850262, 1.003171929053516612E-16 ) ) ;
#63255 =( GEOMETRIC_REPRESENTATION_CONTEXT ( 3 ) GLOBAL_UNCERTAINTY_ASSIGNED_CONTEXT ( ( #38064 ) ) GLOBAL_UNIT_ASSIGNED_CONTEXT ( ( #56485, #41909, #15507 ) ) REPRESENTATION_CONTEXT ( 'NONE', 'WORKASPACE' ) );
#63256 = SURFACE_SIDE_STYLE ('',( #61129 ) ) ;
#63257 = CARTESIAN_POINT ( 'NONE',  ( 89.99999999999997158, -60.00000000000000000, 196.0238439516549818 ) ) ;
#63258 = CARTESIAN_POINT ( 'NONE',  ( 2.617478844990903664, 48.00000000000000000, -75.26027323389595836 ) ) ;
#63259 = LINE ( 'NONE', #96150, #47259 ) ;
#63260 = CARTESIAN_POINT ( 'NONE',  ( -43.35910211857093088, 356.0870169904675322, 11.85899587691387147 ) ) ;
#63261 = CARTESIAN_POINT ( 'NONE',  ( 25.55145341416758242, 304.1863475718637346, -9.710152639138275532 ) ) ;
#63262 = VERTEX_POINT ( 'NONE', #13509 ) ;
#63263 = CARTESIAN_POINT ( 'NONE',  ( 0.000000000000000000, 0.000000000000000000, 0.000000000000000000 ) ) ;
#63264 = DIRECTION ( 'NONE',  ( 0.000000000000000000, -1.000000000000000000, 0.000000000000000000 ) ) ;
#63265 = CARTESIAN_POINT ( 'NONE',  ( 36.01760793315731490, -22.19405214988617203, 32.43296674126499823 ) ) ;
#63266 = CARTESIAN_POINT ( 'NONE',  ( -16.57301948836873251, -1.734723475976807094E-15, -4.453875240786733691 ) ) ;
#63267 = ORIENTED_EDGE ( 'NONE', *, *, #80172, .T. ) ;
#63269 = CIRCLE ( 'NONE', #82421, 4.172000000000001485 ) ;
#63268 = DIRECTION ( 'NONE',  ( 0.000000000000000000, -1.000000000000000000, 0.000000000000000000 ) ) ;
#63270 = ORIENTED_EDGE ( 'NONE', *, *, #14425, .T. ) ;
#63272 = CARTESIAN_POINT ( 'NONE',  ( 23.43684916743750080, 295.2641918988800285, 10.02474406024658293 ) ) ;
#63271 = CARTESIAN_POINT ( 'NONE',  ( 9.246231975912676759, -4.999999999999999112, -18.06183020392694871 ) ) ;
#63273 = CARTESIAN_POINT ( 'NONE',  ( 16.66870162890474205, 37.13814613750710691, 21.80698433968582961 ) ) ;
#63274 = CARTESIAN_POINT ( 'NONE',  ( 1.124716868846474149, 43.84887597193111475, -16.86397666530443473 ) ) ;
#63275 = FILL_AREA_STYLE_COLOUR ( '', #65297 ) ;
#63277 = COLOUR_RGB ( '', 0.66274510, 0.83137255, 0.94901961) ;
#63276 = CARTESIAN_POINT ( 'NONE',  ( 4.813668318631095566, -86.79513229826685006, 3.583991016754781711 ) ) ;
#63278 = SURFACE_STYLE_FILL_AREA ( #104244 ) ;
#63279 = CARTESIAN_POINT ( 'NONE',  ( 98.00335581387979289, -60.00000000000000000, 68.94697347453431746 ) ) ;
#63280 = CARTESIAN_POINT ( 'NONE',  ( 36.36650669486618881, 4.000000000000003553, 4.898587196589414801E-16 ) ) ;
#63281 = CARTESIAN_POINT ( 'NONE',  ( -4.000000000000000000, 0.000000000000000000, -3.432199999999999918 ) ) ;
#63282 = CARTESIAN_POINT ( 'NONE',  ( -13.94397698975202537, 6.955966708351442485, -7.994131391027606170 ) ) ;
#63283 = ORIENTED_EDGE ( 'NONE', *, *, #106561, .F. ) ;
#63284 = ADVANCED_FACE ( 'NONE', ( #39930 ), #6055, .T. ) ;
#63285 = CARTESIAN_POINT ( 'NONE',  ( -59.74861173715120088, -29.99999999999999289, 66.22430673131081846 ) ) ;
#63286 = VERTEX_POINT ( 'NONE', #79844 ) ;
#63287 = DIRECTION ( 'NONE',  ( 0.000000000000000000, 0.000000000000000000, 1.000000000000000000 ) ) ;
#63288 = CARTESIAN_POINT ( 'NONE',  ( -16.01234866802003154, 3.721647123655093203, -0.3211924699071123657 ) ) ;
#63289 = CARTESIAN_POINT ( 'NONE',  ( 8.361452242992072570, 30.82456655884618968, 5.000000000000000888 ) ) ;
#63290 = CARTESIAN_POINT ( 'NONE',  ( 32.09911992168216699, 438.9232547152094526, 23.66653216045977359 ) ) ;
#63292 = CARTESIAN_POINT ( 'NONE',  ( 83.48762353522853630, -52.72806324350694496, -16.05720600496736949 ) ) ;
#63291 = AXIS2_PLACEMENT_3D ( 'NONE', #39344, #63076, #72223 ) ;
#63293 = AXIS2_PLACEMENT_3D ( 'NONE', #59509, #92918, #51922 ) ;
#63294 = CARTESIAN_POINT ( 'NONE',  ( -2.977408999572654480, -30.50000000204838813, 7.188101187499999156 ) ) ;
#63295 = DIRECTION ( 'NONE',  ( -0.5356766697699718582, -0.1574227122302049586, 0.8296195484306275736 ) ) ;
#63296 = DIRECTION ( 'NONE',  ( 0.000000000000000000, 1.000000000000000000, 0.000000000000000000 ) ) ;
#63298 = ADVANCED_FACE ( 'NONE', ( #47471 ), #62622, .F. ) ;
#63297 = CARTESIAN_POINT ( 'NONE',  ( -18.00000000000000355, 12.99999999999999289, 0.000000000000000000 ) ) ;
#63299 = EDGE_CURVE ( 'NONE', #86892, #89440, #42569, .T. ) ;
#63300 = EDGE_LOOP ( 'NONE', ( #83691, #29980, #29835, #10975 ) ) ;
#63301 = AXIS2_PLACEMENT_3D ( 'NONE', #59090, #43960, #26229 ) ;
#63302 = VECTOR ( 'NONE', #49705, 1000.000000000000000 ) ;
#63304 = ORIENTED_EDGE ( 'NONE', *, *, #78158, .F. ) ;
#63303 = CARTESIAN_POINT ( 'NONE',  ( 0.000000000000000000, -46.00000000000000000, 112.0000000000000000 ) ) ;
#63305 = CARTESIAN_POINT ( 'NONE',  ( 82.19508700470152007, -18.68693059907149490, 137.0968519703368713 ) ) ;
#63306 = CARTESIAN_POINT ( 'NONE',  ( 14.37676598791153104, 2.000025124005285093, -4.258993516738696528 ) ) ;
#63307 = ORIENTED_EDGE ( 'NONE', *, *, #13698, .F. ) ;
#63308 = CARTESIAN_POINT ( 'NONE',  ( -12.50000000000000355, 26.18163903155594596, -43.67239987017219960 ) ) ;
#63309 = AXIS2_PLACEMENT_3D ( 'NONE', #88095, #63824, #4512 ) ;
#63310 = CARTESIAN_POINT ( 'NONE',  ( 5.441822646184710344, 41.96569307385608028, -59.31342461362935836 ) ) ;
#63311 = CARTESIAN_POINT ( 'NONE',  ( -7.188101187500000044, -19.90625000204838457, -8.802885111219163269E-16 ) ) ;
#63312 = AXIS2_PLACEMENT_3D ( 'NONE', #14399, #65097, #31693 ) ;
#63313 = CARTESIAN_POINT ( 'NONE',  ( -35.73279548032036956, -57.69589661319782437, 49.90756511973714282 ) ) ;
#63314 = CARTESIAN_POINT ( 'NONE',  ( 17.19026434692938565, 294.5876779312053486, 9.880857241781999534 ) ) ;
#63315 = ADVANCED_FACE ( 'NONE', ( #75471 ), #16457, .T. ) ;
#63316 = ORIENTED_EDGE ( 'NONE', *, *, #44650, .T. ) ;
#63317 = FILL_AREA_STYLE ('',( #30423 ) ) ;
#63318 = B_SPLINE_CURVE_WITH_KNOTS ( 'NONE', 3,
 ( #104531, #81303, #6353, #39295 ),
 .UNSPECIFIED., .F., .F.,
 ( 4, 4 ),
 ( 1.908195823574487804E-17, 0.0002807886668484363022 ),
 .UNSPECIFIED. ) ;
#63319 = CARTESIAN_POINT ( 'NONE',  ( 0.000000000000000000, 0.000000000000000000, 5.000000000000000888 ) ) ;
#63320 = CARTESIAN_POINT ( 'NONE',  ( -5.476751506168963779, -13.16357122866993379, -2.461144630687908119 ) ) ;
#63321 = CARTESIAN_POINT ( 'NONE',  ( -9.381593208289373820, 82.98561361880494758, -3.465401811657801368 ) ) ;
#63322 = SURFACE_STYLE_USAGE ( .BOTH. , #30970 ) ;
#63323 = CIRCLE ( 'NONE', #8553, 4.000000000000003553 ) ;
#63324 = CARTESIAN_POINT ( 'NONE',  ( 5.656854249492380582, -11.00000000409677092, -5.656854249492379694 ) ) ;
#63325 = CARTESIAN_POINT ( 'NONE',  ( -32.55262149376069658, -22.90611988631381024, 32.69735316556134563 ) ) ;
#63326 =( NAMED_UNIT ( * ) SI_UNIT ( $, .STERADIAN. ) SOLID_ANGLE_UNIT ( ) );
#63327 = CARTESIAN_POINT ( 'NONE',  ( -1.152188841818234133E-13, -1.200000000000000030E-05, -50.50000000000000000 ) ) ;
#63328 = ADVANCED_FACE ( 'NONE', ( #81953 ), #65795, .T. ) ;
#63329 = VECTOR ( 'NONE', #75438, 1000.000000000000000 ) ;
#63330 = CARTESIAN_POINT ( 'NONE',  ( 4.852941176470592310, -3.000000000000002665, -70.80672828634229177 ) ) ;
#63331 = B_SPLINE_CURVE_WITH_KNOTS ( 'NONE', 3,
 ( #98788, #56737, #82078, #73450, #33042, #57798, #1140, #32510 ),
 .UNSPECIFIED., .F., .F.,
 ( 4, 2, 2, 4 ),
 ( 0.4104551234109616309, 0.4139675920961696232, 0.4174800607813775599, 0.4245049981517935445 ),
 .UNSPECIFIED. ) ;
#63332 = DIRECTION ( 'NONE',  ( 0.000000000000000000, -1.000000000000000000, 0.000000000000000000 ) ) ;
#63333 = SHAPE_DEFINITION_REPRESENTATION ( #50967, #44072 ) ;
#63334 = CARTESIAN_POINT ( 'NONE',  ( -11.96225037626273036, -7.080565903723901933, 19.72249172895450542 ) ) ;
#63335 = ORIENTED_EDGE ( 'NONE', *, *, #16592, .T. ) ;
#63336 = CARTESIAN_POINT ( 'NONE',  ( 10.61508837294732999, 43.20235039013163458, 15.36662796280145038 ) ) ;
#63337 = CARTESIAN_POINT ( 'NONE',  ( -4.210530276627961754, 14.99999999999998934, 10.00000000000003908 ) ) ;
#63338 = AXIS2_PLACEMENT_3D ( 'NONE', #78402, #28300, #61175 ) ;
#63339 = CARTESIAN_POINT ( 'NONE',  ( -38.11055680731723783, 437.2326489915187153, 4.664335030333703891 ) ) ;
#63340 = CARTESIAN_POINT ( 'NONE',  ( -70.52629063140332732, -29.99999999999998579, -20.46674107074536053 ) ) ;
#63341 = CARTESIAN_POINT ( 'NONE',  ( -69.41254636990348104, -30.00000000000000355, 93.44164650999076116 ) ) ;
#63342 = FACE_OUTER_BOUND ( 'NONE', #24555, .T. ) ;
#63343 = VERTEX_POINT ( 'NONE', #8079 ) ;
#63344 = CARTESIAN_POINT ( 'NONE',  ( -43.27291153936683088, 435.9049899631313565, 8.045225097066092346 ) ) ;
#63345 = CARTESIAN_POINT ( 'NONE',  ( 91.34176007303615563, -57.61388464028566148, 204.2308622945469949 ) ) ;
#63346 = CARTESIAN_POINT ( 'NONE',  ( 71.72532340997096867, -34.58959646309544667, -21.02624987897744901 ) ) ;
#63347 = AXIS2_PLACEMENT_3D ( 'NONE', #12158, #59667, #93630 ) ;
#63348 = CARTESIAN_POINT ( 'NONE',  ( 37.88504238421511872, 463.4171042825134350, 19.90923349043885437 ) ) ;
#63349 = CARTESIAN_POINT ( 'NONE',  ( -15.79412934197575602, 22.74951556322103130, -1.014593669880072380 ) ) ;
#63350 = CARTESIAN_POINT ( 'NONE',  ( -5.749871404199004277E-15, -6.732211846623389562, 4.339467034331195627 ) ) ;
#63351 = CARTESIAN_POINT ( 'NONE',  ( -73.50359396478988572, -60.00000000000000000, 167.2255443349855000 ) ) ;
#63352 = AXIS2_PLACEMENT_3D ( 'NONE', #1344, #65575, #100063 ) ;
#63353 = CARTESIAN_POINT ( 'NONE',  ( 0.000000000000000000, 0.000000000000000000, 18.57417562100670949 ) ) ;
#63354 = CARTESIAN_POINT ( 'NONE',  ( -9.165151389911679658, 85.00000000000000000, 4.000000000000000000 ) ) ;
#63355 = CARTESIAN_POINT ( 'NONE',  ( 5.957442974701733007, 49.99999999999999289, 65.00000000000000000 ) ) ;
#63356 = B_SPLINE_CURVE_WITH_KNOTS ( 'NONE', 3,
 ( #9916, #1814, #11502, #67645, #93519, #26681, #101058, #44429 ),
 .UNSPECIFIED., .F., .F.,
 ( 4, 2, 2, 4 ),
 ( 3.469446951953614189E-18, 0.001701863333577075541, 0.003403726667154147612, 0.006807453334308237111 ),
 .UNSPECIFIED. ) ;
#63357 = B_SPLINE_CURVE_WITH_KNOTS ( 'NONE', 3,
 ( #64063, #96937, #55910, #88850, #14940, #34897, #76909, #18164, #44018, #60231, #1402, #17630 ),
 .UNSPECIFIED., .F., .F.,
 ( 4, 2, 2, 2, 2, 4 ),
 ( 0.000000000000000000, 0.001314793157745834488, 0.001972189736618751299, 0.002629586315491668543, 0.003944379473237499996, 0.005259172630983331015 ),
 .UNSPECIFIED. ) ;
#63358 = CARTESIAN_POINT ( 'NONE',  ( -84.96685468468123759, -50.19859687476371590, 189.1434212840244697 ) ) ;
#63359 = ORIENTED_EDGE ( 'NONE', *, *, #47375, .T. ) ;
#63360 = CARTESIAN_POINT ( 'NONE',  ( 32.84830840339214575, 322.5517557799010433, -4.669727346969580140 ) ) ;
#63361 = LINE ( 'NONE', #97286, #45672 ) ;
#63362 = ADVANCED_FACE ( 'NONE', ( #23773 ), #32389, .T. ) ;
#63363 = DIRECTION ( 'NONE',  ( 0.000000000000000000, 0.000000000000000000, 1.000000000000000000 ) ) ;
#63364 = CARTESIAN_POINT ( 'NONE',  ( 41.74605044188654546, 488.3336308464836861, 9.449957167453774787 ) ) ;
#63365 = SURFACE_STYLE_USAGE ( .BOTH. , #12654 ) ;
#63366 = CARTESIAN_POINT ( 'NONE',  ( 4.898587196589412829E-16, -18.31250000409676915, -8.000000000000000000 ) ) ;
#63367 =( GEOMETRIC_REPRESENTATION_CONTEXT ( 3 ) GLOBAL_UNCERTAINTY_ASSIGNED_CONTEXT ( ( #96820 ) ) GLOBAL_UNIT_ASSIGNED_CONTEXT ( ( #8415, #56954, #15982 ) ) REPRESENTATION_CONTEXT ( 'NONE', 'WORKASPACE' ) );
#63368 = ORIENTED_EDGE ( 'NONE', *, *, #78975, .F. ) ;
#63369 = AXIS2_PLACEMENT_3D ( 'NONE', #19494, #76605, #2719 ) ;
#63370 = CARTESIAN_POINT ( 'NONE',  ( 18.96929081463403932, 50.00000000000001421, 60.62668834763405812 ) ) ;
#63371 = LINE ( 'NONE', #45589, #95004 ) ;
#63372 = ADVANCED_FACE ( 'NONE', ( #66862 ), #23418, .T. ) ;
#63373 =( NAMED_UNIT ( * ) PLANE_ANGLE_UNIT ( ) SI_UNIT ( $, .RADIAN. ) );
#63374 = CARTESIAN_POINT ( 'NONE',  ( 0.2573354458087839802, 6.889406814520513400, -1.067197363239225094 ) ) ;
#63375 = ADVANCED_FACE ( 'NONE', ( #73874 ), #33841, .F. ) ;
#63376 = CARTESIAN_POINT ( 'NONE',  ( 94.21214616282756538, -60.00000000000006395, 9.573485886066015027 ) ) ;
#63377 = CARTESIAN_POINT ( 'NONE',  ( -81.43623979954335823, -29.09389058366499370, 143.4191690805281212 ) ) ;
#63378 = VERTEX_POINT ( 'NONE', #4251 ) ;
#63379 =( NAMED_UNIT ( * ) SI_UNIT ( $, .STERADIAN. ) SOLID_ANGLE_UNIT ( ) );
#63380 = CARTESIAN_POINT ( 'NONE',  ( -1.899844873468226281, 42.00000000000000711, -68.00838909559428203 ) ) ;
#63381 = CARTESIAN_POINT ( 'NONE',  ( 104.6988950438752255, -57.64257840656350140, 201.8919179864889770 ) ) ;
#63382 = PRESENTATION_LAYER_ASSIGNMENT (  '', '', ( #18655 ) ) ;
#63383 = AXIS2_PLACEMENT_3D ( 'NONE', #79255, #78711, #70642 ) ;
#63384 = AXIS2_PLACEMENT_3D ( 'NONE', #65520, #14828, #89800 ) ;
#63385 = CARTESIAN_POINT ( 'NONE',  ( 24.21392849876044906, 50.00000000000000711, 58.37490609712320833 ) ) ;
#63386 = CARTESIAN_POINT ( 'NONE',  ( 30.48226588409197291, 308.5642027897181947, -8.691376423780738492 ) ) ;
#63387 = CARTESIAN_POINT ( 'NONE',  ( 0.000000000000000000, 0.000000000000000000, -0.4455245229258316120 ) ) ;
#63388 = ORIENTED_EDGE ( 'NONE', *, *, #70530, .F. ) ;
#63389 = DIRECTION ( 'NONE',  ( 0.000000000000000000, 1.000000000000000000, 0.000000000000000000 ) ) ;
#63390 = SURFACE_STYLE_FILL_AREA ( #62851 ) ;
#63392 = CARTESIAN_POINT ( 'NONE',  ( -102.8019275820111602, -52.71028098699141395, 142.0411747293566407 ) ) ;
#63391 = CARTESIAN_POINT ( 'NONE',  ( -16.75187969033459012, 36.38380281757147827, 24.30698433969199357 ) ) ;
#63393 = CARTESIAN_POINT ( 'NONE',  ( 5.082755093536325930, -24.96875000204838813, -5.082755093536325042 ) ) ;
#63394 = EDGE_CURVE ( 'NONE', #8257, #75630, #59307, .T. ) ;
#63395 = EDGE_CURVE ( 'NONE', #34259, #59573, #84637, .T. ) ;
#63396 = CARTESIAN_POINT ( 'NONE',  ( 45.94900261086841198, 1.482358050883964840E-15, 0.000000000000000000 ) ) ;
#63397 = AXIS2_PLACEMENT_3D ( 'NONE', #43490, #66696, #75848 ) ;
#63398 = CARTESIAN_POINT ( 'NONE',  ( 0.1683342203993841713, 34.17188553058033307, 29.75000000000001066 ) ) ;
#63399 = CARTESIAN_POINT ( 'NONE',  ( 26.01020368950299400, 37.20437420822879204, 8.180924129841026016 ) ) ;
#63400 = CARTESIAN_POINT ( 'NONE',  ( -48.02835407290534420, 14.94086294439724227, -16.85535821593460426 ) ) ;
#63401 = CARTESIAN_POINT ( 'NONE',  ( -24.32789867356884628, 27.33682607920834684, -32.55354264101782036 ) ) ;
#63402 = ORIENTED_EDGE ( 'NONE', *, *, #89462, .F. ) ;
#63403 = CARTESIAN_POINT ( 'NONE',  ( -6.757705282517541434, 41.35007050579768162, -70.67351639275690900 ) ) ;
#63405 = CARTESIAN_POINT ( 'NONE',  ( 25.57206085308608223, -25.56680585492497926, 29.49300859707019740 ) ) ;
#63404 = CARTESIAN_POINT ( 'NONE',  ( -31.98280533637225176, -29.99999999999996447, 41.00520926490388263 ) ) ;
#63406 = CARTESIAN_POINT ( 'NONE',  ( -24.46934747735757298, 25.33804889760450862, 32.00006138626095975 ) ) ;
#63407 = ORIENTED_EDGE ( 'NONE', *, *, #23592, .F. ) ;
#63408 = UNCERTAINTY_MEASURE_WITH_UNIT (LENGTH_MEASURE( 1.000000000000000082E-05 ), #32657, 'distance_accuracy_value', 'NONE');
#63409 = ORIENTED_EDGE ( 'NONE', *, *, #92115, .F. ) ;
#63411 = CARTESIAN_POINT ( 'NONE',  ( 0.08445723013546542479, 52.17923068443687384, 7.750000000000003553 ) ) ;
#63410 = CARTESIAN_POINT ( 'NONE',  ( 0.000000000000000000, 0.000000000000000000, 4.000000000000000000 ) ) ;
#63412 = DIRECTION ( 'NONE',  ( 0.000000000000000000, -1.000000000000000000, 0.000000000000000000 ) ) ;
#63413 =( NAMED_UNIT ( * ) SI_UNIT ( $, .STERADIAN. ) SOLID_ANGLE_UNIT ( ) );
#63414 = CARTESIAN_POINT ( 'NONE',  ( -0.7862562837408798577, 51.35452495058204647, -9.985734753308584288 ) ) ;
#63415 = CARTESIAN_POINT ( 'NONE',  ( 6.251124561268293967, 3.157894736842103534, 14.66382285868950675 ) ) ;
#63416 = CARTESIAN_POINT ( 'NONE',  ( 0.3590100610935850756, 18.74889334034432764, -49.30114299272825917 ) ) ;
#63418 = ORIENTED_EDGE ( 'NONE', *, *, #54219, .F. ) ;
#63417 = AXIS2_PLACEMENT_3D ( 'NONE', #105058, #103979, #29097 ) ;
#63419 = CARTESIAN_POINT ( 'NONE',  ( 40.45747091539019635, -59.99999999999999289, -39.57904950317593062 ) ) ;
#63420 = CARTESIAN_POINT ( 'NONE',  ( 86.82001826315290316, -29.99999999999992184, 183.0449992333263936 ) ) ;
#63421 = CARTESIAN_POINT ( 'NONE',  ( -13.01334625365200992, 23.72039682945885630, 4.358981111881473858 ) ) ;
#63422 = CARTESIAN_POINT ( 'NONE',  ( 7.500000000000002665, -0.7512838658081426590, 2.480112469560591787E-15 ) ) ;
#63423 = CARTESIAN_POINT ( 'NONE',  ( 73.73040302543078894, -29.99999999999999645, -18.77833202125217582 ) ) ;
#63424 = CARTESIAN_POINT ( 'NONE',  ( 11.46409645960816626, 12.99999999999817923, -10.00000000000000178 ) ) ;
#63425 = VERTEX_POINT ( 'NONE', #52792 ) ;
#63426 = EDGE_LOOP ( 'NONE', ( #40299, #83957, #94688, #70115 ) ) ;
#63427 = CIRCLE ( 'NONE', #85832, 4.000000000000007105 ) ;
#63428 = VERTEX_POINT ( 'NONE', #92178 ) ;
#63429 = FACE_OUTER_BOUND ( 'NONE', #3836, .T. ) ;
#63430 = PRESENTATION_STYLE_ASSIGNMENT (( #40181 ) ) ;
#63431 = CARTESIAN_POINT ( 'NONE',  ( -20.00000000000000000, 12.99999999999999289, 0.000000000000000000 ) ) ;
#63432 = LINE ( 'NONE', #61841, #70402 ) ;
#63433 = SURFACE_STYLE_USAGE ( .BOTH. , #31598 ) ;
#63434 = LINE ( 'NONE', #88748, #81155 ) ;
#63435 = ORIENTED_EDGE ( 'NONE', *, *, #64517, .T. ) ;
#63437 = EDGE_CURVE ( 'NONE', #17581, #58778, #18328, .T. ) ;
#63436 = CARTESIAN_POINT ( 'NONE',  ( -6.145467200824003662, 48.00000000000000000, -77.00333157709306420 ) ) ;
#63438 = ORIENTED_EDGE ( 'NONE', *, *, #73465, .F. ) ;
#63439 = CARTESIAN_POINT ( 'NONE',  ( -32.09911992168218831, 438.9232547152092252, 23.66653216045979491 ) ) ;
#63440 = CARTESIAN_POINT ( 'NONE',  ( 32.93513049338658760, 465.6726574193327792, 10.66039033145146142 ) ) ;
#63441 = CARTESIAN_POINT ( 'NONE',  ( 96.28888888888889142, 4.172000000000019249, 0.000000000000000000 ) ) ;
#63442 = CARTESIAN_POINT ( 'NONE',  ( 6.289812543865807015, -6.246946743711094818, -2.837966828325884538 ) ) ;
#63443 = CARTESIAN_POINT ( 'NONE',  ( 61.71159894698526216, -60.33950585225007046, 87.28437287168905812 ) ) ;
#63444 = AXIS2_PLACEMENT_3D ( 'NONE', #21687, #103110, #95032 ) ;
#63445 = ORIENTED_EDGE ( 'NONE', *, *, #43111, .F. ) ;
#63446 = CARTESIAN_POINT ( 'NONE',  ( 37.67124221001638773, 463.6239404278543930, 19.49545380201351463 ) ) ;
#63447 = CARTESIAN_POINT ( 'NONE',  ( -52.90880457622053257, -36.17226545501620905, -35.66381235367310865 ) ) ;
#63448 = LINE ( 'NONE', #45659, #67864 ) ;
#63449 =( BOUNDED_SURFACE ( )  B_SPLINE_SURFACE ( 3, 2, ( 
 ( #94409, #102492, #71688 ),
 ( #28635, #53918, #104063 ),
 ( #30206, #20572, #4856 ),
 ( #53410, #62058, #12394 ),
 ( #86849, #80308, #65740 ),
 ( #98621, #24770, #64679 ),
 ( #31279, #80847, #16654 ),
 ( #57619, #105655, #88431 ),
 ( #57097, #15585, #90545 ),
 ( #32864, #49544, #82449 ),
 ( #6420, #41455, #8554 ),
 ( #74346, #73820, #106714 ),
 ( #423, #65202, #56023 ),
 ( #15049, #73276, #33391 ),
 ( #66263, #22657, #55493 ),
 ( #23175, #24248, #14505 ),
 ( #47417, #39359, #72236 ),
 ( #88954, #105139, #47938 ),
 ( #72749, #64165, #6959 ),
 ( #16115, #7477, #32334 ),
 ( #97037, #106172, #40393 ),
 ( #39876, #31793, #56563 ),
 ( #97552, #8018, #23711 ),
 ( #89490, #48475, #81368 ),
 ( #98097, #90011, #81901 ),
 ( #48999, #40927, #85112 ) ),
 .UNSPECIFIED., .F., .F., .F. ) 
 B_SPLINE_SURFACE_WITH_KNOTS ( ( 4, 2, 2, 2, 2, 2, 2, 2, 2, 2, 2, 2, 4 ),
 ( 3, 3 ),
 ( -8.736501105888194729E-16, 0.0005478302971548104335, 0.001095660594310494517, 0.001643490891466178492, 0.001917406040044020588, 0.002191321188621862467, 0.002465236337199704347, 0.002739151485777546226, 0.003013066634355388539, 0.003286981782933230418, 0.003560896931511072297, 0.003834812080088914610, 0.004382642377244598368 ),
 ( 0.000000000000000000, 1.000000000000000000 ),
 .UNSPECIFIED. ) 
 GEOMETRIC_REPRESENTATION_ITEM ( )  RATIONAL_B_SPLINE_SURFACE ( (
 ( 1.000000000000000000, 0.7071067811865463515, 1.000000000000000000),
 ( 1.000000000000000000, 0.7205633224822174387, 1.000000000000000000),
 ( 1.000000000000000000, 0.7338046748641441352, 1.000000000000000000),
 ( 1.000000000000000000, 0.7598569482828753108, 1.000000000000000000),
 ( 1.000000000000000000, 0.7728059803407538730, 1.000000000000000000),
 ( 1.000000000000000000, 0.7970392697931634185, 1.000000000000000000),
 ( 1.000000000000000000, 0.8084357292879817969, 1.000000000000000000),
 ( 1.000000000000000000, 0.8242617997985818290, 1.000000000000000000),
 ( 1.000000000000000000, 0.8292815833619189281, 1.000000000000000000),
 ( 1.000000000000000000, 0.8385524799095220860, 1.000000000000000000),
 ( 1.000000000000000000, 0.8428399694390146246, 1.000000000000000000),
 ( 1.000000000000000000, 0.8506757475323690754, 1.000000000000000000),
 ( 1.000000000000000000, 0.8542245152660158380, 1.000000000000000000),
 ( 1.000000000000000000, 0.8604965487139214497, 1.000000000000000000),
 ( 1.000000000000000000, 0.8631692933856984773, 1.000000000000000000),
 ( 1.000000000000000000, 0.8674535388008016712, 1.000000000000000000),
 ( 1.000000000000000000, 0.8690878299427780007, 1.000000000000000000),
 ( 1.000000000000000000, 0.8713061800473431706, 1.000000000000000000),
 ( 1.000000000000000000, 0.8718871419634710573, 1.000000000000000000),
 ( 1.000000000000000000, 0.8719209662387543691, 1.000000000000000000),
 ( 1.000000000000000000, 0.8713887681177838740, 1.000000000000000000),
 ( 1.000000000000000000, 0.8692752663532812285, 1.000000000000000000),
 ( 1.000000000000000000, 0.8676790533738677480, 1.000000000000000000),
 ( 1.000000000000000000, 0.8614089247988945264, 1.000000000000000000),
 ( 1.000000000000000000, 0.8553884691243534011, 1.000000000000000000),
 ( 1.000000000000000000, 0.8477912478906586280, 1.000000000000000000) ) ) 
 REPRESENTATION_ITEM ( '' )  SURFACE ( )  );
#63450 = LINE ( 'NONE', #15931, #58419 ) ;
#63451 = VERTEX_POINT ( 'NONE', #77070 ) ;
#63452 = CARTESIAN_POINT ( 'NONE',  ( 47.90217879170857884, 15.22462055664289338, 16.85535821593427031 ) ) ;
#63453 = DIRECTION ( 'NONE',  ( 1.000000000000000000, -0.000000000000000000, -0.000000000000000000 ) ) ;
#63454 = AXIS2_PLACEMENT_3D ( 'NONE', #10541, #43459, #60198 ) ;
#63455 = CARTESIAN_POINT ( 'NONE',  ( 47.33349330513379982, 1.593028355512270567E-15, 0.000000000000000000 ) ) ;
#63456 = CARTESIAN_POINT ( 'NONE',  ( 4.898587196589412829E-16, -27.31250000409677270, -8.000000000000000000 ) ) ;
#63457 = CARTESIAN_POINT ( 'NONE',  ( 10.00000000000000000, -5.000000000000000000, -2.617993873628171375 ) ) ;
#63458 = AXIS2_PLACEMENT_3D ( 'NONE', #17280, #90089, #8632 ) ;
#63459 = CARTESIAN_POINT ( 'NONE',  ( 86.81267294504679910, -42.78936011489643931, 189.6631950169049219 ) ) ;
#63460 = EDGE_CURVE ( 'NONE', #90150, #91492, #64737, .T. ) ;
#63461 = CARTESIAN_POINT ( 'NONE',  ( -5.292942464630674415, 18.36785030193200896, -37.75007169989023481 ) ) ;
#63462 = EDGE_CURVE ( 'NONE', #77575, #58722, #18253, .T. ) ;
#63463 = CARTESIAN_POINT ( 'NONE',  ( -8.988144951968882523, 15.40598489177414976, 4.999999999999999112 ) ) ;
#63464 = VERTEX_POINT ( 'NONE', #44721 ) ;
#63465 = CARTESIAN_POINT ( 'NONE',  ( 0.5805565836007617886, -3.752776749732566142, 6.499999999999999112 ) ) ;
#63466 = CARTESIAN_POINT ( 'NONE',  ( 12.33349330513380693, 1.593028355512270962E-15, 0.000000000000000000 ) ) ;
#63467 = CARTESIAN_POINT ( 'NONE',  ( 35.82122592925417592, -60.00000000000000000, 47.16707035416197868 ) ) ;
#63468 = CARTESIAN_POINT ( 'NONE',  ( -98.35766590278744559, -30.00000000000000355, 140.0735935797200682 ) ) ;
#63469 = VECTOR ( 'NONE', #47534, 1000.000000000000114 ) ;
#63470 = CYLINDRICAL_SURFACE ( 'NONE', #10710, 10.00000000000000355 ) ;
#63471 = CARTESIAN_POINT ( 'NONE',  ( 41.51254023491689082, -57.68873884886530590, 58.24736279105339776 ) ) ;
#63473 = CARTESIAN_POINT ( 'NONE',  ( 0.000000000000000000, 0.000000000000000000, 65.00000000000000000 ) ) ;
#63472 = CARTESIAN_POINT ( 'NONE',  ( -0.9558972795473693607, 25.32440591748497738, -40.30957252762832610 ) ) ;
#63474 = AXIS2_PLACEMENT_3D ( 'NONE', #87931, #80340, #105167 ) ;
#63475 = CARTESIAN_POINT ( 'NONE',  ( -38.85446894546474539, 460.8903912184078422, 2.218456751110488678 ) ) ;
#63476 = CARTESIAN_POINT ( 'NONE',  ( -18.13920979082782736, 50.00000000000000000, 61.71120590876283529 ) ) ;
#63477 = CARTESIAN_POINT ( 'NONE',  ( -14.57895281699998513, -60.00000000000000000, 39.77189858658603328 ) ) ;
#63478 = FACE_BOUND ( 'NONE', #31220, .T. ) ;
#63479 = COLOUR_RGB ( '', 0.72549020, 0.75294118, 0.79215686) ;
#63480 = CARTESIAN_POINT ( 'NONE',  ( -87.19698863470328831, -46.43428023365913759, 191.1401204188958900 ) ) ;
#63481 = ORIENTED_EDGE ( 'NONE', *, *, #98176, .T. ) ;
#63482 = CARTESIAN_POINT ( 'NONE',  ( 36.44482444458351011, 439.0054583426050954, 23.96131986156384031 ) ) ;
#63483 = CARTESIAN_POINT ( 'NONE',  ( -14.50479935719362956, -35.99470073277952054, 30.00759979546209522 ) ) ;
#63484 = B_SPLINE_SURFACE_WITH_KNOTS ( 'NONE', 3, 3, ( 
 ( #8997, #74791, #7399, #869, #15504, #31714, #49455, #48392, #65118, #24168 ),
 ( #48915, #106634, #82364, #8470, #25778, #78387, #44983, #95126, #94601, #77335 ),
 ( #12580, #11511, #46034, #36392, #62241, #86517, #45513, #27766, #13106, #99600 ),
 ( #68728, #70309, #101612, #3446, #84893, #43898, #93528, #29350, #61708, #4504 ),
 ( #60115, #35851, #69779, #28285, #37440, #103204, #21257, #54094, #87037, #94047 ),
 ( #78915, #33848, #85981, #66720, #36908, #92979, #60641, #19673, #61160, #19139 ),
 ( #77869, #51978, #10981, #3979, #76787, #2891, #20207, #52513, #53062, #85428 ),
 ( #44439, #69259, #102130, #102670, #12054, #28833, #20748, #53587, #47599, #29874 ) ),
 .UNSPECIFIED., .F., .F., .F.,
 ( 4, 2, 2, 4 ),
 ( 4, 2, 2, 2, 4 ),
 ( 0.000000000000000000, 0.2500000000000000000, 0.5000000000000000000, 1.000000000000000000 ),
 ( 0.000000000000000000, 0.1250000000000000000, 0.2500000000000000000, 0.5000000000000000000, 1.000000000000000000 ),
 .UNSPECIFIED. ) ;
#63486 = CARTESIAN_POINT ( 'NONE',  ( 40.78808449138612957, 461.0038402359687097, 2.292482253616458632 ) ) ;
#63485 = CARTESIAN_POINT ( 'NONE',  ( -86.75607522730589949, -59.99999999999997158, 27.04728030040551445 ) ) ;
#63487 = ORIENTED_EDGE ( 'NONE', *, *, #14452, .T. ) ;
#63488 = DIRECTION ( 'NONE',  ( 1.000000000000000000, 0.000000000000000000, 0.000000000000000000 ) ) ;
#63489 = CIRCLE ( 'NONE', #47974, 5.000000000000001776 ) ;
#63490 =( NAMED_UNIT ( * ) SI_UNIT ( $, .STERADIAN. ) SOLID_ANGLE_UNIT ( ) );
#63491 = PRESENTATION_LAYER_ASSIGNMENT (  '', '', ( #42759 ) ) ;
#63492 = CARTESIAN_POINT ( 'NONE',  ( 15.50988061984581634, 2.604948194298077002, -0.4026888889232626556 ) ) ;
#63493 = CARTESIAN_POINT ( 'NONE',  ( 73.51685685884034172, -60.00000000000000711, 167.3565946372449957 ) ) ;
#63494 = CARTESIAN_POINT ( 'NONE',  ( -45.31383884518383098, 362.9196860876334085, 5.161789940898600548 ) ) ;
#63495 = VERTEX_POINT ( 'NONE', #10723 ) ;
#63496 = CARTESIAN_POINT ( 'NONE',  ( -7.000000000000001776, -80.00000000000000000, 39.12435565298213902 ) ) ;
#63497 = CARTESIAN_POINT ( 'NONE',  ( 0.000000000000000000, 0.000000000000000000, 0.000000000000000000 ) ) ;
#63498 = CARTESIAN_POINT ( 'NONE',  ( 46.52147948847155590, -60.00000000000000000, 69.35914673975356948 ) ) ;
#63499 = CIRCLE ( 'NONE', #25658, 4.000000000000001776 ) ;
#63500 = SURFACE_STYLE_FILL_AREA ( #32194 ) ;
#63501 = VERTEX_POINT ( 'NONE', #11790 ) ;
#63502 = EDGE_LOOP ( 'NONE', ( #19939, #36619, #5795, #84627, #61710 ) ) ;
#63503 = CARTESIAN_POINT ( 'NONE',  ( -29.24981464811047260, 322.6110501364183847, 13.31810279652815510 ) ) ;
#63504 = ADVANCED_FACE ( 'NONE', ( #100278 ), #26440, .T. ) ;
#63505 = ORIENTED_EDGE ( 'NONE', *, *, #98738, .F. ) ;
#63506 =( NAMED_UNIT ( * ) PLANE_ANGLE_UNIT ( ) SI_UNIT ( $, .RADIAN. ) );
#63507 = ADVANCED_FACE ( 'NONE', ( #43113 ), #67917, .T. ) ;
#63508 = CARTESIAN_POINT ( 'NONE',  ( 0.000000000000000000, 49.00000000000000000, 0.000000000000000000 ) ) ;
#63509 = CARTESIAN_POINT ( 'NONE',  ( 8.000000000000000000, -12.68750000409676915, 0.000000000000000000 ) ) ;
#63510 = ORIENTED_EDGE ( 'NONE', *, *, #28103, .F. ) ;
#63511 =( LENGTH_UNIT ( ) NAMED_UNIT ( * ) SI_UNIT ( .MILLI., .METRE. ) );
#63512 = CARTESIAN_POINT ( 'NONE',  ( -109.7149502225919377, -60.00000000005858425, 124.6291749562062989 ) ) ;
#63513 = CARTESIAN_POINT ( 'NONE',  ( 44.24678642376221660, 485.3508677736838308, 2.236524924813607207 ) ) ;
#63514 = CARTESIAN_POINT ( 'NONE',  ( 77.22884141242977307, -60.00000000000002132, 191.0907396958321272 ) ) ;
#63515 = DIRECTION ( 'NONE',  ( -0.000000000000000000, 1.000000000000000000, -0.000000000000000000 ) ) ;
#63516 = FILL_AREA_STYLE_COLOUR ( '', #3833 ) ;
#63517 = AXIS2_PLACEMENT_3D ( 'NONE', #64941, #14250, #5642 ) ;
#63519 = CARTESIAN_POINT ( 'NONE',  ( 10.15756363273992591, -29.02955213285231295, 28.73800426594050350 ) ) ;
#63518 = CARTESIAN_POINT ( 'NONE',  ( -105.9103127569300966, -29.99999999999996092, 132.9890815309780123 ) ) ;
#63520 = CIRCLE ( 'NONE', #37751, 1.000000000000002442 ) ;
#63521 = CARTESIAN_POINT ( 'NONE',  ( 86.44549218974457006, -37.99999999999996447, 55.87897762973370419 ) ) ;
#63522 = CARTESIAN_POINT ( 'NONE',  ( -47.00724124947766569, -49.90210803779500282, 49.27523530523148310 ) ) ;
#63523 = CARTESIAN_POINT ( 'NONE',  ( 5.615011524526196673, -65.90784209089324008, 14.17484251393565309 ) ) ;
#63524 = EDGE_LOOP ( 'NONE', ( #25612, #77761 ) ) ;
#63525 = CARTESIAN_POINT ( 'NONE',  ( 0.9522645442514227065, 8.765251389120953363, -51.31355066132082499 ) ) ;
#63526 = CIRCLE ( 'NONE', #32583, 5.000000000000010658 ) ;
#63527 = SURFACE_STYLE_USAGE ( .BOTH. , #62460 ) ;
#63528 = CARTESIAN_POINT ( 'NONE',  ( 1.496989374907367739E-10, 304.8518027762758607, -10.00000000000000533 ) ) ;
#63529 = CARTESIAN_POINT ( 'NONE',  ( 28.21644434148578640, 308.7733337496239301, -9.112255642778062992 ) ) ;
#63530 = ORIENTED_EDGE ( 'NONE', *, *, #75555, .T. ) ;
#63531 = CARTESIAN_POINT ( 'NONE',  ( -12.97770155848252926, -9.693230400136535252, 11.45906137556292670 ) ) ;
#63532 = B_SPLINE_CURVE_WITH_KNOTS ( 'NONE', 3,
 ( #92213, #32959, #73909, #57188, #43157, #50679, #1056, #34031 ),
 .UNSPECIFIED., .F., .F.,
 ( 4, 2, 2, 4 ),
 ( 1.852685484479510593E-18, 0.0001460451837441709491, 0.0002190677756162548516, 0.0002920903674883387540 ),
 .UNSPECIFIED. ) ;
#63533 = VERTEX_POINT ( 'NONE', #43639 ) ;
#63534 = CARTESIAN_POINT ( 'NONE',  ( 79.37892552202683305, -30.00000000001325162, 188.6526249938534647 ) ) ;
#63535 = CARTESIAN_POINT ( 'NONE',  ( 8.572527594031477134E-16, -50.00000000000000000, 105.0000000000000000 ) ) ;
#63536 = CARTESIAN_POINT ( 'NONE',  ( 6.846705483647400392, 41.84866126346769732, -59.70429168036804413 ) ) ;
#63537 = CARTESIAN_POINT ( 'NONE',  ( 1.722054852581828504E-15, 24.73290587908618932, 14.06164498842270483 ) ) ;
#63538 = CARTESIAN_POINT ( 'NONE',  ( 99.39107893597980592, -30.00000000000000355, 187.8633685902540833 ) ) ;
#63539 = CARTESIAN_POINT ( 'NONE',  ( -0.9549771330164267269, 36.45450309182552928, 29.31067408448910427 ) ) ;
#63540 = EDGE_LOOP ( 'NONE', ( #106156, #74641, #36715, #33161, #54642 ) ) ;
#63541 = CIRCLE ( 'NONE', #27395, 5.000000000000010658 ) ;
#63542 = ORIENTED_EDGE ( 'NONE', *, *, #61234, .F. ) ;
#63543 = ORIENTED_EDGE ( 'NONE', *, *, #74556, .T. ) ;
#63545 = AXIS2_PLACEMENT_3D ( 'NONE', #23808, #90634, #40484 ) ;
#63544 = DIRECTION ( 'NONE',  ( -2.775557561562873681E-14, 0.9795142562460142921, -0.2013748291391392609 ) ) ;
#63546 = DIRECTION ( 'NONE',  ( 0.000000000000000000, -1.000000000000000000, 0.000000000000000000 ) ) ;
#63547 = DIRECTION ( 'NONE',  ( -0.000000000000000000, -0.000000000000000000, -1.000000000000000000 ) ) ;
#63549 = ORIENTED_EDGE ( 'NONE', *, *, #22066, .F. ) ;
#63548 = CIRCLE ( 'NONE', #17034, 5.000000000000001776 ) ;
#63551 = ADVANCED_FACE ( 'NONE', ( #76528 ), #85367, .F. ) ;
#63550 = CARTESIAN_POINT ( 'NONE',  ( 21.36650669486618881, -3.999999999999998224, 0.000000000000000000 ) ) ;
#63552 = CIRCLE ( 'NONE', #29163, 13.00000000000000000 ) ;
#63553 = ORIENTED_EDGE ( 'NONE', *, *, #92248, .F. ) ;
#63554 = CARTESIAN_POINT ( 'NONE',  ( 41.82792046605465686, 5.000000000000015099, 6.123233995736782060E-16 ) ) ;
#63555 = CARTESIAN_POINT ( 'NONE',  ( 103.1879948328108867, -38.42420025606666911, 198.9909334126319891 ) ) ;
#63556 = CYLINDRICAL_SURFACE ( 'NONE', #9538, 4.000000000000000888 ) ;
#63557 = CARTESIAN_POINT ( 'NONE',  ( 87.03046627057608475, -60.19227689608176490, -6.658524423245185453 ) ) ;
#63558 = CARTESIAN_POINT ( 'NONE',  ( 58.09934139907505113, -38.00000000000000000, 66.71623766452258053 ) ) ;
#63559 = CARTESIAN_POINT ( 'NONE',  ( 37.81751640206508114, 309.3200808856390722, 5.370049675488317575 ) ) ;
#63560 = DIRECTION ( 'NONE',  ( 0.000000000000000000, -1.000000000000000000, 0.000000000000000000 ) ) ;
#63561 = COLOUR_RGB ( '', 0.72549020, 0.75294118, 0.79215686) ;
#63562 = DIRECTION ( 'NONE',  ( 0.000000000000000000, 0.000000000000000000, 1.000000000000000000 ) ) ;
#63563 =( LENGTH_UNIT ( ) NAMED_UNIT ( * ) SI_UNIT ( .MILLI., .METRE. ) );
#63564 = DIRECTION ( 'NONE',  ( 1.000000000000000000, 0.000000000000000000, 0.000000000000000000 ) ) ;
#63565 = VERTEX_POINT ( 'NONE', #2638 ) ;
#63566 = ADVANCED_FACE ( 'NONE', ( #63022 ), #6346, .F. ) ;
#63567 = EDGE_CURVE ( 'NONE', #92669, #75344, #46305, .T. ) ;
#63568 = CARTESIAN_POINT ( 'NONE',  ( -9.981531048852469112, 15.23280014800326398, -0.7018335428337003634 ) ) ;
#63569 = CARTESIAN_POINT ( 'NONE',  ( -38.73386039799286351, 460.3889633641963428, 2.371405894922548274 ) ) ;
#63570 = CARTESIAN_POINT ( 'NONE',  ( -25.86049976764029523, 37.20180571946941228, 8.663517206654082869 ) ) ;
#63571 = VERTEX_POINT ( 'NONE', #95384 ) ;
#63572 = CARTESIAN_POINT ( 'NONE',  ( -42.60956082011767165, 435.9305394648018250, 18.66091589584682708 ) ) ;
#63573 = AXIS2_PLACEMENT_3D ( 'NONE', #100425, #60007, #9810 ) ;
#63574 = CARTESIAN_POINT ( 'NONE',  ( -33.01221401996102145, 301.6247609887375916, 11.48415791863079427 ) ) ;
#63575 = CARTESIAN_POINT ( 'NONE',  ( -12.48746907676934370, -3.545640499966867143, -76.71370838498235400 ) ) ;
#63576 = UNCERTAINTY_MEASURE_WITH_UNIT (LENGTH_MEASURE( 1.000000000000000082E-05 ), #57167, 'distance_accuracy_value', 'NONE');
#63577 = DIRECTION ( 'NONE',  ( 0.000000000000000000, -1.000000000000000000, 0.000000000000000000 ) ) ;
#63578 = CARTESIAN_POINT ( 'NONE',  ( -8.000000000000000000, -16.24999999999999289, -9.797174393178825657E-16 ) ) ;
#63579 = CARTESIAN_POINT ( 'NONE',  ( -7.032460429402416224, -15.50966336658045819, 34.57368686681926562 ) ) ;
#63580 = DIRECTION ( 'NONE',  ( 1.000000000000000000, 0.000000000000000000, 0.000000000000000000 ) ) ;
#63581 = ORIENTED_EDGE ( 'NONE', *, *, #77742, .F. ) ;
#63582 = CARTESIAN_POINT ( 'NONE',  ( 85.87277015767610067, -32.01287046823524207, 183.1770543038046526 ) ) ;
#63583 = CARTESIAN_POINT ( 'NONE',  ( -38.81963395482446089, 27.30149883538651778, 12.34989123519421206 ) ) ;
#63584 = ADVANCED_FACE ( 'NONE', ( #38239 ), #44852, .F. ) ;
#63585 = VECTOR ( 'NONE', #35227, 1000.000000000000000 ) ;
#63586 = DIRECTION ( 'NONE',  ( -0.5735764363510497121, 0.8191520442889892450, 1.003171929053521665E-16 ) ) ;
#63587 = VERTEX_POINT ( 'NONE', #25799 ) ;
#63588 = CARTESIAN_POINT ( 'NONE',  ( 94.41251621664974891, -57.67095265337347598, -0.3265171029545638759 ) ) ;
#63589 = CARTESIAN_POINT ( 'NONE',  ( 36.54117467508514494, 437.9945884957556927, 4.200333155679382813 ) ) ;
#63590 = CARTESIAN_POINT ( 'NONE',  ( -30.87917441950785857, 8.312254468506221627, 41.23121050640273921 ) ) ;
#63591 = CARTESIAN_POINT ( 'NONE',  ( 28.53023071193278426, 11.34323491540342488, 41.35403323942976783 ) ) ;
#63592 = EDGE_CURVE ( 'NONE', #29730, #62962, #17661, .T. ) ;
#63593 = CARTESIAN_POINT ( 'NONE',  ( 0.000000000000000000, 0.000000000000000000, 0.000000000000000000 ) ) ;
#63594 = CARTESIAN_POINT ( 'NONE',  ( 0.000000000000000000, -5.000000000000000000, 10.00000000000000000 ) ) ;
#63595 = CARTESIAN_POINT ( 'NONE',  ( 35.00384615384614762, 4.172000000000003261, 5.109226446042759579E-16 ) ) ;
#63596 = EDGE_CURVE ( 'NONE', #102391, #4391, #76726, .T. ) ;
#63597 = AXIS2_PLACEMENT_3D ( 'NONE', #76155, #98316, #26598 ) ;
#63599 = CARTESIAN_POINT ( 'NONE',  ( -11.11281763409552603, 8.399929652088387044, 9.811721095437990314 ) ) ;
#63598 = DIRECTION ( 'NONE',  ( 0.000000000000000000, -1.000000000000000000, 0.000000000000000000 ) ) ;
#63600 = CARTESIAN_POINT ( 'NONE',  ( 9.789044728060074974, 294.6486233851414909, -2.043184600578055843 ) ) ;
#63601 = CARTESIAN_POINT ( 'NONE',  ( 40.73878142687892279, 503.7113041876743864, 10.19672445236252045 ) ) ;
#63602 = CARTESIAN_POINT ( 'NONE',  ( -27.72596789763197478, 36.41250443191194819, -9.903931038345092475 ) ) ;
#63603 = DIRECTION ( 'NONE',  ( 1.000000000000000000, 0.000000000000000000, 0.000000000000000000 ) ) ;
#63604 = FACE_OUTER_BOUND ( 'NONE', #24430, .T. ) ;
#63605 = CIRCLE ( 'NONE', #75656, 2.999999999999999112 ) ;
#63606 = PRESENTATION_LAYER_ASSIGNMENT (  '', '', ( #91169 ) ) ;
#63607 = CARTESIAN_POINT ( 'NONE',  ( -82.49874227244829683, -38.00000000000002842, 7.946081593716382230 ) ) ;
#63608 = EDGE_CURVE ( 'NONE', #58522, #90581, #6444, .T. ) ;
#63609 = ORIENTED_EDGE ( 'NONE', *, *, #20142, .F. ) ;
#63610 = FILL_AREA_STYLE_COLOUR ( '', #87560 ) ;
#63611 = CARTESIAN_POINT ( 'NONE',  ( 0.000000000000000000, 0.000000000000000000, -0.02540000000000007530 ) ) ;
#63612 = CARTESIAN_POINT ( 'NONE',  ( -10.98135972349570721, -16.40382455065010703, -34.73165818216984491 ) ) ;
#63614 = CARTESIAN_POINT ( 'NONE',  ( -59.93268390808485435, -47.40894763362151565, -27.52547626314329321 ) ) ;
#63613 = CARTESIAN_POINT ( 'NONE',  ( 18.00000000000001421, -20.00000000000001776, 9.000000000000007105 ) ) ;
#63615 = ORIENTED_EDGE ( 'NONE', *, *, #46484, .F. ) ;
#63616 = STYLED_ITEM ( 'NONE', ( #33924 ), #45229 ) ;
#63617 = LINE ( 'NONE', #78699, #23806 ) ;
#63618 = CONICAL_SURFACE ( 'NONE', #54953, 7.500000000000000888, 0.8594454914424817238 ) ;
#63619 = ORIENTED_EDGE ( 'NONE', *, *, #88138, .T. ) ;
#63620 = AXIS2_PLACEMENT_3D ( 'NONE', #80897, #49051, #63685 ) ;
#63621 = CARTESIAN_POINT ( 'NONE',  ( 5.819846122303830249, 6.321060697774965931, 2.051601713726983078 ) ) ;
#63622 = CARTESIAN_POINT ( 'NONE',  ( 22.33349330513380693, 4.000000000000003553, 0.000000000000000000 ) ) ;
#63623 = CARTESIAN_POINT ( 'NONE',  ( -92.60969381247451793, -60.00000000000000000, -10.21457394295196863 ) ) ;
#63624 = VERTEX_POINT ( 'NONE', #89425 ) ;
#63625 = CARTESIAN_POINT ( 'NONE',  ( -7.416129379031016100, 42.00000000000000000, -59.68109090348218615 ) ) ;
#63626 = CARTESIAN_POINT ( 'NONE',  ( -7.940862310547813330, 54.17408618097004336, -1.683098319245891039 ) ) ;
#63627 = CARTESIAN_POINT ( 'NONE',  ( 101.2899080087397437, -60.24371164881011964, 194.9002588125513284 ) ) ;
#63629 = DIRECTION ( 'NONE',  ( 0.000000000000000000, -1.000000000000000000, 0.000000000000000000 ) ) ;
#63628 = FACE_OUTER_BOUND ( 'NONE', #54530, .T. ) ;
#63630 = CARTESIAN_POINT ( 'NONE',  ( -84.35902549046055299, -25.57579481131011079, 160.3285692841058676 ) ) ;
#63631 = EDGE_LOOP ( 'NONE', ( #34473, #54620, #38698, #65783 ) ) ;
#63632 = ORIENTED_EDGE ( 'NONE', *, *, #46527, .F. ) ;
#63633 = ORIENTED_EDGE ( 'NONE', *, *, #20515, .F. ) ;
#63634 = CARTESIAN_POINT ( 'NONE',  ( 41.36650669486618881, 4.898587196589411843E-16, -4.000000000000000888 ) ) ;
#63635 = EDGE_CURVE ( 'NONE', #16749, #47728, #932, .T. ) ;
#63636 =( LENGTH_UNIT ( ) NAMED_UNIT ( * ) SI_UNIT ( .MILLI., .METRE. ) );
#63637 = CARTESIAN_POINT ( 'NONE',  ( 48.10000000000000142, 0.000000000000000000, 0.000000000000000000 ) ) ;
#63638 = ORIENTED_EDGE ( 'NONE', *, *, #86675, .F. ) ;
#63639 = DIRECTION ( 'NONE',  ( 0.000000000000000000, 1.000000000000000000, 0.000000000000000000 ) ) ;
#63640 = CARTESIAN_POINT ( 'NONE',  ( 0.7145311798161616545, -4.618802153517262532, -8.000000000000001776 ) ) ;
#63641 = CARTESIAN_POINT ( 'NONE',  ( -80.45353917958989598, -57.50988970295517788, 199.2734438750461550 ) ) ;
#63642 = DIRECTION ( 'NONE',  ( 0.000000000000000000, -1.000000000000000000, 0.000000000000000000 ) ) ;
#63643 = CARTESIAN_POINT ( 'NONE',  ( -64.32470902915410704, 48.00000000000000711, 10.67393577672269167 ) ) ;
#63644 = DIRECTION ( 'NONE',  ( -0.000000000000000000, 1.000000000000000000, -0.000000000000000000 ) ) ;
#63645 = EDGE_CURVE ( 'NONE', #89804, #41582, #4441, .T. ) ;
#63646 = CARTESIAN_POINT ( 'NONE',  ( 89.98361085880227961, -30.00000000000001776, -2.850603255620693055 ) ) ;
#63647 = CARTESIAN_POINT ( 'NONE',  ( -71.62990520600911282, -30.00000000000002842, 135.6731032779996156 ) ) ;
#63648 = CARTESIAN_POINT ( 'NONE',  ( -53.04679035957766331, -60.31687344103399084, 64.32401062991868912 ) ) ;
#63649 = CIRCLE ( 'NONE', #17148, 7.500000000001509015 ) ;
#63650 = ORIENTED_EDGE ( 'NONE', *, *, #54216, .T. ) ;
#63651 = CARTESIAN_POINT ( 'NONE',  ( -1.469576158976823947E-15, -12.87499999999999467, 8.000000000000000000 ) ) ;
#63652 = ORIENTED_EDGE ( 'NONE', *, *, #81486, .T. ) ;
#63653 = CARTESIAN_POINT ( 'NONE',  ( -100.3133252052276561, -45.25861041073478219, 192.2763107763641983 ) ) ;
#63654 = CARTESIAN_POINT ( 'NONE',  ( 32.84951609414348894, 478.7804999730052486, 7.701738758139213381 ) ) ;
#63655 = AXIS2_PLACEMENT_3D ( 'NONE', #21978, #54832, #46755 ) ;
#63656 = ORIENTED_EDGE ( 'NONE', *, *, #10831, .F. ) ;
#63657 = CARTESIAN_POINT ( 'NONE',  ( 19.10507480816155734, 49.67854560040533585, 61.73104169122685647 ) ) ;
#63658 = CARTESIAN_POINT ( 'NONE',  ( 110.9222412389008667, -38.35615538830503368, 167.0140503051813141 ) ) ;
#63659 = FACE_OUTER_BOUND ( 'NONE', #41138, .T. ) ;
#63660 = CARTESIAN_POINT ( 'NONE',  ( 6.826399921716641117, 2.638123634694619746, -6.344399053232583796 ) ) ;
#63661 = CARTESIAN_POINT ( 'NONE',  ( -6.646264631202571493, 302.7439589117898322, 9.914178208445832752 ) ) ;
#63662 = DIRECTION ( 'NONE',  ( 0.000000000000000000, -1.000000000000000000, 0.000000000000000000 ) ) ;
#63663 = CARTESIAN_POINT ( 'NONE',  ( -40.95420997525301487, 387.0967036739339164, 27.26945002580065136 ) ) ;
#63664 = CARTESIAN_POINT ( 'NONE',  ( -9.948648081855438363, 7.573338139540490843, -0.000000000000000000 ) ) ;
#63665 = CARTESIAN_POINT ( 'NONE',  ( 4.038456955263700188, 51.98520879605556644, -7.231977661697025717 ) ) ;
#63666 = DIRECTION ( 'NONE',  ( -1.000000000000000000, -0.000000000000000000, -0.000000000000000000 ) ) ;
#63667 = ADVANCED_FACE ( 'NONE', ( #48406 ), #30267, .T. ) ;
#63668 = CARTESIAN_POINT ( 'NONE',  ( -33.75766768372585602, 485.0582975308881259, 1.699565690038850274 ) ) ;
#63669 = ORIENTED_EDGE ( 'NONE', *, *, #73666, .T. ) ;
#63670 = VERTEX_POINT ( 'NONE', #66194 ) ;
#63671 = CARTESIAN_POINT ( 'NONE',  ( 49.35569166775938044, -53.36311280355247533, 54.26082778344028412 ) ) ;
#63672 = CARTESIAN_POINT ( 'NONE',  ( -0.07745360819684599107, 7.746009256456465764, 51.75000000000001421 ) ) ;
#63673 =( GEOMETRIC_REPRESENTATION_CONTEXT ( 3 ) GLOBAL_UNCERTAINTY_ASSIGNED_CONTEXT ( ( #90573 ) ) GLOBAL_UNIT_ASSIGNED_CONTEXT ( ( #100043, #91442, #26735 ) ) REPRESENTATION_CONTEXT ( 'NONE', 'WORKASPACE' ) );
#63674 = CARTESIAN_POINT ( 'NONE',  ( -6.999768563658489207, 16.99959498610098052, 0.2746924679829753080 ) ) ;
#63676 = EDGE_CURVE ( 'NONE', #72268, #4316, #23639, .T. ) ;
#63675 = CARTESIAN_POINT ( 'NONE',  ( -110.9162687472649225, -38.35621414700798226, 168.5475671580575465 ) ) ;
#63677 = ORIENTED_EDGE ( 'NONE', *, *, #88867, .F. ) ;
#63678 = CARTESIAN_POINT ( 'NONE',  ( 86.87566845558653483, -38.36515140496537413, -20.99884072241187383 ) ) ;
#63679 = CARTESIAN_POINT ( 'NONE',  ( 11.17923199892331887, 10.30837800928391168, -9.638854972992653813 ) ) ;
#63680 = CARTESIAN_POINT ( 'NONE',  ( 42.98746414932995208, 1.482358050883964840E-15, 0.000000000000000000 ) ) ;
#63681 = FACE_OUTER_BOUND ( 'NONE', #56601, .T. ) ;
#63682 = CARTESIAN_POINT ( 'NONE',  ( 95.54615038124083526, -52.71697105530865457, 96.31251485201036644 ) ) ;
#63683 = CARTESIAN_POINT ( 'NONE',  ( -31.61871763008401715, 439.0122406652411655, 23.38971322451639168 ) ) ;
#63684 = VECTOR ( 'NONE', #72291, 1000.000000000000000 ) ;
#63685 = DIRECTION ( 'NONE',  ( 0.000000000000000000, 0.000000000000000000, 1.000000000000000000 ) ) ;
#63686 = CARTESIAN_POINT ( 'NONE',  ( -36.74064224167297965, 397.1769660793155481, 6.182558990302069013 ) ) ;
#63687 = DIRECTION ( 'NONE',  ( 0.000000000000000000, -1.000000000000000000, 0.000000000000000000 ) ) ;
#63688 = CARTESIAN_POINT ( 'NONE',  ( 10.50000000000000711, -5.000000000000000000, -78.42624373368740009 ) ) ;
#63689 = CARTESIAN_POINT ( 'NONE',  ( 92.16328301628017527, -60.00000000000002132, 202.3748522514294450 ) ) ;
#63690 = CARTESIAN_POINT ( 'NONE',  ( -15.53255836610350116, 34.96781356575814215, 22.77000419570328305 ) ) ;
#63691 = ORIENTED_EDGE ( 'NONE', *, *, #27848, .F. ) ;
#63692 = CARTESIAN_POINT ( 'NONE',  ( 57.09500382191800583, -60.32684846654004929, 74.31043819818451368 ) ) ;
#63693 = CARTESIAN_POINT ( 'NONE',  ( -35.39714039450764460, 301.8757354096758263, -8.412418780513528205 ) ) ;
#63694 = EDGE_CURVE ( 'NONE', #56403, #67861, #67038, .T. ) ;
#63695 = CARTESIAN_POINT ( 'NONE',  ( 7.896254658894421574, 33.78929182754200156, 1.307282859663294383 ) ) ;
#63696 = AXIS2_PLACEMENT_3D ( 'NONE', #2452, #101160, #58585 ) ;
#63697 = CARTESIAN_POINT ( 'NONE',  ( -13.49999999999999822, -6.526560492696113158, -12.16017290538970563 ) ) ;
#63698 = VERTEX_POINT ( 'NONE', #9540 ) ;
#63700 = CARTESIAN_POINT ( 'NONE',  ( -9.521335790331885818, -51.55696187956029064, 23.93938989165062026 ) ) ;
#63699 = CARTESIAN_POINT ( 'NONE',  ( -109.5143122852008446, -38.35607115667316691, 149.0097679660275674 ) ) ;
#63701 = DIRECTION ( 'NONE',  ( 0.9915366780650395340, -0.1269898409407454742, -0.02699252395739042479 ) ) ;
#63702 = CARTESIAN_POINT ( 'NONE',  ( 29.00671329096065421, 320.5761524563107514, 12.81707940767795506 ) ) ;
#63703 = PRESENTATION_STYLE_ASSIGNMENT (( #62121 ) ) ;
#63704 = AXIS2_PLACEMENT_3D ( 'NONE', #7303, #75774, #27811 ) ;
#63705 = CARTESIAN_POINT ( 'NONE',  ( -2.977408999572650039, -10.06250000204838280, -7.188101187500001821 ) ) ;
#63706 = CARTESIAN_POINT ( 'NONE',  ( -6.145467200824003662, -3.000000000000002665, -92.99666842290695001 ) ) ;
#63707 = DIRECTION ( 'NONE',  ( -0.000000000000000000, 1.000000000000000000, 0.000000000000000000 ) ) ;
#63708 = MECHANICAL_DESIGN_GEOMETRIC_PRESENTATION_REPRESENTATION (  '', ( #55045 ), #91276 ) ;
#63709 = EDGE_LOOP ( 'NONE', ( #92639, #8597, #78097, #75826, #70201, #33410, #19897, #59804 ) ) ;
#63710 = CARTESIAN_POINT ( 'NONE',  ( 83.53591657301284101, -39.46790697894184774, 174.7263257596978576 ) ) ;
#63711 = CARTESIAN_POINT ( 'NONE',  ( -46.00000000000000000, 461.5066419892383465, 9.508543545636769068 ) ) ;
#63712 = CARTESIAN_POINT ( 'NONE',  ( -37.10378445358433908, 439.7078499482008738, 24.11597218741631465 ) ) ;
#63713 = ORIENTED_EDGE ( 'NONE', *, *, #19756, .F. ) ;
#63714 = DIRECTION ( 'NONE',  ( -1.000000000000000000, -1.224606353822377258E-16, -0.000000000000000000 ) ) ;
#63715 = CARTESIAN_POINT ( 'NONE',  ( 6.738141070036304470, -4.358126490543009268, -16.85492060642630818 ) ) ;
#63716 = DIRECTION ( 'NONE',  ( 0.000000000000000000, 1.000000000000000000, 0.000000000000000000 ) ) ;
#63717 = CARTESIAN_POINT ( 'NONE',  ( 14.59153803999176802, 1.704952136592581935, -3.465235867580846563 ) ) ;
#63718 = DIRECTION ( 'NONE',  ( -0.000000000000000000, 1.000000000000000000, -0.000000000000000000 ) ) ;
#63719 = AXIS2_PLACEMENT_3D ( 'NONE', #92033, #18167, #1947 ) ;
#63720 = EDGE_CURVE ( 'NONE', #70305, #49400, #104298, .T. ) ;
#63721 = ORIENTED_EDGE ( 'NONE', *, *, #38775, .T. ) ;
#63722 = PRESENTATION_STYLE_ASSIGNMENT (( #38390 ) ) ;
#63723 = CIRCLE ( 'NONE', #36182, 4.000000000000000888 ) ;
#63724 = CARTESIAN_POINT ( 'NONE',  ( 6.499999999999999112, 1.355443906731582659, -5.756734754743127347 ) ) ;
#63725 = CARTESIAN_POINT ( 'NONE',  ( 1.250782632067709566, 25.50131467620691694, 39.81516996845464007 ) ) ;
#63726 = EDGE_CURVE ( 'NONE', #91723, #61967, #2665, .T. ) ;
#63728 = CARTESIAN_POINT ( 'NONE',  ( -10.62175334653542791, 14.24948917130530113, -9.926452663087374617 ) ) ;
#63727 = CARTESIAN_POINT ( 'NONE',  ( -0.04262759816315875305, -18.02988087835976927, 35.00498014658149515 ) ) ;
#63729 = CIRCLE ( 'NONE', #17220, 0.9999999999999993339 ) ;
#63730 = CARTESIAN_POINT ( 'NONE',  ( -5.082755093536325042, -18.59375000204838457, -5.082755093536325930 ) ) ;
#63731 = CARTESIAN_POINT ( 'NONE',  ( -23.38163988282185812, 40.83906611472609427, 60.94087333793187611 ) ) ;
#63732 = FACE_OUTER_BOUND ( 'NONE', #90426, .T. ) ;
#63733 = AXIS2_PLACEMENT_3D ( 'NONE', #62828, #104873, #46626 ) ;
#63734 = ORIENTED_EDGE ( 'NONE', *, *, #17969, .F. ) ;
#63735 = EDGE_CURVE ( 'NONE', #92331, #35260, #88830, .T. ) ;
#63736 = CARTESIAN_POINT ( 'NONE',  ( 46.85000000000000142, 0.000000000000000000, 0.000000000000000000 ) ) ;
#63737 = CARTESIAN_POINT ( 'NONE',  ( -6.827804075409870777, -2.999999999999648281, -71.19745151638491620 ) ) ;
#63738 = DIRECTION ( 'NONE',  ( 0.000000000000000000, 1.000000000000000000, 0.000000000000000000 ) ) ;
#63739 = VERTEX_POINT ( 'NONE', #36540 ) ;
#63740 = CARTESIAN_POINT ( 'NONE',  ( 43.71217423904096222, 435.6632154632235938, 9.092528312217307729 ) ) ;
#63741 = CARTESIAN_POINT ( 'NONE',  ( 0.000000000000000000, 0.000000000000000000, -10.00000000000000000 ) ) ;
#63742 = ORIENTED_EDGE ( 'NONE', *, *, #95544, .F. ) ;
#63743 = DIRECTION ( 'NONE',  ( -1.000000000000000000, -1.224606353822377258E-16, -0.000000000000000000 ) ) ;
#63744 = FACE_OUTER_BOUND ( 'NONE', #104172, .T. ) ;
#63745 = CARTESIAN_POINT ( 'NONE',  ( -48.49771892682847607, 39.00440505407896552, -41.54732596423969682 ) ) ;
#63746 = CARTESIAN_POINT ( 'NONE',  ( -110.1395483373692912, -60.00000000000000000, 144.5712075343598713 ) ) ;
#63747 = CARTESIAN_POINT ( 'NONE',  ( 0.000000000000000000, -54.00000000000000711, 27.00000000000000000 ) ) ;
#63748 = CARTESIAN_POINT ( 'NONE',  ( 29.45362385905110969, 325.9253963054578662, 15.14270878922920716 ) ) ;
#63749 = CARTESIAN_POINT ( 'NONE',  ( 6.488675057781621902, 53.47862480557490983, -7.645533103099348082 ) ) ;
#63750 = CARTESIAN_POINT ( 'NONE',  ( 1.570796324980112679, -5.000000000000002665, -73.00000000000001421 ) ) ;
#63751 = CARTESIAN_POINT ( 'NONE',  ( -83.03303802707752368, -46.50676638669730067, 179.9281315098355947 ) ) ;
#63752 = ORIENTED_EDGE ( 'NONE', *, *, #5294, .T. ) ;
#63753 = CARTESIAN_POINT ( 'NONE',  ( 25.57097515258701748, 43.61428196877569263, -75.34572123083053441 ) ) ;
#63754 = VERTEX_POINT ( 'NONE', #10086 ) ;
#63755 = ADVANCED_FACE ( 'NONE', ( #100683 ), #44035, .T. ) ;
#63756 = CARTESIAN_POINT ( 'NONE',  ( 4.589925132946514275, -66.06526016292515635, 3.864926970398267603 ) ) ;
#63757 = CARTESIAN_POINT ( 'NONE',  ( -84.06247081757707917, -45.26549463277890339, 23.57487689052427982 ) ) ;
#63758 = PLANE ( 'NONE',  #49485 ) ;
#63759 = DIRECTION ( 'NONE',  ( -0.000000000000000000, 1.000000000000000000, -0.000000000000000000 ) ) ;
#63760 = CARTESIAN_POINT ( 'NONE',  ( 9.439578325717800311, 10.07476781602096239, 3.068995344595395032E-13 ) ) ;
#63761 = CARTESIAN_POINT ( 'NONE',  ( -5.699988423468465903, -4.591578518468272030, -6.344710093416088270 ) ) ;
#63762 = CARTESIAN_POINT ( 'NONE',  ( 21.08349330513380693, 1.593028355512270962E-15, 0.000000000000000000 ) ) ;
#63763 = EDGE_CURVE ( 'NONE', #31339, #74683, #73251, .T. ) ;
#63764 = CARTESIAN_POINT ( 'NONE',  ( 104.4175052224803864, -30.00000000000007105, 196.2185630211469629 ) ) ;
#63765 = CIRCLE ( 'NONE', #62094, 5.000000000000002665 ) ;
#63766 = CARTESIAN_POINT ( 'NONE',  ( -89.60210353745294753, -14.21045842199431597, 48.51666376363581890 ) ) ;
#63767 = B_SPLINE_CURVE_WITH_KNOTS ( 'NONE', 3,
 ( #20929, #30578, #46214, #80153, #61889, #39191, #79100, #4695, #5224, #20400, #38152, #78045 ),
 .UNSPECIFIED., .F., .F.,
 ( 4, 2, 2, 2, 2, 4 ),
 ( 0.05929940015525115432, 0.06027543776436967288, 0.06125147537348819143, 0.06320355059172522161, 0.06515562580996224484, 0.06710770102819928196 ),
 .UNSPECIFIED. ) ;
#63768 = CARTESIAN_POINT ( 'NONE',  ( -62.79330346830408160, -42.96297999032424286, 81.57255440324702533 ) ) ;
#63769 = ORIENTED_EDGE ( 'NONE', *, *, #7455, .T. ) ;
#63770 = CARTESIAN_POINT ( 'NONE',  ( -55.03799937935021802, 39.42592066847770127, 34.70786362942529735 ) ) ;
#63771 = CARTESIAN_POINT ( 'NONE',  ( 92.02246887588820812, -59.99999999997538680, 204.8145644407424584 ) ) ;
#63772 = ORIENTED_EDGE ( 'NONE', *, *, #101380, .F. ) ;
#63773 = CARTESIAN_POINT ( 'NONE',  ( 3.091518739326764464, -60.35886547126050772, 33.94409813261457032 ) ) ;
#63774 = CARTESIAN_POINT ( 'NONE',  ( 7.188101187500000044, -21.03125000204838813, 0.000000000000000000 ) ) ;
#63775 = B_SPLINE_CURVE_WITH_KNOTS ( 'NONE', 3,
 ( #68402, #10144, #85652, #10665, #18269, #67858, #18819, #43059, #2045, #43580, #69462, #101813, #60325, #34469, #44664, #42511, #51123, #92659, #75946, #3665, #68938, #51661, #27978, #77548, #93733, #92123, #83499, #84584, #36599, #59783, #76467, #11724, #2578, #44123 ),
 .UNSPECIFIED., .F., .F.,
 ( 4, 2, 2, 2, 2, 2, 2, 2, 2, 2, 2, 2, 2, 2, 2, 2, 4 ),
 ( 0.01272238763756221303, 0.01351613129786393037, 0.01430987495816564599, 0.01510361861846736334, 0.01589736227876907895, 0.01669110593907079804, 0.01748484959937251712, 0.01827859325967423273, 0.01907233691997595182, 0.01986608058027767090, 0.02065982424057938999, 0.02145356790088110560, 0.02224731156118282469, 0.02304105522148454377, 0.02383479888178625938, 0.02462854254208798194, 0.02542228620238969755 ),
 .UNSPECIFIED. ) ;
#63776 = FILL_AREA_STYLE_COLOUR ( '', #39075 ) ;
#63777 = ORIENTED_EDGE ( 'NONE', *, *, #54559, .T. ) ;
#63778 = CARTESIAN_POINT ( 'NONE',  ( -10.61273427954654736, 46.03711080233982500, 12.94042145964155210 ) ) ;
#63779 = VERTEX_POINT ( 'NONE', #28435 ) ;
#63780 = DIRECTION ( 'NONE',  ( -1.000000000000000000, -1.224606353822377258E-16, -0.000000000000000000 ) ) ;
#63781 = FACE_OUTER_BOUND ( 'NONE', #64494, .T. ) ;
#63782 = CARTESIAN_POINT ( 'NONE',  ( -111.4049543193486329, -60.00000000000000000, 185.1671540497623880 ) ) ;
#63783 = CARTESIAN_POINT ( 'NONE',  ( 9.113097280746996987, -54.00000000000000711, 31.11721482942554928 ) ) ;
#63784 = CARTESIAN_POINT ( 'NONE',  ( 2.977408999572650927, -26.75000000204838457, -7.188101187500001821 ) ) ;
#63785 = CONICAL_SURFACE ( 'NONE', #27875, 3.340000000000000746, 0.9599310885968781459 ) ;
#63786 = DIRECTION ( 'NONE',  ( -1.000000000000000000, -1.224606353822377258E-16, -0.000000000000000000 ) ) ;
#63787 = CARTESIAN_POINT ( 'NONE',  ( -32.80436725737452974, 485.2967250516979902, 5.900038805304054890 ) ) ;
#63788 = CARTESIAN_POINT ( 'NONE',  ( 1.000000000000000000, -64.69017754617701144, 10.12118620307032302 ) ) ;
#63789 = VECTOR ( 'NONE', #101997, 1000.000000000000000 ) ;
#63790 = CARTESIAN_POINT ( 'NONE',  ( 9.999999999999989342, 49.99999999999999289, -83.69100306251233690 ) ) ;
#63791 = CARTESIAN_POINT ( 'NONE',  ( 0.5805565836007667846, -3.752776749732578132, -6.500000000000000888 ) ) ;
#63792 = ADVANCED_FACE ( 'NONE', ( #11130 ), #37288, .T. ) ;
#63793 = CARTESIAN_POINT ( 'NONE',  ( 99.65386729655308784, -60.00000000000000000, 195.9220411359386560 ) ) ;
#63794 = CARTESIAN_POINT ( 'NONE',  ( -37.34066781863991480, -46.43450374261344393, 38.17834207212992226 ) ) ;
#63795 = ORIENTED_EDGE ( 'NONE', *, *, #74446, .T. ) ;
#63796 = DIRECTION ( 'NONE',  ( -1.000000000000000000, -1.224606353822377258E-16, -0.000000000000000000 ) ) ;
#63797 = CARTESIAN_POINT ( 'NONE',  ( 38.65958381579444136, -29.13907093716015950, 35.42191563165732049 ) ) ;
#63798 = CARTESIAN_POINT ( 'NONE',  ( 22.23822744035697241, -8.673617379884035472E-16, 2.910977163136220014 ) ) ;
#63799 = VERTEX_POINT ( 'NONE', #35467 ) ;
#63800 = CARTESIAN_POINT ( 'NONE',  ( 34.29149597935467852, 464.1889238633704622, 18.11295844621604445 ) ) ;
#63801 = CIRCLE ( 'NONE', #44865, 4.000000000000001776 ) ;
#63802 = CARTESIAN_POINT ( 'NONE',  ( -74.13051718845747473, -38.32750755219241512, 161.4754845552919278 ) ) ;
#63803 = ORIENTED_EDGE ( 'NONE', *, *, #72083, .F. ) ;
#63805 = CARTESIAN_POINT ( 'NONE',  ( 21.51569398614858031, 294.9107018935607130, -9.987480606144490736 ) ) ;
#63804 = CARTESIAN_POINT ( 'NONE',  ( 9.359070339229566216, -5.000000000000000000, -18.64538651940581815 ) ) ;
#63806 = CARTESIAN_POINT ( 'NONE',  ( -33.00795325653299983, 439.3958174160655403, 23.82489859418982192 ) ) ;
#63807 = CARTESIAN_POINT ( 'NONE',  ( -33.95156263172582101, 464.5083255208627975, 6.608064661821575037 ) ) ;
#63808 = DIRECTION ( 'NONE',  ( -1.000000000000000000, 0.000000000000000000, 0.000000000000000000 ) ) ;
#63809 = CARTESIAN_POINT ( 'NONE',  ( 2.500000000000000444, -30.00000000000000000, 28.88619651857252535 ) ) ;
#63810 = CARTESIAN_POINT ( 'NONE',  ( -10.00000000000000355, 15.00000000000000000, -10.00000000000000000 ) ) ;
#63811 = SURFACE_SIDE_STYLE ('',( #63278 ) ) ;
#63812 = VECTOR ( 'NONE', #26792, 1000.000000000000000 ) ;
#63813 = CARTESIAN_POINT ( 'NONE',  ( 93.34451349968284717, -59.99999999999999289, 35.61397960305716026 ) ) ;
#63814 = CARTESIAN_POINT ( 'NONE',  ( 0.05458999538772730392, -1.264741368073330818, 6.499999999999999112 ) ) ;
#63815 = DIRECTION ( 'NONE',  ( 0.000000000000000000, 0.000000000000000000, -1.000000000000000000 ) ) ;
#63816 = CARTESIAN_POINT ( 'NONE',  ( 0.000000000000000000, 0.000000000000000000, -10.00000000000000000 ) ) ;
#63817 = EDGE_LOOP ( 'NONE', ( #102295, #62876, #11667, #71314, #95373, #56736 ) ) ;
#63818 = CARTESIAN_POINT ( 'NONE',  ( -85.26311336406097041, -29.99999999999986855, 172.8326700376237284 ) ) ;
#63819 = EDGE_LOOP ( 'NONE', ( #26700, #103489, #64893, #30941 ) ) ;
#63820 = CARTESIAN_POINT ( 'NONE',  ( -9.995225837605406838, -57.97473475263401355, 26.59626811386029743 ) ) ;
#63821 = CARTESIAN_POINT ( 'NONE',  ( -16.01731991787316645, 3.900165755870967033, 1.616345057655150574 ) ) ;
#63822 = CARTESIAN_POINT ( 'NONE',  ( 9.609486011791082305, 8.908497650349785246, 5.000000000000000888 ) ) ;
#63823 = DIRECTION ( 'NONE',  ( -1.000000000000000000, 0.000000000000000000, 0.000000000000000000 ) ) ;
#63824 = DIRECTION ( 'NONE',  ( -1.000000000000000000, -0.000000000000000000, -0.000000000000000000 ) ) ;
#63825 = CARTESIAN_POINT ( 'NONE',  ( -1.320432766682874540E-15, -27.40625000204838813, 7.188101187500000044 ) ) ;
#63826 = AXIS2_PLACEMENT_3D ( 'NONE', #10245, #51219, #42080 ) ;
#63827 = CYLINDRICAL_SURFACE ( 'NONE', #86360, 4.000000000000000888 ) ;
#63828 = CARTESIAN_POINT ( 'NONE',  ( 6.249999999999998224, 8.000000000000000000, 0.000000000000000000 ) ) ;
#63829 = CARTESIAN_POINT ( 'NONE',  ( 7.125691916903468481, 41.67430808309654822, -69.26730091920677523 ) ) ;
#63830 = ORIENTED_EDGE ( 'NONE', *, *, #11277, .F. ) ;
#63831 = APPLICATION_CONTEXT ( 'automotive_design' ) ;
#63833 = ORIENTED_EDGE ( 'NONE', *, *, #41416, .T. ) ;
#63832 = CARTESIAN_POINT ( 'NONE',  ( -13.00000000000003730, -85.00000000000000000, -4.000000000000001776 ) ) ;
#63834 = CARTESIAN_POINT ( 'NONE',  ( 83.49039785751061515, -22.14967886183166712, 148.6536833251738585 ) ) ;
#63835 = ORIENTED_EDGE ( 'NONE', *, *, #56646, .T. ) ;
#63836 = CARTESIAN_POINT ( 'NONE',  ( -12.50000000000000000, 34.76801716932426700, -54.02619666611344229 ) ) ;
#63837 = CARTESIAN_POINT ( 'NONE',  ( -1.115893604525096228, 14.48218051350517754, -51.08048210849830184 ) ) ;
#63838 = CARTESIAN_POINT ( 'NONE',  ( -5.082755093536326818, -12.21875000204838635, 5.082755093536325042 ) ) ;
#63839 = CARTESIAN_POINT ( 'NONE',  ( 0.06809871960542410174, -7.710219529346603373, 2.645508037661880252 ) ) ;
#63840 = CARTESIAN_POINT ( 'NONE',  ( -28.75444143438830835, -57.68095489456369762, 44.62365432283354494 ) ) ;
#63841 = DIRECTION ( 'NONE',  ( 0.000000000000000000, -1.000000000000000000, 0.000000000000000000 ) ) ;
#63842 = EDGE_CURVE ( 'NONE', #30328, #56878, #16530, .T. ) ;
#63843 = VERTEX_POINT ( 'NONE', #11669 ) ;
#63844 =( LENGTH_UNIT ( ) NAMED_UNIT ( * ) SI_UNIT ( .MILLI., .METRE. ) );
#63845 = EDGE_CURVE ( 'NONE', #97864, #50155, #102698, .T. ) ;
#63846 = CARTESIAN_POINT ( 'NONE',  ( -23.21751746555247919, 25.98869614573810694, 30.70617127781050471 ) ) ;
#63847 = CARTESIAN_POINT ( 'NONE',  ( 3.168296453696582748, 112.8154174887550880, 5.000000000000000000 ) ) ;
#63848 = CARTESIAN_POINT ( 'NONE',  ( 7.294237765485898528, 41.09455117511487288, -58.80184355254267103 ) ) ;
#63849 = ADVANCED_FACE ( 'NONE', ( #76948 ), #92355, .T. ) ;
#63850 = CARTESIAN_POINT ( 'NONE',  ( 48.48308721883813632, 13.98293033111261785, -16.77185627386677425 ) ) ;
#63851 = ORIENTED_EDGE ( 'NONE', *, *, #4671, .F. ) ;
#63852 = CARTESIAN_POINT ( 'NONE',  ( 8.000000000000000000, -12.68750000409676915, 0.000000000000000000 ) ) ;
#63853 = VECTOR ( 'NONE', #87884, 999.9999999999998863 ) ;
#63854 = CARTESIAN_POINT ( 'NONE',  ( -10.85562601347594658, -13.98149544789687759, 31.85028796763797487 ) ) ;
#63855 = FILL_AREA_STYLE ('',( #23949 ) ) ;
#63856 = EDGE_CURVE ( 'NONE', #7125, #56853, #93678, .T. ) ;
#63857 = FACE_OUTER_BOUND ( 'NONE', #5025, .T. ) ;
#63858 = DIRECTION ( 'NONE',  ( 0.8191520442889884679, 0.000000000000000000, 0.5735764363510508224 ) ) ;
#63859 = SURFACE_STYLE_USAGE ( .BOTH. , #22881 ) ;
#63860 = SHAPE_DEFINITION_REPRESENTATION ( #95797, #16335 ) ;
#63861 = CARTESIAN_POINT ( 'NONE',  ( -9.918010731619569142, 33.79151684843224501, -1.300854425901587286 ) ) ;
#63862 = ORIENTED_EDGE ( 'NONE', *, *, #86666, .F. ) ;
#63863 = CARTESIAN_POINT ( 'NONE',  ( -5.000000000000003553, -45.99999999999999289, 40.27905619136138426 ) ) ;
#63865 = EDGE_CURVE ( 'NONE', #13191, #34768, #23301, .T. ) ;
#63864 = CIRCLE ( 'NONE', #79315, 1.000000000000021316 ) ;
#63866 = CARTESIAN_POINT ( 'NONE',  ( -3.409011323177015385, 15.24615751665830743, 9.403185743874946212 ) ) ;
#63867 = DIRECTION ( 'NONE',  ( 0.000000000000000000, 0.000000000000000000, -1.000000000000000000 ) ) ;
#63868 = CIRCLE ( 'NONE', #17365, 5.000000000000010658 ) ;
#63869 = CARTESIAN_POINT ( 'NONE',  ( -43.16790182456753655, -33.90049227214078087, -37.13562304484096899 ) ) ;
#63870 = DIRECTION ( 'NONE',  ( 0.000000000000000000, -1.000000000000000000, 0.000000000000000000 ) ) ;
#63871 = DIRECTION ( 'NONE',  ( -1.000000000000000000, -1.224606353822377258E-16, -0.000000000000000000 ) ) ;
#63872 = ORIENTED_EDGE ( 'NONE', *, *, #79278, .F. ) ;
#63873 = AXIS2_PLACEMENT_3D ( 'NONE', #48307, #72592, #97388 ) ;
#63874 = CARTESIAN_POINT ( 'NONE',  ( 0.4988340113754576310, 3.871605243940358765, -8.000000000000001776 ) ) ;
#63875 = CARTESIAN_POINT ( 'NONE',  ( 91.97123957640626202, -57.61548619320129916, 204.3264942780886884 ) ) ;
#63876 = CARTESIAN_POINT ( 'NONE',  ( 58.42741290352864780, -21.77006730897359787, -23.50884316932007678 ) ) ;
#63878 = CARTESIAN_POINT ( 'NONE',  ( -5.744562646538028616, 12.99999999999999289, -4.000000000000000000 ) ) ;
#63877 = VECTOR ( 'NONE', #63707, 1000.000000000000000 ) ;
#63879 = PLANE ( 'NONE',  #12244 ) ;
#63880 = CARTESIAN_POINT ( 'NONE',  ( -6.400037421424863204, 53.43404507722560481, 7.879308159338338946 ) ) ;
#63881 = CARTESIAN_POINT ( 'NONE',  ( -73.23784728930272081, -60.00000000000000711, 164.6514032014629265 ) ) ;
#63882 = CARTESIAN_POINT ( 'NONE',  ( -32.22503847990287795, 485.9064490506194716, 4.829857536089223302 ) ) ;
#63883 =( GEOMETRIC_REPRESENTATION_CONTEXT ( 3 ) GLOBAL_UNCERTAINTY_ASSIGNED_CONTEXT ( ( #90419 ) ) GLOBAL_UNIT_ASSIGNED_CONTEXT ( ( #3003, #11614, #70409 ) ) REPRESENTATION_CONTEXT ( 'NONE', 'WORKASPACE' ) );
#63884 = CARTESIAN_POINT ( 'NONE',  ( 52.56483885390522914, 49.99999999999999289, -38.23529411764705799 ) ) ;
#63885 = CARTESIAN_POINT ( 'NONE',  ( -83.83620841830486370, -61.03244567992550174, 192.0783191055589327 ) ) ;
#63886 = ORIENTED_EDGE ( 'NONE', *, *, #92997, .T. ) ;
#63887 = CARTESIAN_POINT ( 'NONE',  ( 35.76597479665002055, 391.1875820052122776, 5.701159071636620723 ) ) ;
#63888 = VERTEX_POINT ( 'NONE', #22468 ) ;
#63889 = CARTESIAN_POINT ( 'NONE',  ( 10.85300161406142827, -4.996537049336601477, -77.21885189815951378 ) ) ;
#63890 = ADVANCED_FACE ( 'NONE', ( #86136 ), #70983, .F. ) ;
#63891 = CARTESIAN_POINT ( 'NONE',  ( -28.21762564305430487, 307.3147646130399835, -9.222953370498792935 ) ) ;
#63892 = FACE_OUTER_BOUND ( 'NONE', #81136, .T. ) ;
#63893 = CARTESIAN_POINT ( 'NONE',  ( -32.43164319908640891, 464.5283015133046547, 9.485638277864330448 ) ) ;
#63894 = DIRECTION ( 'NONE',  ( -1.000000000000000000, -1.224606353822377258E-16, -0.000000000000000000 ) ) ;
#63895 = EDGE_LOOP ( 'NONE', ( #33706, #104582, #35071, #2685, #48548 ) ) ;
#63896 = AXIS2_PLACEMENT_3D ( 'NONE', #90963, #17071, #82856 ) ;
#63897 = CARTESIAN_POINT ( 'NONE',  ( 17.90864227309694812, 50.00000000000000000, 62.01285158411673137 ) ) ;
#63898 = CARTESIAN_POINT ( 'NONE',  ( 10.52825140974290008, 10.23960916619757100, 10.31893537375141889 ) ) ;
#63899 = ADVANCED_FACE ( 'NONE', ( #96342 ), #75101, .T. ) ;
#63900 = EDGE_CURVE ( 'NONE', #55679, #96624, #11359, .T. ) ;
#63901 = DIRECTION ( 'NONE',  ( -1.734723475976807094E-16, -0.000000000000000000, -1.000000000000000000 ) ) ;
#63902 = CARTESIAN_POINT ( 'NONE',  ( -32.22503847990285664, 485.9064490506194716, 4.829857536089268599 ) ) ;
#63903 = CARTESIAN_POINT ( 'NONE',  ( 90.08848753752288019, -30.00000000000005684, -9.081672415796756326 ) ) ;
#63904 = AXIS2_PLACEMENT_3D ( 'NONE', #30541, #24051, #80116 ) ;
#63905 = CARTESIAN_POINT ( 'NONE',  ( -78.93788605875903386, -39.49883670821371595, 139.5007675430211123 ) ) ;
#63906 = ORIENTED_EDGE ( 'NONE', *, *, #84476, .F. ) ;
#63907 = CARTESIAN_POINT ( 'NONE',  ( 40.90273407096766078, -60.00000000000019185, 57.82174102673914007 ) ) ;
#63908 = CARTESIAN_POINT ( 'NONE',  ( 14.29190075645216496, 21.26710225494213802, 5.626279437277409201 ) ) ;
#63909 = CARTESIAN_POINT ( 'NONE',  ( 76.72290838289761439, -57.52930957181557403, 194.6109501198345413 ) ) ;
#63910 = CARTESIAN_POINT ( 'NONE',  ( 1.224646799147353848E-15, 274.9999999999999432, 10.00000000000000533 ) ) ;
#63911 = CARTESIAN_POINT ( 'NONE',  ( 35.63739937222026555, 303.4054289079292630, -0.03810013948418256025 ) ) ;
#63912 = CARTESIAN_POINT ( 'NONE',  ( -30.00000000000000355, 461.9594878872932213, 14.33673855776301131 ) ) ;
#63913 = ORIENTED_EDGE ( 'NONE', *, *, #79768, .F. ) ;
#63914 = CARTESIAN_POINT ( 'NONE',  ( -22.88430703375227893, 26.05182353366611281, 30.73977527160241507 ) ) ;
#63915 = DIRECTION ( 'NONE',  ( -1.000000000000000000, -0.000000000000000000, -0.000000000000000000 ) ) ;
#63917 = CARTESIAN_POINT ( 'NONE',  ( -106.3498447864860736, -60.15519976726687901, 165.8917114895338329 ) ) ;
#63916 = CARTESIAN_POINT ( 'NONE',  ( -10.00000000000000355, 30.00000000000000000, 0.000000000000000000 ) ) ;
#63918 = CARTESIAN_POINT ( 'NONE',  ( -5.082755093536326818, -18.21875000204838457, 5.082755093536325042 ) ) ;
#63919 = CARTESIAN_POINT ( 'NONE',  ( 43.03265099500018920, 484.2747968070553952, -0.8099405866666991027 ) ) ;
#63920 = CARTESIAN_POINT ( 'NONE',  ( 9.165151389911681434, 85.00000000000001421, -4.000000000000000000 ) ) ;
#63921 = CARTESIAN_POINT ( 'NONE',  ( 1.218458762081870761, 34.73422897157483646, 28.17869402526995160 ) ) ;
#63922 = CARTESIAN_POINT ( 'NONE',  ( 26.48484422076975164, 37.08860641375430589, 7.709683435484037339 ) ) ;
#63923 = SURFACE_STYLE_USAGE ( .BOTH. , #104905 ) ;
#63924 = EDGE_CURVE ( 'NONE', #25775, #75872, #76817, .T. ) ;
#63925 = AXIS2_PLACEMENT_3D ( 'NONE', #33967, #16148, #106203 ) ;
#63926 = ORIENTED_EDGE ( 'NONE', *, *, #2696, .F. ) ;
#63927 = CARTESIAN_POINT ( 'NONE',  ( 0.000000000000000000, 1.502314598737160412E-15, 6.500000000000000888 ) ) ;
#63929 = CARTESIAN_POINT ( 'NONE',  ( 27.52884087114259160, -60.34135499268811031, 35.96017823446348416 ) ) ;
#63928 = DIRECTION ( 'NONE',  ( 0.9807128367236916944, 0.000000000000000000, 0.1954541682476217956 ) ) ;
#63930 = CARTESIAN_POINT ( 'NONE',  ( 24.00241574749180273, 27.29294457708169830, -32.94367910540196931 ) ) ;
#63932 = ORIENTED_EDGE ( 'NONE', *, *, #96025, .F. ) ;
#63931 = SHAPE_REPRESENTATION ( '10. Furnel', ( #10728 ), #79579 ) ;
#63933 = EDGE_CURVE ( 'NONE', #56640, #85522, #25186, .T. ) ;
#63934 = VERTEX_POINT ( 'NONE', #46704 ) ;
#63935 = CARTESIAN_POINT ( 'NONE',  ( -1.013018381689523073, 43.34736372649656033, -18.25026088174005423 ) ) ;
#63936 = B_SPLINE_CURVE_WITH_KNOTS ( 'NONE', 3,
 ( #71416, #13180, #7215, #104865, #46107, #88680, #72486, #23442, #104319, #56278, #30468, #89214, #96261, #6151, #32055, #82705, #1221, #8276, #83232, #64933, #49260, #33640, #8809, #49799, #67064, #99944, #106435, #82162, #41716, #74068, #66523, #26117, #65466, #25577 ),
 .UNSPECIFIED., .F., .F.,
 ( 4, 2, 2, 2, 2, 2, 2, 2, 2, 2, 2, 2, 2, 2, 2, 2, 4 ),
 ( 1.734723475976807094E-18, 0.0007951492273476404825, 0.001590298454695279230, 0.002385447682042917978, 0.003180596909390556726, 0.003975746136738195907, 0.004770895364085834221, 0.005566044591433471668, 0.006361193818781109982, 0.007156343046128748296, 0.007951492273476388345, 0.008746641500824024057, 0.009541790728171661504, 0.01033693995551930069, 0.01113208918286693640, 0.01192723841021457558, 0.01272238763756221303 ),
 .UNSPECIFIED. ) ;
#63937 = CARTESIAN_POINT ( 'NONE',  ( 19.50000000000000000, 12.99999999999999289, 0.000000000000000000 ) ) ;
#63938 = CARTESIAN_POINT ( 'NONE',  ( 37.33349330513379982, 1.593028355512270567E-15, 0.000000000000000000 ) ) ;
#63939 = DIRECTION ( 'NONE',  ( -0.5735764363510494901, -0.8191520442889894671, 0.000000000000000000 ) ) ;
#63940 = EDGE_CURVE ( 'NONE', #90543, #38839, #104269, .T. ) ;
#63941 = CARTESIAN_POINT ( 'NONE',  ( -7.500000000000000888, 0.000000000000000000, 1.734723475976807094E-15 ) ) ;
#63942 = EDGE_LOOP ( 'NONE', ( #104325, #8168, #70189, #27103, #80063 ) ) ;
#63943 = CARTESIAN_POINT ( 'NONE',  ( 47.48558071520947976, -60.00000000000001421, -38.38385089910498493 ) ) ;
#63944 = CARTESIAN_POINT ( 'NONE',  ( 81.45724438388656097, -29.99999999999998224, 142.5290932105678792 ) ) ;
#63946 = CARTESIAN_POINT ( 'NONE',  ( 0.000000000000000000, 43.22324503868515677, -36.14046114390016839 ) ) ;
#63945 = CIRCLE ( 'NONE', #94893, 7.500000000000006217 ) ;
#63947 = CARTESIAN_POINT ( 'NONE',  ( -7.360624614850912906, -5.000000000000000000, -75.38987561218263522 ) ) ;
#63948 = AXIS2_PLACEMENT_3D ( 'NONE', #29362, #104260, #79980 ) ;
#63949 = CARTESIAN_POINT ( 'NONE',  ( 47.90408546931266898, 11.89605000366072396, -14.35535821593550487 ) ) ;
#63950 = EDGE_LOOP ( 'NONE', ( #2486, #78341, #8551, #7667, #8992, #64873, #64989, #92896 ) ) ;
#63951 = VECTOR ( 'NONE', #49520, 999.9999999999998863 ) ;
#63952 = ORIENTED_EDGE ( 'NONE', *, *, #55041, .F. ) ;
#63953 = VERTEX_POINT ( 'NONE', #44749 ) ;
#63954 =( NAMED_UNIT ( * ) PLANE_ANGLE_UNIT ( ) SI_UNIT ( $, .RADIAN. ) );
#63955 = FACE_OUTER_BOUND ( 'NONE', #9051, .T. ) ;
#63956 = CARTESIAN_POINT ( 'NONE',  ( -39.99722689368601891, 437.4316783397098334, 22.45542938418691037 ) ) ;
#63957 = CARTESIAN_POINT ( 'NONE',  ( 33.07261358295323816, 370.8611101514977122, 23.85133237395751493 ) ) ;
#63958 = CARTESIAN_POINT ( 'NONE',  ( -36.35895093008763013, 334.2607040896156718, -2.357503963907021216 ) ) ;
#63959 = CARTESIAN_POINT ( 'NONE',  ( 32.88333705524082973, 439.7317646416722141, 24.13381181826093069 ) ) ;
#63960 = CARTESIAN_POINT ( 'NONE',  ( -45.99999999999426592, 485.9565049917123929, 0.8651369461898777979 ) ) ;
#63961 = DIRECTION ( 'NONE',  ( -0.000000000000000000, 1.000000000000000000, -0.000000000000000000 ) ) ;
#63962 = ORIENTED_EDGE ( 'NONE', *, *, #27185, .T. ) ;
#63963 = DIRECTION ( 'NONE',  ( 0.000000000000000000, 0.000000000000000000, 1.000000000000000000 ) ) ;
#63964 = VECTOR ( 'NONE', #18769, 1000.000000000000114 ) ;
#63965 = ORIENTED_EDGE ( 'NONE', *, *, #97368, .T. ) ;
#63966 = DIRECTION ( 'NONE',  ( 0.000000000000000000, -1.000000000000000000, 0.000000000000000000 ) ) ;
#63967 = CARTESIAN_POINT ( 'NONE',  ( 16.96954359408614366, 304.5683848806726814, 9.876757081930351845 ) ) ;
#63968 = CARTESIAN_POINT ( 'NONE',  ( -39.28947510688171008, 485.2043936288998225, -4.359233426732905592 ) ) ;
#63969 = CARTESIAN_POINT ( 'NONE',  ( 26.08349330513380693, 1.593028355512270962E-15, 0.000000000000000000 ) ) ;
#63970 = CARTESIAN_POINT ( 'NONE',  ( 62.36095931845834173, -49.91109934801575321, 83.85664639578627089 ) ) ;
#63971 = B_SPLINE_CURVE_WITH_KNOTS ( 'NONE', 3,
 ( #90749, #97758, #6633, #14713, #23925, #47087, #106376, #65409, #24457, #80514, #57293, #82105 ),
 .UNSPECIFIED., .F., .F.,
 ( 4, 2, 2, 2, 2, 4 ),
 ( 0.000000000000000000, 0.0008138854558913180548, 0.001220828183836985756, 0.001627770911782653457, 0.002441656367673991027, 0.003255541823565328598 ),
 .UNSPECIFIED. ) ;
#63972 = EDGE_LOOP ( 'NONE', ( #21062, #4132, #1512, #95940, #36394 ) ) ;
#63973 = CARTESIAN_POINT ( 'NONE',  ( 42.99999999999995737, 464.8825480873695710, 15.07585856869434515 ) ) ;
#63974 = CARTESIAN_POINT ( 'NONE',  ( 2.977408999572652260, -28.43750000204839523, 7.188101187500000044 ) ) ;
#63975 = LINE ( 'NONE', #7293, #68764 ) ;
#63976 = EDGE_CURVE ( 'NONE', #92028, #44354, #100911, .T. ) ;
#63977 = ORIENTED_EDGE ( 'NONE', *, *, #233, .F. ) ;
#63978 = AXIS2_PLACEMENT_3D ( 'NONE', #106033, #91479, #97960 ) ;
#63979 =( LENGTH_UNIT ( ) NAMED_UNIT ( * ) SI_UNIT ( .MILLI., .METRE. ) );
#63980 = B_SPLINE_CURVE_WITH_KNOTS ( 'NONE', 3,
 ( #105004, #88815, #74210, #97416 ),
 .UNSPECIFIED., .F., .F.,
 ( 4, 4 ),
 ( 0.000000000000000000, 0.0002123325198302290187 ),
 .UNSPECIFIED. ) ;
#63981 = AXIS2_PLACEMENT_3D ( 'NONE', #3820, #36757, #53434 ) ;
#63982 = EDGE_CURVE ( 'NONE', #5935, #8490, #90134, .T. ) ;
#63983 = DIRECTION ( 'NONE',  ( 1.000000000000000000, 1.224606353822377258E-16, 0.000000000000000000 ) ) ;
#63984 = EDGE_CURVE ( 'NONE', #13534, #9794, #94075, .T. ) ;
#63985 = AXIS2_PLACEMENT_3D ( 'NONE', #98427, #16996, #49331 ) ;
#63986 = B_SPLINE_CURVE_WITH_KNOTS ( 'NONE', 3,
 ( #67434, #35623, #101389, #19453, #27540, #10237 ),
 .UNSPECIFIED., .F., .F.,
 ( 4, 2, 4 ),
 ( 0.4253311034033953608, 0.4347571302760012690, 0.4441831571486072328 ),
 .UNSPECIFIED. ) ;
#63987 = CARTESIAN_POINT ( 'NONE',  ( -8.000000000000000000, -27.03125000409677270, -3.313708498984762496 ) ) ;
#63988 = CARTESIAN_POINT ( 'NONE',  ( 4.175893272574590753, -3.000000000000000000, -7.137815226410167746 ) ) ;
#63989 = CARTESIAN_POINT ( 'NONE',  ( 86.89651759348157611, -28.03138314466304948, 186.5263926684410194 ) ) ;
#63990 = ADVANCED_FACE ( 'NONE', ( #71126 ), #57860, .T. ) ;
#63991 = EDGE_CURVE ( 'NONE', #59552, #22614, #86806, .T. ) ;
#63992 = CYLINDRICAL_SURFACE ( 'NONE', #32724, 5.000000000000000888 ) ;
#63993 = UNCERTAINTY_MEASURE_WITH_UNIT (LENGTH_MEASURE( 1.000000000000000082E-05 ), #22994, 'distance_accuracy_value', 'NONE');
#63994 = CARTESIAN_POINT ( 'NONE',  ( -8.988144951836199326, 15.40598489176668551, -6.352460523676195047E-13 ) ) ;
#63995 = DIRECTION ( 'NONE',  ( 0.000000000000000000, -1.000000000000000000, 0.000000000000000000 ) ) ;
#63996 = EDGE_CURVE ( 'NONE', #29217, #63888, #16777, .T. ) ;
#63997 = CARTESIAN_POINT ( 'NONE',  ( 16.55741780412212449, 303.5680256153840446, 9.876668742581960814 ) ) ;
#63998 = EDGE_LOOP ( 'NONE', ( #72850, #48248, #24284, #12944, #48879, #4230 ) ) ;
#63999 = DIRECTION ( 'NONE',  ( -1.000000000000000000, 0.000000000000000000, 0.000000000000000000 ) ) ;
#64000 = EDGE_CURVE ( 'NONE', #42587, #60121, #99208, .T. ) ;
#64001 = DIRECTION ( 'NONE',  ( 0.000000000000000000, -1.000000000000000000, 0.000000000000000000 ) ) ;
#64002 = CARTESIAN_POINT ( 'NONE',  ( 17.20669968485552559, -60.00000000000000000, 39.93835234338625639 ) ) ;
#64003 = CARTESIAN_POINT ( 'NONE',  ( -97.63590237861488674, -29.99999999999999645, 134.9849753005358934 ) ) ;
#64004 = CIRCLE ( 'NONE', #65671, 12.00000000000001066 ) ;
#64005 = DIRECTION ( 'NONE',  ( -1.000000000000000000, -1.224606353822377258E-16, -0.000000000000000000 ) ) ;
#64006 = CARTESIAN_POINT ( 'NONE',  ( 52.15219236777184619, -57.67660669137886487, 83.12330646720228344 ) ) ;
#64008 = SURFACE_SIDE_STYLE ('',( #31121 ) ) ;
#64007 = CARTESIAN_POINT ( 'NONE',  ( 15.90614609307868399, -3.157894736842107530, 14.66382285868950675 ) ) ;
#64009 = CARTESIAN_POINT ( 'NONE',  ( -41.74778363246318236, 460.3875427940050145, 2.379529480112096529 ) ) ;
#64010 = CARTESIAN_POINT ( 'NONE',  ( -32.14284448310063880, 464.7823907227477775, 11.45521013154555234 ) ) ;
#64011 = CARTESIAN_POINT ( 'NONE',  ( -9.168149550320920937, 15.99999999372935022, 3.997425403568219515 ) ) ;
#64012 = CARTESIAN_POINT ( 'NONE',  ( 67.48317336153286305, 6.856755485862130937E-15, 0.000000000000000000 ) ) ;
#64013 = CARTESIAN_POINT ( 'NONE',  ( -24.16062877281563459, -59.99999999999999289, 40.95735949052681235 ) ) ;
#64014 = CARTESIAN_POINT ( 'NONE',  ( 2.386052322619232946, -15.44095796389983022, -35.20331376883997621 ) ) ;
#64015 = CARTESIAN_POINT ( 'NONE',  ( -87.06507237377361719, -50.09467886413911231, 191.9848466096647428 ) ) ;
#64016 = AXIS2_PLACEMENT_3D ( 'NONE', #9715, #59906, #25973 ) ;
#64018 = B_SPLINE_CURVE_WITH_KNOTS ( 'NONE', 3,
 ( #76632, #83138, #26022, #51287, #83652, #10303, #34630, #2741, #93369, #41620, #67499, #59415, #9235, #75576, #19521, #34098, #51823, #25474, #18979, #84738, #10821, #43743, #58330, #35696, #60490, #92277, #84207, #17363, #68571, #35150, #91254, #101456, #43218, #42679 ),
 .UNSPECIFIED., .F., .F.,
 ( 4, 2, 2, 2, 2, 2, 2, 2, 2, 2, 2, 2, 2, 2, 2, 2, 4 ),
 ( 0.000000000000000000, 0.03124999999999995143, 0.06249999999999990286, 0.09374999999999990286, 0.1249999999999999167, 0.1562499999999999167, 0.1874999999999999167, 0.2187499999999999445, 0.2499999999999999445, 0.2812499999999999445, 0.3124999999999999445, 0.3437499999999999445, 0.3749999999999999445, 0.4062500000000000000, 0.4375000000000000000, 0.4687500000000000000, 0.5000000000000000000 ),
 .UNSPECIFIED. ) ;
#64017 = CIRCLE ( 'NONE', #98406, 5.000000000000000888 ) ;
#64019 = ORIENTED_EDGE ( 'NONE', *, *, #34620, .T. ) ;
#64020 =( NAMED_UNIT ( * ) PLANE_ANGLE_UNIT ( ) SI_UNIT ( $, .RADIAN. ) );
#64021 = CARTESIAN_POINT ( 'NONE',  ( -12.48886971890022934, -46.43935809921794799, 31.68723845390683636 ) ) ;
#64023 = CARTESIAN_POINT ( 'NONE',  ( 41.50820411079202898, 461.5963371455317770, 2.703439750996501800 ) ) ;
#64022 = CARTESIAN_POINT ( 'NONE',  ( -90.21012822187128677, -59.99999999999999289, 56.28790610766393598 ) ) ;
#64024 = EDGE_LOOP ( 'NONE', ( #19909, #34267, #74910, #275 ) ) ;
#64025 = CARTESIAN_POINT ( 'NONE',  ( -7.500000000000007105, 39.99999999999998579, -68.91429205786793943 ) ) ;
#64026 = CARTESIAN_POINT ( 'NONE',  ( -4.649486852896246525, -5.000000000000039968, -15.66810684149979771 ) ) ;
#64027 = DIRECTION ( 'NONE',  ( 0.000000000000000000, -1.000000000000000000, 0.000000000000000000 ) ) ;
#64028 = COLOUR_RGB ( '', 0.66274510, 0.83137255, 0.94901961) ;
#64029 = CARTESIAN_POINT ( 'NONE',  ( 5.290067270632161645, -1.200000000000000030E-05, -8.531152949374595451 ) ) ;
#64030 = EDGE_CURVE ( 'NONE', #94321, #15506, #26915, .T. ) ;
#64031 = CARTESIAN_POINT ( 'NONE',  ( 65.82730706677887156, -60.00000000000000711, 121.6744210731262825 ) ) ;
#64032 = CARTESIAN_POINT ( 'NONE',  ( -0.1699152989463506569, 54.30758622938874680, -7.750000000000000888 ) ) ;
#64033 = EDGE_LOOP ( 'NONE', ( #87515, #14908, #84899, #22915, #74015, #51665, #5298, #34542 ) ) ;
#64034 = CARTESIAN_POINT ( 'NONE',  ( 0.000000000000000000, 30.00000000000000000, 74.46152422706630603 ) ) ;
#64035 = CARTESIAN_POINT ( 'NONE',  ( -8.000000000000000000, -20.93750000409676915, -9.797174393178825657E-16 ) ) ;
#64036 = DIRECTION ( 'NONE',  ( 0.000000000000000000, -1.000000000000000000, 0.000000000000000000 ) ) ;
#64037 = DIRECTION ( 'NONE',  ( 0.000000000000000000, -1.000000000000000000, 0.000000000000000000 ) ) ;
#64038 = CARTESIAN_POINT ( 'NONE',  ( -4.680975426248723537, -2.415770170678390727, 103.4780497728483226 ) ) ;
#64039 = ORIENTED_EDGE ( 'NONE', *, *, #81987, .F. ) ;
#64040 = CARTESIAN_POINT ( 'NONE',  ( -30.08887150021950774, 331.1717924776848463, 15.36326397572592661 ) ) ;
#64041 = VERTEX_POINT ( 'NONE', #23668 ) ;
#64042 = DIRECTION ( 'NONE',  ( -1.000000000000000000, -1.224606353822377258E-16, -0.000000000000000000 ) ) ;
#64043 = CARTESIAN_POINT ( 'NONE',  ( -34.16642289233710983, 464.7650419733863600, 19.36631221619108700 ) ) ;
#64044 = FACE_OUTER_BOUND ( 'NONE', #36700, .T. ) ;
#64045 = EDGE_LOOP ( 'NONE', ( #48066, #677, #23091, #8361 ) ) ;
#64046 =( LENGTH_UNIT ( ) NAMED_UNIT ( * ) SI_UNIT ( .MILLI., .METRE. ) );
#64048 = CARTESIAN_POINT ( 'NONE',  ( -113.9570076106580103, -59.99999999998043876, 158.2873460090529534 ) ) ;
#64047 = STYLED_ITEM ( 'NONE', ( #37264 ), #106412 ) ;
#64049 = CARTESIAN_POINT ( 'NONE',  ( 46.00000000000000000, 488.1813821183642972, 2.479370420756042748 ) ) ;
#64050 = CARTESIAN_POINT ( 'NONE',  ( 44.33732900979256897, -59.99999999999998579, 59.29852098770807345 ) ) ;
#64051 = DIRECTION ( 'NONE',  ( -1.000000000000000000, -1.224606353822377258E-16, -0.000000000000000000 ) ) ;
#64052 = DIRECTION ( 'NONE',  ( -1.000000000000000000, -1.224606353822377258E-16, -0.000000000000000000 ) ) ;
#64054 = CARTESIAN_POINT ( 'NONE',  ( 12.66751964286181575, -60.35877864777715018, 34.01265280193257468 ) ) ;
#64053 = CARTESIAN_POINT ( 'NONE',  ( -106.8236106313706699, -14.21045842199435150, 178.1018237235793151 ) ) ;
#64055 = CARTESIAN_POINT ( 'NONE',  ( 99.93939408685974968, -38.00000000000001421, 190.7851520131013388 ) ) ;
#64056 = DIRECTION ( 'NONE',  ( 0.000000000000000000, 1.000000000000000000, 0.000000000000000000 ) ) ;
#64057 = CARTESIAN_POINT ( 'NONE',  ( -44.07123412536562057, -46.43995785254333697, 44.37406601753968260 ) ) ;
#64058 = AXIS2_PLACEMENT_3D ( 'NONE', #30055, #54820, #87748 ) ;
#64059 = CARTESIAN_POINT ( 'NONE',  ( -0.1698782441665641074, 34.17493339656093809, -29.74125536344337917 ) ) ;
#64060 = B_SPLINE_CURVE_WITH_KNOTS ( 'NONE', 3,
 ( #87079, #78429, #88134, #4555, #37492, #87607, #71939, #86563, #22887, #46082, #63339, #96233 ),
 .UNSPECIFIED., .F., .F.,
 ( 4, 2, 2, 2, 2, 4 ),
 ( 0.000000000000000000, 0.001521572489514788412, 0.003043144979029576824, 0.003803931223786971572, 0.004564717468544366753, 0.006086289958059119820 ),
 .UNSPECIFIED. ) ;
#64061 = ORIENTED_EDGE ( 'NONE', *, *, #79789, .T. ) ;
#64062 = CYLINDRICAL_SURFACE ( 'NONE', #30679, 1.250000000000001110 ) ;
#64063 = CARTESIAN_POINT ( 'NONE',  ( -43.63899620156477965, 434.3182181978404515, 14.37213632273176422 ) ) ;
#64064 = CARTESIAN_POINT ( 'NONE',  ( 2.470381878726035567E-14, 18.87382441218300144, 49.24999999999992184 ) ) ;
#64065 = CARTESIAN_POINT ( 'NONE',  ( 2.500000000000002665, -17.75174924879615546, -25.82778434327287798 ) ) ;
#64066 = EDGE_CURVE ( 'NONE', #51009, #18709, #40884, .T. ) ;
#64067 = DIRECTION ( 'NONE',  ( -0.000000000000000000, 1.000000000000000000, -0.000000000000000000 ) ) ;
#64068 = ORIENTED_EDGE ( 'NONE', *, *, #55416, .F. ) ;
#64069 = CARTESIAN_POINT ( 'NONE',  ( -14.03901844863619530, -8.437680008516872832, 12.41437985069090466 ) ) ;
#64070 = ORIENTED_EDGE ( 'NONE', *, *, #101410, .T. ) ;
#64071 = CARTESIAN_POINT ( 'NONE',  ( 103.0665016853196363, -30.00000000000061462, 197.4198734183501358 ) ) ;
#64072 = CARTESIAN_POINT ( 'NONE',  ( 46.00000000000000711, 461.5914298688537656, 9.837083399362915870 ) ) ;
#64073 = CARTESIAN_POINT ( 'NONE',  ( 6.075720087193105634, 41.99394347255277182, -59.86320241472431292 ) ) ;
#64074 = PRESENTATION_STYLE_ASSIGNMENT (( #89918 ) ) ;
#64075 = CARTESIAN_POINT ( 'NONE',  ( 87.07233282619432657, -30.00000000000000000, 70.95073359267735214 ) ) ;
#64076 =( BOUNDED_CURVE ( )  B_SPLINE_CURVE ( 2, ( #31627, #81197, #48300, #47245, #73091, #40222, #87736, #80147, #106541 ),
 .UNSPECIFIED., .F., .F. ) 
 B_SPLINE_CURVE_WITH_KNOTS ( ( 3, 2, 2, 2, 3 ),
 ( 0.9558823529411765163, 0.9632352941176470784, 0.9705882352941176405, 0.9779411764705882026, 0.9804062239465977102 ),
 .UNSPECIFIED. ) 
 CURVE ( )  GEOMETRIC_REPRESENTATION_ITEM ( )  RATIONAL_B_SPLINE_CURVE ( ( 1.000000000000000000, 0.9238795325112867385, 1.000000000000000000, 0.9238795325112867385, 1.000000000000000000, 0.9238795325112867385, 1.000000000000000000, 0.9744808829892229740, 0.9660721530923004341 ) ) 
 REPRESENTATION_ITEM ( '' )  );
#64077 = B_SPLINE_CURVE_WITH_KNOTS ( 'NONE', 3,
 ( #4735, #70535, #101310, #105543 ),
 .UNSPECIFIED., .F., .F.,
 ( 4, 4 ),
 ( 1.034338964446688375E-15, 0.002502641776601218122 ),
 .UNSPECIFIED. ) ;
#64078 = CARTESIAN_POINT ( 'NONE',  ( -28.99999999999998934, 0.000000000000000000, 9.000000000000000000 ) ) ;
#64079 = VERTEX_POINT ( 'NONE', #73228 ) ;
#64080 = VERTEX_POINT ( 'NONE', #98579 ) ;
#64081 = EDGE_LOOP ( 'NONE', ( #411, #23110, #70648, #15353, #97344 ) ) ;
#64082 = CARTESIAN_POINT ( 'NONE',  ( 33.16501691561000342, 438.9509064377053846, 23.91453236866924215 ) ) ;
#64083 = CARTESIAN_POINT ( 'NONE',  ( 43.21801493134148586, 434.4543138599221948, 16.17410598210216222 ) ) ;
#64084 = CARTESIAN_POINT ( 'NONE',  ( 3.269135563215229023, 294.8518027752268722, -10.00000000024436275 ) ) ;
#64085 = ORIENTED_EDGE ( 'NONE', *, *, #20283, .F. ) ;
#64086 = DIRECTION ( 'NONE',  ( 1.000000000000000000, 0.000000000000000000, -0.000000000000000000 ) ) ;
#64087 = VERTEX_POINT ( 'NONE', #97503 ) ;
#64088 = FACE_OUTER_BOUND ( 'NONE', #101287, .T. ) ;
#64089 = CARTESIAN_POINT ( 'NONE',  ( 81.01023851859548586, -38.83486255393263775, 194.6255486919564532 ) ) ;
#64090 = CYLINDRICAL_SURFACE ( 'NONE', #93945, 5.000000000000002665 ) ;
#64091 = PRODUCT_RELATED_PRODUCT_CATEGORY ( 'part', '', ( #79411 ) ) ;
#64092 = CARTESIAN_POINT ( 'NONE',  ( 85.62592449253092752, -52.72843542154268448, -2.857092586073228357 ) ) ;
#64093 = CARTESIAN_POINT ( 'NONE',  ( 85.96116874757127846, -38.00000000000002842, 186.3684374995824271 ) ) ;
#64094 = CARTESIAN_POINT ( 'NONE',  ( 36.83410552012148997, 306.6732998202488147, 4.709818881448565975 ) ) ;
#64095 =( NAMED_UNIT ( * ) PLANE_ANGLE_UNIT ( ) SI_UNIT ( $, .RADIAN. ) );
#64096 = DIRECTION ( 'NONE',  ( -1.000000000000000000, 0.000000000000000000, 0.000000000000000000 ) ) ;
#64097 = CIRCLE ( 'NONE', #38237, 5.000000000000001776 ) ;
#64098 = CARTESIAN_POINT ( 'NONE',  ( -39.26668904306311703, 460.2385666352529938, 2.228751329586619701 ) ) ;
#64099 = DIRECTION ( 'NONE',  ( -1.000000000000000000, -1.224606353822377258E-16, -0.000000000000000000 ) ) ;
#64100 = ORIENTED_EDGE ( 'NONE', *, *, #342, .F. ) ;
#64101 = CARTESIAN_POINT ( 'NONE',  ( 32.67323224503917345, 485.6332095909920099, 6.597358449831840055 ) ) ;
#64102 = CARTESIAN_POINT ( 'NONE',  ( -36.10337418012809962, 461.0502312562470593, 3.050677930906189772 ) ) ;
#64103 = CARTESIAN_POINT ( 'NONE',  ( -4.201585111823095353, 12.27236537274642991, 5.000000000000000888 ) ) ;
#64104 = EDGE_LOOP ( 'NONE', ( #52385, #85153, #28530, #100765 ) ) ;
#64105 = CARTESIAN_POINT ( 'NONE',  ( 0.000000000000000000, 0.000000000000000000, 0.000000000000000000 ) ) ;
#64106 = CARTESIAN_POINT ( 'NONE',  ( -34.53449118956828556, 302.4528159859040670, 3.673939189084939105 ) ) ;
#64107 = CARTESIAN_POINT ( 'NONE',  ( 7.382723172920433008, 54.19823143065442395, -3.210640374493870297 ) ) ;
#64108 = ADVANCED_FACE ( 'NONE', ( #55976 ), #39837, .F. ) ;
#64109 = FACE_OUTER_BOUND ( 'NONE', #67648, .T. ) ;
#64110 = CARTESIAN_POINT ( 'NONE',  ( 8.000000000000000000, -13.90624999999999112, -3.313708498984761608 ) ) ;
#64111 = CARTESIAN_POINT ( 'NONE',  ( 0.9118253755784003767, -18.00287762888658349, 35.00125712497896302 ) ) ;
#64112 = STYLED_ITEM ( 'NONE', ( #64958 ), #19858 ) ;
#64113 = EDGE_CURVE ( 'NONE', #13857, #23677, #21721, .T. ) ;
#64114 = PRESENTATION_LAYER_ASSIGNMENT (  '', '', ( #65844 ) ) ;
#64115 = PRODUCT_DEFINITION_SHAPE ( 'NONE', 'NONE',  #106800 ) ;
#64116 = CYLINDRICAL_SURFACE ( 'NONE', #26103, 1.250000000000001110 ) ;
#64117 = ORIENTED_EDGE ( 'NONE', *, *, #97959, .F. ) ;
#64118 = CARTESIAN_POINT ( 'NONE',  ( 86.09880483962514575, -24.81058578010869908, 180.0994920548855021 ) ) ;
#64119 = FACE_OUTER_BOUND ( 'NONE', #2581, .T. ) ;
#64120 = ORIENTED_EDGE ( 'NONE', *, *, #59744, .F. ) ;
#64121 = CARTESIAN_POINT ( 'NONE',  ( 94.19131188920297859, -57.67257310899840661, 22.54837274470326847 ) ) ;
#64122 = CARTESIAN_POINT ( 'NONE',  ( 42.57704743493908950, 486.1612337113410263, 7.852296464539637810 ) ) ;
#64123 = CARTESIAN_POINT ( 'NONE',  ( -15.05785784214257461, 3.824195276785042896, 4.604276673521232155 ) ) ;
#64124 = EDGE_CURVE ( 'NONE', #35260, #92331, #66496, .T. ) ;
#64125 = DIRECTION ( 'NONE',  ( -1.000000000000000000, -1.224606353822377258E-16, -0.000000000000000000 ) ) ;
#64126 = EDGE_CURVE ( 'NONE', #49838, #27681, #30364, .T. ) ;
#64127 = ADVANCED_BREP_SHAPE_REPRESENTATION ( '', ( #16793, #10728 ), #93743 ) ;
#64128 = TOROIDAL_SURFACE ( 'NONE', #86546, 12.00000000000001066, 3.000000000000000000 ) ;
#64129 = EDGE_CURVE ( 'NONE', #55862, #44189, #92619, .T. ) ;
#64130 = AXIS2_PLACEMENT_3D ( 'NONE', #42822, #1811, #24021 ) ;
#64131 = CARTESIAN_POINT ( 'NONE',  ( 29.68315524077033629, 13.47185074185905584, 42.10535821593451544 ) ) ;
#64132 = CARTESIAN_POINT ( 'NONE',  ( -1.211595439868049962, 7.960739084487649109, -0.4504974108211952655 ) ) ;
#64134 = CARTESIAN_POINT ( 'NONE',  ( -11.81728811066984086, 6.698763365558540350, 9.056117883122757561 ) ) ;
#64133 = FACE_OUTER_BOUND ( 'NONE', #58568, .T. ) ;
#64135 = VECTOR ( 'NONE', #67460, 1000.000000000000000 ) ;
#64136 = PLANE ( 'NONE',  #98714 ) ;
#64137 = CARTESIAN_POINT ( 'NONE',  ( 40.88293604215247967, 432.5779639752643675, 26.56799667982232549 ) ) ;
#64138 = CARTESIAN_POINT ( 'NONE',  ( -28.19205650684127562, 36.30852143868257542, -9.429946862361873627 ) ) ;
#64139 = DIRECTION ( 'NONE',  ( -0.000000000000000000, -1.000000000000000000, -0.000000000000000000 ) ) ;
#64140 =( NAMED_UNIT ( * ) PLANE_ANGLE_UNIT ( ) SI_UNIT ( $, .RADIAN. ) );
#64141 = STYLED_ITEM ( 'NONE', ( #31592 ), #10316 ) ;
#64142 = CARTESIAN_POINT ( 'NONE',  ( 43.49286403356602193, 484.8086342565614473, 4.190194857772357118 ) ) ;
#64143 = ORIENTED_EDGE ( 'NONE', *, *, #53704, .T. ) ;
#64144 = SURFACE_SIDE_STYLE ('',( #80283 ) ) ;
#64145 = CARTESIAN_POINT ( 'NONE',  ( 5.650483388624516046, -61.54433403149616311, 2.031129859422141859 ) ) ;
#64146 = CARTESIAN_POINT ( 'NONE',  ( -40.94509419489318702, -34.58952987473475105, -29.39275092839041292 ) ) ;
#64147 = ORIENTED_EDGE ( 'NONE', *, *, #46579, .F. ) ;
#64148 = EDGE_LOOP ( 'NONE', ( #65124, #70425, #91940, #1655, #84563 ) ) ;
#64149 = EDGE_CURVE ( 'NONE', #1802, #14939, #78579, .T. ) ;
#64150 = CARTESIAN_POINT ( 'NONE',  ( -44.12589798587348611, 464.4133173135365382, 9.756011010160211328 ) ) ;
#64151 = CARTESIAN_POINT ( 'NONE',  ( -91.96355247515836595, -59.99999999999998579, -14.08785575593242889 ) ) ;
#64152 = ORIENTED_EDGE ( 'NONE', *, *, #61853, .T. ) ;
#64153 = CARTESIAN_POINT ( 'NONE',  ( -3.294249609603382645, 39.99999999999999289, -70.27378291343094929 ) ) ;
#64154 = CARTESIAN_POINT ( 'NONE',  ( -7.306728573036795460, 54.30193072519075059, -2.634352804278476512 ) ) ;
#64155 = CARTESIAN_POINT ( 'NONE',  ( 99.71449018044667412, -52.77652230665619726, 194.3813892764564173 ) ) ;
#64157 = DIRECTION ( 'NONE',  ( 0.000000000000000000, 1.000000000000000000, -3.466879843239602429E-16 ) ) ;
#64156 = FILL_AREA_STYLE_COLOUR ( '', #78444 ) ;
#64158 = CARTESIAN_POINT ( 'NONE',  ( -83.26220561033844092, -32.54356584210299985, 161.2381412266789198 ) ) ;
#64159 = EDGE_LOOP ( 'NONE', ( #75123, #43968, #93781, #61819 ) ) ;
#64160 = CIRCLE ( 'NONE', #76222, 5.000000000000001776 ) ;
#64161 = VERTEX_POINT ( 'NONE', #92087 ) ;
#64162 = VERTEX_POINT ( 'NONE', #18227 ) ;
#64163 = DIRECTION ( 'NONE',  ( -0.5735764363510512664, 0.8191520442889881348, 1.003171929053520309E-16 ) ) ;
#64164 = ADVANCED_FACE ( 'NONE', ( #51081 ), #101260, .F. ) ;
#64165 = CARTESIAN_POINT ( 'NONE',  ( -4.999999999999999112, -13.81090860391436514, 13.12305563960475752 ) ) ;
#64166 =( NAMED_UNIT ( * ) PLANE_ANGLE_UNIT ( ) SI_UNIT ( $, .RADIAN. ) );
#64167 = ORIENTED_EDGE ( 'NONE', *, *, #87186, .F. ) ;
#64168 = FACE_OUTER_BOUND ( 'NONE', #9382, .T. ) ;
#64169 = FACE_OUTER_BOUND ( 'NONE', #79810, .T. ) ;
#64170 = DIRECTION ( 'NONE',  ( 0.000000000000000000, 0.000000000000000000, 1.000000000000000000 ) ) ;
#64171 = CARTESIAN_POINT ( 'NONE',  ( -108.6808209725780330, -57.66364365951052662, 198.1525503354515081 ) ) ;
#64172 = CARTESIAN_POINT ( 'NONE',  ( 7.188101187500000044, -34.15625000204838813, 0.000000000000000000 ) ) ;
#64173 = CARTESIAN_POINT ( 'NONE',  ( 2.832728918602883450, 6.234773369952728572, -6.171481112545254000 ) ) ;
#64174 = CARTESIAN_POINT ( 'NONE',  ( -23.95564068939877345, 305.6666757346319514, -9.824255363917307804 ) ) ;
#64175 = CARTESIAN_POINT ( 'NONE',  ( 0.9542819463626004417, 27.45207584973554304, -40.31149540464158321 ) ) ;
#64176 = AXIS2_PLACEMENT_3D ( 'NONE', #23075, #38720, #73169 ) ;
#64177 = CARTESIAN_POINT ( 'NONE',  ( -69.60683966046387638, -29.99999999999998224, -29.88974110699236775 ) ) ;
#64178 = CARTESIAN_POINT ( 'NONE',  ( -31.71194513525783165, -14.21045842199430709, 37.70210531190891601 ) ) ;
#64179 = CARTESIAN_POINT ( 'NONE',  ( -52.85655506056811959, -25.64035322949781914, 50.79863798127239249 ) ) ;
#64180 = ORIENTED_EDGE ( 'NONE', *, *, #78245, .F. ) ;
#64181 = CARTESIAN_POINT ( 'NONE',  ( -33.97359119245066239, 434.1099241184709285, 11.80501937577158778 ) ) ;
#64182 = VERTEX_POINT ( 'NONE', #75907 ) ;
#64183 = CARTESIAN_POINT ( 'NONE',  ( -98.26664012846288188, -37.73380340095903307, 192.3703194023427159 ) ) ;
#64184 = CARTESIAN_POINT ( 'NONE',  ( -0.3382046435677298901, 52.16426612011243691, 7.785187884561949545 ) ) ;
#64185 = ADVANCED_FACE ( 'NONE', ( #52158 ), #80341, .T. ) ;
#64186 = EDGE_LOOP ( 'NONE', ( #77123, #16600, #31716, #10257 ) ) ;
#64187 = CARTESIAN_POINT ( 'NONE',  ( 19.09341000947918943, 49.66424469652579887, 61.75080758588853058 ) ) ;
#64188 = CARTESIAN_POINT ( 'NONE',  ( 109.4076176909565845, -38.35605075573632661, 188.6800926733125152 ) ) ;
#64189 = CARTESIAN_POINT ( 'NONE',  ( -9.113097280746996987, -54.00000000000000711, 31.11721482942554928 ) ) ;
#64190 = CARTESIAN_POINT ( 'NONE',  ( -1.320432766682874540E-15, -10.90625000204838457, 7.188101187500000044 ) ) ;
#64191 = CARTESIAN_POINT ( 'NONE',  ( -7.447697371462428606, 302.7211807851450658, 9.909313283245410275 ) ) ;
#64192 = CARTESIAN_POINT ( 'NONE',  ( -42.18756898894582008, 484.4522853017719513, -2.425645685620466452 ) ) ;
#64193 = CARTESIAN_POINT ( 'NONE',  ( 82.85293946109428020, -30.00000000000000711, 151.7967064736782845 ) ) ;
#64194 = CONICAL_SURFACE ( 'NONE', #81395, 3.309500000000001663, 0.9599310885968770357 ) ;
#64195 = EDGE_CURVE ( 'NONE', #8878, #96901, #47388, .T. ) ;
#64196 = CARTESIAN_POINT ( 'NONE',  ( -9.090909090909093493, 16.00000000000000000, -4.165977904505304252 ) ) ;
#64197 = CARTESIAN_POINT ( 'NONE',  ( 5.123541259261425118, 51.37833675238564268, -8.531152949374599004 ) ) ;
#64198 = CARTESIAN_POINT ( 'NONE',  ( -0.4143444918978542724, 35.05607634723067889, 27.31767140698388729 ) ) ;
#64199 = MECHANICAL_DESIGN_GEOMETRIC_PRESENTATION_REPRESENTATION (  '', ( #74473 ), #12498 ) ;
#64200 = EDGE_LOOP ( 'NONE', ( #23930, #6873 ) ) ;
#64201 = ORIENTED_EDGE ( 'NONE', *, *, #86543, .T. ) ;
#64202 = CARTESIAN_POINT ( 'NONE',  ( 49.26203278476850755, -42.97728400714042607, 50.67361426740096420 ) ) ;
#64203 = CIRCLE ( 'NONE', #48686, 4.000000000000001776 ) ;
#64204 = DIRECTION ( 'NONE',  ( 0.000000000000000000, -1.000000000000000000, 0.000000000000000000 ) ) ;
#64205 = CARTESIAN_POINT ( 'NONE',  ( 22.33349330513380693, 4.898587196589411843E-16, -4.000000000000001776 ) ) ;
#64206 = CARTESIAN_POINT ( 'NONE',  ( -110.4362257262843059, -38.35609804039832227, 182.9338296351233168 ) ) ;
#64207 = ORIENTED_EDGE ( 'NONE', *, *, #88787, .T. ) ;
#64208 = CARTESIAN_POINT ( 'NONE',  ( 84.80912723296837896, -38.35879924987171563, -23.01720600995700750 ) ) ;
#64209 = CARTESIAN_POINT ( 'NONE',  ( 11.43665049262130928, 13.07896887865097213, -10.01657062917009000 ) ) ;
#64210 = DIRECTION ( 'NONE',  ( -1.000000000000000000, -1.224606353822377258E-16, -0.000000000000000000 ) ) ;
#64211 = CARTESIAN_POINT ( 'NONE',  ( 32.25199865210457517, 464.6771562214399296, 10.60479922512074147 ) ) ;
#64212 = CARTESIAN_POINT ( 'NONE',  ( 104.1878238513955353, -52.71701965651387667, 153.9813814288278593 ) ) ;
#64213 = CARTESIAN_POINT ( 'NONE',  ( 0.000000000000000000, 0.000000000000000000, 1.734723475976807094E-15 ) ) ;
#64214 = SURFACE_SIDE_STYLE ('',( #89539 ) ) ;
#64215 = CARTESIAN_POINT ( 'NONE',  ( -35.35381222550667957, 364.7255732624930147, 3.995359698804311854 ) ) ;
#64216 = SURFACE_SIDE_STYLE ('',( #9526 ) ) ;
#64217 = CARTESIAN_POINT ( 'NONE',  ( -32.25691083757232747, 485.8985639246204187, 4.832559767440749887 ) ) ;
#64218 = CARTESIAN_POINT ( 'NONE',  ( 96.44948892551855124, -60.00000000000000711, 202.5258697066679758 ) ) ;
#64219 = EDGE_CURVE ( 'NONE', #4198, #59152, #88758, .T. ) ;
#64220 = CARTESIAN_POINT ( 'NONE',  ( 28.09999999999999787, 1.533819458162526451E-15, 0.000000000000000000 ) ) ;
#64221 = ORIENTED_EDGE ( 'NONE', *, *, #98743, .T. ) ;
#64222 = CARTESIAN_POINT ( 'NONE',  ( 57.23890203722747572, -42.96409028050587864, 66.85176157112299222 ) ) ;
#64223 = CARTESIAN_POINT ( 'NONE',  ( -33.06064406479386975, 299.5759903008183755, -8.949493189068455479 ) ) ;
#64224 = CARTESIAN_POINT ( 'NONE',  ( 9.442395496852061143, -51.55837707188687347, 30.29618450995123169 ) ) ;
#64225 = DIRECTION ( 'NONE',  ( -1.000000000000000000, -1.224606353822377258E-16, -0.000000000000000000 ) ) ;
#64226 = ORIENTED_EDGE ( 'NONE', *, *, #42472, .T. ) ;
#64228 = CARTESIAN_POINT ( 'NONE',  ( -9.821751540093583088, -50.53182543592436815, 25.10730599066359758 ) ) ;
#64227 = CARTESIAN_POINT ( 'NONE',  ( -107.6099443991786444, -38.36026800758562416, 193.7261362466381343 ) ) ;
#64229 = CARTESIAN_POINT ( 'NONE',  ( 6.397334739185440711, -2.999999999999999556, -4.916373759799318677 ) ) ;
#64230 = DIRECTION ( 'NONE',  ( 0.5735764363510442720, -0.8191520442889930198, 1.003171929053526349E-16 ) ) ;
#64231 = FACE_OUTER_BOUND ( 'NONE', #42088, .T. ) ;
#64232 = CARTESIAN_POINT ( 'NONE',  ( 8.000000000000000000, -33.40625000000000000, -3.313708498984761608 ) ) ;
#64233 = CARTESIAN_POINT ( 'NONE',  ( 9.739726766102963396, -5.000000000000000888, -82.38252115499879835 ) ) ;
#64234 = CONICAL_SURFACE ( 'NONE', #83161, 5.000000000000010658, 0.9599310885968697082 ) ;
#64235 = EDGE_LOOP ( 'NONE', ( #48844, #81482, #95165, #26070, #99223 ) ) ;
#64236 = CARTESIAN_POINT ( 'NONE',  ( 84.32059328291249756, -32.45894075901123443, 171.3683495658556524 ) ) ;
#64237 = DIRECTION ( 'NONE',  ( 0.000000000000000000, 0.000000000000000000, 1.000000000000000000 ) ) ;
#64238 = EDGE_LOOP ( 'NONE', ( #24061, #29565 ) ) ;
#64239 = CIRCLE ( 'NONE', #81442, 5.000000000000010658 ) ;
#64240 = DIRECTION ( 'NONE',  ( 0.000000000000000000, 1.000000000000000000, 0.000000000000000000 ) ) ;
#64241 = CARTESIAN_POINT ( 'NONE',  ( 5.538604458977774314, -5.000000000025686120, -16.33373421804029135 ) ) ;
#64242 = CARTESIAN_POINT ( 'NONE',  ( 41.49038059205248885, 469.1084758719956085, 1.096707336962226442 ) ) ;
#64243 = CARTESIAN_POINT ( 'NONE',  ( -3.122594241941514692, 50.00000000000000711, -73.30485703408217546 ) ) ;
#64244 = FACE_OUTER_BOUND ( 'NONE', #88564, .T. ) ;
#64245 = EDGE_CURVE ( 'NONE', #75882, #46481, #39897, .T. ) ;
#64246 = CARTESIAN_POINT ( 'NONE',  ( -29.49969761086808617, 8.554442461696824651, -42.10535821593507677 ) ) ;
#64247 = EDGE_CURVE ( 'NONE', #104530, #104064, #35588, .T. ) ;
#64248 = ORIENTED_EDGE ( 'NONE', *, *, #103526, .F. ) ;
#64249 = SHAPE_REPRESENTATION_RELATIONSHIP ( 'NONE' , 'NONE' ,  #66748, #78240 ) ;
#64250 = AXIS2_PLACEMENT_3D ( 'NONE', #64341, #103720, #30931 ) ;
#64251 = EDGE_CURVE ( 'NONE', #63843, #40108, #73297, .T. ) ;
#64252 = EDGE_CURVE ( 'NONE', #41862, #5701, #49314, .T. ) ;
#64253 = CARTESIAN_POINT ( 'NONE',  ( 6.928203230275509661, 105.2647926725356911, 4.000000000000000888 ) ) ;
#64254 = CARTESIAN_POINT ( 'NONE',  ( -5.580966921651770022E-13, 25.16821295365027211, 40.75000000000505906 ) ) ;
#64256 = CARTESIAN_POINT ( 'NONE',  ( -10.35656535444040216, 10.94469993726888468, -10.44094449561934290 ) ) ;
#64255 = CARTESIAN_POINT ( 'NONE',  ( -4.625902140663016304, -18.51163087806139629, 35.07735223482339393 ) ) ;
#64257 = CARTESIAN_POINT ( 'NONE',  ( 7.188101187500000044, -19.15625000204838457, 0.000000000000000000 ) ) ;
#64258 = CARTESIAN_POINT ( 'NONE',  ( -5.957442974920758694, 40.83906611472500714, 65.00000000000298428 ) ) ;
#64259 =( NAMED_UNIT ( * ) PLANE_ANGLE_UNIT ( ) SI_UNIT ( $, .RADIAN. ) );
#64260 = ORIENTED_EDGE ( 'NONE', *, *, #34332, .T. ) ;
#64261 = CARTESIAN_POINT ( 'NONE',  ( 24.43710448268778990, 25.27504818406982778, 32.24217181898259099 ) ) ;
#64262 = CARTESIAN_POINT ( 'NONE',  ( -8.734619362451120139, 132.0311980842931519, -5.000000000000003553 ) ) ;
#64263 = VECTOR ( 'NONE', #106136, 1000.000000000000000 ) ;
#64264 = B_SPLINE_CURVE_WITH_KNOTS ( 'NONE', 3,
 ( #64289, #80972, #56696, #98228, #22253, #55620, #55102, #553, #2178, #91230, #59933, #9736, #100354, #29, #32999, #58857, #73947, #67999, #99273, #90680, #18959, #50721, #35129, #50211, #66394, #92252, #65866, #9208, #25452, #57754, #75551, #66944, #26519, #98746 ),
 .UNSPECIFIED., .F., .F.,
 ( 4, 2, 2, 2, 2, 2, 2, 2, 2, 2, 2, 2, 2, 2, 2, 2, 4 ),
 ( 0.01272238763756221996, 0.01351613129786394946, 0.01430987495816567895, 0.01510361861846740844, 0.01589736227876913793, 0.01669110593907085355, 0.01748484959937256569, 0.01827859325967428131, 0.01907233691997599692, 0.01986608058027770907, 0.02065982424057942468, 0.02145356790088113683, 0.02224731156118284897, 0.02304105522148456459, 0.02383479888178628020, 0.02462854254208799235, 0.02542228620238970449 ),
 .UNSPECIFIED. ) ;
#64265 = CYLINDRICAL_SURFACE ( 'NONE', #72188, 4.000000000000001776 ) ;
#64266 = FACE_BOUND ( 'NONE', #90910, .T. ) ;
#64267 = MECHANICAL_DESIGN_GEOMETRIC_PRESENTATION_REPRESENTATION (  '', ( #22943 ), #83192 ) ;
#64268 = VERTEX_POINT ( 'NONE', #78037 ) ;
#64269 = CARTESIAN_POINT ( 'NONE',  ( -4.000000000000001776, 4.898587196589415787E-16, -25.03750572909317285 ) ) ;
#64270 = STYLED_ITEM ( 'NONE', ( #25245 ), #95259 ) ;
#64271 = ORIENTED_EDGE ( 'NONE', *, *, #30652, .T. ) ;
#64272 = EDGE_CURVE ( 'NONE', #28378, #86142, #14656, .T. ) ;
#64273 = SURFACE_STYLE_FILL_AREA ( #96631 ) ;
#64274 =( NAMED_UNIT ( * ) SI_UNIT ( $, .STERADIAN. ) SOLID_ANGLE_UNIT ( ) );
#64275 = UNCERTAINTY_MEASURE_WITH_UNIT (LENGTH_MEASURE( 1.000000000000000082E-05 ), #17440, 'distance_accuracy_value', 'NONE');
#64276 = CARTESIAN_POINT ( 'NONE',  ( -111.9595133392371622, -60.00000000000000711, 163.3268968678650594 ) ) ;
#64277 = DIRECTION ( 'NONE',  ( 0.000000000000000000, 0.000000000000000000, 1.000000000000000000 ) ) ;
#64278 = DIRECTION ( 'NONE',  ( 0.000000000000000000, -1.000000000000000000, 0.000000000000000000 ) ) ;
#64279 = DIRECTION ( 'NONE',  ( -0.000000000000000000, 1.000000000000000000, -0.000000000000000000 ) ) ;
#64280 = CARTESIAN_POINT ( 'NONE',  ( -5.036189802309414709, -5.000000000000015099, -93.73786388411730286 ) ) ;
#64281 = EDGE_CURVE ( 'NONE', #75344, #21876, #11432, .T. ) ;
#64282 = CARTESIAN_POINT ( 'NONE',  ( -82.22570924946400339, -53.55338277734435337, 182.7255397530098833 ) ) ;
#64283 = ORIENTED_EDGE ( 'NONE', *, *, #41470, .T. ) ;
#64284 = ORIENTED_EDGE ( 'NONE', *, *, #96884, .F. ) ;
#64285 = DIRECTION ( 'NONE',  ( -0.000000000000000000, 0.000000000000000000, -1.000000000000000000 ) ) ;
#64286 = EDGE_CURVE ( 'NONE', #9120, #33881, #42473, .T. ) ;
#64287 = CARTESIAN_POINT ( 'NONE',  ( 0.000000000000000000, 0.000000000000000000, 0.000000000000000000 ) ) ;
#64288 = DIRECTION ( 'NONE',  ( -0.000000000000000000, -1.000000000000000000, -0.000000000000000000 ) ) ;
#64289 = CARTESIAN_POINT ( 'NONE',  ( -6.928203230275508773, -65.00000000000000000, 4.000000000000002665 ) ) ;
#64290 = CARTESIAN_POINT ( 'NONE',  ( 4.561387878959841657, 8.776520571373385593, -5.000000000000000000 ) ) ;
#64291 = CARTESIAN_POINT ( 'NONE',  ( -12.98438343323941346, -5.000000000000000000, -86.33384241255676272 ) ) ;
#64292 = DIRECTION ( 'NONE',  ( 0.000000000000000000, 0.000000000000000000, -1.000000000000000000 ) ) ;
#64293 = CARTESIAN_POINT ( 'NONE',  ( 106.9545358495978036, -14.21045842199422715, 174.0142581296349249 ) ) ;
#64294 = CARTESIAN_POINT ( 'NONE',  ( -96.66672766003948425, -59.99999999999999289, 43.67975107286704883 ) ) ;
#64295 = CARTESIAN_POINT ( 'NONE',  ( -63.30547496605215230, -29.05771995010201536, 76.03326579632651772 ) ) ;
#64296 = VERTEX_POINT ( 'NONE', #95291 ) ;
#64297 = CARTESIAN_POINT ( 'NONE',  ( 61.12566064942861033, 38.95341179545530963, 18.04917667391267244 ) ) ;
#64298 = CARTESIAN_POINT ( 'NONE',  ( 70.10167902634712789, -59.99999999999998579, 157.8050041458824353 ) ) ;
#64299 = ORIENTED_EDGE ( 'NONE', *, *, #64705, .T. ) ;
#64300 = CARTESIAN_POINT ( 'NONE',  ( 13.59366797464709720, -56.00856538105860949, 23.64820470065338753 ) ) ;
#64301 = CARTESIAN_POINT ( 'NONE',  ( -7.188101187500002709, -21.68750000204838813, 2.977408999572647819 ) ) ;
#64302 = PRESENTATION_LAYER_ASSIGNMENT (  '', '', ( #57422 ) ) ;
#64303 = ADVANCED_FACE ( 'NONE', ( #85615 ), #41366, .F. ) ;
#64304 = CARTESIAN_POINT ( 'NONE',  ( 19.00000000000000711, 4.000000000000000000, -2.500000000000000000 ) ) ;
#64305 = ORIENTED_EDGE ( 'NONE', *, *, #68757, .T. ) ;
#64306 = CARTESIAN_POINT ( 'NONE',  ( -5.000000000000000000, 0.000000000000000000, -7.131971428571428184 ) ) ;
#64307 = ORIENTED_EDGE ( 'NONE', *, *, #71198, .F. ) ;
#64308 = CARTESIAN_POINT ( 'NONE',  ( 11.39656771499216070, 45.34267223356316379, -14.75529722941197619 ) ) ;
#64309 = AXIS2_PLACEMENT_3D ( 'NONE', #58838, #98728, #42100 ) ;
#64310 = CARTESIAN_POINT ( 'NONE',  ( 2.977408999572650927, -29.75000000204838813, -7.188101187500000933 ) ) ;
#64311 = CARTESIAN_POINT ( 'NONE',  ( -110.8662299446404518, -60.00000000000001421, 187.9351797466592018 ) ) ;
#64312 = CARTESIAN_POINT ( 'NONE',  ( -3.769311339736956867, -1.074854658864006440, 104.1674216685381822 ) ) ;
#64313 = CARTESIAN_POINT ( 'NONE',  ( -7.188101187500002709, -27.68750000204838813, 2.977408999572648707 ) ) ;
#64314 = CARTESIAN_POINT ( 'NONE',  ( 34.67263685779008853, 485.1278622359851624, -2.016271555161434303 ) ) ;
#64315 = CARTESIAN_POINT ( 'NONE',  ( -14.13609923219729758, 21.04331586717165337, 5.955105079798755696 ) ) ;
#64316 =( LENGTH_UNIT ( ) NAMED_UNIT ( * ) SI_UNIT ( .MILLI., .METRE. ) );
#64317 = CARTESIAN_POINT ( 'NONE',  ( 1.308996937480704670, 48.00000000000000000, -75.00000000000001421 ) ) ;
#64318 = EDGE_CURVE ( 'NONE', #95821, #13709, #102312, .T. ) ;
#64319 = CARTESIAN_POINT ( 'NONE',  ( -6.943482370013978944, 105.5284837026072182, 3.973876482044367275 ) ) ;
#64320 = CARTESIAN_POINT ( 'NONE',  ( -43.61687410915253338, 428.0539954125393933, 15.22877806374068932 ) ) ;
#64321 = CARTESIAN_POINT ( 'NONE',  ( 28.05001115153095270, 305.7972385202601231, -9.345431085968183282 ) ) ;
#64322 = B_SPLINE_CURVE_WITH_KNOTS ( 'NONE', 3,
 ( #22240, #70238, #20140, #3379, #95576, #54024 ),
 .UNSPECIFIED., .F., .F.,
 ( 4, 2, 4 ),
 ( 0.003841072314098378879, 0.005765657563962189869, 0.007690242813826001292 ),
 .UNSPECIFIED. ) ;
#64323 = CARTESIAN_POINT ( 'NONE',  ( -33.29236794668833710, -53.37323687183614851, 37.05240020734890294 ) ) ;
#64324 = VERTEX_POINT ( 'NONE', #61340 ) ;
#64325 = CARTESIAN_POINT ( 'NONE',  ( 72.37206225042174879, 4.000000000000015099, 4.898587196589422689E-16 ) ) ;
#64326 = CONICAL_SURFACE ( 'NONE', #98700, 4.172000000000009479, 0.9599310885968813656 ) ;
#64327 = CARTESIAN_POINT ( 'NONE',  ( 41.65387604968816504, -25.70000439954323213, 36.84591881860966822 ) ) ;
#64328 = CARTESIAN_POINT ( 'NONE',  ( 16.57301948837260497, -3.469446951953614189E-15, -4.453875240779963107 ) ) ;
#64329 = ORIENTED_EDGE ( 'NONE', *, *, #82380, .T. ) ;
#64330 = EDGE_CURVE ( 'NONE', #30181, #21224, #104448, .T. ) ;
#64331 = CARTESIAN_POINT ( 'NONE',  ( 5.819846122303831137, -6.321060697774816717, 2.051601713727242871 ) ) ;
#64332 = CARTESIAN_POINT ( 'NONE',  ( -57.76361387290374694, -38.34427059577949137, 89.53802776920677786 ) ) ;
#64333 = VERTEX_POINT ( 'NONE', #13814 ) ;
#64335 = CARTESIAN_POINT ( 'NONE',  ( 27.47093694407817210, 296.2799286419132727, -9.692114557243211692 ) ) ;
#64334 = DIRECTION ( 'NONE',  ( -1.000000000000000000, -1.224606353822377258E-16, -0.000000000000000000 ) ) ;
#64336 = CARTESIAN_POINT ( 'NONE',  ( -52.56483885390523625, 40.83906611473335602, -38.23529411764706509 ) ) ;
#64337 = FACE_OUTER_BOUND ( 'NONE', #39268, .T. ) ;
#64338 = CARTESIAN_POINT ( 'NONE',  ( 6.326622418652847024, 1.327077765693000178, -6.831545684615178970 ) ) ;
#64339 = CARTESIAN_POINT ( 'NONE',  ( 20.77592568779148863, 1.482358050883964840E-15, 0.000000000000000000 ) ) ;
#64340 = CARTESIAN_POINT ( 'NONE',  ( 81.84444444444444855, -4.171999999999998820, 0.000000000000000000 ) ) ;
#64341 = CARTESIAN_POINT ( 'NONE',  ( 9.833493305133801599, 1.593028355512270567E-15, 0.000000000000000000 ) ) ;
#64342 = CARTESIAN_POINT ( 'NONE',  ( 92.12568682370377360, -60.00000000000000000, 21.31078671776630529 ) ) ;
#64343 = CARTESIAN_POINT ( 'NONE',  ( 0.000000000000000000, 2.253471898105741801E-15, 6.500000000000000000 ) ) ;
#64345 = EDGE_CURVE ( 'NONE', #1254, #97405, #47624, .T. ) ;
#64344 = CIRCLE ( 'NONE', #50523, 4.000000000000000000 ) ;
#64346 = FACE_OUTER_BOUND ( 'NONE', #61714, .T. ) ;
#64347 = FACE_OUTER_BOUND ( 'NONE', #20964, .T. ) ;
#64348 = ORIENTED_EDGE ( 'NONE', *, *, #75385, .T. ) ;
#64349 = PRESENTATION_LAYER_ASSIGNMENT (  '', '', ( #69502 ) ) ;
#64350 = AXIS2_PLACEMENT_3D ( 'NONE', #81589, #72978, #30982 ) ;
#64351 = CARTESIAN_POINT ( 'NONE',  ( -68.83349455627663360, -30.00000000000000711, 91.58528215561763375 ) ) ;
#64352 = ORIENTED_EDGE ( 'NONE', *, *, #57891, .F. ) ;
#64353 = DIRECTION ( 'NONE',  ( 1.000000000000000000, -0.000000000000000000, 1.224646799147353207E-16 ) ) ;
#64354 = CARTESIAN_POINT ( 'NONE',  ( -15.50079525336249731, 2.626985771265121450, 0.7904007781020662149 ) ) ;
#64355 = CARTESIAN_POINT ( 'NONE',  ( 9.439237903995151058, 10.07757316356634192, 5.000000000001538325 ) ) ;
#64356 = CARTESIAN_POINT ( 'NONE',  ( 0.000000000000000000, 0.000000000000000000, 0.000000000000000000 ) ) ;
#64357 = CARTESIAN_POINT ( 'NONE',  ( 9.644834624769975662, 26.99109499794224831, 2.648308524638413264 ) ) ;
#64358 = CIRCLE ( 'NONE', #17843, 5.000000000000010658 ) ;
#64359 = CARTESIAN_POINT ( 'NONE',  ( -5.082755093536325042, -24.96875000204838813, -5.082755093536325930 ) ) ;
#64360 = DIRECTION ( 'NONE',  ( -1.000000000000000000, -1.224606353822377258E-16, -0.000000000000000000 ) ) ;
#64361 = CARTESIAN_POINT ( 'NONE',  ( 7.159011423967576171, 41.04792438623271522, -70.58264807953590037 ) ) ;
#64362 = ORIENTED_EDGE ( 'NONE', *, *, #17834, .T. ) ;
#64364 = ORIENTED_EDGE ( 'NONE', *, *, #49060, .F. ) ;
#64363 = CARTESIAN_POINT ( 'NONE',  ( 23.73746414932995208, 1.482358050883964840E-15, 0.000000000000000000 ) ) ;
#64365 = CARTESIAN_POINT ( 'NONE',  ( 82.94231461304056552, -29.08498905877214824, 153.6257325888713581 ) ) ;
#64366 = CARTESIAN_POINT ( 'NONE',  ( -38.78836065780162556, 27.29347728569982223, -12.51982235623151851 ) ) ;
#64367 = ORIENTED_EDGE ( 'NONE', *, *, #33933, .T. ) ;
#64368 = CARTESIAN_POINT ( 'NONE',  ( 96.86866073052655679, 1.030564683017419500E-14, 0.000000000000000000 ) ) ;
#64369 = CARTESIAN_POINT ( 'NONE',  ( 7.551560007654698481, -88.00910351806993503, -2.648022159607833270 ) ) ;
#64370 = CARTESIAN_POINT ( 'NONE',  ( 7.188101187500000044, -14.65625000204838457, 0.000000000000000000 ) ) ;
#64371 = DIRECTION ( 'NONE',  ( -1.000000000000000000, -1.224606353822377258E-16, -0.000000000000000000 ) ) ;
#64372 = CARTESIAN_POINT ( 'NONE',  ( -62.53353137064869571, -57.67819947725070051, 116.5065130283015975 ) ) ;
#64373 = CARTESIAN_POINT ( 'NONE',  ( 16.30148223401143071, 294.5672717626525809, 9.876519804568172134 ) ) ;
#64374 = EDGE_CURVE ( 'NONE', #14056, #25843, #86156, .T. ) ;
#64375 = ORIENTED_EDGE ( 'NONE', *, *, #80635, .T. ) ;
#64376 = DIRECTION ( 'NONE',  ( 0.000000000000000000, 0.000000000000000000, -1.000000000000000000 ) ) ;
#64377 = EDGE_CURVE ( 'NONE', #90268, #34787, #53031, .T. ) ;
#64378 = DIRECTION ( 'NONE',  ( 0.000000000000000000, -1.000000000000000000, 0.000000000000000000 ) ) ;
#64379 = ORIENTED_EDGE ( 'NONE', *, *, #18234, .F. ) ;
#64380 = CARTESIAN_POINT ( 'NONE',  ( -1.469576158976823947E-15, -14.56250000409677092, 8.000000000000000000 ) ) ;
#64381 = CARTESIAN_POINT ( 'NONE',  ( -8.788806404158220786, -13.49444637299766114, 31.95348751068649662 ) ) ;
#64382 = CYLINDRICAL_SURFACE ( 'NONE', #38849, 62.00000000000000000 ) ;
#64383 = MECHANICAL_DESIGN_GEOMETRIC_PRESENTATION_REPRESENTATION (  '', ( #93712 ), #19695 ) ;
#64384 = CARTESIAN_POINT ( 'NONE',  ( 1.248516582103246009, 51.80897656934063633, -8.678012929920056351 ) ) ;
#64385 = CARTESIAN_POINT ( 'NONE',  ( -9.380871178326117388, 87.01116379798325795, 3.467392232194206780 ) ) ;
#64386 = CARTESIAN_POINT ( 'NONE',  ( 39.98585230618361663, 437.4394976705481781, 22.46424175529162426 ) ) ;
#64387 = SHAPE_DEFINITION_REPRESENTATION ( #30457, #84690 ) ;
#64388 = CARTESIAN_POINT ( 'NONE',  ( 38.78798808878313054, 27.29340589088336344, 12.52162365134328503 ) ) ;
#64389 = ORIENTED_EDGE ( 'NONE', *, *, #10849, .F. ) ;
#64390 = CARTESIAN_POINT ( 'NONE',  ( -6.663161659568015871, -48.60989497021113692, 39.31288131909047223 ) ) ;
#64391 = CARTESIAN_POINT ( 'NONE',  ( -0.7408669144221268210, 15.11700796859948426, 9.999999999997887912 ) ) ;
#64392 = MECHANICAL_DESIGN_GEOMETRIC_PRESENTATION_REPRESENTATION (  '', ( #7392 ), #28226 ) ;
#64393 = CARTESIAN_POINT ( 'NONE',  ( 13.46787234807529288, 42.86411582142483923, -91.98473665448270253 ) ) ;
#64394 = CARTESIAN_POINT ( 'NONE',  ( -45.99999999996033750, 464.1057728260254294, 11.12967041736123797 ) ) ;
#64395 = CARTESIAN_POINT ( 'NONE',  ( -58.94526255509084933, -30.00000000000000355, 64.40875316220729019 ) ) ;
#64396 = CARTESIAN_POINT ( 'NONE',  ( 13.87686780678898479, 43.16530558042392585, -91.42246085994810301 ) ) ;
#64397 = ADVANCED_FACE ( 'NONE', ( #14338 ), #88784, .T. ) ;
#64398 = VERTEX_POINT ( 'NONE', #22493 ) ;
#64399 = CARTESIAN_POINT ( 'NONE',  ( -26.02875901964593908, 37.04802764152638872, -9.463460753397949787 ) ) ;
#64400 = CARTESIAN_POINT ( 'NONE',  ( 97.52685887306888901, -57.62337308210403819, 204.3890786062049187 ) ) ;
#64401 = CARTESIAN_POINT ( 'NONE',  ( 97.15356149169568312, 6.123233995736582872E-16, -5.000000000000011546 ) ) ;
#64402 = EDGE_CURVE ( 'NONE', #10553, #32012, #39034, .T. ) ;
#64403 = CARTESIAN_POINT ( 'NONE',  ( 1.734723475976807094E-15, 8.660254037844390851, -10.00000000000000000 ) ) ;
#64404 = CARTESIAN_POINT ( 'NONE',  ( -6.541984439259562301, 53.55430410265342545, 7.323266717688901473 ) ) ;
#64405 = CARTESIAN_POINT ( 'NONE',  ( -74.91408771145276546, -60.00000000000002842, 180.6267571641686516 ) ) ;
#64406 = CARTESIAN_POINT ( 'NONE',  ( -40.77380256327629837, 468.8478597483947965, 21.13608272249925690 ) ) ;
#64407 = CARTESIAN_POINT ( 'NONE',  ( -2.868955696345051593E-16, 7.505553499465148271, -6.177802698399965209 ) ) ;
#64408 = CARTESIAN_POINT ( 'NONE',  ( -45.31383884518383098, 362.9196860876334085, 5.161789940898600548 ) ) ;
#64409 = CARTESIAN_POINT ( 'NONE',  ( -86.40356866038837325, -17.55479932359841655, 177.8634248572934382 ) ) ;
#64411 = ORIENTED_EDGE ( 'NONE', *, *, #72527, .F. ) ;
#64410 = VECTOR ( 'NONE', #99490, 1000.000000000000000 ) ;
#64412 = CARTESIAN_POINT ( 'NONE',  ( 29.65316434010261304, 311.3236015583557901, -7.491929621755849311 ) ) ;
#64413 = VECTOR ( 'NONE', #70465, 1000.000000000000000 ) ;
#64414 = ORIENTED_EDGE ( 'NONE', *, *, #60495, .F. ) ;
#64415 = DIRECTION ( 'NONE',  ( -0.5735764363510494901, -0.8191520442889894671, 0.000000000000000000 ) ) ;
#64416 = EDGE_CURVE ( 'NONE', #32331, #93999, #64076, .T. ) ;
#64417 = FILL_AREA_STYLE ('',( #5114 ) ) ;
#64418 = PRESENTATION_LAYER_ASSIGNMENT (  '', '', ( #23089 ) ) ;
#64419 = B_SPLINE_CURVE_WITH_KNOTS ( 'NONE', 3,
 ( #71176, #104070, #97559, #104601 ),
 .UNSPECIFIED., .F., .F.,
 ( 4, 4 ),
 ( 5.204170427930421283E-18, 0.001842998688486628808 ),
 .UNSPECIFIED. ) ;
#64420 = AXIS2_PLACEMENT_3D ( 'NONE', #31351, #7546, #105205 ) ;
#64421 = CARTESIAN_POINT ( 'NONE',  ( -82.25616362586248442, -37.78509365397592745, -13.24265913212705570 ) ) ;
#64422 = CARTESIAN_POINT ( 'NONE',  ( -42.09158233638501656, 465.7816406625409513, 14.79318349170026003 ) ) ;
#64423 = DIRECTION ( 'NONE',  ( 0.000000000000000000, 0.000000000000000000, 1.000000000000000000 ) ) ;
#64424 = ORIENTED_EDGE ( 'NONE', *, *, #91324, .F. ) ;
#64425 = CARTESIAN_POINT ( 'NONE',  ( -2.504960188439524060, -0.4123968666590282495, 103.1314300587539776 ) ) ;
#64426 = CARTESIAN_POINT ( 'NONE',  ( 13.36238532258455614, 3.698099845770522531, -6.736202370257811545 ) ) ;
#64427 = CARTESIAN_POINT ( 'NONE',  ( -22.45459161911049506, 27.61281158839761574, 32.95901622140758036 ) ) ;
#64428 = DIRECTION ( 'NONE',  ( 0.000000000000000000, -1.000000000000000000, 0.000000000000000000 ) ) ;
#64429 = CARTESIAN_POINT ( 'NONE',  ( 87.24803233485737053, -14.21045842199430709, -0.3983294879921217557 ) ) ;
#64430 = CARTESIAN_POINT ( 'NONE',  ( -77.51929025316718480, -46.43764116288181754, 138.1700848619338728 ) ) ;
#64431 = ORIENTED_EDGE ( 'NONE', *, *, #59478, .T. ) ;
#64432 = CARTESIAN_POINT ( 'NONE',  ( 4.277780656302746287, -59.99999999999995737, 41.98959578111988122 ) ) ;
#64433 = CARTESIAN_POINT ( 'NONE',  ( 77.34876605350574152, -57.51968639827215668, 195.6293917740978827 ) ) ;
#64434 = CARTESIAN_POINT ( 'NONE',  ( 27.26479357511244572, 34.70231048953318265, 7.556984339685708818 ) ) ;
#64435 = CARTESIAN_POINT ( 'NONE',  ( 40.91975823258974998, 312.7996260062327565, -5.723410787371364883 ) ) ;
#64436 = CARTESIAN_POINT ( 'NONE',  ( -30.00000000000000000, 462.0143252985370736, 13.78012569455894720 ) ) ;
#64437 = ORIENTED_EDGE ( 'NONE', *, *, #45847, .F. ) ;
#64438 = DIRECTION ( 'NONE',  ( 0.000000000000000000, 1.000000000000000000, 0.000000000000000000 ) ) ;
#64439 = CARTESIAN_POINT ( 'NONE',  ( -12.50000000000000178, -2.171334558878634802, -15.32410538599969030 ) ) ;
#64441 = CARTESIAN_POINT ( 'NONE',  ( -103.9496743848372375, -52.71021183741716243, 151.5995497774347029 ) ) ;
#64440 = CARTESIAN_POINT ( 'NONE',  ( 16.48330046594864484, 43.81266695705367908, 4.157797401561414752 ) ) ;
#64442 = CARTESIAN_POINT ( 'NONE',  ( 5.082755093536324154, -19.34375000204838457, 5.082755093536326818 ) ) ;
#64443 = CARTESIAN_POINT ( 'NONE',  ( 43.68669919769894960, 485.1453384654001866, 2.541696494115609273 ) ) ;
#64444 = PRESENTATION_STYLE_ASSIGNMENT (( #48227 ) ) ;
#64445 = CARTESIAN_POINT ( 'NONE',  ( 43.74985542820358830, 435.5770091380369422, 16.96136490515564788 ) ) ;
#64446 = ADVANCED_FACE ( 'NONE', ( #98451 ), #44185, .F. ) ;
#64447 = DIRECTION ( 'NONE',  ( -1.000000000000000000, -1.224606353822377258E-16, -0.000000000000000000 ) ) ;
#64448 = PRESENTATION_STYLE_ASSIGNMENT (( #97853 ) ) ;
#64449 = ORIENTED_EDGE ( 'NONE', *, *, #72874, .F. ) ;
#64450 = CARTESIAN_POINT ( 'NONE',  ( -27.99999999999999645, 1.102182119232617714E-15, -9.000000000000000000 ) ) ;
#64452 = CARTESIAN_POINT ( 'NONE',  ( 28.24466138624848455, -32.53086730938267124, 31.34497064575486647 ) ) ;
#64451 = CARTESIAN_POINT ( 'NONE',  ( -32.49743750560201505, -59.99999999999998579, 47.28107978972537495 ) ) ;
#64453 = CARTESIAN_POINT ( 'NONE',  ( 24.41558313457649376, 27.38491394452229954, -32.32218024782121546 ) ) ;
#64454 = EDGE_LOOP ( 'NONE', ( #14288, #19390, #42516, #43728, #90327 ) ) ;
#64455 = EDGE_CURVE ( 'NONE', #50280, #3333, #25264, .T. ) ;
#64456 = EDGE_LOOP ( 'NONE', ( #36625, #6594, #53602, #28847 ) ) ;
#64458 = CARTESIAN_POINT ( 'NONE',  ( 35.40410126533816282, 462.9417065736251402, 4.215193980341727986 ) ) ;
#64457 = DIRECTION ( 'NONE',  ( -1.000000000000000000, -1.224606353822377258E-16, -0.000000000000000000 ) ) ;
#64459 = FACE_OUTER_BOUND ( 'NONE', #100746, .T. ) ;
#64460 = CARTESIAN_POINT ( 'NONE',  ( -43.69307663853834356, 464.9794299858425006, 8.444152807401959393 ) ) ;
#64461 = ADVANCED_FACE ( 'NONE', ( #6247 ), #85538, .F. ) ;
#64462 = AXIS2_PLACEMENT_3D ( 'NONE', #34581, #50188, #25423 ) ;
#64463 = CARTESIAN_POINT ( 'NONE',  ( 5.787483263666111100, 41.99999999999999289, -68.91429206946564534 ) ) ;
#64464 = DIRECTION ( 'NONE',  ( -0.000000000000000000, 1.000000000000000000, 1.877893248421449036E-16 ) ) ;
#64465 = SURFACE_SIDE_STYLE ('',( #32098 ) ) ;
#64466 = ORIENTED_EDGE ( 'NONE', *, *, #37754, .T. ) ;
#64467 = LINE ( 'NONE', #98404, #8318 ) ;
#64468 = CARTESIAN_POINT ( 'NONE',  ( 22.37334360784583964, 26.07629531780827037, -31.03047284417121432 ) ) ;
#64469 = VECTOR ( 'NONE', #35417, 1000.000000000000000 ) ;
#64471 = EDGE_CURVE ( 'NONE', #19214, #100701, #88987, .T. ) ;
#64470 = CARTESIAN_POINT ( 'NONE',  ( 8.572527594031464315E-16, 61.50000000000000000, -6.999999999999992895 ) ) ;
#64472 = FILL_AREA_STYLE_COLOUR ( '', #59913 ) ;
#64473 = DIRECTION ( 'NONE',  ( 1.000000000000000000, 0.000000000000000000, 0.000000000000000000 ) ) ;
#64474 = EDGE_LOOP ( 'NONE', ( #73398, #71065, #55158, #6404 ) ) ;
#64475 = VERTEX_POINT ( 'NONE', #47766 ) ;
#64476 = VERTEX_POINT ( 'NONE', #15948 ) ;
#64477 =( NAMED_UNIT ( * ) SI_UNIT ( $, .STERADIAN. ) SOLID_ANGLE_UNIT ( ) );
#64478 = CARTESIAN_POINT ( 'NONE',  ( 49.53030419665140016, 39.42532954512722654, -42.40708954556809829 ) ) ;
#64479 = FILL_AREA_STYLE_COLOUR ( '', #53993 ) ;
#64480 = CARTESIAN_POINT ( 'NONE',  ( 22.87192968767251955, 303.4467615960384705, 10.06536293368748680 ) ) ;
#64481 = CARTESIAN_POINT ( 'NONE',  ( -42.72097986434771855, 338.4462485437400687, 8.451945447247039667 ) ) ;
#64482 = CARTESIAN_POINT ( 'NONE',  ( -2.551467019400163405, -69.79337258748924455, 13.23174192411898353 ) ) ;
#64483 = PRESENTATION_STYLE_ASSIGNMENT (( #63433 ) ) ;
#64484 = CARTESIAN_POINT ( 'NONE',  ( 0.000000000000000000, 0.000000000000000000, 0.000000000000000000 ) ) ;
#64485 = ORIENTED_EDGE ( 'NONE', *, *, #51806, .F. ) ;
#64486 = CARTESIAN_POINT ( 'NONE',  ( -10.28624191511820207, 43.25714326066858462, 15.40779740156164124 ) ) ;
#64487 = ORIENTED_EDGE ( 'NONE', *, *, #40478, .T. ) ;
#64488 = CARTESIAN_POINT ( 'NONE',  ( 0.000000000000000000, -0.5000000000000000000, 0.000000000000000000 ) ) ;
#64489 = CARTESIAN_POINT ( 'NONE',  ( -6.663120783604504993, -3.846954578057071750, -6.460786012260017586 ) ) ;
#64490 = DIRECTION ( 'NONE',  ( 0.000000000000000000, -1.000000000000000000, 0.000000000000000000 ) ) ;
#64491 = DIRECTION ( 'NONE',  ( 0.000000000000000000, 1.000000000000000000, 0.000000000000000000 ) ) ;
#64492 = CARTESIAN_POINT ( 'NONE',  ( 67.07649707454891086, -42.95850431900807109, 94.37125772477908470 ) ) ;
#64493 = AXIS2_PLACEMENT_3D ( 'NONE', #93288, #2663, #76024 ) ;
#64494 = EDGE_LOOP ( 'NONE', ( #86325, #85781, #15711, #62691, #86254, #61177 ) ) ;
#64495 = CARTESIAN_POINT ( 'NONE',  ( 18.58349330513380337, 1.593028355512270567E-15, 0.000000000000000000 ) ) ;
#64496 = CARTESIAN_POINT ( 'NONE',  ( 5.082755093536324154, -28.34375000204838813, 5.082755093536326818 ) ) ;
#64497 = CONICAL_SURFACE ( 'NONE', #17984, 5.000000000000001776, 0.9599310885968803664 ) ;
#64498 = DIRECTION ( 'NONE',  ( -0.000000000000000000, -1.000000000000000000, -0.000000000000000000 ) ) ;
#64499 = ADVANCED_FACE ( 'NONE', ( #39183 ), #40704, .T. ) ;
#64500 = AXIS2_PLACEMENT_3D ( 'NONE', #76299, #27812, #11557 ) ;
#64502 = EDGE_LOOP ( 'NONE', ( #26066, #93106, #98094, #50826, #8311 ) ) ;
#64501 = COLOUR_RGB ( '', 0.40784314, 0.44705882, 0.49803922) ;
#64503 = CARTESIAN_POINT ( 'NONE',  ( 47.24255575150607456, 16.92138162734670459, 16.58509488952848443 ) ) ;
#64504 = EDGE_CURVE ( 'NONE', #85144, #73958, #61443, .T. ) ;
#64505 = EDGE_CURVE ( 'NONE', #4508, #80260, #63124, .T. ) ;
#64506 = CARTESIAN_POINT ( 'NONE',  ( -37.51493083963608655, 491.7337707781560425, 12.51683509955429408 ) ) ;
#64507 = CARTESIAN_POINT ( 'NONE',  ( 4.898587196589412829E-16, -28.81250000409677270, -8.000000000000000000 ) ) ;
#64508 = SURFACE_SIDE_STYLE ('',( #97375 ) ) ;
#64509 = CARTESIAN_POINT ( 'NONE',  ( 9.797372177749775091, 246.5349050515243903, 2.014953862275845609 ) ) ;
#64510 = CARTESIAN_POINT ( 'NONE',  ( 10.00004721872059754, 34.00011804681151517, -0.2617599822266539755 ) ) ;
#64511 = CARTESIAN_POINT ( 'NONE',  ( 7.934914944860276265, -6.131543527998897680, -1.051261972695689328 ) ) ;
#64512 = CARTESIAN_POINT ( 'NONE',  ( 16.53374548247488462, 304.5679859715410771, 9.876672295198167362 ) ) ;
#64513 = VERTEX_POINT ( 'NONE', #23009 ) ;
#64514 = CARTESIAN_POINT ( 'NONE',  ( 0.000000000000000000, 0.000000000000000000, -4.987924522925830217 ) ) ;
#64515 = CARTESIAN_POINT ( 'NONE',  ( 16.39870140197033876, -60.00000000000000000, 39.87645633822717883 ) ) ;
#64516 = CARTESIAN_POINT ( 'NONE',  ( -98.88010798912279142, -29.99999999999999289, 189.1023777079059869 ) ) ;
#64517 = EDGE_CURVE ( 'NONE', #35056, #27202, #19891, .T. ) ;
#64518 = DIRECTION ( 'NONE',  ( 0.000000000000000000, 1.000000000000000000, 0.000000000000000000 ) ) ;
#64519 = CARTESIAN_POINT ( 'NONE',  ( 52.48690415104037754, -57.67637498706665866, 84.06783307720677101 ) ) ;
#64521 = CARTESIAN_POINT ( 'NONE',  ( 73.59428447264397732, 6.856755485862130937E-15, 0.000000000000000000 ) ) ;
#64520 = CARTESIAN_POINT ( 'NONE',  ( 0.000000000000000000, 4.898587196589412829E-16, -4.000000000000000000 ) ) ;
#64522 = CARTESIAN_POINT ( 'NONE',  ( -0.01393140247697588312, -21.31702117966834109, -38.55283400289633278 ) ) ;
#64523 = CARTESIAN_POINT ( 'NONE',  ( -30.00000000000000355, 461.8887775513397287, 11.55279652844096994 ) ) ;
#64524 = COLOUR_RGB ( '', 0.09019608, 0.27058824, 0.51372549) ;
#64525 = CARTESIAN_POINT ( 'NONE',  ( 6.516354785991091835E-11, 40.83842593836580903, 65.00000000086684793 ) ) ;
#64526 = CARTESIAN_POINT ( 'NONE',  ( -26.01021955176325662, -60.00000000000000711, 41.44826368662123173 ) ) ;
#64527 = AXIS2_PLACEMENT_3D ( 'NONE', #47045, #28263, #79943 ) ;
#64528 = CIRCLE ( 'NONE', #42183, 3.400000000000000355 ) ;
#64529 = CIRCLE ( 'NONE', #40413, 4.000000000000000888 ) ;
#64530 = CARTESIAN_POINT ( 'NONE',  ( -5.000000000000000888, 0.000000000000000000, -5.000000000000000000 ) ) ;
#64531 = CARTESIAN_POINT ( 'NONE',  ( -86.81214770105786727, -42.79374714232908872, 189.6642773476453954 ) ) ;
#64532 = ORIENTED_EDGE ( 'NONE', *, *, #91917, .T. ) ;
#64533 = CARTESIAN_POINT ( 'NONE',  ( 17.50000000000007105, 51.77766888149943014, 61.91533629922624016 ) ) ;
#64534 = CARTESIAN_POINT ( 'NONE',  ( -2.504928271494545555, -49.58762337132401399, 103.1313799838700191 ) ) ;
#64535 = CARTESIAN_POINT ( 'NONE',  ( -12.44423993302578779, -42.95776644870394989, 31.10559508463949285 ) ) ;
#64536 = CIRCLE ( 'NONE', #9453, 1.000000000000002220 ) ;
#64538 = CARTESIAN_POINT ( 'NONE',  ( 17.61650669486618881, -3.999999999999998224, 0.000000000000000000 ) ) ;
#64537 = DIRECTION ( 'NONE',  ( -1.000000000000000000, 0.000000000000000000, 0.000000000000000000 ) ) ;
#64539 = VERTEX_POINT ( 'NONE', #57449 ) ;
#64540 = DIRECTION ( 'NONE',  ( 0.000000000000000000, 0.000000000000000000, 1.000000000000000000 ) ) ;
#64541 = CARTESIAN_POINT ( 'NONE',  ( -7.466456039917235721, -3.088347863564611995, -19.53079660665211037 ) ) ;
#64542 = CARTESIAN_POINT ( 'NONE',  ( -6.928203230275508773, 30.26526156932586176, 4.000000000000000000 ) ) ;
#64543 = CARTESIAN_POINT ( 'NONE',  ( 0.000000000000000000, -3.138931148610827481E-15, 0.000000000000000000 ) ) ;
#64544 =( BOUNDED_SURFACE ( )  B_SPLINE_SURFACE ( 3, 2, ( 
 ( #48694, #56789, #81068 ),
 ( #16891, #97259, #49771 ),
 ( #48167, #7180, #89714 ),
 ( #40094, #32020, #74041 ),
 ( #24483, #81580, #98837 ),
 ( #73502, #106400, #123 ),
 ( #90236, #33093, #71929 ),
 ( #104830, #30974, #96746 ),
 ( #35215, #91834, #50298 ),
 ( #84805, #27676, #35764 ),
 ( #43804, #9831, #2809 ),
 ( #19049, #84270, #10888 ) ),
 .UNSPECIFIED., .F., .F., .F. ) 
 B_SPLINE_SURFACE_WITH_KNOTS ( ( 4, 2, 2, 2, 2, 4 ),
 ( 3, 3 ),
 ( -8.946836327350382589E-16, 0.001912832793471382726, 0.002869249190207521540, 0.003825665586943660136, 0.005738498380415937329, 0.007651331173888214522 ),
 ( 0.000000000000000000, 1.000000000000000000 ),
 .UNSPECIFIED. ) 
 GEOMETRIC_REPRESENTATION_ITEM ( )  RATIONAL_B_SPLINE_SURFACE ( (
 ( 1.000000000000000000, 0.8904848454311998784, 1.000000000000000000),
 ( 1.000000000000000000, 0.8829526975545493039, 1.000000000000000000),
 ( 1.000000000000000000, 0.8737225350168510429, 1.000000000000000000),
 ( 1.000000000000000000, 0.8580093906384770319, 1.000000000000000000),
 ( 1.000000000000000000, 0.8524583445354902977, 1.000000000000000000),
 ( 1.000000000000000000, 0.8408236507810400440, 1.000000000000000000),
 ( 1.000000000000000000, 0.8347220996876830723, 1.000000000000000000),
 ( 1.000000000000000000, 0.8161438705883578004, 1.000000000000000000),
 ( 1.000000000000000000, 0.8032788134801324142, 1.000000000000000000),
 ( 1.000000000000000000, 0.7776932730515783154, 1.000000000000000000),
 ( 1.000000000000000000, 0.7649057602317937965, 1.000000000000000000),
 ( 1.000000000000000000, 0.7533433155455840913, 1.000000000000000000) ) ) 
 REPRESENTATION_ITEM ( '' )  SURFACE ( )  );
#64545 = EDGE_CURVE ( 'NONE', #73958, #71240, #99046, .T. ) ;
#64546 = PRESENTATION_STYLE_ASSIGNMENT (( #816 ) ) ;
#64547 = CARTESIAN_POINT ( 'NONE',  ( 73.08118796046841226, -60.00000000000000711, 163.2004635648854105 ) ) ;
#64548 = CARTESIAN_POINT ( 'NONE',  ( -22.18906107735381283, 305.1406206946286943, -9.938500898755204815 ) ) ;
#64549 = ORIENTED_EDGE ( 'NONE', *, *, #82143, .T. ) ;
#64550 = CARTESIAN_POINT ( 'NONE',  ( -5.637738193748796256, -30.00000000000000711, 5.087150282644762989 ) ) ;
#64552 = DIRECTION ( 'NONE',  ( 0.000000000000000000, -1.000000000000000000, 0.000000000000000000 ) ) ;
#64551 = PRESENTATION_STYLE_ASSIGNMENT (( #36069 ) ) ;
#64553 = DIRECTION ( 'NONE',  ( -1.000000000000000000, -0.000000000000000000, -0.000000000000000000 ) ) ;
#64554 = CARTESIAN_POINT ( 'NONE',  ( -5.833333333333327708, -4.000000000000004441, 103.8776713793258608 ) ) ;
#64555 = ORIENTED_EDGE ( 'NONE', *, *, #3634, .F. ) ;
#64556 = CARTESIAN_POINT ( 'NONE',  ( -26.27602720945015236, 310.0396763463044181, 11.16635102967653026 ) ) ;
#64557 = VERTEX_POINT ( 'NONE', #98968 ) ;
#64558 = CARTESIAN_POINT ( 'NONE',  ( 21.10321973014934827, 305.0244315187235884, 8.973846506840480686 ) ) ;
#64559 = AXIS2_PLACEMENT_3D ( 'NONE', #50158, #83064, #17810 ) ;
#64560 = CARTESIAN_POINT ( 'NONE',  ( 4.034557488804142444, 15.07443463110229054, 9.151133496029162373 ) ) ;
#64561 =( NAMED_UNIT ( * ) PLANE_ANGLE_UNIT ( ) SI_UNIT ( $, .RADIAN. ) );
#64562 = ORIENTED_EDGE ( 'NONE', *, *, #70472, .T. ) ;
#64563 = EDGE_CURVE ( 'NONE', #39684, #77823, #80121, .T. ) ;
#64564 = CARTESIAN_POINT ( 'NONE',  ( 23.38163988261896620, 48.00000000000000000, 60.94087333798638895 ) ) ;
#64565 = CARTESIAN_POINT ( 'NONE',  ( -107.0258504621141640, -59.99999999988283861, 107.9273113137431466 ) ) ;
#64566 = EDGE_CURVE ( 'NONE', #19034, #52131, #82027, .T. ) ;
#64567 = CARTESIAN_POINT ( 'NONE',  ( 6.449780583204731244, 2.701143306770497965, -6.840188146834836225 ) ) ;
#64568 = CARTESIAN_POINT ( 'NONE',  ( 77.49317349146313916, -59.99999999999997158, 191.7494575080134780 ) ) ;
#64569 = CARTESIAN_POINT ( 'NONE',  ( 8.099999999999999645, 3.752776749732565253, 6.499999999999997335 ) ) ;
#64570 = CARTESIAN_POINT ( 'NONE',  ( 0.7778616825338859897, 25.97774080628767734, -38.51804523354821441 ) ) ;
#64572 = CARTESIAN_POINT ( 'NONE',  ( 14.55850093289553548, -39.47278144515117759, 30.59000656356446513 ) ) ;
#64571 = CARTESIAN_POINT ( 'NONE',  ( -114.0746799351349665, -60.00000000000000000, 159.9915189542998633 ) ) ;
#64573 = ADVANCED_FACE ( 'NONE', ( #83867 ), #52552, .T. ) ;
#64574 = CARTESIAN_POINT ( 'NONE',  ( 102.2641418190583096, -37.99999999999998579, 159.8959632408159166 ) ) ;
#64575 = CARTESIAN_POINT ( 'NONE',  ( 0.8415227374406197836, 53.50197623860572804, -9.927990696562751793 ) ) ;
#64576 = EDGE_CURVE ( 'NONE', #41809, #5324, #85293, .T. ) ;
#64577 = CARTESIAN_POINT ( 'NONE',  ( -44.85643671809746991, -46.44168872824101868, 45.33582960114114968 ) ) ;
#64578 = CARTESIAN_POINT ( 'NONE',  ( 6.125000000000000000, -60.71953810597977252, 14.41094225130411033 ) ) ;
#64579 = ORIENTED_EDGE ( 'NONE', *, *, #72187, .T. ) ;
#64580 = DIRECTION ( 'NONE',  ( 0.000000000000000000, 1.000000000000000000, 0.000000000000000000 ) ) ;
#64581 = DIRECTION ( 'NONE',  ( -0.000000000000000000, -1.000000000000000000, -0.000000000000000000 ) ) ;
#64582 = CARTESIAN_POINT ( 'NONE',  ( 6.644028492724101120, -3.901260126079175716, 6.757180751914474648 ) ) ;
#64583 = CARTESIAN_POINT ( 'NONE',  ( 5.192560085536412018, -7.356945573687594830, 3.013051918867557077 ) ) ;
#64584 = CARTESIAN_POINT ( 'NONE',  ( 35.57955382936916067, 363.3973965622570859, 2.919629247011395368 ) ) ;
#64585 = ORIENTED_EDGE ( 'NONE', *, *, #77334, .F. ) ;
#64586 = PRESENTATION_STYLE_ASSIGNMENT (( #49441 ) ) ;
#64587 = VERTEX_POINT ( 'NONE', #82268 ) ;
#64588 = CARTESIAN_POINT ( 'NONE',  ( 105.5552223516102828, -29.99999999999804245, 194.5626790352639830 ) ) ;
#64589 = FACE_OUTER_BOUND ( 'NONE', #93808, .T. ) ;
#64591 = EDGE_CURVE ( 'NONE', #90138, #11885, #99268, .T. ) ;
#64590 = CARTESIAN_POINT ( 'NONE',  ( 5.989966392672700479, 41.99624791910017763, -59.62336946609740806 ) ) ;
#64592 = PRESENTATION_STYLE_ASSIGNMENT (( #65109 ) ) ;
#64593 = CARTESIAN_POINT ( 'NONE',  ( 92.54325103475800063, -29.99999999999999645, 103.3538081942403011 ) ) ;
#64594 = FACE_BOUND ( 'NONE', #100055, .T. ) ;
#64595 = VERTEX_POINT ( 'NONE', #8380 ) ;
#64596 = CONICAL_SURFACE ( 'NONE', #18097, 4.000000000000001776, 0.9599310885968808105 ) ;
#64597 = ORIENTED_EDGE ( 'NONE', *, *, #62967, .T. ) ;
#64598 = VERTEX_POINT ( 'NONE', #9979 ) ;
#64599 = CYLINDRICAL_SURFACE ( 'NONE', #42240, 5.000000000000002665 ) ;
#64600 = CARTESIAN_POINT ( 'NONE',  ( 2.435347819570957628E-07, -57.67120202539301488, -44.61186700419775519 ) ) ;
#64601 = FILL_AREA_STYLE ('',( #82366 ) ) ;
#64602 = ORIENTED_EDGE ( 'NONE', *, *, #3920, .F. ) ;
#64603 = SURFACE_STYLE_FILL_AREA ( #99610 ) ;
#64604 = ORIENTED_EDGE ( 'NONE', *, *, #102462, .F. ) ;
#64605 = LINE ( 'NONE', #80232, #56929 ) ;
#64606 = CARTESIAN_POINT ( 'NONE',  ( 78.80898649105323273, -38.66954475436662619, 190.4763790698753496 ) ) ;
#64607 = CARTESIAN_POINT ( 'NONE',  ( 14.35785620000815754, 3.948300967435905751, 4.282865182293652317 ) ) ;
#64608 = AXIS2_PLACEMENT_3D ( 'NONE', #84830, #50840, #93465 ) ;
#64609 = DIRECTION ( 'NONE',  ( 0.000000000000000000, -1.000000000000000000, 0.000000000000000000 ) ) ;
#64610 = CARTESIAN_POINT ( 'NONE',  ( 30.72158347774164611, 320.3865038906847644, 14.25020464585016278 ) ) ;
#64611 = AXIS2_PLACEMENT_3D ( 'NONE', #64287, #16784, #73942 ) ;
#64612 = DIRECTION ( 'NONE',  ( 0.000000000000000000, 0.000000000000000000, 1.000000000000000000 ) ) ;
#64613 = DIRECTION ( 'NONE',  ( 0.000000000000000000, -1.000000000000000000, 0.000000000000000000 ) ) ;
#64614 = AXIS2_PLACEMENT_3D ( 'NONE', #71074, #80749, #55918 ) ;
#64615 = CIRCLE ( 'NONE', #76760, 10.00000000000000000 ) ;
#64616 = DIRECTION ( 'NONE',  ( -0.000000000000000000, -1.000000000000000000, -0.000000000000000000 ) ) ;
#64617 = CARTESIAN_POINT ( 'NONE',  ( 42.71830997089508486, 375.3504811699607444, 18.35052788392003364 ) ) ;
#64618 = EDGE_CURVE ( 'NONE', #87871, #56640, #75232, .T. ) ;
#64619 = CARTESIAN_POINT ( 'NONE',  ( -4.699253986252788451, 7.937442318057748025, 5.000000000000000000 ) ) ;
#64620 = B_SPLINE_CURVE_WITH_KNOTS ( 'NONE', 3,
 ( #83330, #778, #90909, #89841, #33215, #8377, #49898, #61202, #84410, #102713, #68225, #3492, #12618, #27279, #51495, #92485, #18635, #20791, #77912, #37487, #35897, #93569, #77376, #85477, #86559, #60161, #68774 ),
 .UNSPECIFIED., .F., .F.,
 ( 4, 2, 2, 2, 2, 2, 2, 2, 2, 2, 1, 2, 2, 4 ),
 ( 4.772854504744018845E-17, 0.001861613648588184705, 0.002792420472882253205, 0.003723227297176320838, 0.004654034121470389772, 0.005584840945764458706, 0.006515647770058525905, 0.007446454594352594838, 0.009308068242940732706, 0.01023887506723480251, 0.01116968189152887057, 0.01210048871582293864, 0.01303129554011700671, 0.01489290918870514804 ),
 .UNSPECIFIED. ) ;
#64621 = ORIENTED_EDGE ( 'NONE', *, *, #81656, .T. ) ;
#64622 = CARTESIAN_POINT ( 'NONE',  ( -35.49087625329003259, 378.7048482322750260, 5.690525758283039082 ) ) ;
#64623 = CARTESIAN_POINT ( 'NONE',  ( -27.03877384839983833, 307.0702461234657221, 10.91122626378502503 ) ) ;
#64624 = CARTESIAN_POINT ( 'NONE',  ( -4.147930821993661255, -48.94936713426047703, 104.5115743862824331 ) ) ;
#64625 = UNCERTAINTY_MEASURE_WITH_UNIT (LENGTH_MEASURE( 1.000000000000000082E-05 ), #65092, 'distance_accuracy_value', 'NONE');
#64626 = CARTESIAN_POINT ( 'NONE',  ( -3.313708498984765161, -12.96874999999999289, 7.999999999999998224 ) ) ;
#64627 = CARTESIAN_POINT ( 'NONE',  ( 12.33349330513380693, 4.898587196589411843E-16, -4.000000000000001776 ) ) ;
#64628 = EDGE_CURVE ( 'NONE', #99488, #79080, #49901, .T. ) ;
#64629 = ORIENTED_EDGE ( 'NONE', *, *, #43936, .F. ) ;
#64630 = CARTESIAN_POINT ( 'NONE',  ( 85.78844419382012632, -32.04248467167011682, 182.7523993070230972 ) ) ;
#64631 = EDGE_LOOP ( 'NONE', ( #82827, #75622, #103009, #89288, #16965, #48995 ) ) ;
#64632 = CARTESIAN_POINT ( 'NONE',  ( 94.30094425679524761, -57.67269112088474259, 1.199366103519862836 ) ) ;
#64633 = CARTESIAN_POINT ( 'NONE',  ( 35.94513182849205180, 437.3829582663516362, 4.385777999725890552 ) ) ;
#64634 = DIRECTION ( 'NONE',  ( 0.000000000000000000, 1.000000000000000000, 0.000000000000000000 ) ) ;
#64635 = COLOUR_RGB ( '', 0.66274510, 0.83137255, 0.94901961) ;
#64636 = CARTESIAN_POINT ( 'NONE',  ( -79.79064827434378060, -37.99999999999993605, 142.8556830992165203 ) ) ;
#64637 = CARTESIAN_POINT ( 'NONE',  ( 4.175893272574590753, -3.000000000000000000, -7.137815226410167746 ) ) ;
#64638 = CARTESIAN_POINT ( 'NONE',  ( 8.572527594031464315E-16, 60.00000000000000000, -6.999999999999992895 ) ) ;
#64640 = CARTESIAN_POINT ( 'NONE',  ( -44.10120706205752583, 485.7576699374420741, 4.111328371166674600 ) ) ;
#64639 = CARTESIAN_POINT ( 'NONE',  ( 69.67238219402268840, 6.975173280561618775E-15, 0.000000000000000000 ) ) ;
#64641 = ORIENTED_EDGE ( 'NONE', *, *, #7251, .F. ) ;
#64642 = DIRECTION ( 'NONE',  ( 0.000000000000000000, 1.000000000000000000, 0.000000000000000000 ) ) ;
#64643 = CARTESIAN_POINT ( 'NONE',  ( -10.50000000000000000, -5.000000000000000000, -9.904958390907868448 ) ) ;
#64644 = B_SPLINE_CURVE_WITH_KNOTS ( 'NONE', 3,
 ( #58771, #83553, #9653, #75466, #35048, #18323, #51177, #10197, #26959, #61319, #3604, #101235, #69406, #68881, #93137, #12735, #27388, #76946 ),
 .UNSPECIFIED., .F., .F.,
 ( 4, 2, 2, 2, 2, 2, 2, 2, 4 ),
 ( 0.000000000000000000, 0.06250000000000000000, 0.1250000000000000000, 0.1875000000000000000, 0.2500000000000000000, 0.3125000000000000000, 0.3750000000000000000, 0.4375000000000000000, 0.5000000000000000000 ),
 .UNSPECIFIED. ) ;
#64645 = CARTESIAN_POINT ( 'NONE',  ( 9.435590127032984498, 15.92795519102023860, -3.316968746324189699 ) ) ;
#64646 = DIRECTION ( 'NONE',  ( 1.000000000000000000, -0.000000000000000000, -0.000000000000000000 ) ) ;
#64647 = EDGE_CURVE ( 'NONE', #57692, #35426, #6271, .T. ) ;
#64648 = CARTESIAN_POINT ( 'NONE',  ( 67.30223688326144327, -29.89188614501962249, -22.05636472815148963 ) ) ;
#64649 = AXIS2_PLACEMENT_3D ( 'NONE', #70353, #62279, #95167 ) ;
#64650 = ORIENTED_EDGE ( 'NONE', *, *, #45945, .F. ) ;
#64651 = CARTESIAN_POINT ( 'NONE',  ( 67.96666666666666856, 6.915964383211875250E-15, 0.000000000000000000 ) ) ;
#64652 = CARTESIAN_POINT ( 'NONE',  ( -20.22589539060425778, -18.61607622294231490, -33.69375874054126285 ) ) ;
#64654 = CARTESIAN_POINT ( 'NONE',  ( -47.11704795911705190, -34.58946938708281493, -28.29307930567724227 ) ) ;
#64653 = DIRECTION ( 'NONE',  ( -1.000000000000000000, -1.224606353822377258E-16, -0.000000000000000000 ) ) ;
#64655 = AXIS2_PLACEMENT_3D ( 'NONE', #9263, #81539, #17922 ) ;
#64656 = ORIENTED_EDGE ( 'NONE', *, *, #34598, .T. ) ;
#64657 = ORIENTED_EDGE ( 'NONE', *, *, #57838, .T. ) ;
#64658 = CIRCLE ( 'NONE', #23343, 4.000000000000001776 ) ;
#64659 = SURFACE_STYLE_FILL_AREA ( #16102 ) ;
#64660 = CARTESIAN_POINT ( 'NONE',  ( 0.000000000000000000, 0.000000000000000000, -8.574621033218877031 ) ) ;
#64661 = AXIS2_PLACEMENT_3D ( 'NONE', #60971, #85787, #93857 ) ;
#64662 = CARTESIAN_POINT ( 'NONE',  ( -92.52198040298654291, -59.99999999999999289, -1.574747665964571830 ) ) ;
#64663 = ORIENTED_EDGE ( 'NONE', *, *, #15999, .T. ) ;
#64664 = CARTESIAN_POINT ( 'NONE',  ( 0.000000000000000000, -3.331654917651224235, 18.72828050308589454 ) ) ;
#64665 = AXIS2_PLACEMENT_3D ( 'NONE', #46022, #53576, #29862 ) ;
#64666 = CARTESIAN_POINT ( 'NONE',  ( 0.000000000000000000, 273.9999999999999432, 0.000000000000000000 ) ) ;
#64667 = AXIS2_PLACEMENT_3D ( 'NONE', #20440, #61927, #28501 ) ;
#64668 = CARTESIAN_POINT ( 'NONE',  ( 94.84481684524081402, -45.27023405461187622, 194.1702102290486494 ) ) ;
#64670 = CARTESIAN_POINT ( 'NONE',  ( -5.000000000000000000, 0.000000000000000000, -4.289342857142857568 ) ) ;
#64669 = DIRECTION ( 'NONE',  ( 0.000000000000000000, -1.000000000000000000, 0.000000000000000000 ) ) ;
#64671 = CARTESIAN_POINT ( 'NONE',  ( -81.53173708633690353, -46.45041501876503531, 167.1433614008564632 ) ) ;
#64672 = ORIENTED_EDGE ( 'NONE', *, *, #105765, .T. ) ;
#64673 = CIRCLE ( 'NONE', #54109, 10.02537308446410869 ) ;
#64674 = ORIENTED_EDGE ( 'NONE', *, *, #5485, .T. ) ;
#64675 = CONICAL_SURFACE ( 'NONE', #78458, 4.250000000000000000, 0.9599310885968754814 ) ;
#64676 = ORIENTED_EDGE ( 'NONE', *, *, #64628, .F. ) ;
#64678 =( BOUNDED_SURFACE ( )  B_SPLINE_SURFACE ( 1, 2, ( 
 ( #13271, #53228, #20915, #86677, #46197, #34013, #91695, #17808, #9682, #104961, #31619, #48290, #88249, #80660, #71511, #97913, #55836, #89835, #23000, #13804, #88772, #14329, #5723, #32142, #46716, #96350, #62918, #15936, #47235, #80133, #6782, #6237, #5208, #65020, #14866, #70993, #47757, #56372, #81188, #104413, #24065, #30030, #56910, #7298, #54792, #38139, #39701, #40210, #39173, #89308, #103883, #22481, #64507, #55322, #30558, #72577, #97373, #73084, #105479, #72055, #79608, #38647, #105993, #23534, #79085, #15403, #95813, #31103, #63456, #21940, #87723, #63987, #96867, #66614, #33208, #99498, #57979, #16468, #50941, #98443, #1863, #26731, #25672, #50412, #90358, #83856, #1319, #57437, #42870, #83323, #17015, #58537, #48814, #59603, #92476, #7831, #81708, #49891, #82799, #40741, #49351, #74688, #17553, #73626, #8899, #41800, #106531, #75768, #75221, #91952, #25118, #32686, #82258, #9415, #771, #65554, #42333, #8371, #33739, #98959, #24590, #9967, #91439, #18082, #34282, #34821, #67155, #100569, #41273, #66080, #100040, #67687, #74163, #26208, #244, #90900, #59066, #45021, #52546, #60675, #68213, #77369, #27269, #84931, #19709, #20247, #77903, #61741, #101648, #84402, #19181, #53095, #11550, #76294, #86017, #52019, #3485, #68767, #35349, #86552, #69294, #94636, #102168, #4538, #12088, #70343, #11019, #2934, #44478, #37480, #62271, #36425, #101109, #51486, #93562, #4011, #85467, #28317, #60154, #61194, #93018, #43937, #94083, #36941, #69808, #76825, #102704, #27805, #35889, #78418, #28869, #20782, #2404, #29385, #53617, #12609, #45546, #103240, #10497, #18627, #43413, #87067, #104828, #72453, #64380, #87592, #81066, #46069, #7178, #97257, #70871, #21288, #71927, #23400, #104282, #105361, #54124, #38519, #80534, #71382, #13677, #30972, #6652, #56241, #63852, #22350, #29900, #62786, #89179, #96744, #15280, #22877, #39579, #30430, #95675, #95156, #55712, #13140, #55194, #6116, #79486, #39041, #63324, #21817, #48165, #38008, #40092, #72967, #88642, #14734, #54656, #105875, #47633, #103763, #32018, #31500, #96219, #78952, #5074, #46586, #5596, #88123, #14203, #47105, #80007, #1739, #65431, #90771, #33611 ),
 ( #83200, #98835, #34156, #58941, #99913, #50297, #644, #16889, #17422, #67032, #74039, #66483, #57316, #83721, #41682, #75637, #58401, #9296, #33091, #50815, #98325, #82672, #17954, #42208, #106398, #99361, #74570, #24481, #9829, #75090, #26083, #8244, #25543, #65956, #91313, #91833, #90234, #1185, #15811, #49769, #8777, #16339, #57845, #64894, #49225, #42746, #7704, #97781, #23947, #56787, #89712, #82126, #48692, #81578, #40615, #41156, #73499, #32559, #121, #24992, #52418, #93436, #20116, #10366, #84269, #11962, #10887, #67567, #35214, #28202, #43279, #45421, #19588, #102038, #100447, #85889, #92885, #60025, #34693, #76165, #2265, #85336, #3889, #18494, #61613, #51887, #61070, #93965, #44894, #11420, #27675, #59480, #52962, #44346, #77243, #101519, #68084, #36302, #102581, #77778, #36821, #53499, #86423, #28728, #100978, #69687, #19048, #26606, #69168, #3358, #94508, #35761, #27135, #20660, #12487, #78292, #84804, #92345, #51358, #68641, #43803, #76697, #2808, #60547, #63190, #37349, #87996, #6516, #13550, #88524, #70212, #54525, #96614, #87469, #29787, #46982, #22749, #80403, #79880, #38398, #45940, #78819, #39451, #14074, #72328, #5988, #55587, #46468, #4952, #4411, #38915, #29266, #71263, #22217, #95548, #55066, #79356, #37882, #105232, #54005, #64257, #89047, #71782, #104691, #70740, #31376, #63730, #13013, #97128, #30845, #5473, #14600, #103115, #15149, #48034, #62148, #95038, #104157, #30302, #21175, #103635, #96083, #47512, #86945, #23268, #56112, #62665, #21692, #514, #17297, #57186, #39968, #81456, #8647, #73907, #31888, #82543, #7570, #65826, #24344, #97645, #42079, #24860, #50171, #57711, #66902, #41551, #25957, #73367, #65299, #40455, #99786, #17826, #32957, #23813, #7051, #16208, #33479, #8111, #49091, #56658, #98705, #89583, #40488, #81993, #74435, #90637, #15676, #16745, #90102, #106265, #34029, #48565, #98189, #64770, #91708, #41024, #49636, #66353, #99237, #72839, #58816, #25405, #105750, #58265, #91190, #83074, #32428, #80941, #9165, #74962, #1054, #26474, #68501, #10758, #51218, #52291, #11830, #101911, #28068, #69559, #102449, #44760, #84143, #11287, #76037, #9699, #85202, #19456 ) ),
 .UNSPECIFIED., .F., .F., .F. ) 
 B_SPLINE_SURFACE_WITH_KNOTS ( ( 2, 2 ),
 ( 3, 2, 2, 2, 2, 2, 2, 2, 2, 2, 2, 2, 2, 2, 2, 2, 2, 2, 2, 2, 2, 2, 2, 2, 2, 2, 2, 2, 2, 2, 2, 2, 2, 2, 2, 2, 2, 2, 2, 2, 2, 2, 2, 2, 2, 2, 2, 2, 2, 2, 2, 2, 2, 2, 2, 2, 2, 2, 2, 2, 2, 2, 2, 2, 2, 2, 2, 2, 2, 2, 2, 2, 2, 2, 2, 2, 2, 2, 2, 2, 2, 2, 2, 2, 2, 2, 2, 2, 2, 2, 2, 2, 2, 2, 2, 2, 2, 2, 2, 2, 2, 2, 2, 2, 2, 2, 2, 2, 2, 2, 2, 2, 2, 2, 2, 2, 2, 2, 2, 2, 2, 2, 2, 2, 2, 2, 2, 2, 2, 2, 2, 2, 2, 2, 3 ),
 ( 0.000000000000000000, 1.000000000000000000 ),
 ( 0.000000000000000000, 0.007352941176470588133, 0.01470588235294117627, 0.02205882352941176613, 0.02941176470588235253, 0.03676470588235294240, 0.04411764705882353227, 0.05147058823529411520, 0.05882352941176470507, 0.06617647058823529493, 0.07352941176470588480, 0.08088235294117647467, 0.08823529411764706454, 0.09558823529411764053, 0.1029411764705882304, 0.1102941176470588203, 0.1176470588235294101, 0.1250000000000000000, 0.1323529411764705899, 0.1397058823529411797, 0.1470588235294117696, 0.1544117647058823595, 0.1617647058823529493, 0.1691176470588235392, 0.1764705882352941291, 0.1838235294117647189, 0.1911764705882352811, 0.1985294117647058709, 0.2058823529411764608, 0.2132352941176470507, 0.2205882352941176405, 0.2279411764705882304, 0.2352941176470588203, 0.2426470588235294101, 0.2500000000000000000, 0.2573529411764705621, 0.2647058823529411797, 0.2720588235294117418, 0.2794117647058823595, 0.2867647058823529216, 0.2941176470588235392, 0.3014705882352941013, 0.3088235294117647189, 0.3161764705882352811, 0.3235294117647058987, 0.3308823529411764608, 0.3382352941176470784, 0.3455882352941176405, 0.3529411764705882582, 0.3602941176470588203, 0.3676470588235294379, 0.3750000000000000000, 0.3823529411764705621, 0.3897058823529411797, 0.3970588235294117418, 0.4044117647058823595, 0.4117647058823529216, 0.4191176470588235392, 0.4264705882352941013, 0.4338235294117647189, 0.4411764705882352811, 0.4485294117647058987, 0.4558823529411764608, 0.4632352941176470784, 0.4705882352941176405, 0.4779411764705882582, 0.4852941176470588203, 0.4926470588235294379, 0.5000000000000000000, 0.5073529411764705621, 0.5147058823529411242, 0.5220588235294117974, 0.5294117647058823595, 0.5367647058823529216, 0.5441176470588234837, 0.5514705882352941568, 0.5588235294117647189, 0.5661764705882352811, 0.5735294117647058432, 0.5808823529411765163, 0.5882352941176470784, 0.5955882352941176405, 0.6029411764705882026, 0.6102941176470588758, 0.6176470588235294379, 0.6250000000000000000, 0.6323529411764705621, 0.6397058823529411242, 0.6470588235294117974, 0.6544117647058823595, 0.6617647058823529216, 0.6691176470588234837, 0.6764705882352941568, 0.6838235294117647189, 0.6911764705882352811, 0.6985294117647058432, 0.7058823529411765163, 0.7132352941176470784, 0.7205882352941176405, 0.7279411764705882026, 0.7352941176470588758, 0.7426470588235294379, 0.7500000000000000000, 0.7573529411764705621, 0.7647058823529411242, 0.7720588235294117974, 0.7794117647058823595, 0.7867647058823529216, 0.7941176470588234837, 0.8014705882352941568, 0.8088235294117647189, 0.8161764705882352811, 0.8235294117647058432, 0.8308823529411765163, 0.8382352941176470784, 0.8455882352941176405, 0.8529411764705882026, 0.8602941176470588758, 0.8676470588235294379, 0.8750000000000000000, 0.8823529411764705621, 0.8897058823529411242, 0.8970588235294117974, 0.9044117647058823595, 0.9117647058823529216, 0.9191176470588234837, 0.9264705882352941568, 0.9338235294117647189, 0.9411764705882352811, 0.9485294117647058432, 0.9558823529411765163, 0.9632352941176470784, 0.9705882352941176405, 0.9779411764705882026, 0.9804062415945057340 ),
 .UNSPECIFIED. ) 
 GEOMETRIC_REPRESENTATION_ITEM ( )  RATIONAL_B_SPLINE_SURFACE ( (
 ( 1.000000000000000000, 0.9238795325112867385, 1.000000000000000000, 0.9238795325112867385, 1.000000000000000000, 0.9238795325112867385, 1.000000000000000000, 0.9238795325112867385, 1.000000000000000000, 0.9238795325112867385, 1.000000000000000000, 0.9238795325112867385, 1.000000000000000000, 0.9238795325112867385, 1.000000000000000000, 0.9238795325112867385, 1.000000000000000000, 0.9238795325112867385, 1.000000000000000000, 0.9238795325112867385, 1.000000000000000000, 0.9238795325112867385, 1.000000000000000000, 0.9238795325112867385, 1.000000000000000000, 0.9238795325112867385, 1.000000000000000000, 0.9238795325112867385, 1.000000000000000000, 0.9238795325112867385, 1.000000000000000000, 0.9238795325112867385, 1.000000000000000000, 0.9238795325112867385, 1.000000000000000000, 0.9238795325112867385, 1.000000000000000000, 0.9238795325112867385, 1.000000000000000000, 0.9238795325112867385, 1.000000000000000000, 0.9238795325112867385, 1.000000000000000000, 0.9238795325112867385, 1.000000000000000000, 0.9238795325112867385, 1.000000000000000000, 0.9238795325112867385, 1.000000000000000000, 0.9238795325112867385, 1.000000000000000000, 0.9238795325112867385, 1.000000000000000000, 0.9238795325112867385, 1.000000000000000000, 0.9238795325112867385, 1.000000000000000000, 0.9238795325112867385, 1.000000000000000000, 0.9238795325112867385, 1.000000000000000000, 0.9238795325112867385, 1.000000000000000000, 0.9238795325112867385, 1.000000000000000000, 0.9238795325112867385, 1.000000000000000000, 0.9238795325112867385, 1.000000000000000000, 0.9238795325112867385, 1.000000000000000000, 0.9238795325112867385, 1.000000000000000000, 0.9238795325112867385, 1.000000000000000000, 0.9238795325112867385, 1.000000000000000000, 0.9238795325112867385, 1.000000000000000000, 0.9238795325112867385, 1.000000000000000000, 0.9238795325112867385, 1.000000000000000000, 0.9238795325112867385, 1.000000000000000000, 0.9238795325112867385, 1.000000000000000000, 0.9238795325112867385, 1.000000000000000000, 0.9238795325112867385, 1.000000000000000000, 0.9238795325112867385, 1.000000000000000000, 0.9238795325112867385, 1.000000000000000000, 0.9238795325112867385, 1.000000000000000000, 0.9238795325112867385, 1.000000000000000000, 0.9238795325112867385, 1.000000000000000000, 0.9238795325112867385, 1.000000000000000000, 0.9238795325112867385, 1.000000000000000000, 0.9238795325112867385, 1.000000000000000000, 0.9238795325112867385, 1.000000000000000000, 0.9238795325112867385, 1.000000000000000000, 0.9238795325112867385, 1.000000000000000000, 0.9238795325112867385, 1.000000000000000000, 0.9238795325112867385, 1.000000000000000000, 0.9238795325112867385, 1.000000000000000000, 0.9238795325112867385, 1.000000000000000000, 0.9238795325112867385, 1.000000000000000000, 0.9238795325112867385, 1.000000000000000000, 0.9238795325112867385, 1.000000000000000000, 0.9238795325112867385, 1.000000000000000000, 0.9238795325112867385, 1.000000000000000000, 0.9238795325112867385, 1.000000000000000000, 0.9238795325112867385, 1.000000000000000000, 0.9238795325112867385, 1.000000000000000000, 0.9238795325112867385, 1.000000000000000000, 0.9238795325112867385, 1.000000000000000000, 0.9238795325112867385, 1.000000000000000000, 0.9238795325112867385, 1.000000000000000000, 0.9238795325112867385, 1.000000000000000000, 0.9238795325112867385, 1.000000000000000000, 0.9238795325112867385, 1.000000000000000000, 0.9238795325112867385, 1.000000000000000000, 0.9238795325112867385, 1.000000000000000000, 0.9238795325112867385, 1.000000000000000000, 0.9238795325112867385, 1.000000000000000000, 0.9238795325112867385, 1.000000000000000000, 0.9238795325112867385, 1.000000000000000000, 0.9238795325112867385, 1.000000000000000000, 0.9238795325112867385, 1.000000000000000000, 0.9238795325112867385, 1.000000000000000000, 0.9238795325112867385, 1.000000000000000000, 0.9238795325112867385, 1.000000000000000000, 0.9238795325112867385, 1.000000000000000000, 0.9238795325112867385, 1.000000000000000000, 0.9238795325112867385, 1.000000000000000000, 0.9238795325112867385, 1.000000000000000000, 0.9238795325112867385, 1.000000000000000000, 0.9238795325112867385, 1.000000000000000000, 0.9238795325112867385, 1.000000000000000000, 0.9238795325112867385, 1.000000000000000000, 0.9238795325112867385, 1.000000000000000000, 0.9238795325112867385, 1.000000000000000000, 0.9238795325112867385, 1.000000000000000000, 0.9238795325112867385, 1.000000000000000000, 0.9238795325112867385, 1.000000000000000000, 0.9238795325112867385, 1.000000000000000000, 0.9238795325112867385, 1.000000000000000000, 0.9238795325112867385, 1.000000000000000000, 0.9238795325112867385, 1.000000000000000000, 0.9238795325112867385, 1.000000000000000000, 0.9238795325112867385, 1.000000000000000000, 0.9238795325112867385, 1.000000000000000000, 0.9238795325112867385, 1.000000000000000000, 0.9238795325112867385, 1.000000000000000000, 0.9238795325112867385, 1.000000000000000000, 0.9238795325112867385, 1.000000000000000000, 0.9238795325112867385, 1.000000000000000000, 0.9238795325112867385, 1.000000000000000000, 0.9238795325112867385, 1.000000000000000000, 0.9238795325112867385, 1.000000000000000000, 0.9238795325112867385, 1.000000000000000000, 0.9238795325112867385, 1.000000000000000000, 0.9238795325112867385, 1.000000000000000000, 0.9238795325112867385, 1.000000000000000000, 0.9238795325112867385, 1.000000000000000000, 0.9238795325112867385, 1.000000000000000000, 0.9238795325112867385, 1.000000000000000000, 0.9238795325112867385, 1.000000000000000000, 0.9238795325112867385, 1.000000000000000000, 0.9238795325112867385, 1.000000000000000000, 0.9238795325112867385, 1.000000000000000000, 0.9238795325112867385, 1.000000000000000000, 0.9238795325112867385, 1.000000000000000000, 0.9238795325112867385, 1.000000000000000000, 0.9238795325112867385, 1.000000000000000000, 0.9238795325112867385, 1.000000000000000000, 0.9238795325112867385, 1.000000000000000000, 0.9238795325112867385, 1.000000000000000000, 0.9238795325112867385, 1.000000000000000000, 0.9744807002913096206, 0.9660720326926630630),
 ( 1.000000000000000000, 0.9238795325112867385, 1.000000000000000000, 0.9238795325112867385, 1.000000000000000000, 0.9238795325112867385, 1.000000000000000000, 0.9238795325112867385, 1.000000000000000000, 0.9238795325112867385, 1.000000000000000000, 0.9238795325112867385, 1.000000000000000000, 0.9238795325112867385, 1.000000000000000000, 0.9238795325112867385, 1.000000000000000000, 0.9238795325112867385, 1.000000000000000000, 0.9238795325112867385, 1.000000000000000000, 0.9238795325112867385, 1.000000000000000000, 0.9238795325112867385, 1.000000000000000000, 0.9238795325112867385, 1.000000000000000000, 0.9238795325112867385, 1.000000000000000000, 0.9238795325112867385, 1.000000000000000000, 0.9238795325112867385, 1.000000000000000000, 0.9238795325112867385, 1.000000000000000000, 0.9238795325112867385, 1.000000000000000000, 0.9238795325112867385, 1.000000000000000000, 0.9238795325112867385, 1.000000000000000000, 0.9238795325112867385, 1.000000000000000000, 0.9238795325112867385, 1.000000000000000000, 0.9238795325112867385, 1.000000000000000000, 0.9238795325112867385, 1.000000000000000000, 0.9238795325112867385, 1.000000000000000000, 0.9238795325112867385, 1.000000000000000000, 0.9238795325112867385, 1.000000000000000000, 0.9238795325112867385, 1.000000000000000000, 0.9238795325112867385, 1.000000000000000000, 0.9238795325112867385, 1.000000000000000000, 0.9238795325112867385, 1.000000000000000000, 0.9238795325112867385, 1.000000000000000000, 0.9238795325112867385, 1.000000000000000000, 0.9238795325112867385, 1.000000000000000000, 0.9238795325112867385, 1.000000000000000000, 0.9238795325112867385, 1.000000000000000000, 0.9238795325112867385, 1.000000000000000000, 0.9238795325112867385, 1.000000000000000000, 0.9238795325112867385, 1.000000000000000000, 0.9238795325112867385, 1.000000000000000000, 0.9238795325112867385, 1.000000000000000000, 0.9238795325112867385, 1.000000000000000000, 0.9238795325112867385, 1.000000000000000000, 0.9238795325112867385, 1.000000000000000000, 0.9238795325112867385, 1.000000000000000000, 0.9238795325112867385, 1.000000000000000000, 0.9238795325112867385, 1.000000000000000000, 0.9238795325112867385, 1.000000000000000000, 0.9238795325112867385, 1.000000000000000000, 0.9238795325112867385, 1.000000000000000000, 0.9238795325112867385, 1.000000000000000000, 0.9238795325112867385, 1.000000000000000000, 0.9238795325112867385, 1.000000000000000000, 0.9238795325112867385, 1.000000000000000000, 0.9238795325112867385, 1.000000000000000000, 0.9238795325112867385, 1.000000000000000000, 0.9238795325112867385, 1.000000000000000000, 0.9238795325112867385, 1.000000000000000000, 0.9238795325112867385, 1.000000000000000000, 0.9238795325112867385, 1.000000000000000000, 0.9238795325112867385, 1.000000000000000000, 0.9238795325112867385, 1.000000000000000000, 0.9238795325112867385, 1.000000000000000000, 0.9238795325112867385, 1.000000000000000000, 0.9238795325112867385, 1.000000000000000000, 0.9238795325112867385, 1.000000000000000000, 0.9238795325112867385, 1.000000000000000000, 0.9238795325112867385, 1.000000000000000000, 0.9238795325112867385, 1.000000000000000000, 0.9238795325112867385, 1.000000000000000000, 0.9238795325112867385, 1.000000000000000000, 0.9238795325112867385, 1.000000000000000000, 0.9238795325112867385, 1.000000000000000000, 0.9238795325112867385, 1.000000000000000000, 0.9238795325112867385, 1.000000000000000000, 0.9238795325112867385, 1.000000000000000000, 0.9238795325112867385, 1.000000000000000000, 0.9238795325112867385, 1.000000000000000000, 0.9238795325112867385, 1.000000000000000000, 0.9238795325112867385, 1.000000000000000000, 0.9238795325112867385, 1.000000000000000000, 0.9238795325112867385, 1.000000000000000000, 0.9238795325112867385, 1.000000000000000000, 0.9238795325112867385, 1.000000000000000000, 0.9238795325112867385, 1.000000000000000000, 0.9238795325112867385, 1.000000000000000000, 0.9238795325112867385, 1.000000000000000000, 0.9238795325112867385, 1.000000000000000000, 0.9238795325112867385, 1.000000000000000000, 0.9238795325112867385, 1.000000000000000000, 0.9238795325112867385, 1.000000000000000000, 0.9238795325112867385, 1.000000000000000000, 0.9238795325112867385, 1.000000000000000000, 0.9238795325112867385, 1.000000000000000000, 0.9238795325112867385, 1.000000000000000000, 0.9238795325112867385, 1.000000000000000000, 0.9238795325112867385, 1.000000000000000000, 0.9238795325112867385, 1.000000000000000000, 0.9238795325112867385, 1.000000000000000000, 0.9238795325112867385, 1.000000000000000000, 0.9238795325112867385, 1.000000000000000000, 0.9238795325112867385, 1.000000000000000000, 0.9238795325112867385, 1.000000000000000000, 0.9238795325112867385, 1.000000000000000000, 0.9238795325112867385, 1.000000000000000000, 0.9238795325112867385, 1.000000000000000000, 0.9238795325112867385, 1.000000000000000000, 0.9238795325112867385, 1.000000000000000000, 0.9238795325112867385, 1.000000000000000000, 0.9238795325112867385, 1.000000000000000000, 0.9238795325112867385, 1.000000000000000000, 0.9238795325112867385, 1.000000000000000000, 0.9238795325112867385, 1.000000000000000000, 0.9238795325112867385, 1.000000000000000000, 0.9238795325112867385, 1.000000000000000000, 0.9238795325112867385, 1.000000000000000000, 0.9238795325112867385, 1.000000000000000000, 0.9238795325112867385, 1.000000000000000000, 0.9238795325112867385, 1.000000000000000000, 0.9238795325112867385, 1.000000000000000000, 0.9238795325112867385, 1.000000000000000000, 0.9238795325112867385, 1.000000000000000000, 0.9238795325112867385, 1.000000000000000000, 0.9238795325112867385, 1.000000000000000000, 0.9238795325112867385, 1.000000000000000000, 0.9238795325112867385, 1.000000000000000000, 0.9238795325112867385, 1.000000000000000000, 0.9238795325112867385, 1.000000000000000000, 0.9238795325112867385, 1.000000000000000000, 0.9238795325112867385, 1.000000000000000000, 0.9238795325112867385, 1.000000000000000000, 0.9238795325112867385, 1.000000000000000000, 0.9238795325112867385, 1.000000000000000000, 0.9744807002913096206, 0.9660720326926630630) ) ) 
 REPRESENTATION_ITEM ( '' )  SURFACE ( )  );
#64677 = CARTESIAN_POINT ( 'NONE',  ( 3.400000000000000355, 0.000000000000000000, -0.4455245229258316120 ) ) ;
#64679 = CARTESIAN_POINT ( 'NONE',  ( -5.000000000000000000, -13.80294717177778274, 10.52286356751779550 ) ) ;
#64680 = FACE_OUTER_BOUND ( 'NONE', #86645, .T. ) ;
#64681 = EDGE_LOOP ( 'NONE', ( #12712, #74126, #96859, #103835, #37442 ) ) ;
#64682 = ADVANCED_FACE ( 'NONE', ( #50953 ), #18092, .T. ) ;
#64683 = DIRECTION ( 'NONE',  ( 0.000000000000000000, 0.000000000000000000, 1.000000000000000000 ) ) ;
#64684 = CARTESIAN_POINT ( 'NONE',  ( -7.290763246116593538E-15, 7.666536031838887766, 59.53359981990485750 ) ) ;
#64685 = CARTESIAN_POINT ( 'NONE',  ( 12.50000000000000355, 41.59226156894002457, -76.70843802411151557 ) ) ;
#64686 = CARTESIAN_POINT ( 'NONE',  ( -111.0360493097450529, -57.67057850706027722, 194.0974529949267549 ) ) ;
#64687 = LINE ( 'NONE', #38829, #24976 ) ;
#64688 = LINE ( 'NONE', #13991, #54774 ) ;
#64689 = DIRECTION ( 'NONE',  ( 0.000000000000000000, 0.000000000000000000, -1.000000000000000000 ) ) ;
#64690 = FACE_BOUND ( 'NONE', #14873, .T. ) ;
#64691 = CARTESIAN_POINT ( 'NONE',  ( -2.851760031137707596, -60.00000000000000000, -45.00000000000002132 ) ) ;
#64692 = EDGE_CURVE ( 'NONE', #60457, #105650, #75020, .T. ) ;
#64693 = CARTESIAN_POINT ( 'NONE',  ( -37.63111671575072137, -14.21045842199439235, 41.24562198507008759 ) ) ;
#64694 = EDGE_CURVE ( 'NONE', #45219, #231, #34294, .T. ) ;
#64695 = CARTESIAN_POINT ( 'NONE',  ( -53.60733004976390248, -46.44083241526271166, 60.07166913633320604 ) ) ;
#64696 = ORIENTED_EDGE ( 'NONE', *, *, #20483, .F. ) ;
#64697 = CARTESIAN_POINT ( 'NONE',  ( -95.90005584971282815, -45.25350020261503659, 194.1417000045240968 ) ) ;
#64698 = LINE ( 'NONE', #32355, #54660 ) ;
#64699 = EDGE_LOOP ( 'NONE', ( #14221, #2106, #87369, #60092, #59242, #86750 ) ) ;
#64700 = CARTESIAN_POINT ( 'NONE',  ( -18.00634752349238710, 34.31709907050714037, -23.17894427062218554 ) ) ;
#64701 = CARTESIAN_POINT ( 'NONE',  ( 91.13477408414057379, -38.40443913744169890, -11.79364926309030892 ) ) ;
#64702 = CARTESIAN_POINT ( 'NONE',  ( 49.13563689125552258, 12.95301730162418252, 16.19018188726472474 ) ) ;
#64703 = CARTESIAN_POINT ( 'NONE',  ( 5.082755093536325930, -10.34375000204838457, -5.082755093536325042 ) ) ;
#64705 = EDGE_CURVE ( 'NONE', #59024, #77351, #16451, .T. ) ;
#64704 = CARTESIAN_POINT ( 'NONE',  ( -8.363902830498242125, 294.6905147064353514, 1.902776017109438556 ) ) ;
#64706 =( GEOMETRIC_REPRESENTATION_CONTEXT ( 3 ) GLOBAL_UNCERTAINTY_ASSIGNED_CONTEXT ( ( #43749 ) ) GLOBAL_UNIT_ASSIGNED_CONTEXT ( ( #50172, #35628, #100313 ) ) REPRESENTATION_CONTEXT ( 'NONE', 'WORKASPACE' ) );
#64707 = CARTESIAN_POINT ( 'NONE',  ( 22.33349330513380337, 4.000000000000002665, 0.000000000000000000 ) ) ;
#64708 = CARTESIAN_POINT ( 'NONE',  ( 80.75155016999305246, -30.00000000000000711, 138.6041971985428631 ) ) ;
#64709 = FACE_OUTER_BOUND ( 'NONE', #24347, .T. ) ;
#64710 = CARTESIAN_POINT ( 'NONE',  ( 35.58515402554368023, 490.6697164559536191, 12.32566724388707513 ) ) ;
#64711 = CARTESIAN_POINT ( 'NONE',  ( -36.01602535166301067, 463.8907346520921351, 20.04892332327189308 ) ) ;
#64712 =( LENGTH_UNIT ( ) NAMED_UNIT ( * ) SI_UNIT ( .MILLI., .METRE. ) );
#64713 = ORIENTED_EDGE ( 'NONE', *, *, #63608, .F. ) ;
#64714 = EDGE_LOOP ( 'NONE', ( #14491, #53386, #7226, #90119 ) ) ;
#64715 = CARTESIAN_POINT ( 'NONE',  ( 50.24668090215569549, -60.29526498424313985, 58.32267405694980056 ) ) ;
#64716 = CARTESIAN_POINT ( 'NONE',  ( 5.402795611188940583, 41.73472188612398526, -58.79867419242892623 ) ) ;
#64717 = CARTESIAN_POINT ( 'NONE',  ( 9.735511751164029448, 51.35490659063075469, 2.349585191579547150 ) ) ;
#64718 = EDGE_LOOP ( 'NONE', ( #86226, #7279, #102820, #17241, #73192 ) ) ;
#64719 = CARTESIAN_POINT ( 'NONE',  ( -109.9674670641295080, -38.35608556422234727, 186.0885245604343083 ) ) ;
#64720 = EDGE_LOOP ( 'NONE', ( #38862, #81939, #40801, #4077, #84065 ) ) ;
#64721 = DIRECTION ( 'NONE',  ( -1.000000000000000000, -0.000000000000000000, -0.000000000000000000 ) ) ;
#64722 = CARTESIAN_POINT ( 'NONE',  ( 98.21170614753282280, -38.35583079657099859, 77.88820735297903752 ) ) ;
#64723 = CARTESIAN_POINT ( 'NONE',  ( 11.88624655040385214, 16.70885896114117486, -9.290919399962746184 ) ) ;
#64724 = CARTESIAN_POINT ( 'NONE',  ( -5.787480046464959393, 41.99999999999999289, -68.91429205815936143 ) ) ;
#64725 = DIRECTION ( 'NONE',  ( -1.000000000000000000, -0.000000000000000000, -0.000000000000000000 ) ) ;
#64726 = CARTESIAN_POINT ( 'NONE',  ( 97.17576315571548662, -37.84846074978354835, 120.9268184589083717 ) ) ;
#64727 = LINE ( 'NONE', #6472, #102728 ) ;
#64728 = FILL_AREA_STYLE_COLOUR ( '', #49811 ) ;
#64729 = CARTESIAN_POINT ( 'NONE',  ( -34.77877198785877511, 338.7120930708800302, -1.786898488397636875 ) ) ;
#64730 =( NAMED_UNIT ( * ) PLANE_ANGLE_UNIT ( ) SI_UNIT ( $, .RADIAN. ) );
#64731 = CARTESIAN_POINT ( 'NONE',  ( 77.93163905888464171, -59.99999999999997868, 192.6887321471520238 ) ) ;
#64732 = COLOUR_RGB ( '', 0.72549020, 0.75294118, 0.79215686) ;
#64733 = VERTEX_POINT ( 'NONE', #78428 ) ;
#64734 = CARTESIAN_POINT ( 'NONE',  ( 56.75702308777373162, -36.02330638279852337, 62.71544796725239479 ) ) ;
#64735 = CARTESIAN_POINT ( 'NONE',  ( -26.71843530640310505, 304.8394554359867925, -9.563866172168349777 ) ) ;
#64736 = CARTESIAN_POINT ( 'NONE',  ( 9.728434877168217199, -50.82153073783059227, 24.67462639010848946 ) ) ;
#64737 = CIRCLE ( 'NONE', #81874, 2.000000000000003553 ) ;
#64738 = CARTESIAN_POINT ( 'NONE',  ( -7.503613543180902568, -5.000000000000000888, -15.58785114095667623 ) ) ;
#64739 = VERTEX_POINT ( 'NONE', #29395 ) ;
#64741 = DIRECTION ( 'NONE',  ( 0.000000000000000000, 0.000000000000000000, 1.000000000000000000 ) ) ;
#64740 = CARTESIAN_POINT ( 'NONE',  ( -91.08926842279480240, -38.40455573169174386, -12.07822636003188954 ) ) ;
#64742 = CARTESIAN_POINT ( 'NONE',  ( 1.047197551196598519, -2.999999999999999556, -7.999999999999998224 ) ) ;
#64743 = CARTESIAN_POINT ( 'NONE',  ( 24.36647833307484490, 306.6270560823984397, 9.333673104374161866 ) ) ;
#64744 = CARTESIAN_POINT ( 'NONE',  ( 88.20199406385988539, -5.000000000000000888, 6.123233995736779101E-16 ) ) ;
#64745 = CARTESIAN_POINT ( 'NONE',  ( -5.656854249492381470, -34.06249999999999289, 5.656854249492379694 ) ) ;
#64746 = CIRCLE ( 'NONE', #57791, 4.000000000000001776 ) ;
#64747 = FACE_BOUND ( 'NONE', #91805, .T. ) ;
#64748 = ADVANCED_FACE ( 'NONE', ( #53105 ), #19967, .T. ) ;
#64749 = STYLED_ITEM ( 'NONE', ( #64551 ), #88323 ) ;
#64750 = CONICAL_SURFACE ( 'NONE', #83676, 22.55262289886175964, 1.221730476396026388 ) ;
#64751 = AXIS2_PLACEMENT_3D ( 'NONE', #26656, #61674, #43337 ) ;
#64752 = DIRECTION ( 'NONE',  ( 0.000000000000000000, -1.000000000000000000, 0.000000000000000000 ) ) ;
#64753 = ORIENTED_EDGE ( 'NONE', *, *, #59267, .F. ) ;
#64754 = CARTESIAN_POINT ( 'NONE',  ( 81.78911868813072772, -53.49039721618134280, 179.9874179505537768 ) ) ;
#64755 = DIRECTION ( 'NONE',  ( 0.000000000000000000, 1.000000000000000000, 0.000000000000000000 ) ) ;
#64756 = CARTESIAN_POINT ( 'NONE',  ( -33.59588613957706116, 439.5203103051574089, 23.94499399079802160 ) ) ;
#64757 = ORIENTED_EDGE ( 'NONE', *, *, #4076, .T. ) ;
#64758 = CARTESIAN_POINT ( 'NONE',  ( 5.073014709119004984, -4.333232302192993934, -17.09748285339890117 ) ) ;
#64759 = DIRECTION ( 'NONE',  ( -1.000000000000000000, 0.000000000000000000, 0.000000000000000000 ) ) ;
#64760 = CARTESIAN_POINT ( 'NONE',  ( -14.11571568429346968, 5.211159435664322714, -3.514002131771437831 ) ) ;
#64761 = CARTESIAN_POINT ( 'NONE',  ( -39.97406772777365802, 41.90729804012168103, -55.54474264065575539 ) ) ;
#64762 = AXIS2_PLACEMENT_3D ( 'NONE', #104036, #45298, #30176 ) ;
#64763 = CARTESIAN_POINT ( 'NONE',  ( -28.79633237789201772, 10.21664471455435397, -41.74470786255343313 ) ) ;
#64764 = ORIENTED_EDGE ( 'NONE', *, *, #49313, .F. ) ;
#64765 = AXIS2_PLACEMENT_3D ( 'NONE', #43401, #42861, #18615 ) ;
#64766 = CARTESIAN_POINT ( 'NONE',  ( 7.002990960197232440, 106.0526681838345837, 3.868040364119523566 ) ) ;
#64767 = CARTESIAN_POINT ( 'NONE',  ( -3.857142857142847880, -48.79941684889506348, 103.1763305333244318 ) ) ;
#64769 = CARTESIAN_POINT ( 'NONE',  ( -12.45589307813304814, 7.205894838730145580, -8.168563394729352112 ) ) ;
#64768 = CARTESIAN_POINT ( 'NONE',  ( -21.98111356096458024, -27.00318221690102050, 37.33131516330131205 ) ) ;
#64770 = CARTESIAN_POINT ( 'NONE',  ( -5.082755093536326818, -12.21875000204838635, 5.082755093536325042 ) ) ;
#64771 = CARTESIAN_POINT ( 'NONE',  ( -62.59524157938066224, 40.83906611472970383, 18.50207713795375142 ) ) ;
#64772 = EDGE_CURVE ( 'NONE', #45464, #69452, #46080, .T. ) ;
#64773 = EDGE_CURVE ( 'NONE', #87776, #4091, #35900, .T. ) ;
#64774 = ORIENTED_EDGE ( 'NONE', *, *, #59486, .T. ) ;
#64775 = DIRECTION ( 'NONE',  ( -0.000000000000000000, -1.000000000000000000, -0.000000000000000000 ) ) ;
#64776 = DIRECTION ( 'NONE',  ( -0.9230641662213927567, 0.000000000000000000, 0.3846459996386352720 ) ) ;
#64777 = CIRCLE ( 'NONE', #85503, 4.172000000000009479 ) ;
#64778 = CARTESIAN_POINT ( 'NONE',  ( -4.557400256674738692, 143.1997842995386634, -5.000000000000000000 ) ) ;
#64779 = CARTESIAN_POINT ( 'NONE',  ( 14.54015256618498242, 142.2617268803927288, 5.000000000000000000 ) ) ;
#64780 = CARTESIAN_POINT ( 'NONE',  ( -14.11595029531375900, 2.410436752333459776, 5.024000119300219502 ) ) ;
#64781 = ORIENTED_EDGE ( 'NONE', *, *, #83797, .T. ) ;
#64782 = CARTESIAN_POINT ( 'NONE',  ( 0.000000000000000000, -1.000000000000000000, 0.000000000000000000 ) ) ;
#64783 = PLANE ( 'NONE',  #15118 ) ;
#64784 = EDGE_LOOP ( 'NONE', ( #40972, #78721, #30248, #31262 ) ) ;
#64785 = LINE ( 'NONE', #47528, #36926 ) ;
#64786 = FILL_AREA_STYLE_COLOUR ( '', #43369 ) ;
#64787 = CARTESIAN_POINT ( 'NONE',  ( 25.53945892759312031, -5.000000000000000000, 0.000000000000000000 ) ) ;
#64788 = CARTESIAN_POINT ( 'NONE',  ( -109.1115345680586586, -60.00000000000000711, 136.7728363596365568 ) ) ;
#64789 = CARTESIAN_POINT ( 'NONE',  ( 0.000000000000000000, 0.000000000000000000, 0.000000000000000000 ) ) ;
#64790 = CARTESIAN_POINT ( 'NONE',  ( 4.699999999999999289, -3.752776749732578132, -6.500000000000000888 ) ) ;
#64791 = CARTESIAN_POINT ( 'NONE',  ( 16.75187969033571989, 34.99134772383131065, 21.80698433968582961 ) ) ;
#64793 = CARTESIAN_POINT ( 'NONE',  ( 37.83989825151499531, 491.6297408768496098, 12.44743998625077630 ) ) ;
#64792 = CARTESIAN_POINT ( 'NONE',  ( -9.596002107492989097, -5.000000000000002665, -77.62543935900905012 ) ) ;
#64794 = CARTESIAN_POINT ( 'NONE',  ( -81.43653422135359676, -57.01209690326547985, 181.8861859459519792 ) ) ;
#64795 = AXIS2_PLACEMENT_3D ( 'NONE', #13135, #54651, #14729 ) ;
#64796 = ORIENTED_EDGE ( 'NONE', *, *, #85983, .T. ) ;
#64797 = ORIENTED_EDGE ( 'NONE', *, *, #13287, .F. ) ;
#64798 = VERTEX_POINT ( 'NONE', #53626 ) ;
#64799 = LINE ( 'NONE', #106300, #99141 ) ;
#64801 = CARTESIAN_POINT ( 'NONE',  ( 16.08349330513380337, 4.898587196589411843E-16, -4.000000000000001776 ) ) ;
#64800 = PRESENTATION_LAYER_ASSIGNMENT (  '', '', ( #51005 ) ) ;
#64802 = B_SPLINE_CURVE_WITH_KNOTS ( 'NONE', 3,
 ( #4805, #45794, #13405, #60408 ),
 .UNSPECIFIED., .F., .F.,
 ( 4, 4 ),
 ( 0.000000000000000000, 0.001833966606958285740 ),
 .UNSPECIFIED. ) ;
#64803 = DIRECTION ( 'NONE',  ( 0.000000000000000000, 0.000000000000000000, -1.000000000000000000 ) ) ;
#64804 =( LENGTH_UNIT ( ) NAMED_UNIT ( * ) SI_UNIT ( .MILLI., .METRE. ) );
#64805 = AXIS2_PLACEMENT_3D ( 'NONE', #100997, #18515, #103134 ) ;
#64806 = CARTESIAN_POINT ( 'NONE',  ( 9.518114778801557208, 9.451441023734561853, -4.999999999999691802 ) ) ;
#64807 = DIRECTION ( 'NONE',  ( 0.000000000000000000, 1.000000000000000000, 0.000000000000000000 ) ) ;
#64808 = DIRECTION ( 'NONE',  ( 0.000000000000000000, 1.000000000000000000, 0.000000000000000000 ) ) ;
#64809 = CARTESIAN_POINT ( 'NONE',  ( 113.7193001496157052, -60.00000000000001421, 185.6034734595149871 ) ) ;
#64810 = CARTESIAN_POINT ( 'NONE',  ( -112.2649012439172793, -59.99999999999995026, 191.8495178741738130 ) ) ;
#64811 = CARTESIAN_POINT ( 'NONE',  ( -63.22578340066489488, -36.00976971212025290, 79.28688979505365353 ) ) ;
#64812 = VECTOR ( 'NONE', #83535, 1000.000000000000114 ) ;
#64813 = ORIENTED_EDGE ( 'NONE', *, *, #79841, .F. ) ;
#64814 = AXIS2_PLACEMENT_3D ( 'NONE', #36901, #102662, #103197 ) ;
#64815 = CARTESIAN_POINT ( 'NONE',  ( -43.68875470849008025, 484.4240665651603877, 2.019269197006389849 ) ) ;
#64816 = CARTESIAN_POINT ( 'NONE',  ( 114.0273069743737295, -59.99999999998534861, 183.4122421493096908 ) ) ;
#64817 = PRESENTATION_LAYER_ASSIGNMENT (  '', '', ( #75114 ) ) ;
#64819 = ORIENTED_EDGE ( 'NONE', *, *, #10824, .T. ) ;
#64818 = AXIS2_PLACEMENT_3D ( 'NONE', #90506, #73779, #106680 ) ;
#64820 = CARTESIAN_POINT ( 'NONE',  ( 0.9878741920119958886, -22.06731700408509766, 27.56753612694989997 ) ) ;
#64822 = COLOUR_RGB ( '', 0.66274510, 0.83137255, 0.94901961) ;
#64821 = CARTESIAN_POINT ( 'NONE',  ( -2.977408999572654480, -14.00000000204838457, 7.188101187499999156 ) ) ;
#64823 = CARTESIAN_POINT ( 'NONE',  ( 0.000000000000000000, 80.00000000000000000, -8.000000000000010658 ) ) ;
#64824 = ORIENTED_EDGE ( 'NONE', *, *, #99623, .F. ) ;
#64825 = CARTESIAN_POINT ( 'NONE',  ( 35.81083583144190641, 464.1171150618853289, 19.43519701782722464 ) ) ;
#64826 = VERTEX_POINT ( 'NONE', #69305 ) ;
#64827 = DIRECTION ( 'NONE',  ( 0.000000000000000000, 0.000000000000000000, 1.000000000000000000 ) ) ;
#64828 = CARTESIAN_POINT ( 'NONE',  ( 2.977408999572652260, -28.81250000204838813, 7.188101187500000044 ) ) ;
#64829 = CARTESIAN_POINT ( 'NONE',  ( -105.7231067272802107, -60.00000000000002132, 198.5820885245993850 ) ) ;
#64830 = CARTESIAN_POINT ( 'NONE',  ( 9.960739174314243272, -57.87150899010582350, 26.07695415532590033 ) ) ;
#64831 = CARTESIAN_POINT ( 'NONE',  ( 7.188101187500000044, -27.03125000204838813, 0.000000000000000000 ) ) ;
#64832 = CARTESIAN_POINT ( 'NONE',  ( 45.99999999999995737, 463.3824904069770128, 8.976947363133223945 ) ) ;
#64833 = EDGE_CURVE ( 'NONE', #81655, #88824, #96456, .T. ) ;
#64834 = CARTESIAN_POINT ( 'NONE',  ( -13.97088187905699108, 20.79957665017152735, 6.270615721353047789 ) ) ;
#64835 = CARTESIAN_POINT ( 'NONE',  ( 5.000000000000000000, -30.70749484266840312, -0.3356907877405980178 ) ) ;
#64836 = EDGE_CURVE ( 'NONE', #63571, #87282, #66412, .T. ) ;
#64837 = CARTESIAN_POINT ( 'NONE',  ( 15.82312105870659025, -3.732472542269488880, 14.54008594198294801 ) ) ;
#64838 = CARTESIAN_POINT ( 'NONE',  ( -42.97908324528840751, 343.6987997973317874, 9.561931291602665084 ) ) ;
#64839 = CARTESIAN_POINT ( 'NONE',  ( 97.75542164735125539, -59.99999999999992895, 196.5577905707872617 ) ) ;
#64840 = CARTESIAN_POINT ( 'NONE',  ( -33.08517237052004134, -32.56037428575159964, 33.08091690792520012 ) ) ;
#64841 = CARTESIAN_POINT ( 'NONE',  ( 38.62684451199579172, -49.88772538349552832, 39.81651187074815823 ) ) ;
#64842 = FACE_OUTER_BOUND ( 'NONE', #58718, .T. ) ;
#64843 = ORIENTED_EDGE ( 'NONE', *, *, #47428, .T. ) ;
#64844 = CARTESIAN_POINT ( 'NONE',  ( 34.16642289233133312, 463.8422268500519294, 18.98106911353331938 ) ) ;
#64845 = CARTESIAN_POINT ( 'NONE',  ( -58.12203222560709293, -38.34410314818605769, 90.61017755120225559 ) ) ;
#64846 = VERTEX_POINT ( 'NONE', #52557 ) ;
#64848 = CARTESIAN_POINT ( 'NONE',  ( -22.91885868373643831, 305.6172567281201964, 10.10309701371861912 ) ) ;
#64847 = CARTESIAN_POINT ( 'NONE',  ( 4.142849616820252293E-15, 0.000000000000000000, -33.82893434829263413 ) ) ;
#64849 = CARTESIAN_POINT ( 'NONE',  ( 0.000000000000000000, 0.000000000000000000, 0.000000000000000000 ) ) ;
#64850 = CARTESIAN_POINT ( 'NONE',  ( 0.000000000000000000, 3.999999999999996447, 0.000000000000000000 ) ) ;
#64851 = CARTESIAN_POINT ( 'NONE',  ( 0.3379670387979981649, 44.07169264148151910, -16.28508512065656788 ) ) ;
#64852 = CARTESIAN_POINT ( 'NONE',  ( -38.10433946279282935, 437.2340514686374604, 4.662695304592548773 ) ) ;
#64853 = CARTESIAN_POINT ( 'NONE',  ( -31.39953160533619325, 423.6490974968072010, 23.88548958732392435 ) ) ;
#64854 = DIRECTION ( 'NONE',  ( -1.000000000000000000, -0.000000000000000000, -0.000000000000000000 ) ) ;
#64855 = CARTESIAN_POINT ( 'NONE',  ( 100.5416370945685287, -59.99999999999999289, 84.20779271781832165 ) ) ;
#64856 = CARTESIAN_POINT ( 'NONE',  ( -29.68315524076989576, 13.12249633091057177, 39.60535821593503414 ) ) ;
#64857 = DIRECTION ( 'NONE',  ( 0.000000000000000000, 0.000000000000000000, -1.000000000000000000 ) ) ;
#64858 = DIRECTION ( 'NONE',  ( 0.000000000000000000, -1.000000000000000000, 0.000000000000000000 ) ) ;
#64859 = VERTEX_POINT ( 'NONE', #21300 ) ;
#64860 = CARTESIAN_POINT ( 'NONE',  ( -89.28949256530911782, -29.99999999994691890, 17.42366683985877884 ) ) ;
#64861 = ORIENTED_EDGE ( 'NONE', *, *, #52200, .T. ) ;
#64862 = CARTESIAN_POINT ( 'NONE',  ( 7.922281120364393914, 4.573931137438267847, -8.047472243342932430 ) ) ;
#64863 = CARTESIAN_POINT ( 'NONE',  ( -16.01731991114684206, 3.900112512633671980, -1.615757124594061400 ) ) ;
#64864 = SURFACE_SIDE_STYLE ('',( #23914 ) ) ;
#64865 = CARTESIAN_POINT ( 'NONE',  ( 0.000000000000000000, 70.00000000000000000, 0.000000000000000000 ) ) ;
#64866 = CARTESIAN_POINT ( 'NONE',  ( 9.842473135306407883, 26.41068182886412785, 1.785129593756274113 ) ) ;
#64867 = CARTESIAN_POINT ( 'NONE',  ( 7.188101187500001821, -26.93750000204838457, -2.977408999572650483 ) ) ;
#64868 = CARTESIAN_POINT ( 'NONE',  ( -10.00000000000000000, -15.00000000000000000, 10.00000000000000178 ) ) ;
#64869 = CARTESIAN_POINT ( 'NONE',  ( 7.226138801442005821, 41.34018720343522801, -70.07054281437619636 ) ) ;
#64870 = ORIENTED_EDGE ( 'NONE', *, *, #36887, .T. ) ;
#64871 = EDGE_CURVE ( 'NONE', #1846, #9249, #85480, .T. ) ;
#64873 = ORIENTED_EDGE ( 'NONE', *, *, #48432, .F. ) ;
#64872 = DIRECTION ( 'NONE',  ( 1.000000000000000000, 1.224606353822377258E-16, 0.000000000000000000 ) ) ;
#64874 = CARTESIAN_POINT ( 'NONE',  ( 84.18868867901204567, -18.67344423748746252, 149.2193650899454553 ) ) ;
#64875 = CARTESIAN_POINT ( 'NONE',  ( -10.00000000000000178, 15.00000000000000000, -4.582575694955834500 ) ) ;
#64876 = AXIS2_PLACEMENT_3D ( 'NONE', #9398, #59586, #42315 ) ;
#64877 = CARTESIAN_POINT ( 'NONE',  ( -37.56673239365863282, 27.60449318992554879, -13.45617127781024891 ) ) ;
#64878 = ORIENTED_EDGE ( 'NONE', *, *, #44650, .F. ) ;
#64879 = CARTESIAN_POINT ( 'NONE',  ( -46.29054874100096129, 50.00000000000002842, 42.75167762495752299 ) ) ;
#64880 = CARTESIAN_POINT ( 'NONE',  ( 7.003653396366579464, -86.05706205559677358, -3.866846144092870308 ) ) ;
#64881 = CARTESIAN_POINT ( 'NONE',  ( -7.188101187500000044, -13.90625000204838457, -8.802885111219163269E-16 ) ) ;
#64882 = CARTESIAN_POINT ( 'NONE',  ( 20.77592568779148863, 3.851859888774471706E-31, 5.000000000000001776 ) ) ;
#64883 = CARTESIAN_POINT ( 'NONE',  ( -44.89949488402420030, -57.68324447995585302, 64.92693994880102082 ) ) ;
#64884 = CARTESIAN_POINT ( 'NONE',  ( 8.763303353751069835, 294.6787833753287487, 1.900260937711448328 ) ) ;
#64885 = EDGE_CURVE ( 'NONE', #72268, #91201, #78962, .T. ) ;
#64886 = ADVANCED_FACE ( 'NONE', ( #77379 ), #82637, .F. ) ;
#64887 = ORIENTED_EDGE ( 'NONE', *, *, #32270, .T. ) ;
#64888 = CYLINDRICAL_SURFACE ( 'NONE', #70041, 1.250000000000001110 ) ;
#64889 = VECTOR ( 'NONE', #3524, 1000.000000000000000 ) ;
#64890 = CARTESIAN_POINT ( 'NONE',  ( 0.000000000000000000, 38.19193163660327173, 0.000000000000000000 ) ) ;
#64891 = CARTESIAN_POINT ( 'NONE',  ( -3.313708498984726969, -18.96874999999998934, 8.000000000000039080 ) ) ;
#64892 =( LENGTH_UNIT ( ) NAMED_UNIT ( * ) SI_UNIT ( .MILLI., .METRE. ) );
#64893 = ORIENTED_EDGE ( 'NONE', *, *, #91059, .T. ) ;
#64894 = CARTESIAN_POINT ( 'NONE',  ( -2.977408999572654480, -30.12500000204838813, 7.188101187499999156 ) ) ;
#64895 = AXIS2_PLACEMENT_3D ( 'NONE', #2898, #84372, #9385 ) ;
#64896 = CARTESIAN_POINT ( 'NONE',  ( -21.78783193603920765, -17.85986078249778330, 31.47006901580117599 ) ) ;
#64897 = AXIS2_PLACEMENT_3D ( 'NONE', #5230, #94244, #45171 ) ;
#64898 = SURFACE_STYLE_USAGE ( .BOTH. , #14736 ) ;
#64899 = PRESENTATION_LAYER_ASSIGNMENT (  '', '', ( #102791 ) ) ;
#64900 = AXIS2_PLACEMENT_3D ( 'NONE', #94955, #5900, #86338 ) ;
#64901 = CARTESIAN_POINT ( 'NONE',  ( 1.013110838965806781, 51.43236336151769450, -9.750292636990165462 ) ) ;
#64902 = EDGE_CURVE ( 'NONE', #66536, #24036, #59503, .T. ) ;
#64903 = CARTESIAN_POINT ( 'NONE',  ( -9.918010731619574472, 88.79151684843223791, -1.300854425901573519 ) ) ;
#64904 = CARTESIAN_POINT ( 'NONE',  ( 34.07726008484836200, 439.5806258003244693, 24.00265428230595433 ) ) ;
#64905 = SHAPE_DEFINITION_REPRESENTATION ( #85495, #62661 ) ;
#64906 = CARTESIAN_POINT ( 'NONE',  ( 49.28004588020311161, 7.871673175840917303, 15.62336800674797033 ) ) ;
#64907 = ORIENTED_EDGE ( 'NONE', *, *, #102859, .T. ) ;
#64909 = AXIS2_PLACEMENT_3D ( 'NONE', #83377, #9472, #76342 ) ;
#64908 = CARTESIAN_POINT ( 'NONE',  ( -7.000000000000000888, -46.00000000000000711, 39.12435565298213902 ) ) ;
#64910 = CARTESIAN_POINT ( 'NONE',  ( -4.165977904505308693, 15.00000000000000000, 9.090909090909091717 ) ) ;
#64911 = CARTESIAN_POINT ( 'NONE',  ( 68.45015997180047407, 6.975173280561618775E-15, 0.000000000000000000 ) ) ;
#64912 = CARTESIAN_POINT ( 'NONE',  ( -16.75187969033459012, 36.38380281757147827, 24.30698433969199357 ) ) ;
#64913 = CARTESIAN_POINT ( 'NONE',  ( -3.704240196697770049, -48.94878093480736680, 103.3230214382350596 ) ) ;
#64914 = EDGE_CURVE ( 'NONE', #76395, #35999, #15291, .T. ) ;
#64915 = LINE ( 'NONE', #58412, #87597 ) ;
#64916 = ORIENTED_EDGE ( 'NONE', *, *, #87900, .T. ) ;
#64917 = LINE ( 'NONE', #7724, #80627 ) ;
#64918 = CARTESIAN_POINT ( 'NONE',  ( 99.48231450907248075, -57.62624137959831216, 204.0649224731593279 ) ) ;
#64919 = ADVANCED_FACE ( 'NONE', ( #103772 ), #29910, .T. ) ;
#64920 = DIRECTION ( 'NONE',  ( -1.000000000000000000, -1.224606353822377258E-16, -0.000000000000000000 ) ) ;
#64921 = CARTESIAN_POINT ( 'NONE',  ( -8.879818925004332897, 51.45542084839959074, -4.000492447368358739 ) ) ;
#64922 = CARTESIAN_POINT ( 'NONE',  ( -6.076451815340398355, 53.39448025720301416, 8.267155348349421118 ) ) ;
#64923 = CARTESIAN_POINT ( 'NONE',  ( -74.75251265819703406, -60.00000000000001421, 179.3165659446441396 ) ) ;
#64924 = EDGE_CURVE ( 'NONE', #78785, #55889, #55989, .T. ) ;
#64925 = CARTESIAN_POINT ( 'NONE',  ( -40.88293604215247967, 432.5779639752643675, 26.56799667982232549 ) ) ;
#64926 = CARTESIAN_POINT ( 'NONE',  ( -43.29658055318886767, 324.1952503670673877, -2.852919881210743913 ) ) ;
#64927 = AXIS2_PLACEMENT_3D ( 'NONE', #18008, #58993, #99967 ) ;
#64928 = CARTESIAN_POINT ( 'NONE',  ( -84.69605050066350316, -46.57368461021737716, 186.7912660905877260 ) ) ;
#64930 = EDGE_CURVE ( 'NONE', #68266, #104924, #38532, .T. ) ;
#64929 = ORIENTED_EDGE ( 'NONE', *, *, #11170, .F. ) ;
#64931 = CARTESIAN_POINT ( 'NONE',  ( 27.07237153509079874, 306.2907637360925719, -9.460208576581653261 ) ) ;
#64932 = ORIENTED_EDGE ( 'NONE', *, *, #50449, .F. ) ;
#64933 = CARTESIAN_POINT ( 'NONE',  ( -7.934883677559678716, -13.86839177937552314, 1.051380792122691643 ) ) ;
#64934 = CARTESIAN_POINT ( 'NONE',  ( -5.371950044183565254, -2.205168805904307305, 104.0625755208173473 ) ) ;
#64935 = CARTESIAN_POINT ( 'NONE',  ( -83.19139743512374707, -37.80357306262363437, -4.125305165967327881 ) ) ;
#64936 = CARTESIAN_POINT ( 'NONE',  ( 6.289692432696784685, -1.240516797660047330E-13, -6.828989928337167115 ) ) ;
#64937 = VERTEX_POINT ( 'NONE', #88133 ) ;
#64938 = CARTESIAN_POINT ( 'NONE',  ( -42.23079339798738374, 460.7352525929354101, 2.726051457480726636 ) ) ;
#64939 = CARTESIAN_POINT ( 'NONE',  ( 13.28963858130279441, 24.22795872967301634, -3.151957778078536609 ) ) ;
#64940 = CARTESIAN_POINT ( 'NONE',  ( 13.66642973270348627, -9.677049996499534265E-13, 17.78317311657527000 ) ) ;
#64941 = CARTESIAN_POINT ( 'NONE',  ( 0.000000000000000000, 69.00000000000000000, -5.999999999999994671 ) ) ;
#64942 = CARTESIAN_POINT ( 'NONE',  ( -64.67113474307254251, -14.21045842199435505, -28.81208810413780697 ) ) ;
#64943 = CARTESIAN_POINT ( 'NONE',  ( -76.18563976863433140, -60.31830717657551588, 143.7070035543199822 ) ) ;
#64944 = EDGE_LOOP ( 'NONE', ( #49172, #9246, #69457, #10451, #99766 ) ) ;
#64945 = CARTESIAN_POINT ( 'NONE',  ( 42.10926113833883022, -14.21045842199418452, 45.52176705710515847 ) ) ;
#64946 = CARTESIAN_POINT ( 'NONE',  ( 7.045755811259135193, 86.30341603013555130, 3.790843699961853552 ) ) ;
#64947 = CARTESIAN_POINT ( 'NONE',  ( 112.6079886463091100, -57.67117955158271059, 189.1529986196025561 ) ) ;
#64948 = DIRECTION ( 'NONE',  ( 0.000000000000000000, 0.9795142562459571156, -0.2013748291394176493 ) ) ;
#64949 = CIRCLE ( 'NONE', #21943, 5.000000000000011546 ) ;
#64950 = FACE_BOUND ( 'NONE', #72751, .T. ) ;
#64951 = ORIENTED_EDGE ( 'NONE', *, *, #82873, .T. ) ;
#64952 = FACE_OUTER_BOUND ( 'NONE', #19270, .T. ) ;
#64953 = DIRECTION ( 'NONE',  ( 0.5735764363510470476, -0.8191520442889911324, 1.003171929053524007E-16 ) ) ;
#64954 = CYLINDRICAL_SURFACE ( 'NONE', #13894, 5.000000000000000888 ) ;
#64955 = CARTESIAN_POINT ( 'NONE',  ( -7.188101187500002709, -19.81250000204838813, 2.977408999572648707 ) ) ;
#64956 = CARTESIAN_POINT ( 'NONE',  ( 5.299999999999999822, -3.752776749732578132, -6.500000000000000888 ) ) ;
#64957 = CARTESIAN_POINT ( 'NONE',  ( 9.797537890442933772, 81.53442202333808098, 2.014215961808879296 ) ) ;
#64958 = PRESENTATION_STYLE_ASSIGNMENT (( #8837 ) ) ;
#64959 = EDGE_CURVE ( 'NONE', #69907, #64079, #21649, .T. ) ;
#64960 = CARTESIAN_POINT ( 'NONE',  ( 3.400000000000000355, 0.000000000000000000, -6.123524522925831270 ) ) ;
#64961 = CARTESIAN_POINT ( 'NONE',  ( -8.000000000000000000, -13.43750000409676915, -9.797174393178825657E-16 ) ) ;
#64962 = ORIENTED_EDGE ( 'NONE', *, *, #12047, .F. ) ;
#64963 = CARTESIAN_POINT ( 'NONE',  ( -6.890281280090281513, 41.03680257558234246, -70.85895802555796763 ) ) ;
#64964 = AXIS2_PLACEMENT_3D ( 'NONE', #105907, #56282, #97824 ) ;
#64966 = CARTESIAN_POINT ( 'NONE',  ( 30.06199366251785676, -32.53957342301957567, 31.90491467160951800 ) ) ;
#64965 = DIRECTION ( 'NONE',  ( -0.1946996363145598874, 0.08778327892740174498, 0.9769268895673475228 ) ) ;
#64967 = CARTESIAN_POINT ( 'NONE',  ( 0.000000000000000000, -15.00000000000000000, 0.000000000000000000 ) ) ;
#64968 = EDGE_CURVE ( 'NONE', #50361, #93305, #83622, .T. ) ;
#64969 = ORIENTED_EDGE ( 'NONE', *, *, #82052, .F. ) ;
#64970 = EDGE_LOOP ( 'NONE', ( #105059, #10037, #801, #106519 ) ) ;
#64972 = PLANE ( 'NONE',  #6137 ) ;
#64971 = FILL_AREA_STYLE ('',( #32093 ) ) ;
#64973 = AXIS2_PLACEMENT_3D ( 'NONE', #92367, #58964, #2284 ) ;
#64974 = DIRECTION ( 'NONE',  ( 0.000000000000000000, 0.000000000000000000, 1.000000000000000000 ) ) ;
#64975 = CARTESIAN_POINT ( 'NONE',  ( -16.40059842617682051, 294.5680859342442659, -10.06030655347179703 ) ) ;
#64976 = AXIS2_PLACEMENT_3D ( 'NONE', #13334, #12283, #78087 ) ;
#64977 = CARTESIAN_POINT ( 'NONE',  ( 6.917892303299533197, 41.82074860089118573, -68.91429206365098992 ) ) ;
#64978 = DIRECTION ( 'NONE',  ( -1.000000000000000000, -0.000000000000000000, -0.000000000000000000 ) ) ;
#64979 = DIRECTION ( 'NONE',  ( 0.000000000000000000, 1.000000000000000000, 0.000000000000000000 ) ) ;
#64980 = VERTEX_POINT ( 'NONE', #100454 ) ;
#64981 = CARTESIAN_POINT ( 'NONE',  ( 49.18716589317016741, -60.00000000000000000, -38.06278613323081572 ) ) ;
#64982 = DIRECTION ( 'NONE',  ( 1.000000000000000000, 0.000000000000000000, 0.000000000000000000 ) ) ;
#64983 = CARTESIAN_POINT ( 'NONE',  ( -15.26755105656414990, -0.4567640699404665883, 14.99506816343297011 ) ) ;
#64984 = CARTESIAN_POINT ( 'NONE',  ( 37.56673239365841255, -1.200000000000000030E-05, -13.45617127781092215 ) ) ;
#64985 = VECTOR ( 'NONE', #20286, 1000.000000000000000 ) ;
#64986 = CARTESIAN_POINT ( 'NONE',  ( 84.15356149169568312, 1.016364837396684119E-14, 0.000000000000000000 ) ) ;
#64987 = ORIENTED_EDGE ( 'NONE', *, *, #99945, .F. ) ;
#64988 = EDGE_CURVE ( 'NONE', #34125, #84498, #82679, .T. ) ;
#64989 = ORIENTED_EDGE ( 'NONE', *, *, #25141, .T. ) ;
#64990 = EDGE_LOOP ( 'NONE', ( #79124, #94276, #81694, #99393, #92866 ) ) ;
#64991 = SURFACE_STYLE_FILL_AREA ( #39146 ) ;
#64992 = CARTESIAN_POINT ( 'NONE',  ( 36.15879880962841497, 40.31104328174256324, -58.06769010848005053 ) ) ;
#64993 = CARTESIAN_POINT ( 'NONE',  ( 102.9313392694734688, -5.000000000000000000, 0.000000000000000000 ) ) ;
#64994 = CARTESIAN_POINT ( 'NONE',  ( 30.40486732246983337, 318.3402785233949430, 13.73959638705492026 ) ) ;
#64995 = CARTESIAN_POINT ( 'NONE',  ( -42.27245208472728422, 331.6484278788518623, 6.927277335194249375 ) ) ;
#64996 = LINE ( 'NONE', #14839, #98992 ) ;
#64997 = DIRECTION ( 'NONE',  ( 0.000000000000000000, 0.000000000000000000, -1.000000000000000000 ) ) ;
#64998 = DIRECTION ( 'NONE',  ( 0.000000000000000000, 1.000000000000000000, 0.000000000000000000 ) ) ;
#64999 = ORIENTED_EDGE ( 'NONE', *, *, #9570, .F. ) ;
#65000 = CARTESIAN_POINT ( 'NONE',  ( 30.92868852183930883, 8.704894651777095760, 40.98784967800731494 ) ) ;
#65001 = B_SPLINE_CURVE_WITH_KNOTS ( 'NONE', 3,
 ( #84257, #58384, #43268, #76151, #34143, #92869, #51874, #43791, #76686, #35745, #98824, #57832, #16875, #49755, #82661, #41668, #74557, #60535, #85323, #21679 ),
 .UNSPECIFIED., .F., .F.,
 ( 4, 2, 2, 2, 2, 2, 2, 2, 2, 4 ),
 ( 0.003104382421020200622, 0.003608261970678582845, 0.004112141520336965068, 0.004616021069995346858, 0.005119900619653729515, 0.005371840394482917808, 0.005623780169312107835, 0.006127659718970490492, 0.006631539268628873149, 0.007135418818287256673 ),
 .UNSPECIFIED. ) ;
#65002 = ORIENTED_EDGE ( 'NONE', *, *, #4373, .T. ) ;
#65003 = EDGE_CURVE ( 'NONE', #100861, #89689, #80945, .T. ) ;
#65004 = CIRCLE ( 'NONE', #73608, 15.00000000000001243 ) ;
#65005 = DIRECTION ( 'NONE',  ( -1.000000000000000000, 0.000000000000000000, 0.000000000000000000 ) ) ;
#65006 = SURFACE_SIDE_STYLE ('',( #42853 ) ) ;
#65007 = CIRCLE ( 'NONE', #9856, 0.9999999999999800160 ) ;
#65008 = CARTESIAN_POINT ( 'NONE',  ( -68.97173617594968675, -59.99999999999997868, 110.4809570121333877 ) ) ;
#65009 = CARTESIAN_POINT ( 'NONE',  ( 68.05421936547546125, -46.43370952207241942, 99.56240759577892163 ) ) ;
#65010 = VERTEX_POINT ( 'NONE', #75097 ) ;
#65011 = CARTESIAN_POINT ( 'NONE',  ( 17.50000000000002842, 49.71153760032640889, 63.93192698917948746 ) ) ;
#65012 = FACE_OUTER_BOUND ( 'NONE', #55136, .T. ) ;
#65013 = ADVANCED_FACE ( 'NONE', ( #8252 ), #130, .T. ) ;
#65014 = ADVANCED_FACE ( 'NONE', ( #75645 ), #71561, .T. ) ;
#65015 = ORIENTED_EDGE ( 'NONE', *, *, #48124, .T. ) ;
#65016 = SURFACE_STYLE_FILL_AREA ( #32138 ) ;
#65017 = CARTESIAN_POINT ( 'NONE',  ( 90.51111111111110574, -4.171999999999998820, 5.616230220889773285E-16 ) ) ;
#65018 = MECHANICAL_DESIGN_GEOMETRIC_PRESENTATION_REPRESENTATION (  '', ( #1230 ), #58151 ) ;
#65019 = CARTESIAN_POINT ( 'NONE',  ( -37.02702338563431539, 490.9575081778414187, 12.45591594067345120 ) ) ;
#65020 = CARTESIAN_POINT ( 'NONE',  ( 8.000000000000000000, -30.59375000409677270, -3.313708498984761608 ) ) ;
#65021 = LINE ( 'NONE', #31620, #31851 ) ;
#65022 = STYLED_ITEM ( 'NONE', ( #18107 ), #7550 ) ;
#65023 = CARTESIAN_POINT ( 'NONE',  ( -10.00988628808512182, 7.485880917377084387, 5.000000000000004441 ) ) ;
#65024 = DIRECTION ( 'NONE',  ( -1.000000000000000000, -0.000000000000000000, -0.000000000000000000 ) ) ;
#65025 = CARTESIAN_POINT ( 'NONE',  ( 19.70764564238366390, 304.7954121406192485, 9.925013215726748328 ) ) ;
#65026 = VERTEX_POINT ( 'NONE', #50302 ) ;
#65027 =( NAMED_UNIT ( * ) PLANE_ANGLE_UNIT ( ) SI_UNIT ( $, .RADIAN. ) );
#65028 = DIRECTION ( 'NONE',  ( 0.000000000000000000, 0.000000000000000000, 1.000000000000000000 ) ) ;
#65029 = CARTESIAN_POINT ( 'NONE',  ( 4.997114387724912454, -59.99999999999999289, 39.62950257011186039 ) ) ;
#65030 = CARTESIAN_POINT ( 'NONE',  ( -98.12941349166321459, -30.00000000000000000, 190.3859582420429888 ) ) ;
#65031 = EDGE_CURVE ( 'NONE', #17567, #1846, #21779, .T. ) ;
#65032 = AXIS2_PLACEMENT_3D ( 'NONE', #76870, #18130, #99545 ) ;
#65033 = CARTESIAN_POINT ( 'NONE',  ( -40.18077987341683865, 485.1789679560215518, -4.313737565909713467 ) ) ;
#65034 = MECHANICAL_DESIGN_GEOMETRIC_PRESENTATION_REPRESENTATION (  '', ( #46115 ), #11678 ) ;
#65035 = CARTESIAN_POINT ( 'NONE',  ( 35.33287217233590383, -57.69550832373160176, 49.48941122886714794 ) ) ;
#65037 = DIRECTION ( 'NONE',  ( 0.000000000000000000, -1.000000000000000000, 0.000000000000000000 ) ) ;
#65036 = CARTESIAN_POINT ( 'NONE',  ( 8.000000000000000000, -15.59375000409677270, -3.313708498984761164 ) ) ;
#65038 = ADVANCED_FACE ( 'NONE', ( #73509 ), #83572, .T. ) ;
#65039 = CARTESIAN_POINT ( 'NONE',  ( -39.85564080104247608, 459.8412824357644126, 1.882109076563900363 ) ) ;
#65040 = DIRECTION ( 'NONE',  ( -1.000000000000000000, -1.224606353822377258E-16, -0.000000000000000000 ) ) ;
#65041 = CARTESIAN_POINT ( 'NONE',  ( -46.00000000000000000, 438.3878896346935221, 16.22878885428545104 ) ) ;
#65042 = CARTESIAN_POINT ( 'NONE',  ( -12.15260666804171130, -59.99999999999999289, 39.69048265552311250 ) ) ;
#65043 = AXIS2_PLACEMENT_3D ( 'NONE', #88946, #12916, #5381 ) ;
#65044 = CONICAL_SURFACE ( 'NONE', #2993, 5.000000000000001776, 0.9599310885968803664 ) ;
#65045 = CARTESIAN_POINT ( 'NONE',  ( 30.11650669486618881, 0.000000000000000000, 4.000000000000000888 ) ) ;
#65046 = CARTESIAN_POINT ( 'NONE',  ( 1.012109584170803878, 45.47521634855998229, -18.25170135021002338 ) ) ;
#65047 = CARTESIAN_POINT ( 'NONE',  ( -86.40926781137700630, -53.79403237629073686, 192.3592306068764515 ) ) ;
#65048 = EDGE_CURVE ( 'NONE', #24916, #26344, #73243, .T. ) ;
#65049 = ORIENTED_EDGE ( 'NONE', *, *, #48232, .F. ) ;
#65050 = CARTESIAN_POINT ( 'NONE',  ( 17.50000000000002842, 51.99987222567164480, 59.97465830876894444 ) ) ;
#65051 = CARTESIAN_POINT ( 'NONE',  ( 20.00000000000001066, -4.000000000000000000, 25.00000000000000000 ) ) ;
#65052 = CARTESIAN_POINT ( 'NONE',  ( -10.37493441333220900, -49.92101058743562447, 32.22302584859001229 ) ) ;
#65053 = CARTESIAN_POINT ( 'NONE',  ( -30.00000000000000000, 0.000000000000000000, 5.999999999999998224 ) ) ;
#65054 = AXIS2_PLACEMENT_3D ( 'NONE', #49433, #16547, #96936 ) ;
#65055 = CARTESIAN_POINT ( 'NONE',  ( 2.075968632161603100, -6.306992450857173971, -6.056431503346049183 ) ) ;
#65056 = ORIENTED_EDGE ( 'NONE', *, *, #95989, .F. ) ;
#65057 = DIRECTION ( 'NONE',  ( -1.000000000000000000, -1.224606353822377258E-16, -0.000000000000000000 ) ) ;
#65058 = CIRCLE ( 'NONE', #85725, 5.000000000000000888 ) ;
#65059 = CARTESIAN_POINT ( 'NONE',  ( -6.738141070038324187, -4.358126490537220121, -16.85492060643100842 ) ) ;
#65060 = CARTESIAN_POINT ( 'NONE',  ( -7.744991119775237465, 33.46438785425129936, -2.016316005557099000 ) ) ;
#65061 = CARTESIAN_POINT ( 'NONE',  ( 27.30955641668146328, 305.2295048154397250, -9.475470306339881077 ) ) ;
#65062 = CARTESIAN_POINT ( 'NONE',  ( 0.000000000000000000, 0.000000000000000000, 0.000000000000000000 ) ) ;
#65063 = FACE_OUTER_BOUND ( 'NONE', #61785, .T. ) ;
#65064 = CARTESIAN_POINT ( 'NONE',  ( 69.39616242234656340, -60.00000000000000711, 138.1480787444137661 ) ) ;
#65065 =( GEOMETRIC_REPRESENTATION_CONTEXT ( 3 ) GLOBAL_UNCERTAINTY_ASSIGNED_CONTEXT ( ( #89433 ) ) GLOBAL_UNIT_ASSIGNED_CONTEXT ( ( #709, #82193, #26149 ) ) REPRESENTATION_CONTEXT ( 'NONE', 'WORKASPACE' ) );
#65066 = CARTESIAN_POINT ( 'NONE',  ( -35.56416567323501710, 480.2820146177156175, -4.363888856302766683 ) ) ;
#65067 = VERTEX_POINT ( 'NONE', #24489 ) ;
#65068 = CARTESIAN_POINT ( 'NONE',  ( 105.5353273971932140, -2.002967142162725287E-29, 5.000000000000011546 ) ) ;
#65069 = CARTESIAN_POINT ( 'NONE',  ( -9.948688207305217190, 253.8702314949018444, -1.044946705213418259 ) ) ;
#65071 = DIRECTION ( 'NONE',  ( -1.000000000000000000, 0.000000000000000000, 0.000000000000000000 ) ) ;
#65070 = CARTESIAN_POINT ( 'NONE',  ( 12.27067942234224418, -14.21045842199423959, 34.40196113412964962 ) ) ;
#65072 = AXIS2_PLACEMENT_3D ( 'NONE', #79156, #54324, #95351 ) ;
#65073 = CARTESIAN_POINT ( 'NONE',  ( -4.211261491276407476, -1.586805402943917587, 103.7733746176806875 ) ) ;
#65074 = ORIENTED_EDGE ( 'NONE', *, *, #46061, .T. ) ;
#65075 = CARTESIAN_POINT ( 'NONE',  ( -21.63763341358889392, 304.1253123683783315, 9.995563593792510915 ) ) ;
#65076 = ORIENTED_EDGE ( 'NONE', *, *, #90578, .T. ) ;
#65077 = CARTESIAN_POINT ( 'NONE',  ( 33.21930856118554942, 484.9903775147098486, 0.3261662439072586794 ) ) ;
#65078 = DIRECTION ( 'NONE',  ( 0.000000000000000000, 0.000000000000000000, -1.000000000000000000 ) ) ;
#65079 = ORIENTED_EDGE ( 'NONE', *, *, #26095, .T. ) ;
#65080 = ADVANCED_FACE ( 'NONE', ( #90244 ), #77785, .T. ) ;
#65081 = CARTESIAN_POINT ( 'NONE',  ( 64.91565662643154155, 50.00000000002004441, 6.815324757472883910 ) ) ;
#65082 = CARTESIAN_POINT ( 'NONE',  ( -9.590319992950549377, 7.202961444570311400, -2.216063517372654612 ) ) ;
#65083 = CARTESIAN_POINT ( 'NONE',  ( -14.01278929553941488, -60.00000000000000711, 42.10626255143397856 ) ) ;
#65085 = CARTESIAN_POINT ( 'NONE',  ( 46.00000000000000000, 438.4646224975067526, 9.895601460514084735 ) ) ;
#65084 = CIRCLE ( 'NONE', #66870, 5.000000000000000888 ) ;
#65086 = CARTESIAN_POINT ( 'NONE',  ( 74.07531781632955870, -60.00000000000001421, 172.9861120789492475 ) ) ;
#65087 = CARTESIAN_POINT ( 'NONE',  ( 8.349999999999999645, -4.171999999999999709, 0.000000000000000000 ) ) ;
#65089 = CARTESIAN_POINT ( 'NONE',  ( 16.57071829965135024, -29.03055317263135748, 28.95038203199459659 ) ) ;
#65088 = CARTESIAN_POINT ( 'NONE',  ( -114.5769593907454862, -59.99999999999998579, 170.6727965893586827 ) ) ;
#65091 = CARTESIAN_POINT ( 'NONE',  ( 85.23752753509168656, -37.99999999999997158, 47.19075432804262960 ) ) ;
#65090 = UNCERTAINTY_MEASURE_WITH_UNIT (LENGTH_MEASURE( 1.000000000000000082E-05 ), #7699, 'distance_accuracy_value', 'NONE');
#65093 = EDGE_CURVE ( 'NONE', #19064, #2149, #20121, .T. ) ;
#65092 =( LENGTH_UNIT ( ) NAMED_UNIT ( * ) SI_UNIT ( .MILLI., .METRE. ) );
#65094 = CARTESIAN_POINT ( 'NONE',  ( -46.31354256535421854, -42.98738504804538962, 46.26985113983830900 ) ) ;
#65095 = CARTESIAN_POINT ( 'NONE',  ( -8.913811505013349290, 18.64284798592955283, 37.38269509653747491 ) ) ;
#65096 = VERTEX_POINT ( 'NONE', #11428 ) ;
#65097 = DIRECTION ( 'NONE',  ( -1.000000000000000000, -1.224606353822377258E-16, -0.000000000000000000 ) ) ;
#65098 = DIRECTION ( 'NONE',  ( 0.000000000000000000, 0.000000000000000000, 1.000000000000000000 ) ) ;
#65099 = CARTESIAN_POINT ( 'NONE',  ( 5.973896061805174185, -13.10340519129061043, 13.28276905619554427 ) ) ;
#65100 = VECTOR ( 'NONE', #101434, 1000.000000000000227 ) ;
#65101 = DIRECTION ( 'NONE',  ( -1.000000000000000000, -1.224606353822377258E-16, -0.000000000000000000 ) ) ;
#65102 = CARTESIAN_POINT ( 'NONE',  ( 31.00389226249483698, 502.9289871839745842, 8.047326149841639520 ) ) ;
#65103 = ORIENTED_EDGE ( 'NONE', *, *, #64247, .T. ) ;
#65104 = VECTOR ( 'NONE', #31497, 1000.000000000000000 ) ;
#65105 = VERTEX_POINT ( 'NONE', #94515 ) ;
#65106 = CARTESIAN_POINT ( 'NONE',  ( 95.99808094090420241, -30.00000000000683542, 199.9041741166194868 ) ) ;
#65107 = CARTESIAN_POINT ( 'NONE',  ( 19.34264572229572821, 41.87583415776160933, -80.60122430450024922 ) ) ;
#65108 = CARTESIAN_POINT ( 'NONE',  ( 5.441822646184710344, 41.96569307385608028, -59.31342461362935836 ) ) ;
#65109 = SURFACE_STYLE_USAGE ( .BOTH. , #46804 ) ;
#65110 = CARTESIAN_POINT ( 'NONE',  ( 98.15759235675383820, -30.00000000000000000, 138.6648893879348350 ) ) ;
#65111 = DIRECTION ( 'NONE',  ( 0.000000000000000000, 1.000000000000000000, 0.000000000000000000 ) ) ;
#65112 = ORIENTED_EDGE ( 'NONE', *, *, #3866, .T. ) ;
#65113 = EDGE_CURVE ( 'NONE', #97567, #25329, #45426, .T. ) ;
#65114 = ORIENTED_EDGE ( 'NONE', *, *, #35625, .T. ) ;
#65115 = ORIENTED_EDGE ( 'NONE', *, *, #38428, .T. ) ;
#65116 = AXIS2_PLACEMENT_3D ( 'NONE', #4200, #18828, #19898 ) ;
#65117 = CARTESIAN_POINT ( 'NONE',  ( 22.25669491856071858, 1.482358050883964840E-15, 0.000000000000000000 ) ) ;
#65118 = CARTESIAN_POINT ( 'NONE',  ( -5.308064226573042887, 41.67430808342687243, -70.56675994572434263 ) ) ;
#65119 = CONICAL_SURFACE ( 'NONE', #46192, 4.250000000000000000, 0.9599310885968754814 ) ;
#65120 = CIRCLE ( 'NONE', #49630, 0.9999999999999934497 ) ;
#65121 = CARTESIAN_POINT ( 'NONE',  ( -38.70871301288035227, 463.8566175871105770, 18.97601667485638544 ) ) ;
#65122 = ORIENTED_EDGE ( 'NONE', *, *, #63117, .F. ) ;
#65123 = CARTESIAN_POINT ( 'NONE',  ( 9.165151389911677882, 105.2671078128291384, -4.000000000000000888 ) ) ;
#65124 = ORIENTED_EDGE ( 'NONE', *, *, #46579, .T. ) ;
#65125 = CARTESIAN_POINT ( 'NONE',  ( 86.75754961941542831, 1.030564683017419500E-14, 0.000000000000000000 ) ) ;
#65126 = CARTESIAN_POINT ( 'NONE',  ( 81.68106932928363051, -38.84191837104209100, 195.5020664298707800 ) ) ;
#65127 = CARTESIAN_POINT ( 'NONE',  ( 11.66741649944374615, 8.917103227961233003, 9.153057184382511480 ) ) ;
#65128 = CARTESIAN_POINT ( 'NONE',  ( 51.84565611112584804, -38.00000000000000711, 53.44666998630373911 ) ) ;
#65129 = CONICAL_SURFACE ( 'NONE', #34136, 3.309500000000001663, 0.9599310885968770357 ) ;
#65130 = CARTESIAN_POINT ( 'NONE',  ( 38.37563681287258532, 311.1791213484684704, 5.838097343055311583 ) ) ;
#65131 = AXIS2_PLACEMENT_3D ( 'NONE', #31585, #92432, #18588 ) ;
#65132 = DIRECTION ( 'NONE',  ( 0.9722532735311555374, 0.000000000000000000, 0.2339306993704594051 ) ) ;
#65133 = PLANE ( 'NONE',  #4521 ) ;
#65134 = CARTESIAN_POINT ( 'NONE',  ( -40.66084078640387389, 460.3808361429900060, 2.363412739912913452 ) ) ;
#65135 = CARTESIAN_POINT ( 'NONE',  ( -5.603804764708762320, -47.29776092513153429, 103.9691152301449790 ) ) ;
#65136 = CARTESIAN_POINT ( 'NONE',  ( 32.80395775117305845, 487.0274233559335357, 8.980975396778106301 ) ) ;
#65137 = ORIENTED_EDGE ( 'NONE', *, *, #51879, .F. ) ;
#65138 = CIRCLE ( 'NONE', #85799, 4.000000000000001776 ) ;
#65139 = CARTESIAN_POINT ( 'NONE',  ( -43.00000000000000000, 436.5989882784185738, 19.94133085611155920 ) ) ;
#65141 = CARTESIAN_POINT ( 'NONE',  ( 9.819056950928633398, 294.6481068335447731, 1.893705519456528208 ) ) ;
#65140 = CARTESIAN_POINT ( 'NONE',  ( 7.000000000000000000, -80.00000000000000000, 12.61250543006184088 ) ) ;
#65142 = CARTESIAN_POINT ( 'NONE',  ( 7.804526534074642363, 54.21474955791582317, -1.781545048635569506 ) ) ;
#65143 = CARTESIAN_POINT ( 'NONE',  ( -1.469576158976823947E-15, -15.87499999999999289, 8.000000000000000000 ) ) ;
#65144 = CARTESIAN_POINT ( 'NONE',  ( -1.083333333333333703, 6.880090707843048214, -5.848636054922038419 ) ) ;
#65145 = DIRECTION ( 'NONE',  ( 0.000000000000000000, -1.000000000000000000, 0.000000000000000000 ) ) ;
#65146 = CARTESIAN_POINT ( 'NONE',  ( 19.01537497148453681, 303.6985849714293408, 9.904431725647269147 ) ) ;
#65147 = ORIENTED_EDGE ( 'NONE', *, *, #55290, .T. ) ;
#65148 = CARTESIAN_POINT ( 'NONE',  ( 84.96212205827315245, -46.56643884038170711, 187.4507856897367049 ) ) ;
#65149 = AXIS2_PLACEMENT_3D ( 'NONE', #4898, #47979, #30245 ) ;
#65150 = FACE_OUTER_BOUND ( 'NONE', #39257, .T. ) ;
#65151 = ORIENTED_EDGE ( 'NONE', *, *, #53539, .F. ) ;
#65152 = CARTESIAN_POINT ( 'NONE',  ( 82.82192797015540009, -57.67108540965746499, -28.52013474738419774 ) ) ;
#65153 = CARTESIAN_POINT ( 'NONE',  ( 36.35757485292823077, 437.5916776841876299, 4.247500867393328328 ) ) ;
#65154 = FACE_OUTER_BOUND ( 'NONE', #58635, .T. ) ;
#65155 = CARTESIAN_POINT ( 'NONE',  ( 0.000000000000000000, 274.9999999999999432, 0.000000000000000000 ) ) ;
#65156 = CARTESIAN_POINT ( 'NONE',  ( -81.59886796681669807, -29.99999999999999645, -6.443727801133209532 ) ) ;
#65157 = EDGE_CURVE ( 'NONE', #59854, #95973, #51896, .T. ) ;
#65158 = EDGE_CURVE ( 'NONE', #41040, #16697, #84784, .T. ) ;
#65159 = CARTESIAN_POINT ( 'NONE',  ( 28.98628617572774502, 14.82338180310330600, 41.90038909576666981 ) ) ;
#65160 = CARTESIAN_POINT ( 'NONE',  ( 5.219866590718106991, -5.000000000000000000, 8.922269033012842243 ) ) ;
#65161 = DIRECTION ( 'NONE',  ( -0.5735764363510512664, 0.8191520442889881348, 1.003171929053520309E-16 ) ) ;
#65162 = AXIS2_PLACEMENT_3D ( 'NONE', #46033, #70834, #103725 ) ;
#65164 = CARTESIAN_POINT ( 'NONE',  ( -13.93128718024267165, 2.716980047703895451, 5.530599625801929875 ) ) ;
#65163 = DIRECTION ( 'NONE',  ( 0.000000000000000000, -1.000000000000000000, 0.000000000000000000 ) ) ;
#65165 = EDGE_CURVE ( 'NONE', #54135, #15655, #89939, .T. ) ;
#65166 = DIRECTION ( 'NONE',  ( -0.000000000000000000, 1.000000000000000000, 0.000000000000000000 ) ) ;
#65167 = CARTESIAN_POINT ( 'NONE',  ( -28.88608732843799842, 18.87339843927421157, 39.88959139356617811 ) ) ;
#65168 =( NAMED_UNIT ( * ) PLANE_ANGLE_UNIT ( ) SI_UNIT ( $, .RADIAN. ) );
#65169 = CARTESIAN_POINT ( 'NONE',  ( 10.47772246152235986, -5.000000000000000000, -78.93829266523391652 ) ) ;
#65170 = CARTESIAN_POINT ( 'NONE',  ( 98.59800593614012598, 1.016364837396684119E-14, 0.000000000000000000 ) ) ;
#65171 = CARTESIAN_POINT ( 'NONE',  ( 38.09999999999999432, 3.309500000000003439, 4.052968581778167743E-16 ) ) ;
#65172 = EDGE_CURVE ( 'NONE', #4391, #58764, #92892, .T. ) ;
#65173 = CIRCLE ( 'NONE', #8356, 45.10524579772351217 ) ;
#65174 =( BOUNDED_SURFACE ( )  B_SPLINE_SURFACE ( 2, 3, ( 
 ( #2961, #11044, #101137, #53126, #101673, #27831, #27298, #75796, #86043, #12118, #60701, #43438, #45048, #68243, #100598, #59094, #43965, #1890, #92504, #60181, #93049, #34843, #84432, #10522, #52043, #76854, #95709, #22903, #103787, #29418, #78982, #62816, #39074, #46098 ),
 ( #63884, #104313, #6145, #94668, #39607, #21847, #5106, #54689, #70373, #71956, #38037, #29930, #80560, #30462, #78452, #14232, #63355, #87623, #12641, #104860, #80032, #31002, #20813, #70898, #38547, #55740, #13707, #96774, #46617, #37510, #79514, #103268, #88151, #5626 ),
 ( #88674, #47138, #61771, #71412, #53647, #14764, #96256, #62295, #4572, #22381, #47665, #55226, #6681, #72480, #28897, #86577, #95186, #45573, #21317, #54154, #87095, #13171, #90801, #40643, #106427, #25571, #25021, #49794, #149, #49254, #32586, #48195, #57876, #56270 ) ),
 .UNSPECIFIED., .F., .F., .F. ) 
 B_SPLINE_SURFACE_WITH_KNOTS ( ( 3, 3 ),
 ( 4, 2, 2, 2, 2, 2, 2, 2, 2, 2, 2, 2, 2, 2, 2, 2, 4 ),
 ( 0.000000000000000000, 1.000000000000000000 ),
 ( 0.9419214012998449181, 1.216880307836088360, 1.491839214372332023, 1.766798120908575465, 2.041757027444818906, 2.316715933981062570, 2.591674840517305789, 2.866633747053549452, 3.141592653589793116, 3.416551560126036780, 3.691510466662280443, 3.966469373198524107, 4.241428279734767770, 4.516387186271010989, 4.791346092807254209, 5.066304999343497428, 5.341263905879741536 ),
 .UNSPECIFIED. ) 
 GEOMETRIC_REPRESENTATION_ITEM ( )  RATIONAL_B_SPLINE_SURFACE ( (
 ( 1.000000000000000000, 1.000000000000000000, 1.000000000000000000, 1.000000000000000000, 1.000000000000000000, 1.000000000000000000, 1.000000000000000000, 1.000000000000000000, 1.000000000000000000, 1.000000000000000000, 1.000000000000000000, 1.000000000000000000, 1.000000000000000000, 1.000000000000000000, 1.000000000000000000, 1.000000000000000000, 1.000000000000000000, 1.000000000000000000, 1.000000000000000000, 1.000000000000000000, 1.000000000000000000, 1.000000000000000000, 1.000000000000000000, 1.000000000000000000, 1.000000000000000000, 1.000000000000000000, 1.000000000000000000, 1.000000000000000000, 1.000000000000000000, 1.000000000000000000, 1.000000000000000000, 1.000000000000000000, 1.000000000000000000, 1.000000000000000000),
 ( 1.857142857142858317, 1.857142857142858317, 1.857142857142858317, 1.857142857142858317, 1.857142857142858317, 1.857142857142858317, 1.857142857142858317, 1.857142857142858317, 1.857142857142858317, 1.857142857142858317, 1.857142857142858317, 1.857142857142858317, 1.857142857142858317, 1.857142857142858317, 1.857142857142858317, 1.857142857142858317, 1.857142857142858317, 1.857142857142858317, 1.857142857142858317, 1.857142857142858317, 1.857142857142858317, 1.857142857142858317, 1.857142857142858317, 1.857142857142858317, 1.857142857142858317, 1.857142857142858317, 1.857142857142858317, 1.857142857142858317, 1.857142857142858317, 1.857142857142858317, 1.857142857142858317, 1.857142857142858317, 1.857142857142858317, 1.857142857142858317),
 ( 1.000000000000000000, 1.000000000000000000, 1.000000000000000000, 1.000000000000000000, 1.000000000000000000, 1.000000000000000000, 1.000000000000000000, 1.000000000000000000, 1.000000000000000000, 1.000000000000000000, 1.000000000000000000, 1.000000000000000000, 1.000000000000000000, 1.000000000000000000, 1.000000000000000000, 1.000000000000000000, 1.000000000000000000, 1.000000000000000000, 1.000000000000000000, 1.000000000000000000, 1.000000000000000000, 1.000000000000000000, 1.000000000000000000, 1.000000000000000000, 1.000000000000000000, 1.000000000000000000, 1.000000000000000000, 1.000000000000000000, 1.000000000000000000, 1.000000000000000000, 1.000000000000000000, 1.000000000000000000, 1.000000000000000000, 1.000000000000000000) ) ) 
 REPRESENTATION_ITEM ( '' )  SURFACE ( )  );
#65175 = DIRECTION ( 'NONE',  ( -1.000000000000000000, -1.224606353822377258E-16, -0.000000000000000000 ) ) ;
#65176 = EDGE_CURVE ( 'NONE', #21079, #33104, #2657, .T. ) ;
#65177 = ORIENTED_EDGE ( 'NONE', *, *, #105637, .T. ) ;
#65178 = DIRECTION ( 'NONE',  ( -0.000000000000000000, -0.000000000000000000, -1.000000000000000000 ) ) ;
#65179 = CARTESIAN_POINT ( 'NONE',  ( 7.500000000000007105, -4.330127018922198090, -7.564338275809343592 ) ) ;
#65180 = CARTESIAN_POINT ( 'NONE',  ( -21.07344922941815213, -18.86340865632357122, -33.57730334312562803 ) ) ;
#65182 = CARTESIAN_POINT ( 'NONE',  ( -50.18744314967482723, -34.58944621710350020, -27.70643596530725716 ) ) ;
#65181 = DIRECTION ( 'NONE',  ( 1.000000000000000000, 1.224606353822377258E-16, 0.000000000000000000 ) ) ;
#65183 = ORIENTED_EDGE ( 'NONE', *, *, #71450, .F. ) ;
#65184 = COLOUR_RGB ( '', 0.40784314, 0.44705882, 0.49803922) ;
#65185 = ORIENTED_EDGE ( 'NONE', *, *, #783, .F. ) ;
#65186 = CARTESIAN_POINT ( 'NONE',  ( 0.000000000000000000, 0.000000000000000000, -3.432199999999999918 ) ) ;
#65187 = VECTOR ( 'NONE', #25037, 1000.000000000000000 ) ;
#65188 = AXIS2_PLACEMENT_3D ( 'NONE', #34406, #1444, #100160 ) ;
#65189 = CARTESIAN_POINT ( 'NONE',  ( 11.42599714053744009, 43.22993183554735452, -14.67767878811811499 ) ) ;
#65190 = CARTESIAN_POINT ( 'NONE',  ( -19.99999999999999289, -4.000000000000000000, 25.00000000000000000 ) ) ;
#65191 = CARTESIAN_POINT ( 'NONE',  ( -50.19229659092784601, -60.00000000000001421, -37.86681916100207701 ) ) ;
#65192 = VERTEX_POINT ( 'NONE', #19053 ) ;
#65193 = CARTESIAN_POINT ( 'NONE',  ( 5.467818114163457643, -22.30699358996656656, -30.53336729979983488 ) ) ;
#65194 = CARTESIAN_POINT ( 'NONE',  ( -71.80342408229677176, -30.00000000000000000, -19.71767938363507966 ) ) ;
#65195 = CIRCLE ( 'NONE', #35917, 4.400000000000000355 ) ;
#65196 = CARTESIAN_POINT ( 'NONE',  ( 97.51699909924960252, -45.26833302863503405, 193.9111182486593066 ) ) ;
#65197 = CARTESIAN_POINT ( 'NONE',  ( -17.71915776462827452, 45.45154592806376570, 4.750161495150144297 ) ) ;
#65198 = ORIENTED_EDGE ( 'NONE', *, *, #69675, .T. ) ;
#65199 = ORIENTED_EDGE ( 'NONE', *, *, #74780, .F. ) ;
#65200 = ORIENTED_EDGE ( 'NONE', *, *, #30508, .T. ) ;
#65201 = CARTESIAN_POINT ( 'NONE',  ( 30.59246000750163219, 327.9779158149556793, 15.85446903023333221 ) ) ;
#65202 = CARTESIAN_POINT ( 'NONE',  ( -5.000000000000039968, -12.89614509140995224, 12.11365041472577886 ) ) ;
#65203 = PRESENTATION_STYLE_ASSIGNMENT (( #49000 ) ) ;
#65204 = ORIENTED_EDGE ( 'NONE', *, *, #26591, .F. ) ;
#65205 = EDGE_CURVE ( 'NONE', #62746, #102908, #93680, .T. ) ;
#65206 = LINE ( 'NONE', #98101, #103001 ) ;
#65207 = CARTESIAN_POINT ( 'NONE',  ( -110.0428892116504755, 17.51648154115788358, 55.02144460582523777 ) ) ;
#65208 = CIRCLE ( 'NONE', #36013, 5.000000000000000000 ) ;
#65209 = CARTESIAN_POINT ( 'NONE',  ( -9.999999999997182698, 15.11700796860534268, -0.7408669144211869062 ) ) ;
#65210 = CARTESIAN_POINT ( 'NONE',  ( -114.2112478298105174, -57.67107988235927252, 175.3835541016526349 ) ) ;
#65211 = CARTESIAN_POINT ( 'NONE',  ( -1.320432766682874540E-15, -28.53125000204838813, 7.188101187500000044 ) ) ;
#65212 = CARTESIAN_POINT ( 'NONE',  ( 23.21751746555303342, -1.200000000000000030E-05, 30.70617127781016720 ) ) ;
#65213 = COLOUR_RGB ( '', 0.09019608, 0.27058824, 0.51372549) ;
#65214 = CARTESIAN_POINT ( 'NONE',  ( -0.08424723020174174071, 25.16821295365208044, 40.74999999999992895 ) ) ;
#65215 = CARTESIAN_POINT ( 'NONE',  ( 66.00571552735603120, 6.975173280561618775E-15, 0.000000000000000000 ) ) ;
#65216 = CARTESIAN_POINT ( 'NONE',  ( -68.53940498225642841, -14.21045842199433729, -27.47940008941059276 ) ) ;
#65217 = EDGE_CURVE ( 'NONE', #866, #35550, #100820, .T. ) ;
#65219 = EDGE_CURVE ( 'NONE', #68198, #85025, #93971, .T. ) ;
#65218 = LINE ( 'NONE', #74881, #11995 ) ;
#65220 = CARTESIAN_POINT ( 'NONE',  ( -53.40209911825037636, -39.50465069708222643, 56.96612769989180691 ) ) ;
#65221 = AXIS2_PLACEMENT_3D ( 'NONE', #98452, #106006, #32697 ) ;
#65222 = DIRECTION ( 'NONE',  ( 0.000000000000000000, -1.000000000000000000, 0.000000000000000000 ) ) ;
#65223 = EDGE_LOOP ( 'NONE', ( #3469, #995, #63065, #50400 ) ) ;
#65224 = CARTESIAN_POINT ( 'NONE',  ( -100.4704357492387601, -52.74943876303672141, 193.8537836153791147 ) ) ;
#65225 =( REPRESENTATION_RELATIONSHIP ('NONE','NONE', #69581, #25516 ) REPRESENTATION_RELATIONSHIP_WITH_TRANSFORMATION ( #61620 )SHAPE_REPRESENTATION_RELATIONSHIP( ) );
#65226 = CARTESIAN_POINT ( 'NONE',  ( -0.9108375754614689290, 296.5938209096384526, -10.00058097679043634 ) ) ;
#65227 = AXIS2_PLACEMENT_3D ( 'NONE', #89929, #72674, #40314 ) ;
#65228 = VERTEX_POINT ( 'NONE', #104699 ) ;
#65229 = CARTESIAN_POINT ( 'NONE',  ( -17.62469156230236678, 43.36877173574055888, 4.616701353127022678 ) ) ;
#65230 = CARTESIAN_POINT ( 'NONE',  ( 91.04369531743766686, -38.35020560426966796, 1.585978844074899419 ) ) ;
#65231 = CARTESIAN_POINT ( 'NONE',  ( 5.007715329123895321E-16, -7.505553499465175804, -6.064240316920414209 ) ) ;
#65232 = FACE_OUTER_BOUND ( 'NONE', #23049, .T. ) ;
#65233 = CARTESIAN_POINT ( 'NONE',  ( -15.77381400630083164, 302.5604448265047495, 9.875089995772468043 ) ) ;
#65234 = DIRECTION ( 'NONE',  ( -1.000000000000000000, -0.000000000000000000, -0.000000000000000000 ) ) ;
#65235 = CARTESIAN_POINT ( 'NONE',  ( 80.50372827376243379, -29.99999999999999645, 137.2448855364089297 ) ) ;
#65236 = EDGE_CURVE ( 'NONE', #77143, #106756, #7818, .T. ) ;
#65237 = CARTESIAN_POINT ( 'NONE',  ( 33.58349330513380693, 4.000000000000003553, 0.000000000000000000 ) ) ;
#65238 = CARTESIAN_POINT ( 'NONE',  ( -29.28872172473212032, 8.962789800749089153, 42.04350091203786377 ) ) ;
#65239 = DIRECTION ( 'NONE',  ( 0.000000000000000000, -0.3964176948853116444, -0.9180702648391440013 ) ) ;
#65240 = EDGE_CURVE ( 'NONE', #72931, #20962, #72842, .T. ) ;
#65241 = ORIENTED_EDGE ( 'NONE', *, *, #42760, .T. ) ;
#65242 = EDGE_LOOP ( 'NONE', ( #47603, #95175, #24872, #82440, #22015, #95862 ) ) ;
#65243 = CARTESIAN_POINT ( 'NONE',  ( 49.80781392084993087, -29.12675541338599672, 47.03600289386830013 ) ) ;
#65244 = CARTESIAN_POINT ( 'NONE',  ( 5.420470438621152631, 41.88321586334136981, -59.04137885805278785 ) ) ;
#65245 = CARTESIAN_POINT ( 'NONE',  ( 9.761892272724042030, 51.33867874450312740, 2.429489512219626057 ) ) ;
#65246 = EDGE_CURVE ( 'NONE', #100266, #77600, #55591, .T. ) ;
#65247 = ORIENTED_EDGE ( 'NONE', *, *, #89999, .T. ) ;
#65248 = CARTESIAN_POINT ( 'NONE',  ( -109.4490193154211966, -38.35608385809126730, 149.1993996903198081 ) ) ;
#65249 = EDGE_LOOP ( 'NONE', ( #84326, #48256, #45587, #4361, #101605 ) ) ;
#65250 = CARTESIAN_POINT ( 'NONE',  ( 35.59999999999999432, 1.533819458162526451E-15, 0.000000000000000000 ) ) ;
#65251 = CARTESIAN_POINT ( 'NONE',  ( 95.02435692186872984, -38.35555520635520566, 58.02324002954877358 ) ) ;
#65252 = CARTESIAN_POINT ( 'NONE',  ( 10.87357903135575121, 11.49182943363048359, -9.891806379494946455 ) ) ;
#65253 = CARTESIAN_POINT ( 'NONE',  ( -37.25037493859557003, 25.86378812652969472, -10.99421910838864491 ) ) ;
#65254 = CARTESIAN_POINT ( 'NONE',  ( 102.3385178479906443, -60.15132848126114595, 129.8721470524102983 ) ) ;
#65255 = CARTESIAN_POINT ( 'NONE',  ( -31.50909062064772570, 439.7150268719240671, 23.57203536488566797 ) ) ;
#65256 = CARTESIAN_POINT ( 'NONE',  ( -35.04726026986955389, 344.4762064160754562, -0.5379253706595517048 ) ) ;
#65257 = CARTESIAN_POINT ( 'NONE',  ( 6.463344223170836678, 4.601472318010335627, -5.710032555828794543 ) ) ;
#65258 = EDGE_CURVE ( 'NONE', #77934, #8789, #104370, .T. ) ;
#65259 = CARTESIAN_POINT ( 'NONE',  ( 74.65033017998224807, -60.00000000000001421, 178.4634517001849190 ) ) ;
#65260 = VECTOR ( 'NONE', #33351, 1000.000000000000000 ) ;
#65261 = CARTESIAN_POINT ( 'NONE',  ( 17.53457271110117333, 45.00000000000002842, 63.41726470817021521 ) ) ;
#65262 = ORIENTED_EDGE ( 'NONE', *, *, #49824, .F. ) ;
#65263 = CARTESIAN_POINT ( 'NONE',  ( 55.55584471301806104, -60.32186133166744924, 70.31348763753899789 ) ) ;
#65264 = CARTESIAN_POINT ( 'NONE',  ( -23.76958652213907541, 303.5250860149631080, -9.855208255818627805 ) ) ;
#65265 = CARTESIAN_POINT ( 'NONE',  ( 9.901690565149895207, -50.20903247757873089, 28.42036373910763558 ) ) ;
#65266 = DIRECTION ( 'NONE',  ( 0.000000000000000000, -1.000000000000000000, 0.000000000000000000 ) ) ;
#65267 = ORIENTED_EDGE ( 'NONE', *, *, #58110, .T. ) ;
#65269 = CARTESIAN_POINT ( 'NONE',  ( -9.934548988108780065, -50.13240894597250019, 28.17116772486389564 ) ) ;
#65268 = CARTESIAN_POINT ( 'NONE',  ( -89.79833081493985958, -38.39354622375766013, -16.47870807438435392 ) ) ;
#65270 = CARTESIAN_POINT ( 'NONE',  ( 4.916373759799319565, -2.999999999999999556, 6.397334739185442487 ) ) ;
#65271 = CARTESIAN_POINT ( 'NONE',  ( 31.27150491832618329, 363.0626246711562999, 21.43651293828456161 ) ) ;
#65272 = CARTESIAN_POINT ( 'NONE',  ( -41.72129495923037723, 464.4839086838818503, 17.13525251804149008 ) ) ;
#65273 = CARTESIAN_POINT ( 'NONE',  ( 4.898587196589412829E-16, -34.62499999999999289, -8.000000000000000000 ) ) ;
#65274 = FILL_AREA_STYLE ('',( #48009 ) ) ;
#65275 = COLOUR_RGB ( '', 0.09019608, 0.27058824, 0.51372549) ;
#65276 = AXIS2_PLACEMENT_3D ( 'NONE', #62390, #35072, #94766 ) ;
#65277 = CARTESIAN_POINT ( 'NONE',  ( 16.36650669486618881, 1.474610560812782335E-15, 0.000000000000000000 ) ) ;
#65278 = ORIENTED_EDGE ( 'NONE', *, *, #66239, .F. ) ;
#65279 = CARTESIAN_POINT ( 'NONE',  ( 82.48598427777827169, -50.01050129768884034, 180.4116382470554356 ) ) ;
#65280 = CARTESIAN_POINT ( 'NONE',  ( 5.802268690544500451, -46.54360925828362383, 103.8899761878886494 ) ) ;
#65281 = CARTESIAN_POINT ( 'NONE',  ( -41.39445455245019190, 437.1938976948999880, 21.06043167853144737 ) ) ;
#65282 = EDGE_LOOP ( 'NONE', ( #55303, #59614, #8926, #55697, #49058 ) ) ;
#65283 = CARTESIAN_POINT ( 'NONE',  ( 12.39938211278620450, -4.333194019920618700, -12.81742571347198911 ) ) ;
#65284 = CARTESIAN_POINT ( 'NONE',  ( 25.85375728719300170, 35.06604825452144070, -8.747230897557770390 ) ) ;
#65285 = CARTESIAN_POINT ( 'NONE',  ( 14.59067579026366701, 1.706082412480378396, 3.468700283488842739 ) ) ;
#65286 =( LENGTH_UNIT ( ) NAMED_UNIT ( * ) SI_UNIT ( .MILLI., .METRE. ) );
#65287 = DIRECTION ( 'NONE',  ( -1.000000000000000000, -0.000000000000000000, -0.000000000000000000 ) ) ;
#65288 = ADVANCED_FACE ( 'NONE', ( #23278, #103642 ), #14607, .T. ) ;
#65289 = PRESENTATION_STYLE_ASSIGNMENT (( #71254 ) ) ;
#65290 = CIRCLE ( 'NONE', #30913, 4.000000000000001776 ) ;
#65291 = EDGE_CURVE ( 'NONE', #73045, #29160, #50929, .T. ) ;
#65292 = CARTESIAN_POINT ( 'NONE',  ( 7.151597709147948123, 106.7892926505221283, 3.587174531012140566 ) ) ;
#65293 = DIRECTION ( 'NONE',  ( -1.000000000000000000, -0.000000000000000000, -0.000000000000000000 ) ) ;
#65294 = EDGE_CURVE ( 'NONE', #84725, #69241, #87475, .T. ) ;
#65297 = COLOUR_RGB ( '', 0.08235294, 0.09019608, 0.10196078) ;
#65296 = CARTESIAN_POINT ( 'NONE',  ( -10.07644798939788267, 15.01242816752345099, -10.37971395138495367 ) ) ;
#65295 = CARTESIAN_POINT ( 'NONE',  ( -8.594949192134683003, -19.66686426804723098, 35.27552358496240714 ) ) ;
#65298 = EDGE_CURVE ( 'NONE', #3581, #63037, #71637, .T. ) ;
#65299 = CARTESIAN_POINT ( 'NONE',  ( 7.188101187500001821, -14.56250000204838457, -2.977408999572650483 ) ) ;
#65300 = CARTESIAN_POINT ( 'NONE',  ( 20.19866560624230090, 294.7559120050365777, -2.020382211974508735 ) ) ;
#65301 = DIRECTION ( 'NONE',  ( -1.000000000000000000, -0.000000000000000000, -0.000000000000000000 ) ) ;
#65302 = AXIS2_PLACEMENT_3D ( 'NONE', #3548, #10032, #59662 ) ;
#65303 = ADVANCED_FACE ( 'NONE', ( #23821, #30850 ), #71788, .T. ) ;
#65304 = B_SPLINE_CURVE_WITH_KNOTS ( 'NONE', 3,
 ( #65128, #71616, #88880, #13906, #63558, #97478, #96451, #22588, #7408, #6340, #55425, #23633, #54896, #39282, #88358, #5826, #39808, #96969, #56490, #46820, #40321, #14434, #14969, #47343, #48402, #105068, #104518, #80236, #72160, #31208, #64093, #47865, #106100, #89420, #80772, #79717 ),
 .UNSPECIFIED., .F., .F.,
 ( 4, 2, 2, 2, 2, 2, 2, 2, 2, 2, 2, 2, 2, 2, 2, 2, 2, 4 ),
 ( 0.000000000000000000, 0.008790666710044045193, 0.01758133342008806957, 0.02637200013013209568, 0.03516266684017610444, 0.05274400026026411503, 0.07032533368035212562, 0.08790666710044017784, 0.09669733381048414844, 0.1054880005205281468, 0.1142786672305721174, 0.1230693339406161019, 0.1274646672956381566, 0.1318600006506601696, 0.1362553340056822104, 0.1384530006831932447, 0.1395518340219487896, 0.1406506673607043345 ),
 .UNSPECIFIED. ) ;
#65305 = ORIENTED_EDGE ( 'NONE', *, *, #88020, .T. ) ;
#65306 = CARTESIAN_POINT ( 'NONE',  ( -17.49999999999997158, 50.30551795522193004, 63.70247084375006352 ) ) ;
#65307 = EDGE_CURVE ( 'NONE', #51415, #13309, #92272, .T. ) ;
#65308 = EDGE_CURVE ( 'NONE', #19124, #29545, #106045, .T. ) ;
#65309 = CARTESIAN_POINT ( 'NONE',  ( 24.46941191925081327, 25.33812252964237999, 31.99975807270328332 ) ) ;
#65310 = CARTESIAN_POINT ( 'NONE',  ( -8.147310229349574939, 111.6670789908333745, -5.000000000003809397 ) ) ;
#65311 =( BOUNDED_SURFACE ( )  B_SPLINE_SURFACE ( 3, 2, ( 
 ( #91941, #49342, #83845 ),
 ( #42860, #89824, #98433 ),
 ( #15928, #16453, #60665 ),
 ( #68755, #12600, #27255 ),
 ( #18614, #12077, #45007 ),
 ( #85454, #101099, #67675 ),
 ( #4003, #2390, #69283 ),
 ( #36413, #11539, #93552 ),
 ( #61184, #51476, #84391 ),
 ( #52004, #1850, #76282 ),
 ( #10480, #86540, #27793 ),
 ( #20238, #60142, #93006 ),
 ( #43400, #35337, #19701 ),
 ( #59591, #102695, #19170 ),
 ( #102158, #86007, #52534 ),
 ( #100558, #28308, #44464 ),
 ( #35876, #68199, #77359 ),
 ( #53085, #77892, #94626 ),
 ( #69798, #84921, #94071 ),
 ( #34807, #3470, #36933 ),
 ( #76812, #11006, #28857 ),
 ( #43923, #2922, #61731 ),
 ( #101636, #20771, #53606 ),
 ( #75753, #26719, #92463 ) ),
 .UNSPECIFIED., .F., .F., .T. ) 
 B_SPLINE_SURFACE_WITH_KNOTS ( ( 4, 2, 2, 2, 2, 2, 2, 2, 2, 2, 2, 4 ),
 ( 3, 3 ),
 ( 0.004964016820073290440, 0.006562036933636941453, 0.008160057047200592467, 0.009758077160764244348, 0.01055708721754607116, 0.01135609727432789623, 0.01215510733110972130, 0.01295411738789154811, 0.01455213750145519999, 0.01535114755823702680, 0.01615015761501885361, 0.01774817772858250375 ),
 ( 0.000000000000000000, 1.000000000000000000 ),
 .UNSPECIFIED. ) 
 GEOMETRIC_REPRESENTATION_ITEM ( )  RATIONAL_B_SPLINE_SURFACE ( (
 ( 1.000000000000000000, 0.8660254037844384856, 1.000000000000000000),
 ( 1.000000000000000000, 0.8660222092865146326, 1.000000000000000000),
 ( 1.000000000000000000, 0.8641678725695443042, 1.000000000000000000),
 ( 1.000000000000000000, 0.8570944999502960737, 1.000000000000000000),
 ( 1.000000000000000000, 0.8517853798393946185, 1.000000000000000000),
 ( 1.000000000000000000, 0.8386467772024601697, 1.000000000000000000),
 ( 1.000000000000000000, 0.8308203150020515571, 1.000000000000000000),
 ( 1.000000000000000000, 0.8176719580059066406, 1.000000000000000000),
 ( 1.000000000000000000, 0.8130708599674437709, 1.000000000000000000),
 ( 1.000000000000000000, 0.8036702313420579502, 1.000000000000000000),
 ( 1.000000000000000000, 0.7988516037130688474, 1.000000000000000000),
 ( 1.000000000000000000, 0.7890840531758207543, 1.000000000000000000),
 ( 1.000000000000000000, 0.7841348415510249747, 1.000000000000000000),
 ( 1.000000000000000000, 0.7742194781316240615, 1.000000000000000000),
 ( 1.000000000000000000, 0.7692300867738712800, 1.000000000000000000),
 ( 1.000000000000000000, 0.7547027778490736916, 1.000000000000000000),
 ( 1.000000000000000000, 0.7455429868461489473, 1.000000000000000000),
 ( 1.000000000000000000, 0.7333839939153369292, 1.000000000000000000),
 ( 1.000000000000000000, 0.7295956578554230187, 1.000000000000000000),
 ( 1.000000000000000000, 0.7227015210647820265, 1.000000000000000000),
 ( 1.000000000000000000, 0.7196248032678934647, 1.000000000000000000),
 ( 1.000000000000000000, 0.7118099142936535895, 1.000000000000000000),
 ( 1.000000000000000000, 0.7084153614166502910, 1.000000000000000000),
 ( 1.000000000000000000, 0.7071067811865475727, 1.000000000000000000) ) ) 
 REPRESENTATION_ITEM ( '' )  SURFACE ( )  );
#65312 = DIRECTION ( 'NONE',  ( -1.000000000000000000, 0.000000000000000000, 0.000000000000000000 ) ) ;
#65313 = DIRECTION ( 'NONE',  ( 0.8191520442889974607, 1.003171929053531649E-16, -0.5735764363510380548 ) ) ;
#65314 = EDGE_LOOP ( 'NONE', ( #48337, #95775, #296, #86401, #374, #36914 ) ) ;
#65315 = VECTOR ( 'NONE', #33737, 1000.000000000000000 ) ;
#65316 = DIRECTION ( 'NONE',  ( 0.000000000000000000, -1.000000000000000000, 0.000000000000000000 ) ) ;
#65317 = FACE_OUTER_BOUND ( 'NONE', #6097, .T. ) ;
#65318 = ORIENTED_EDGE ( 'NONE', *, *, #92045, .T. ) ;
#65319 =( NAMED_UNIT ( * ) SI_UNIT ( $, .STERADIAN. ) SOLID_ANGLE_UNIT ( ) );
#65320 = CARTESIAN_POINT ( 'NONE',  ( -23.98369711357355527, 41.62067903365006316, -74.32819821803104787 ) ) ;
#65321 = CARTESIAN_POINT ( 'NONE',  ( -100.8702459599107897, -60.00000000000000000, 86.13901550309863353 ) ) ;
#65322 = CARTESIAN_POINT ( 'NONE',  ( 28.77727207546485744, 18.82954237789024532, -39.99083609194124023 ) ) ;
#65323 = CARTESIAN_POINT ( 'NONE',  ( 3.789997851623448167E-05, -46.43937203793843338, 31.62954529925878688 ) ) ;
#65324 = CARTESIAN_POINT ( 'NONE',  ( 19.70764564238371719, 304.7954121406193622, 9.925013215726785631 ) ) ;
#65325 = FACE_OUTER_BOUND ( 'NONE', #53111, .T. ) ;
#65327 = DIRECTION ( 'NONE',  ( -1.000000000000000000, 0.000000000000000000, 0.000000000000000000 ) ) ;
#65326 = CARTESIAN_POINT ( 'NONE',  ( 11.68767211932491712, -5.000000000000002665, -88.14097461399492772 ) ) ;
#65328 = AXIS2_PLACEMENT_3D ( 'NONE', #36830, #29276, #102591 ) ;
#65329 = CARTESIAN_POINT ( 'NONE',  ( -81.08908342379014300, -60.53280594523494784, 183.7735889067742221 ) ) ;
#65330 = VERTEX_POINT ( 'NONE', #13555 ) ;
#65331 = CARTESIAN_POINT ( 'NONE',  ( 7.500000000000005329, 44.25000000000000711, -71.71180648257555390 ) ) ;
#65332 = ORIENTED_EDGE ( 'NONE', *, *, #106495, .T. ) ;
#65333 = ORIENTED_EDGE ( 'NONE', *, *, #75474, .T. ) ;
#65334 = FACE_OUTER_BOUND ( 'NONE', #11708, .T. ) ;
#65335 = CARTESIAN_POINT ( 'NONE',  ( 18.91781669292794987, 48.00000000000000000, 62.18610382930901892 ) ) ;
#65336 = DIRECTION ( 'NONE',  ( -1.000000000000000000, -1.224606353822377258E-16, -0.000000000000000000 ) ) ;
#65337 = CARTESIAN_POINT ( 'NONE',  ( -15.79261075262967040, 4.810720122702830004, -5.431533035174125779 ) ) ;
#65338 = CARTESIAN_POINT ( 'NONE',  ( 3.768877481701073950, 19.36516179434251939, -5.000000000000000000 ) ) ;
#65339 = DIRECTION ( 'NONE',  ( 0.000000000000000000, -1.000000000000000000, 0.000000000000000000 ) ) ;
#65340 = LINE ( 'NONE', #49679, #19287 ) ;
#65341 = MECHANICAL_DESIGN_GEOMETRIC_PRESENTATION_REPRESENTATION (  '', ( #24045 ), #18890 ) ;
#65342 = CARTESIAN_POINT ( 'NONE',  ( 113.5291039388664700, -60.00000000000007105, 153.5981272189337403 ) ) ;
#65343 = ADVANCED_FACE ( 'NONE', ( #70746 ), #1329, .T. ) ;
#65344 = CARTESIAN_POINT ( 'NONE',  ( -109.5313977869038098, -29.99999999999998934, 176.4136249138144876 ) ) ;
#65345 = CARTESIAN_POINT ( 'NONE',  ( -62.66137373571188363, -39.48701201810304440, 79.45161525184568063 ) ) ;
#65346 = ORIENTED_EDGE ( 'NONE', *, *, #37779, .T. ) ;
#65347 = CARTESIAN_POINT ( 'NONE',  ( 63.92823401217728474, 38.95221377027642973, 0.7461719994844789872 ) ) ;
#65348 = CARTESIAN_POINT ( 'NONE',  ( 94.21848556752277659, -59.99999999996594369, 13.18754133863892974 ) ) ;
#65349 = VECTOR ( 'NONE', #63203, 999.9999999999998863 ) ;
#65350 = EDGE_LOOP ( 'NONE', ( #101192, #35179, #64764, #92833, #66141, #64180, #88190, #79702 ) ) ;
#65351 = FACE_OUTER_BOUND ( 'NONE', #76753, .T. ) ;
#65352 = AXIS2_PLACEMENT_3D ( 'NONE', #24292, #98140, #49045 ) ;
#65353 = CARTESIAN_POINT ( 'NONE',  ( -5.082755093536325042, -15.96875000204838635, -5.082755093536325930 ) ) ;
#65354 = CARTESIAN_POINT ( 'NONE',  ( -5.934079579182491848, 51.88593101752500303, 6.163529546931266978 ) ) ;
#65355 = ORIENTED_EDGE ( 'NONE', *, *, #55486, .F. ) ;
#65356 = DIRECTION ( 'NONE',  ( 0.000000000000000000, 0.000000000000000000, 1.000000000000000000 ) ) ;
#65357 = VERTEX_POINT ( 'NONE', #59892 ) ;
#65358 = DIRECTION ( 'NONE',  ( 0.000000000000000000, 0.000000000000000000, 1.000000000000000000 ) ) ;
#65359 = DIRECTION ( 'NONE',  ( 0.000000000000000000, -1.000000000000000000, 0.000000000000000000 ) ) ;
#65360 = CARTESIAN_POINT ( 'NONE',  ( -112.2379140073269497, -59.99999999999998579, 175.3422743821848258 ) ) ;
#65361 = CARTESIAN_POINT ( 'NONE',  ( -3.787335548950263142, -1.092153040502706896, 104.1352136098626318 ) ) ;
#65362 = CARTESIAN_POINT ( 'NONE',  ( -5.082755093536326818, -26.09375000204838813, 5.082755093536325042 ) ) ;
#65363 = DIRECTION ( 'NONE',  ( 0.000000000000000000, 0.000000000000000000, 1.000000000000000000 ) ) ;
#65364 = CARTESIAN_POINT ( 'NONE',  ( -37.56208910882862995, 463.3609840191068088, 20.02047205468374358 ) ) ;
#65365 = CARTESIAN_POINT ( 'NONE',  ( -6.310069744396033187, 53.41366035806711920, -8.023364406089665835 ) ) ;
#65366 = CARTESIAN_POINT ( 'NONE',  ( -11.00613692184842485, -4.988161163938196196, -12.57568679169951054 ) ) ;
#65367 =( LENGTH_UNIT ( ) NAMED_UNIT ( * ) SI_UNIT ( .MILLI., .METRE. ) );
#65368 = CARTESIAN_POINT ( 'NONE',  ( -21.29975379448946171, 294.8969325209483259, -1.990407376643346327 ) ) ;
#65369 = CARTESIAN_POINT ( 'NONE',  ( 106.0232194623858106, -59.99999999999999289, 182.0013391524945519 ) ) ;
#65370 = B_SPLINE_CURVE_WITH_KNOTS ( 'NONE', 3,
 ( #87891, #12386, #13444, #94936, #61505, #70106, #36723, #20563 ),
 .UNSPECIFIED., .F., .F.,
 ( 4, 2, 2, 4 ),
 ( -5.999999998302399854E-08, 0.002844838416977306123, 0.005689736833954595410, 0.01137953366790916965 ),
 .UNSPECIFIED. ) ;
#65371 = CARTESIAN_POINT ( 'NONE',  ( -32.10230308758781348, -25.61542695683890969, 31.36975326410992793 ) ) ;
#65372 = CIRCLE ( 'NONE', #106694, 5.000000000000011546 ) ;
#65373 = SURFACE_STYLE_FILL_AREA ( #66977 ) ;
#65374 =( GEOMETRIC_REPRESENTATION_CONTEXT ( 3 ) GLOBAL_UNCERTAINTY_ASSIGNED_CONTEXT ( ( #70686 ) ) GLOBAL_UNIT_ASSIGNED_CONTEXT ( ( #101775, #69426, #28459 ) ) REPRESENTATION_CONTEXT ( 'NONE', 'WORKASPACE' ) );
#65375 = CARTESIAN_POINT ( 'NONE',  ( 39.12690398050479246, -60.26094875330049661, 42.39772928756006110 ) ) ;
#65376 = CARTESIAN_POINT ( 'NONE',  ( 0.000000000000000000, 0.000000000000000000, -1.875285714285714445 ) ) ;
#65377 = ORIENTED_EDGE ( 'NONE', *, *, #100197, .T. ) ;
#65378 = DIRECTION ( 'NONE',  ( -0.9167413600884036784, 0.000000000000000000, -0.3994812620177121132 ) ) ;
#65379 = TOROIDAL_SURFACE ( 'NONE', #11937, 12.00000000000000711, 3.000000000000000000 ) ;
#65380 = CARTESIAN_POINT ( 'NONE',  ( -80.08331211031514840, -38.78820510874865590, 193.1379239215828250 ) ) ;
#65381 = EDGE_LOOP ( 'NONE', ( #73875, #93200 ) ) ;
#65383 = CARTESIAN_POINT ( 'NONE',  ( -23.61963550967466574, 306.0340374937824777, 10.19690224617928287 ) ) ;
#65382 = DIRECTION ( 'NONE',  ( -1.000000000000000000, -0.000000000000000000, -0.000000000000000000 ) ) ;
#65384 = CARTESIAN_POINT ( 'NONE',  ( -12.48597083465239876, 22.70279443506876760, 5.925685832145178189 ) ) ;
#65385 = DIRECTION ( 'NONE',  ( -1.000000000000000000, -1.224606353822377258E-16, -0.000000000000000000 ) ) ;
#65386 = CARTESIAN_POINT ( 'NONE',  ( -6.786616733794230250, 41.72678875807561383, -59.11526074045958268 ) ) ;
#65387 = CARTESIAN_POINT ( 'NONE',  ( 0.9546611534775700791, 43.32630963623820008, -18.31104130856166989 ) ) ;
#65388 = CARTESIAN_POINT ( 'NONE',  ( -39.62826361664709651, 437.5693818447127796, 4.806172978297276188 ) ) ;
#65389 = CARTESIAN_POINT ( 'NONE',  ( 5.191144708981714651, -87.64030085521270053, 3.015512395308853844 ) ) ;
#65390 = CARTESIAN_POINT ( 'NONE',  ( 17.73803972846102894, 45.30907581182018617, 6.035033385463663080 ) ) ;
#65391 = AXIS2_PLACEMENT_3D ( 'NONE', #22280, #55128, #88057 ) ;
#65392 = EDGE_CURVE ( 'NONE', #5935, #49696, #92763, .T. ) ;
#65393 = CARTESIAN_POINT ( 'NONE',  ( 110.0335605139551234, -59.99999999999999289, 143.7182336800421183 ) ) ;
#65394 = LINE ( 'NONE', #82636, #25278 ) ;
#65395 = ORIENTED_EDGE ( 'NONE', *, *, #93760, .F. ) ;
#65396 = CARTESIAN_POINT ( 'NONE',  ( -98.08299448810690535, -29.99999999999990763, 190.4420231606735570 ) ) ;
#65397 = ORIENTED_EDGE ( 'NONE', *, *, #40958, .T. ) ;
#65398 = VECTOR ( 'NONE', #15809, 1000.000000000000114 ) ;
#65399 = DIRECTION ( 'NONE',  ( -1.000000000000000000, -0.000000000000000000, -0.000000000000000000 ) ) ;
#65400 = CARTESIAN_POINT ( 'NONE',  ( -15.46526232232293907, 2.714356162034628817, -1.556038473642534115 ) ) ;
#65401 = CARTESIAN_POINT ( 'NONE',  ( 16.84999999999999787, 1.533819458162526451E-15, 0.000000000000000000 ) ) ;
#65402 = DIRECTION ( 'NONE',  ( 0.000000000000000000, -1.000000000000000000, 0.000000000000000000 ) ) ;
#65403 = CARTESIAN_POINT ( 'NONE',  ( 4.401442555609581635E-16, -23.65625000204838457, -7.188101187500000044 ) ) ;
#65404 = CARTESIAN_POINT ( 'NONE',  ( 17.23461538461538467, -4.171999999999999709, 0.000000000000000000 ) ) ;
#65405 = CARTESIAN_POINT ( 'NONE',  ( 7.224854171662427049, 41.52722309002922429, -69.60668040565890635 ) ) ;
#65406 = EDGE_LOOP ( 'NONE', ( #1949, #34704, #21591 ) ) ;
#65407 = AXIS2_PLACEMENT_3D ( 'NONE', #87527, #88056, #15743 ) ;
#65408 = PRODUCT_DEFINITION ( 'UNKNOWN', '', #19877, #26277 ) ;
#65410 = ORIENTED_EDGE ( 'NONE', *, *, #97724, .F. ) ;
#65409 = CARTESIAN_POINT ( 'NONE',  ( 4.781335833249819700, -2.669875467129551705, 102.4226025779373401 ) ) ;
#65411 = CARTESIAN_POINT ( 'NONE',  ( 80.49938719612642046, -42.96636524030287063, 153.2983854078102581 ) ) ;
#65412 = AXIS2_PLACEMENT_3D ( 'NONE', #80238, #38751, #78644 ) ;
#65413 = CARTESIAN_POINT ( 'NONE',  ( -6.503373625913253520, 41.93912930209143042, -59.84719177782724131 ) ) ;
#65414 = DIRECTION ( 'NONE',  ( -0.000000000000000000, 1.000000000000000000, 0.000000000000000000 ) ) ;
#65415 = EDGE_LOOP ( 'NONE', ( #17806, #39560, #417, #47053, #33306, #51656, #2320 ) ) ;
#65416 = CARTESIAN_POINT ( 'NONE',  ( -28.69358546713185021, 50.00000000000000000, 56.30708833178594830 ) ) ;
#65417 = CARTESIAN_POINT ( 'NONE',  ( -14.99515772855993134, 1.250937070399350537, -0.4481625125107416840 ) ) ;
#65418 = CARTESIAN_POINT ( 'NONE',  ( 5.082755093536325930, -12.96875000204838280, -5.082755093536325042 ) ) ;
#65419 = CARTESIAN_POINT ( 'NONE',  ( 7.045965687440314262, 28.69607536213965560, 3.790395326974319357 ) ) ;
#65420 = CARTESIAN_POINT ( 'NONE',  ( -43.89814859212165743, -59.99999999999997868, -33.20116366665202179 ) ) ;
#65421 = CARTESIAN_POINT ( 'NONE',  ( -32.88842731267402542, -57.69106633777249016, 47.18465683205923966 ) ) ;
#65422 = FILL_AREA_STYLE ('',( #111 ) ) ;
#65423 = ORIENTED_EDGE ( 'NONE', *, *, #45808, .F. ) ;
#65424 = APPLICATION_PROTOCOL_DEFINITION ( 'draft international standard', 'automotive_design', 1998, #41757 ) ;
#65425 = CARTESIAN_POINT ( 'NONE',  ( 39.44615384615384812, 1.411358822780289120E-15, 0.000000000000000000 ) ) ;
#65426 =( GEOMETRIC_REPRESENTATION_CONTEXT ( 3 ) GLOBAL_UNCERTAINTY_ASSIGNED_CONTEXT ( ( #79818 ) ) GLOBAL_UNIT_ASSIGNED_CONTEXT ( ( #31621, #23536, #92480 ) ) REPRESENTATION_CONTEXT ( 'NONE', 'WORKASPACE' ) );
#65427 = CARTESIAN_POINT ( 'NONE',  ( -8.000000000000000000, -19.34374999999999289, -3.313708498984762496 ) ) ;
#65428 = EDGE_CURVE ( 'NONE', #17674, #98844, #25179, .T. ) ;
#65429 = CARTESIAN_POINT ( 'NONE',  ( 23.58349330513380337, 1.593028355512270567E-15, 0.000000000000000000 ) ) ;
#65430 = ORIENTED_EDGE ( 'NONE', *, *, #66432, .T. ) ;
#65431 = CARTESIAN_POINT ( 'NONE',  ( -5.656854249492381470, -8.750000004096769146, 5.656854249492379694 ) ) ;
#65432 = CARTESIAN_POINT ( 'NONE',  ( 24.35999770972153300, -28.60365089118337423, 38.05418454928949501 ) ) ;
#65433 = CARTESIAN_POINT ( 'NONE',  ( 9.999999999999998224, 15.00000000000000000, -2.832769448823991188E-15 ) ) ;
#65434 = CARTESIAN_POINT ( 'NONE',  ( 9.757377548409222196E-14, 52.17923068443732149, -7.749999999998994582 ) ) ;
#65435 = CARTESIAN_POINT ( 'NONE',  ( 39.08940286296796529, 438.6059018380323096, 22.97295384703932086 ) ) ;
#65436 = SHAPE_DEFINITION_REPRESENTATION ( #86297, #59830 ) ;
#65437 = CARTESIAN_POINT ( 'NONE',  ( 49.19734730806133882, 7.744866885593247652, 16.05423930868156646 ) ) ;
#65438 = ORIENTED_EDGE ( 'NONE', *, *, #6513, .F. ) ;
#65439 = DIRECTION ( 'NONE',  ( 0.000000000000000000, 0.000000000000000000, -1.000000000000000000 ) ) ;
#65440 = ADVANCED_FACE ( 'NONE', ( #43160, #18923 ), #19993, .T. ) ;
#65441 = DIRECTION ( 'NONE',  ( -1.000000000000000000, -1.224606353822377258E-16, -0.000000000000000000 ) ) ;
#65442 = CARTESIAN_POINT ( 'NONE',  ( 69.40321497448834975, -38.19972286543485041, -31.40616810314683605 ) ) ;
#65443 = CARTESIAN_POINT ( 'NONE',  ( 43.30868969682389036, 1.340359594676612611E-15, 0.000000000000000000 ) ) ;
#65444 = EDGE_CURVE ( 'NONE', #94469, #102908, #69319, .T. ) ;
#65445 = CARTESIAN_POINT ( 'NONE',  ( 12.13034742782428310, 42.00000299666817938, -93.82352941176471006 ) ) ;
#65446 = B_SPLINE_CURVE_WITH_KNOTS ( 'NONE', 3,
 ( #11313, #22518, #47797, #103013, #85785, #39738, #44787, #72090 ),
 .UNSPECIFIED., .F., .F.,
 ( 4, 2, 2, 4 ),
 ( 0.000000000000000000, 0.2500000000000000000, 0.5000000000000000000, 1.000000000000000000 ),
 .UNSPECIFIED. ) ;
#65447 = PRESENTATION_LAYER_ASSIGNMENT (  '', '', ( #5174 ) ) ;
#65448 = EDGE_LOOP ( 'NONE', ( #42440, #82956, #62656, #49380, #80231 ) ) ;
#65449 = CARTESIAN_POINT ( 'NONE',  ( 0.1317522424410015880, 1.959574484677832018, -8.000000000000003553 ) ) ;
#65450 = CARTESIAN_POINT ( 'NONE',  ( 112.1546642664688704, -57.67108995165709473, 190.8163332172947833 ) ) ;
#65451 = AXIS2_PLACEMENT_3D ( 'NONE', #388, #16080, #49506 ) ;
#65452 = CARTESIAN_POINT ( 'NONE',  ( 36.00698207622300373, 463.3390700132977713, 20.06331035628539183 ) ) ;
#65453 = CARTESIAN_POINT ( 'NONE',  ( 17.23461538461538467, 1.411358822780289120E-15, 0.000000000000000000 ) ) ;
#65454 = CARTESIAN_POINT ( 'NONE',  ( 0.000000000000000000, 200.0000000000000000, 0.000000000000000000 ) ) ;
#65455 = CARTESIAN_POINT ( 'NONE',  ( -5.912056797256391327, 54.01423965850416664, 6.185180643280336454 ) ) ;
#65456 = CARTESIAN_POINT ( 'NONE',  ( -73.49971499675589826, -60.00000000000000000, 167.1873391204008783 ) ) ;
#65457 = CARTESIAN_POINT ( 'NONE',  ( -39.13885763974980136, 324.4948203046521371, 17.18769520460729439 ) ) ;
#65458 = SURFACE_STYLE_FILL_AREA ( #32048 ) ;
#65459 = CARTESIAN_POINT ( 'NONE',  ( -23.43684916743750080, 295.2641918988800285, 10.02474406024658293 ) ) ;
#65460 = CARTESIAN_POINT ( 'NONE',  ( -85.90370816398340992, -28.44268232177473621, 181.2109021316425412 ) ) ;
#65461 = ORIENTED_EDGE ( 'NONE', *, *, #31341, .T. ) ;
#65462 = CARTESIAN_POINT ( 'NONE',  ( 26.46671012315133353, 307.0860250144660881, -9.505648234697030574 ) ) ;
#65463 = CIRCLE ( 'NONE', #60327, 4.172000000000009479 ) ;
#65464 = AXIS2_PLACEMENT_3D ( 'NONE', #45738, #53817, #12820 ) ;
#65465 = ORIENTED_EDGE ( 'NONE', *, *, #62587, .F. ) ;
#65466 = CARTESIAN_POINT ( 'NONE',  ( -6.928203230275510549, -10.26526156932588130, 4.000000000000000888 ) ) ;
#65467 = CARTESIAN_POINT ( 'NONE',  ( 16.36650669486618881, 1.474610560812782335E-15, 0.000000000000000000 ) ) ;
#65468 = CARTESIAN_POINT ( 'NONE',  ( -82.96937446443966735, -37.77006566532177345, -10.80790838508248441 ) ) ;
#65469 = AXIS2_PLACEMENT_3D ( 'NONE', #104689, #23265, #29263 ) ;
#65470 = DIRECTION ( 'NONE',  ( -1.000000000000000000, -1.224606353822377258E-16, -0.000000000000000000 ) ) ;
#65471 = FILL_AREA_STYLE_COLOUR ( '', #75795 ) ;
#65472 = VERTEX_POINT ( 'NONE', #18811 ) ;
#65473 = CARTESIAN_POINT ( 'NONE',  ( 6.326592304916275111, 5.253140224433044736, -4.564380808752273921 ) ) ;
#65474 = CARTESIAN_POINT ( 'NONE',  ( 12.51321390371315267, 5.264046911284898655, -8.149122212578729929 ) ) ;
#65475 = CARTESIAN_POINT ( 'NONE',  ( 8.569529079651905690, -1.734723475976807094E-15, -14.86825985027703290 ) ) ;
#65476 = CARTESIAN_POINT ( 'NONE',  ( -36.07271708247948538, 437.4941479923684255, 4.311972135658442618 ) ) ;
#65477 = EDGE_CURVE ( 'NONE', #101891, #86867, #102692, .T. ) ;
#65478 = TOROIDAL_SURFACE ( 'NONE', #24233, 10.12668159690567826, 0.7733184030943209830 ) ;
#65479 = CARTESIAN_POINT ( 'NONE',  ( -8.554898963428433589, -59.99999999999994316, -44.87740334038038270 ) ) ;
#65480 = CARTESIAN_POINT ( 'NONE',  ( -79.07968554265760019, -25.61633390025545864, 127.8515609946744576 ) ) ;
#65481 = ORIENTED_EDGE ( 'NONE', *, *, #27401, .T. ) ;
#65482 = CARTESIAN_POINT ( 'NONE',  ( 36.05900422978820075, -60.00000000000002132, 50.77828662454974307 ) ) ;
#65483 = FILL_AREA_STYLE_COLOUR ( '', #98846 ) ;
#65484 = CARTESIAN_POINT ( 'NONE',  ( 113.8203870463297562, -57.67116299849189431, 161.9121400180774799 ) ) ;
#65485 = EDGE_LOOP ( 'NONE', ( #46506, #99712, #54204, #65204 ) ) ;
#65486 = CARTESIAN_POINT ( 'NONE',  ( 34.83349330513380693, 1.593028355512270962E-15, 0.000000000000000000 ) ) ;
#65487 = CIRCLE ( 'NONE', #84431, 4.000000000000000888 ) ;
#65488 = CARTESIAN_POINT ( 'NONE',  ( 9.349999999999997868, 1.533819458162526451E-15, 0.000000000000000000 ) ) ;
#65489 = ORIENTED_EDGE ( 'NONE', *, *, #47971, .T. ) ;
#65490 = DIRECTION ( 'NONE',  ( 0.5735764363510440500, 0.8191520442889932418, 0.000000000000000000 ) ) ;
#65491 = CARTESIAN_POINT ( 'NONE',  ( 17.33349330513380693, 1.593028355512270962E-15, 0.000000000000000000 ) ) ;
#65492 = DIRECTION ( 'NONE',  ( 0.000000000000000000, 1.000000000000000000, 0.000000000000000000 ) ) ;
#65493 = CARTESIAN_POINT ( 'NONE',  ( 7.188101187500000044, -16.15625000204838457, 0.000000000000000000 ) ) ;
#65494 = DIRECTION ( 'NONE',  ( -0.000000000000000000, 0.8660254037844391517, 0.4999999999999992228 ) ) ;
#65495 = CARTESIAN_POINT ( 'NONE',  ( 0.000000000000000000, 5.629165124598848990, 3.250000000000002220 ) ) ;
#65496 = CARTESIAN_POINT ( 'NONE',  ( -10.51296777078104050, 50.00000000000000000, -92.64705882352942012 ) ) ;
#65497 = ADVANCED_FACE ( 'NONE', ( #61913 ), #49229, .T. ) ;
#65498 = CARTESIAN_POINT ( 'NONE',  ( -17.83392795039137724, 45.30293236282058444, -5.798433727367500623 ) ) ;
#65499 = DIRECTION ( 'NONE',  ( -1.000000000000000000, -1.224606353822377258E-16, -0.000000000000000000 ) ) ;
#65500 = ORIENTED_EDGE ( 'NONE', *, *, #89607, .T. ) ;
#65501 = CARTESIAN_POINT ( 'NONE',  ( -7.499999999999896971, 40.28819309265733750, -69.28872504362320228 ) ) ;
#65503 = CARTESIAN_POINT ( 'NONE',  ( 28.19617395168271656, -18.63290521535086697, 28.87333934571989502 ) ) ;
#65502 = DIRECTION ( 'NONE',  ( 1.000000000000000000, 0.000000000000000000, 0.000000000000000000 ) ) ;
#65504 = CIRCLE ( 'NONE', #32807, 24.55262289886175964 ) ;
#65505 = CARTESIAN_POINT ( 'NONE',  ( -4.524349771038530754, 51.56521623581706137, -8.281859981072610566 ) ) ;
#65506 = VERTEX_POINT ( 'NONE', #84579 ) ;
#65507 = ORIENTED_EDGE ( 'NONE', *, *, #55218, .F. ) ;
#65509 = CARTESIAN_POINT ( 'NONE',  ( 1.250952833799880093, 51.63827851261836344, 9.151171491867097885 ) ) ;
#65508 = DIRECTION ( 'NONE',  ( 0.000000000000000000, -1.000000000000000000, 0.000000000000000000 ) ) ;
#65510 = FILL_AREA_STYLE_COLOUR ( '', #66355 ) ;
#65511 = CARTESIAN_POINT ( 'NONE',  ( -16.92109608899381001, 302.5811311245806223, -10.05744425352880533 ) ) ;
#65512 = CARTESIAN_POINT ( 'NONE',  ( 4.898587196589412829E-16, -19.81250000409677270, -8.000000000000000000 ) ) ;
#65513 = CARTESIAN_POINT ( 'NONE',  ( 1.990040563172386960E-15, 46.21383923812596350, 16.25000000000000000 ) ) ;
#65514 = CARTESIAN_POINT ( 'NONE',  ( -36.12805158198089117, 463.5537319797288092, 19.64593688561376794 ) ) ;
#65515 = ORIENTED_EDGE ( 'NONE', *, *, #8807, .T. ) ;
#65516 = EDGE_CURVE ( 'NONE', #31421, #74005, #4181, .T. ) ;
#65517 = CARTESIAN_POINT ( 'NONE',  ( 49.73772649942210222, -60.00000000000002132, -37.95607009740780313 ) ) ;
#65518 = CARTESIAN_POINT ( 'NONE',  ( -10.28624191511830155, 45.38549880562041494, -15.40779740156157196 ) ) ;
#65519 = CARTESIAN_POINT ( 'NONE',  ( 32.16723388112094284, 464.8262935154354523, 14.67703231816536658 ) ) ;
#65520 = CARTESIAN_POINT ( 'NONE',  ( 0.000000000000000000, 0.000000000000000000, -13.00000000000000000 ) ) ;
#65521 = EDGE_CURVE ( 'NONE', #10553, #75882, #106537, .T. ) ;
#65522 = CARTESIAN_POINT ( 'NONE',  ( 0.7145311798161605443, -4.618802153517258979, -8.000000000000001776 ) ) ;
#65523 = VERTEX_POINT ( 'NONE', #2574 ) ;
#65524 = CIRCLE ( 'NONE', #25992, 4.000000000000001776 ) ;
#65525 = CARTESIAN_POINT ( 'NONE',  ( -37.24777618596957751, 27.71756692439280556, 13.42512197595613799 ) ) ;
#65526 = EDGE_LOOP ( 'NONE', ( #102527, #91046, #15777 ) ) ;
#65527 = EDGE_LOOP ( 'NONE', ( #51496, #90670 ) ) ;
#65528 = CARTESIAN_POINT ( 'NONE',  ( 1.251035906659782038, 53.76664673156008689, 9.151124987501372487 ) ) ;
#65529 = FILL_AREA_STYLE_COLOUR ( '', #14850 ) ;
#65530 = CARTESIAN_POINT ( 'NONE',  ( -36.35273129748642873, 28.20658870731680778, 11.89657741949426217 ) ) ;
#65531 = CARTESIAN_POINT ( 'NONE',  ( 0.000000000000000000, -30.00000000000000000, 0.000000000000000000 ) ) ;
#65532 = CARTESIAN_POINT ( 'NONE',  ( -43.65150702672222138, 382.1424289287486999, 15.13344470041056411 ) ) ;
#65533 = CARTESIAN_POINT ( 'NONE',  ( 32.15310320217080431, 439.7024266304582056, 23.94087012106557211 ) ) ;
#65534 = DIRECTION ( 'NONE',  ( -0.000000000000000000, 1.000000000000000000, -0.000000000000000000 ) ) ;
#65536 = VERTEX_POINT ( 'NONE', #10138 ) ;
#65535 = AXIS2_PLACEMENT_3D ( 'NONE', #67843, #26894, #59235 ) ;
#65537 = CARTESIAN_POINT ( 'NONE',  ( -9.294025530568919891, 43.59757399217205887, 14.93482143293892683 ) ) ;
#65538 = VERTEX_POINT ( 'NONE', #68396 ) ;
#65539 = CARTESIAN_POINT ( 'NONE',  ( 8.719384894354538673, 51.50373999171648620, -4.031152949374879668 ) ) ;
#65540 = CARTESIAN_POINT ( 'NONE',  ( 4.440267933154150803, -48.84299975118083381, 104.3849335852974605 ) ) ;
#65541 = FACE_BOUND ( 'NONE', #8769, .T. ) ;
#65542 = CARTESIAN_POINT ( 'NONE',  ( 69.00182384322468465, -32.53477014765218911, 94.70385995679106372 ) ) ;
#65543 = EDGE_CURVE ( 'NONE', #76065, #106696, #21716, .T. ) ;
#65544 = ORIENTED_EDGE ( 'NONE', *, *, #85230, .F. ) ;
#65545 = TOROIDAL_SURFACE ( 'NONE', #105190, 74.46152422706630603, 68.00000000000000000 ) ;
#65546 =( LENGTH_UNIT ( ) NAMED_UNIT ( * ) SI_UNIT ( .MILLI., .METRE. ) );
#65547 = CARTESIAN_POINT ( 'NONE',  ( -6.770546484616568605, 9.415636748037993442, 1.794795801736669638 ) ) ;
#65548 = CARTESIAN_POINT ( 'NONE',  ( 6.281175601187043434, -3.752776749732574579, -6.500000000000000888 ) ) ;
#65549 = VERTEX_POINT ( 'NONE', #85098 ) ;
#65550 = CIRCLE ( 'NONE', #39765, 4.000000000000000888 ) ;
#65551 = FACE_OUTER_BOUND ( 'NONE', #87674, .T. ) ;
#65552 = AXIS2_PLACEMENT_3D ( 'NONE', #90080, #16724, #89027 ) ;
#65553 = CARTESIAN_POINT ( 'NONE',  ( 6.162888688655347558, -7.505553499465142053, -3.129864801432410934E-16 ) ) ;
#65554 = CARTESIAN_POINT ( 'NONE',  ( 3.313708498984762052, -22.90625000409676915, -8.000000000000000000 ) ) ;
#65555 = CARTESIAN_POINT ( 'NONE',  ( 45.11650669486618881, 4.000000000000003553, 4.898587196589414801E-16 ) ) ;
#65556 = CARTESIAN_POINT ( 'NONE',  ( 4.999999999999997335, -4.000000000000003553, 35.66025403784438197 ) ) ;
#65557 = VECTOR ( 'NONE', #21597, 1000.000000000000000 ) ;
#65558 = CARTESIAN_POINT ( 'NONE',  ( -10.31642403553700404, 7.048099644362463501, 5.000000000000000888 ) ) ;
#65559 = CARTESIAN_POINT ( 'NONE',  ( 7.045965687440313374, -8.696075362139659148, 3.790395326974318024 ) ) ;
#65560 =( NAMED_UNIT ( * ) PLANE_ANGLE_UNIT ( ) SI_UNIT ( $, .RADIAN. ) );
#65561 = CARTESIAN_POINT ( 'NONE',  ( -3.082707893549470501, 15.00000000000000178, -9.999999999999998224 ) ) ;
#65562 = ORIENTED_EDGE ( 'NONE', *, *, #77519, .F. ) ;
#65563 = DIRECTION ( 'NONE',  ( -0.000000000000000000, -0.000000000000000000, -1.000000000000000000 ) ) ;
#65564 = CARTESIAN_POINT ( 'NONE',  ( 7.006887204118438461, -59.99999999999998579, 39.62928630090096505 ) ) ;
#65565 = CARTESIAN_POINT ( 'NONE',  ( -96.67163991703634451, -30.00000000000000000, 191.1777818508784037 ) ) ;
#65566 = EDGE_CURVE ( 'NONE', #57881, #7789, #3118, .T. ) ;
#65567 = CARTESIAN_POINT ( 'NONE',  ( -32.94021323899823983, 485.0599191339510980, 5.361609822537303671 ) ) ;
#65568 = CARTESIAN_POINT ( 'NONE',  ( 73.76917559204071040, -57.62240879868848964, 185.9086365273194019 ) ) ;
#65569 = COLOUR_RGB ( '', 0.66274510, 0.83137255, 0.94901961) ;
#65570 = ADVANCED_FACE ( 'NONE', ( #77002 ), #1007, .T. ) ;
#65572 = CARTESIAN_POINT ( 'NONE',  ( -9.323499571257183760, 53.46640638443131621, 3.784400446240228533 ) ) ;
#65571 = CARTESIAN_POINT ( 'NONE',  ( 11.84999999999999787, -3.309499999999999886, 0.000000000000000000 ) ) ;
#65573 = CARTESIAN_POINT ( 'NONE',  ( 19.15691834943884331, -25.52937350832362995, -38.49469340411490492 ) ) ;
#65574 =( GEOMETRIC_REPRESENTATION_CONTEXT ( 3 ) GLOBAL_UNCERTAINTY_ASSIGNED_CONTEXT ( ( #103814 ) ) GLOBAL_UNIT_ASSIGNED_CONTEXT ( ( #16698, #51712, #467 ) ) REPRESENTATION_CONTEXT ( 'NONE', 'WORKASPACE' ) );
#65575 = DIRECTION ( 'NONE',  ( -1.000000000000000000, -1.224606353822377258E-16, -0.000000000000000000 ) ) ;
#65576 = UNCERTAINTY_MEASURE_WITH_UNIT (LENGTH_MEASURE( 1.000000000000000082E-05 ), #85460, 'distance_accuracy_value', 'NONE');
#65577 = CARTESIAN_POINT ( 'NONE',  ( -43.87333262554025026, 435.3945242957007054, 16.14343998352092413 ) ) ;
#65578 = CARTESIAN_POINT ( 'NONE',  ( -2.469906284812917185, -59.99999999999999289, 39.63522433654287624 ) ) ;
#65579 = CARTESIAN_POINT ( 'NONE',  ( 11.79490731899838885, 11.29963343840072021, 9.860884599382247373 ) ) ;
#65580 = CARTESIAN_POINT ( 'NONE',  ( 1.219168918416350333, 45.85934970230554342, -17.18082165270119788 ) ) ;
#65581 = CARTESIAN_POINT ( 'NONE',  ( -86.50123036836470192, -17.01944231672239383, 184.1032767441589328 ) ) ;
#65582 = EDGE_LOOP ( 'NONE', ( #15115, #37249, #75490, #21803, #83865, #105173, #90803 ) ) ;
#65583 = CARTESIAN_POINT ( 'NONE',  ( 17.50000000000003908, 51.97748320729017735, 60.75044042985544479 ) ) ;
#65584 = LINE ( 'NONE', #41832, #103872 ) ;
#65585 = CARTESIAN_POINT ( 'NONE',  ( -7.180605313813533286, -46.43926895535531685, 31.61986485186096019 ) ) ;
#65587 = CARTESIAN_POINT ( 'NONE',  ( 1.769226153621908271, -70.08155570559151215, 13.10633261097420643 ) ) ;
#65586 = CARTESIAN_POINT ( 'NONE',  ( 4.424031367838395568, -4.951337798340586183, -6.056431503346049183 ) ) ;
#65588 = EDGE_CURVE ( 'NONE', #30899, #28630, #52476, .T. ) ;
#65589 = ORIENTED_EDGE ( 'NONE', *, *, #23623, .T. ) ;
#65590 = VECTOR ( 'NONE', #105051, 1000.000000000000000 ) ;
#65591 = DIRECTION ( 'NONE',  ( 0.5735764363510468256, 0.8191520442889913545, 0.000000000000000000 ) ) ;
#65592 = CARTESIAN_POINT ( 'NONE',  ( -7.597212443346953670, -5.000000000001859846, -19.53267873631771323 ) ) ;
#65593 = CARTESIAN_POINT ( 'NONE',  ( -7.046289519167718396, 31.30591819944377008, -3.789821819998816288 ) ) ;
#65594 = CARTESIAN_POINT ( 'NONE',  ( 29.84172392461965728, 297.6780703762060512, -1.379986926139241676 ) ) ;
#65595 = DIRECTION ( 'NONE',  ( -1.000000000000000000, -1.224606353822377258E-16, -0.000000000000000000 ) ) ;
#65596 = CARTESIAN_POINT ( 'NONE',  ( -7.046357527897573192, -83.69384349398995937, -3.789683693877209159 ) ) ;
#65597 = EDGE_CURVE ( 'NONE', #57731, #16013, #52382, .T. ) ;
#65598 = CARTESIAN_POINT ( 'NONE',  ( 109.4307067020638726, -30.00000000000001066, 166.0292171922573345 ) ) ;
#65599 = DIRECTION ( 'NONE',  ( 0.000000000000000000, 1.000000000000000000, 0.000000000000000000 ) ) ;
#65600 = ORIENTED_EDGE ( 'NONE', *, *, #104134, .T. ) ;
#65601 = CARTESIAN_POINT ( 'NONE',  ( -1.529297411792386763, -30.00000000000000711, 7.172883640994426990 ) ) ;
#65602 = CARTESIAN_POINT ( 'NONE',  ( -9.537927238823533216, 252.6462685711817073, -3.010735687602405619 ) ) ;
#65603 = FILL_AREA_STYLE_COLOUR ( '', #9301 ) ;
#65604 = CARTESIAN_POINT ( 'NONE',  ( -2.621086668468698200, -7.606368536631376465, -7.634085501268432772 ) ) ;
#65605 = CARTESIAN_POINT ( 'NONE',  ( 45.50350659930133190, 397.4670913484075072, 8.242918921510581143 ) ) ;
#65606 = ADVANCED_FACE ( 'NONE', ( #27973, #43052, #75942, #93728 ), #20954, .T. ) ;
#65607 = CARTESIAN_POINT ( 'NONE',  ( 44.17588657940204655, 463.1658906400379578, 6.343983253506471520 ) ) ;
#65608 = VERTEX_POINT ( 'NONE', #80704 ) ;
#65609 = CIRCLE ( 'NONE', #19169, 1.000000000000000000 ) ;
#65610 = CARTESIAN_POINT ( 'NONE',  ( -22.90481894975329880, 305.6283220865303178, 10.10585484844669502 ) ) ;
#65611 = ORIENTED_EDGE ( 'NONE', *, *, #89709, .T. ) ;
#65613 = CARTESIAN_POINT ( 'NONE',  ( 32.99999999999987210, 485.0303364503728289, 0.9535057477322441688 ) ) ;
#65612 =( BOUNDED_CURVE ( )  B_SPLINE_CURVE ( 2, ( #67842, #93184, #19351 ),
 .UNSPECIFIED., .F., .F. ) 
 B_SPLINE_CURVE_WITH_KNOTS ( ( 3, 3 ),
 ( 0.000000000000000000, 1.000000000000000000 ),
 .UNSPECIFIED. ) 
 CURVE ( )  GEOMETRIC_REPRESENTATION_ITEM ( )  RATIONAL_B_SPLINE_CURVE ( ( 1.000000000000000000, 1.857142857142858317, 1.000000000000000000 ) ) 
 REPRESENTATION_ITEM ( '' )  );
#65614 = MECHANICAL_DESIGN_GEOMETRIC_PRESENTATION_REPRESENTATION (  '', ( #36327 ), #53527 ) ;
#65615 = CARTESIAN_POINT ( 'NONE',  ( 4.165977904505310470, 16.00000000000000000, 9.090909090909089940 ) ) ;
#65616 =( NAMED_UNIT ( * ) SI_UNIT ( $, .STERADIAN. ) SOLID_ANGLE_UNIT ( ) );
#65617 = CARTESIAN_POINT ( 'NONE',  ( 9.088913997560187141, 46.11732115646233865, 13.78939345329811061 ) ) ;
#65619 = EDGE_CURVE ( 'NONE', #13325, #10855, #30073, .T. ) ;
#65618 = ORIENTED_EDGE ( 'NONE', *, *, #89448, .F. ) ;
#65620 = CARTESIAN_POINT ( 'NONE',  ( 28.89099332390834363, 48.00000000000000000, 58.53034795347323893 ) ) ;
#65621 = CARTESIAN_POINT ( 'NONE',  ( -9.466116368847748319, 7.112870702781648902, -2.503129221841524199 ) ) ;
#65622 = CARTESIAN_POINT ( 'NONE',  ( -18.10756586307027050, -59.99999999999510436, 42.37213598781649893 ) ) ;
#65623 = AXIS2_PLACEMENT_3D ( 'NONE', #73915, #32965, #66364 ) ;
#65624 = CARTESIAN_POINT ( 'NONE',  ( 11.31153846153846132, 4.172000000000003261, 5.109226446042759579E-16 ) ) ;
#65625 = CARTESIAN_POINT ( 'NONE',  ( 92.32305526061090006, -60.00000000000002132, 24.43391867025795960 ) ) ;
#65626 = VECTOR ( 'NONE', #28105, 1000.000000000000000 ) ;
#65628 = CARTESIAN_POINT ( 'NONE',  ( 18.23452885637153997, -56.87686820525264153, 33.72162051064637467 ) ) ;
#65627 = CARTESIAN_POINT ( 'NONE',  ( -106.6034117734591860, -29.99999999999999645, 192.6833206840571791 ) ) ;
#65629 = CARTESIAN_POINT ( 'NONE',  ( 30.00000000000000000, 500.0000000000002274, 0.000000000000000000 ) ) ;
#65630 = SURFACE_STYLE_FILL_AREA ( #6307 ) ;
#65631 = CARTESIAN_POINT ( 'NONE',  ( -42.78963735806012636, -60.25406996619459932, 46.28178354334486500 ) ) ;
#65632 = CARTESIAN_POINT ( 'NONE',  ( -0.08414610906330061146, 35.08181111624585213, -27.24999999999999289 ) ) ;
#65633 = ORIENTED_EDGE ( 'NONE', *, *, #29911, .F. ) ;
#65634 = CARTESIAN_POINT ( 'NONE',  ( 16.10339698264846930, 21.83175592238090346, -0.8850307878419493290 ) ) ;
#65635 = CARTESIAN_POINT ( 'NONE',  ( 24.93816302196866275, 307.4233949143036284, 10.52291764336465008 ) ) ;
#65636 = CARTESIAN_POINT ( 'NONE',  ( 22.25669491856071858, 1.482358050883964840E-15, 0.000000000000000000 ) ) ;
#65638 = EDGE_CURVE ( 'NONE', #26511, #45176, #18243, .T. ) ;
#65637 = CARTESIAN_POINT ( 'NONE',  ( 0.000000000000000000, 0.000000000000000000, 1.734723475976807094E-15 ) ) ;
#65639 = CARTESIAN_POINT ( 'NONE',  ( 31.21933008645656926, 405.2090764464551853, 25.56980379099173817 ) ) ;
#65640 = ORIENTED_EDGE ( 'NONE', *, *, #13081, .T. ) ;
#65641 =( NAMED_UNIT ( * ) SI_UNIT ( $, .STERADIAN. ) SOLID_ANGLE_UNIT ( ) );
#65642 = ORIENTED_EDGE ( 'NONE', *, *, #87499, .F. ) ;
#65643 = CARTESIAN_POINT ( 'NONE',  ( 66.18517126493600244, -29.99999999992071409, 111.4181126619788529 ) ) ;
#65644 = CARTESIAN_POINT ( 'NONE',  ( 17.33910591856571770, 41.94145800377867062, -83.32002807799533173 ) ) ;
#65645 = UNCERTAINTY_MEASURE_WITH_UNIT (LENGTH_MEASURE( 1.000000000000000082E-05 ), #94094, 'distance_accuracy_value', 'NONE');
#65646 = DIRECTION ( 'NONE',  ( 0.000000000000000000, 0.000000000000000000, 1.000000000000000000 ) ) ;
#65647 = DIRECTION ( 'NONE',  ( 0.000000000000000000, 1.000000000000000000, 0.000000000000000000 ) ) ;
#65648 = CARTESIAN_POINT ( 'NONE',  ( 90.56647543664284683, -29.99999999999999645, 91.80300536945385659 ) ) ;
#65649 = ADVANCED_FACE ( 'NONE', ( #96392 ), #7887, .T. ) ;
#65650 = DIRECTION ( 'NONE',  ( 0.000000000000000000, 0.000000000000000000, -1.000000000000000000 ) ) ;
#65651 = ORIENTED_EDGE ( 'NONE', *, *, #55213, .T. ) ;
#65652 = CIRCLE ( 'NONE', #19195, 4.000000000000001776 ) ;
#65653 = VERTEX_POINT ( 'NONE', #46238 ) ;
#65654 = ORIENTED_EDGE ( 'NONE', *, *, #7127, .T. ) ;
#65655 = DIRECTION ( 'NONE',  ( 0.000000000000000000, 1.000000000000000000, 0.000000000000000000 ) ) ;
#65656 = FACE_OUTER_BOUND ( 'NONE', #11713, .T. ) ;
#65657 = VECTOR ( 'NONE', #32078, 1000.000000000000000 ) ;
#65658 = CARTESIAN_POINT ( 'NONE',  ( 39.34999999999999432, 3.309500000000003439, 0.000000000000000000 ) ) ;
#65659 = ORIENTED_EDGE ( 'NONE', *, *, #72182, .F. ) ;
#65660 = CARTESIAN_POINT ( 'NONE',  ( 9.918512371096300129, 108.7928299227055220, -1.297150762882702146 ) ) ;
#65661 = COLOUR_RGB ( '', 0.72549020, 0.75294118, 0.79215686) ;
#65662 = ORIENTED_EDGE ( 'NONE', *, *, #11141, .F. ) ;
#65663 = DIRECTION ( 'NONE',  ( -0.000000000000000000, -1.000000000000000000, -0.000000000000000000 ) ) ;
#65664 = CARTESIAN_POINT ( 'NONE',  ( 80.42530181681347301, -38.80960826814366271, 193.7223798169567033 ) ) ;
#65665 = CARTESIAN_POINT ( 'NONE',  ( 0.000000000000000000, 0.000000000000000000, 0.000000000000000000 ) ) ;
#65666 = CARTESIAN_POINT ( 'NONE',  ( 31.72480828332957614, 329.8229909459315650, 16.52334145234448926 ) ) ;
#65667 = CYLINDRICAL_SURFACE ( 'NONE', #84947, 62.00000000000000000 ) ;
#65668 = CARTESIAN_POINT ( 'NONE',  ( -28.23200706912922797, 34.17505432317837943, -9.354431903020278938 ) ) ;
#65669 = DIRECTION ( 'NONE',  ( -0.000000000000000000, -1.000000000000000000, -0.000000000000000000 ) ) ;
#65670 = DIRECTION ( 'NONE',  ( 1.000000000000000000, -0.000000000000000000, 1.224646799147353207E-16 ) ) ;
#65671 = AXIS2_PLACEMENT_3D ( 'NONE', #6870, #49985, #40306 ) ;
#65672 = CARTESIAN_POINT ( 'NONE',  ( -4.640907980698733226, 8.296333112989275449, 5.000000000000000888 ) ) ;
#65673 = ORIENTED_EDGE ( 'NONE', *, *, #48432, .T. ) ;
#65674 = CARTESIAN_POINT ( 'NONE',  ( 6.162888688655347558, 7.505553499465140277, 0.000000000000000000 ) ) ;
#65675 = CARTESIAN_POINT ( 'NONE',  ( -23.22454000777809924, 295.1922764084953315, 2.010205026916556115 ) ) ;
#65676 = CARTESIAN_POINT ( 'NONE',  ( 7.345812283465320114, 54.30771946477985779, -2.470391858893527193 ) ) ;
#65677 = UNCERTAINTY_MEASURE_WITH_UNIT (LENGTH_MEASURE( 1.000000000000000082E-05 ), #83082, 'distance_accuracy_value', 'NONE');
#65678 = DIRECTION ( 'NONE',  ( 0.000000000000000000, -1.000000000000000000, 0.000000000000000000 ) ) ;
#65679 = CYLINDRICAL_SURFACE ( 'NONE', #23208, 4.000000000000000000 ) ;
#65680 = CARTESIAN_POINT ( 'NONE',  ( 19.49818721152012202, -25.36617680456863155, 36.68312451770463412 ) ) ;
#65681 = CARTESIAN_POINT ( 'NONE',  ( 1.836970198721029589E-15, 0.000000000000000000, -15.00000000000000000 ) ) ;
#65682 = LINE ( 'NONE', #105088, #93192 ) ;
#65683 = VERTEX_POINT ( 'NONE', #54289 ) ;
#65684 = CARTESIAN_POINT ( 'NONE',  ( 84.77457301996732042, -53.82917485777404210, 190.3326470173193457 ) ) ;
#65685 = CARTESIAN_POINT ( 'NONE',  ( 0.000000000000000000, -0.1944580884125599318, -19.78098730681987760 ) ) ;
#65686 = CARTESIAN_POINT ( 'NONE',  ( -4.681380154937285987, 0.7378729568060279354, 103.7259032015045079 ) ) ;
#65687 = EDGE_LOOP ( 'NONE', ( #86729, #94144, #23286, #39778 ) ) ;
#65688 = CARTESIAN_POINT ( 'NONE',  ( 77.01964372777356971, -57.67122230834739582, -31.73091028824633852 ) ) ;
#65689 = B_SPLINE_CURVE_WITH_KNOTS ( 'NONE', 3,
 ( #15108, #95509, #7012, #55025, #21136, #12976, #96578, #47996, #45903, #63690, #78779, #105710, #53967, #29749, #4913, #80902, #39411, #37843, #96048, #38874, #46943, #71744 ),
 .UNSPECIFIED., .F., .F.,
 ( 4, 2, 2, 2, 2, 2, 2, 2, 2, 2, 4 ),
 ( 0.002852421517196360775, 0.003356447398460141000, 0.003860473279723920792, 0.004868525042251481243, 0.005120537982883364633, 0.005372550923515247157, 0.005624563864147129680, 0.005876576804779012203, 0.006380602686042778984, 0.006632615626674665844, 0.006884628567306552704 ),
 .UNSPECIFIED. ) ;
#65690 = AXIS2_PLACEMENT_3D ( 'NONE', #81471, #50190, #6 ) ;
#65691 = AXIS2_PLACEMENT_3D ( 'NONE', #62506, #4261, #3197 ) ;
#65692 = DIRECTION ( 'NONE',  ( 0.000000000000000000, -1.000000000000000000, -0.000000000000000000 ) ) ;
#65693 = CYLINDRICAL_SURFACE ( 'NONE', #83413, 5.000000000000000888 ) ;
#65694 = CARTESIAN_POINT ( 'NONE',  ( 28.46836751014411249, 13.00004364346769847, 40.55018863591786982 ) ) ;
#65695 = AXIS2_PLACEMENT_3D ( 'NONE', #36920, #61721, #43388 ) ;
#65696 = CARTESIAN_POINT ( 'NONE',  ( -81.46673774545078572, -29.99999999999999289, -9.566678094518634268 ) ) ;
#65697 = EDGE_CURVE ( 'NONE', #50266, #8098, #93765, .T. ) ;
#65698 = AXIS2_PLACEMENT_3D ( 'NONE', #26369, #20416, #44648 ) ;
#65699 = CARTESIAN_POINT ( 'NONE',  ( 29.59387530091309060, 18.41945862786180044, 39.60535821593452255 ) ) ;
#65700 = AXIS2_PLACEMENT_3D ( 'NONE', #79138, #23055, #96405 ) ;
#65701 = FACE_OUTER_BOUND ( 'NONE', #53592, .T. ) ;
#65702 = FACE_OUTER_BOUND ( 'NONE', #77995, .T. ) ;
#65703 = EDGE_CURVE ( 'NONE', #88469, #4042, #63040, .T. ) ;
#65705 = PRESENTATION_STYLE_ASSIGNMENT (( #74311 ) ) ;
#65704 = CARTESIAN_POINT ( 'NONE',  ( 31.36650669486618881, -3.851859888774471706E-31, 4.000000000000000888 ) ) ;
#65706 = AXIS2_PLACEMENT_3D ( 'NONE', #102962, #62512, #61996 ) ;
#65707 = CARTESIAN_POINT ( 'NONE',  ( 10.41054107240687188, 1.482358050883964840E-15, 0.000000000000000000 ) ) ;
#65708 = CARTESIAN_POINT ( 'NONE',  ( -28.98629307556481294, 14.82330134267485455, 41.90042541400651999 ) ) ;
#65709 = DIRECTION ( 'NONE',  ( 1.000000000000000000, 0.000000000000000000, 0.000000000000000000 ) ) ;
#65710 = CARTESIAN_POINT ( 'NONE',  ( -21.99019548641716426, 25.96786802809918271, 31.66672321705982895 ) ) ;
#65711 = CARTESIAN_POINT ( 'NONE',  ( 46.85000000000000142, 0.000000000000000000, 0.000000000000000000 ) ) ;
#65712 = CARTESIAN_POINT ( 'NONE',  ( 32.99999999999992895, 485.0303364503728289, 0.9535057477322521624 ) ) ;
#65713 = ORIENTED_EDGE ( 'NONE', *, *, #96878, .F. ) ;
#65714 = CARTESIAN_POINT ( 'NONE',  ( -6.009389902277268547, 3.157894738987889305, 14.66382285822740883 ) ) ;
#65715 = CYLINDRICAL_SURFACE ( 'NONE', #29774, 4.000000000000000000 ) ;
#65716 = LINE ( 'NONE', #16630, #7686 ) ;
#65717 = CARTESIAN_POINT ( 'NONE',  ( -69.34099659244546388, -29.97784688933757025, -21.09145479153141522 ) ) ;
#65719 = CARTESIAN_POINT ( 'NONE',  ( -68.60628786470475404, -47.40885926954825891, -24.67610123206565476 ) ) ;
#65718 = DIRECTION ( 'NONE',  ( -0.5735764363510497121, 0.8191520442889892450, 1.003171929053521665E-16 ) ) ;
#65720 = EDGE_CURVE ( 'NONE', #15534, #20022, #24244, .T. ) ;
#65721 = ORIENTED_EDGE ( 'NONE', *, *, #98891, .T. ) ;
#65722 = VECTOR ( 'NONE', #67479, 1000.000000000000227 ) ;
#65723 = ORIENTED_EDGE ( 'NONE', *, *, #21486, .T. ) ;
#65724 = CARTESIAN_POINT ( 'NONE',  ( 0.06682554136337934270, -4.993536075455425660, 4.350941807883113022 ) ) ;
#65725 =( GEOMETRIC_REPRESENTATION_CONTEXT ( 3 ) GLOBAL_UNCERTAINTY_ASSIGNED_CONTEXT ( ( #97062 ) ) GLOBAL_UNIT_ASSIGNED_CONTEXT ( ( #102514, #71709, #30228 ) ) REPRESENTATION_CONTEXT ( 'NONE', 'WORKASPACE' ) );
#65726 = CARTESIAN_POINT ( 'NONE',  ( 69.92761780597730592, 4.000000000000015099, 4.898587196589422689E-16 ) ) ;
#65727 = AXIS2_PLACEMENT_3D ( 'NONE', #44765, #85206, #77114 ) ;
#65728 = CARTESIAN_POINT ( 'NONE',  ( -6.499999999999999112, 3.752776749732556816, -0.7999999999999821698 ) ) ;
#65729 = CARTESIAN_POINT ( 'NONE',  ( -38.40660055531301253, -60.00000000000000000, -39.85627520488996822 ) ) ;
#65730 = ORIENTED_EDGE ( 'NONE', *, *, #89598, .T. ) ;
#65731 = CARTESIAN_POINT ( 'NONE',  ( 50.36674964328668835, -35.86795674544367074, -27.86065576867944316 ) ) ;
#65732 = CARTESIAN_POINT ( 'NONE',  ( 2.500000000000003109, -8.000000000000000000, 4.679304766526505863E-16 ) ) ;
#65733 = CARTESIAN_POINT ( 'NONE',  ( -3.375199152497164068, -0.8899603717835512517, 104.1123137168933965 ) ) ;
#65735 = CARTESIAN_POINT ( 'NONE',  ( -17.73948671138772326, 45.30893932440049099, 6.031879864029515481 ) ) ;
#65734 = PRESENTATION_STYLE_ASSIGNMENT (( #106164 ) ) ;
#65736 = EDGE_LOOP ( 'NONE', ( #92788, #38191, #5157, #62371, #72320, #100897 ) ) ;
#65737 = ORIENTED_EDGE ( 'NONE', *, *, #47383, .F. ) ;
#65738 = ORIENTED_EDGE ( 'NONE', *, *, #95507, .T. ) ;
#65739 = CARTESIAN_POINT ( 'NONE',  ( 30.08932219074489112, 331.1778411216668019, 15.36465306623354188 ) ) ;
#65740 = CARTESIAN_POINT ( 'NONE',  ( -5.000000000000000000, -13.85537367033497169, 10.16084852766932300 ) ) ;
#65741 = CARTESIAN_POINT ( 'NONE',  ( 15.66121600890972587, 45.99808261488239225, 6.197534896529969473 ) ) ;
#65743 = ADVANCED_FACE ( 'NONE', ( #88294 ), #81567, .F. ) ;
#65742 = ORIENTED_EDGE ( 'NONE', *, *, #35443, .F. ) ;
#65744 = CARTESIAN_POINT ( 'NONE',  ( 8.099999999999999645, -3.752776749732561257, 6.500000000000000000 ) ) ;
#65745 = CARTESIAN_POINT ( 'NONE',  ( -72.28092228780032258, 43.22324503868516388, -36.14046114390016839 ) ) ;
#65746 = CARTESIAN_POINT ( 'NONE',  ( -32.70943946516481304, 465.7622690753373149, 11.83845320051247363 ) ) ;
#65747 = CARTESIAN_POINT ( 'NONE',  ( -66.37944403907447111, -57.68041551771388953, 132.8370836190597686 ) ) ;
#65748 = CARTESIAN_POINT ( 'NONE',  ( -7.188101187500001821, -33.50000000204838813, -2.977408999572651371 ) ) ;
#65749 = CARTESIAN_POINT ( 'NONE',  ( 7.551892080562057075, -68.00987702539384827, 2.647003822403976248 ) ) ;
#65750 = CARTESIAN_POINT ( 'NONE',  ( -0.7828899409542838805, 25.26077281027161447, 40.48829533037867634 ) ) ;
#65751 = CARTESIAN_POINT ( 'NONE',  ( -6.287528586677907235E-14, 28.20649408426966431, -38.24999999999931077 ) ) ;
#65752 = CARTESIAN_POINT ( 'NONE',  ( -52.81151229832320126, -14.21045842199429643, -31.95502044027141153 ) ) ;
#65753 = CARTESIAN_POINT ( 'NONE',  ( -43.52578837347117258, 465.2717874277799979, 9.360669990305815702 ) ) ;
#65754 = CARTESIAN_POINT ( 'NONE',  ( -53.27082796895624739, -42.97299545974212265, 58.02614799047049132 ) ) ;
#65755 = CARTESIAN_POINT ( 'NONE',  ( 2.652922838662404637, 20.85721228183317422, -6.480801738300289827 ) ) ;
#65756 = ORIENTED_EDGE ( 'NONE', *, *, #63645, .T. ) ;
#65757 = CARTESIAN_POINT ( 'NONE',  ( -96.63378167814529718, -37.69171814361656914, 192.9088573962275461 ) ) ;
#65758 = CARTESIAN_POINT ( 'NONE',  ( -1.853816988907133201, 295.4475851226396230, -10.00136337793561658 ) ) ;
#65759 = CARTESIAN_POINT ( 'NONE',  ( 9.720957446278301717, -3.400539410478017555, 14.97579417183843020 ) ) ;
#65760 = ORIENTED_EDGE ( 'NONE', *, *, #81985, .T. ) ;
#65761 = CARTESIAN_POINT ( 'NONE',  ( 42.31104777394612171, 465.8656652864358421, 14.28483731023800551 ) ) ;
#65762 = CARTESIAN_POINT ( 'NONE',  ( 88.07186593688837206, -38.55612627883184729, 199.9830497965955374 ) ) ;
#65763 = DIRECTION ( 'NONE',  ( -3.469446951953614189E-16, 1.000000000000000000, -0.000000000000000000 ) ) ;
#65764 = DIRECTION ( 'NONE',  ( -1.000000000000000000, -1.224606353822377258E-16, -0.000000000000000000 ) ) ;
#65765 = CIRCLE ( 'NONE', #34845, 74.46152422706630603 ) ;
#65766 = CARTESIAN_POINT ( 'NONE',  ( -17.32323128014020241, 302.5970885151348284, 9.883177281172553563 ) ) ;
#65767 = CARTESIAN_POINT ( 'NONE',  ( 75.30000000000001137, 0.000000000000000000, 0.000000000000000000 ) ) ;
#65768 = CARTESIAN_POINT ( 'NONE',  ( 83.22245246229280724, -30.00000000000001066, 154.5341563752995171 ) ) ;
#65769 = CONICAL_SURFACE ( 'NONE', #72610, 3.309500000000001663, 0.9599310885968770357 ) ;
#65770 = CARTESIAN_POINT ( 'NONE',  ( 35.17753024347895519, 490.3634983170069859, 12.17893648721826594 ) ) ;
#65771 = CARTESIAN_POINT ( 'NONE',  ( -28.58246259357190056, 11.06567680426943667, 41.45945986390892557 ) ) ;
#65772 = EDGE_CURVE ( 'NONE', #12412, #59786, #32732, .T. ) ;
#65773 = FACE_BOUND ( 'NONE', #5260, .T. ) ;
#65774 = VERTEX_POINT ( 'NONE', #16513 ) ;
#65775 = EDGE_LOOP ( 'NONE', ( #80844, #16435, #46062, #63906 ) ) ;
#65776 = CARTESIAN_POINT ( 'NONE',  ( 49.92757571601900679, -22.20139394744939310, 44.97315255701366254 ) ) ;
#65777 = CARTESIAN_POINT ( 'NONE',  ( -9.970195021759442611, 302.6460196488377505, -10.04373974541436887 ) ) ;
#65778 = DIRECTION ( 'NONE',  ( -1.000000000000000000, 0.000000000000000000, 0.000000000000000000 ) ) ;
#65779 = ADVANCED_FACE ( 'NONE', ( #7877 ), #68197, .T. ) ;
#65780 = AXIS2_PLACEMENT_3D ( 'NONE', #17675, #74818, #9555 ) ;
#65781 = VERTEX_POINT ( 'NONE', #98485 ) ;
#65782 = CARTESIAN_POINT ( 'NONE',  ( -92.49477123227754305, -38.35497500972908114, 39.22377915011799132 ) ) ;
#65783 = ORIENTED_EDGE ( 'NONE', *, *, #92450, .F. ) ;
#65784 = SURFACE_STYLE_USAGE ( .BOTH. , #32907 ) ;
#65785 = CARTESIAN_POINT ( 'NONE',  ( 90.85852390707832171, -38.35167856242225781, 20.58440466305621896 ) ) ;
#65786 = CARTESIAN_POINT ( 'NONE',  ( 15.53256180499085914, 22.93947847607967105, 1.135875605542641775 ) ) ;
#65787 = CARTESIAN_POINT ( 'NONE',  ( 99.60646395647034979, -52.71694380898900079, 120.4330034612430609 ) ) ;
#65788 = CYLINDRICAL_SURFACE ( 'NONE', #71446, 1.250000000000001110 ) ;
#65789 =( LENGTH_UNIT ( ) NAMED_UNIT ( * ) SI_UNIT ( .MILLI., .METRE. ) );
#65790 = CARTESIAN_POINT ( 'NONE',  ( -36.38929466959749703, 356.0392961366259215, 1.859378810536674198 ) ) ;
#65791 = FILL_AREA_STYLE_COLOUR ( '', #4031 ) ;
#65792 = CARTESIAN_POINT ( 'NONE',  ( 74.21597319742625132, -60.00000000000000000, 174.3876596883068828 ) ) ;
#65793 = B_SPLINE_CURVE_WITH_KNOTS ( 'NONE', 3,
 ( #42697, #76119, #2215, #51841, #85840, #35165, #27087, #85282, #59974, #84754, #43755, #3303, #44297, #87423, #14550, #64208, #47459, #12440, #22163, #63678, #96037, #96566, #46420, #54474, #97078, #55012, #71729, #103068, #46932, #45366, #38352, #29224, #21639, #53957, #13497, #79306, #88475, #45890, #62610, #5428, #79831, #31326, #71212, #104106, #87944, #14026, #38863, #70164, #62098, #94990, #30249, #63137, #78249, #86893, #5936, #21128, #22701, #104641, #37833, #55538, #95496, #30793, #4362, #80352, #37298, #6467, #39399, #72277, #105181, #53454, #86374, #12966, #29737, #78768, #4902, #70697, #103588, #80890, #16699, #90590, #65785, #72793, #98141, #23763, #24293, #57142, #58216, #15627, #32379, #90055, #49590, #81943, #74389, #73319, #98663, #42032, #32908, #89536, #40977, #33979, #16159, #8065, #47983, #56611, #24815, #105698, #33436, #57667, #7521, #25353, #65251, #56061, #73865, #64722, #82498, #106760, #8599, #49046, #41501, #74914, #48519, #17251, #81410, #468, #66310, #99191, #7001, #40439, #91141, #50122, #998, #23222, #83031, #9122, #66851, #89001, #39921, #15096, #31840, #97596, #106215, #1555, #83549, #100271, #44173, #27499, #93249, #43105, #34520, #9649, #36122, #85706, #93783, #60374, #19412, #36650, #76520, #52246, #2091, #84093, #85155, #67389, #26433, #68450, #51713, #50631, #77060, #19944, #91664, #59298, #101866, #77602, #60895, #67908, #11244, #18320, #17778, #3176, #51170, #3720, #10193, #92170, #101345, #42559, #75462, #52784, #68991, #59835, #26955, #11783, #99740, #44713, #58766, #28026, #25910, #75993, #35044, #100795, #92709, #18869, #84628, #10715, #43631, #2631, #35577, #87824, #21512, #78123, #53328, #70034, #13903, #103984, #63014, #12842, #4239, #86246, #5822, #55422, #63555, #30126, #95912, #37714, #30667, #54348, #4772, #20490, #22036, #37173, #102938, #38230, #87290, #12319, #46817, #96448, #61431, #29104, #71613, #47339, #22584, #70577, #54893, #94325, #79714, #21004, #80233, #86775, #38742, #61972, #13369, #45244, #62485, #94863, #104515, #53844, #95376, #6337, #69515, #102400, #45761, #88355, #78637, #14431, #103464, #28550, #29613, #46296, #79185, #5310, #71094, #106640, #81815, #47862, #32246, #7406, #91020, #106097, #40847, #40319, #16041, #14966, #39805, #98023, #90466, #89418, #7941, #58091, #48921, #105580, #57020, #50004, #65126, #32790, #24176, #17126, #89934, #15510, #73740, #64089, #31721, #65664, #82909, #72157, #98545, #80769, #24696, #57546, #16579, #48400, #49465, #39279, #72679, #99069, #82372, #96966, #6884, #8479, #41384, #81290, #73194, #55937, #25234, #74275, #64606, #349, #105065, #31205, #23101, #97476, #33317, #23631, #66189, #88877, #56488, #10080, #19822, #10603, #27382, #58646, #2511, #74798, #100678, #1977, #83969, #60781, #75877, #43521, #42989, #92590, #91548, #9531, #101748, #93670, #67792, #34924, #84514, #76397, #101226, #25790, #17656, #50519, #26842, #59714, #52656, #18746, #92058, #51595, #33857, #75335, #35456, #27918, #68330, #60262, #878, #85042, #66729, #3053, #36002, #93130, #9006, #19302, #26318, #52126, #99613, #83434, #11124, #44049, #59179, #76940, #68875, #18195, #41912, #51052, #42444, #1436, #100152, #34397, #67273, #95266, #36533, #103863, #37593, #102822, #61307, #37054, #30542, #86658, #30013, #3596, #46697, #45651, #69398, #20896, #44594, #62899, #87704, #53730, #79594, #70456 ),
 .UNSPECIFIED., .F., .F.,
 ( 4, 2, 2, 2, 1, 1, 2, 2, 1, 1, 2, 2, 2, 2, 1, 2, 2, 2, 2, 2, 2, 1, 2, 2, 1, 1, 2, 2, 2, 2, 1, 2, 2, 1, 2, 2, 1, 1, 2, 2, 1, 1, 2, 2, 2, 2, 1, 1, 1, 2, 2, 1, 1, 2, 2, 2, 2, 1, 1, 1, 2, 2, 1, 1, 1, 1, 2, 2, 2, 2, 1, 1, 2, 2, 1, 1, 1, 1, 1, 2, 2, 2, 2, 2, 2, 1, 1, 1, 1, 1, 1, 1, 1, 2, 2, 2, 2, 2, 2, 2, 1, 1, 1, 1, 1, 1, 1, 1, 2, 2, 2, 2, 2, 1, 1, 1, 1, 1, 1, 1, 2, 2, 2, 2, 2, 1, 1, 1, 1, 1, 2, 2, 2, 2, 2, 1, 1, 1, 1, 2, 2, 2, 2, 1, 1, 1, 1, 1, 1, 1, 2, 2, 2, 2, 2, 2, 2, 1, 1, 1, 1, 1, 2, 2, 2, 2, 2, 2, 1, 1, 1, 1, 1, 1, 2, 2, 2, 2, 1, 1, 1, 1, 1, 1, 2, 2, 2, 2, 2, 1, 1, 1, 1, 2, 2, 2, 2, 1, 1, 1, 1, 1, 1, 2, 2, 2, 2, 2, 1, 1, 1, 1, 2, 2, 2, 2, 2, 1, 1, 1, 2, 2, 2, 2, 2, 2, 2, 1, 1, 1, 1, 1, 2, 2, 2, 2, 2, 1, 1, 1, 1, 1, 1, 2, 2, 2, 2, 2, 2, 1, 1, 1, 1, 2, 2, 2, 2, 2, 2, 2, 1, 1, 1, 1, 1, 1, 1, 2, 2, 2, 2, 2, 4 ),
 ( 0.000000000000000000, 0.007812499999651020474, 0.01562499999930204095, 0.01953124999912755899, 0.02001953124910586107, 0.02026367187409502599, 0.02038574218658967263, 0.02041625976471338547, 0.02044677734283709830, 0.02050781249908453438, 0.02148437499904310224, 0.02343749999896022757, 0.02734374999879447821, 0.02929687499871158965, 0.03027343749867014017, 0.03051757812365977693, 0.03076171874864941369, 0.03124999999862868721, 0.03515624999846280602, 0.03906249999829693176, 0.04003906249825545105, 0.04052734374823471764, 0.04077148437322434399, 0.04083251952947174884, 0.04089355468571915370, 0.04101562499821394953, 0.04296874999813071055, 0.04687499999796423261, 0.05468749999763128367, 0.05859374999746481266, 0.06054687499738157369, 0.06103515624736076395, 0.06127929687235035561, 0.06152343749733995421, 0.06249999999729832778, 0.07812499999663236050, 0.08007812499654912153, 0.08105468749650750204, 0.08154296874648669924, 0.08166503905898149507, 0.08178710937147629090, 0.08203124999646588256, 0.08593749999629947400, 0.09374999999596665690, 0.1093749999953010227, 0.1171874999949682056, 0.1210937499948017831, 0.1220703124947601914, 0.1223144531197498108, 0.1224365234322446344, 0.1224975585884920670, 0.1225585937447394858, 0.1230468749947207785, 0.1249999999946464768, 0.1406249999940512030, 0.1562499999934559569, 0.1601562499933071315, 0.1621093749932327466, 0.1630859374931955263, 0.1632080078056908912, 0.1632385253838147254, 0.1632690429619385319, 0.1633300781181862837, 0.1635742187431770134, 0.1640624999931583616, 0.1718749999928589345, 0.1874999999922599414, 0.2187499999910620663, 0.2499999999898641634, 0.2812499999886662883, 0.2851562499885165192, 0.2856445312384978119, 0.2857055663947454249, 0.2857666015509930380, 0.2858886718634883195, 0.2861328124884786606, 0.2871093749884404134, 0.2890624999883638080, 0.2968749999880570534, 0.3124999999874435996, 0.3749999999849897292, 0.4374999999825360253, 0.4687499999813090623, 0.4843749999806956086, 0.4921874999803889650, 0.4960937499802356987, 0.4980468749801592043, 0.4990234374801209571, 0.4995117187301018058, 0.4997558593550920913, 0.4998779296675873729, 0.4999389648238350414, 0.4999694824019588757, 0.4999847411910207651, 0.4999999999800827100, 0.5156249999794596528, 0.5312499999788367067, 0.5468749999782136495, 0.5546874999779023430, 0.5585937499777469117, 0.5605468749776695292, 0.5615234374776307824, 0.5620117187276114645, 0.5622558593526023607, 0.5623779296650976978, 0.5624389648213454773, 0.5624694823994693671, 0.5624847411885313120, 0.5624923705830626730, 0.5624999999775941451, 0.5703124999778719229, 0.5742187499780107007, 0.5761718749780803117, 0.5771484374781150617, 0.5776367187281322702, 0.5778808593531409299, 0.5780029296656451487, 0.5780639648218971471, 0.5780944824000230353, 0.5781097411890862015, 0.5781173705836177845, 0.5781249999781493676, 0.5800781249782447357, 0.5810546874782923643, 0.5815429687283162341, 0.5817871093533281135, 0.5819091796658339977, 0.5819702148220871063, 0.5820007324002134386, 0.5820159911892766047, 0.5820236205838081878, 0.5820312499783397708, 0.5830078124783841798, 0.5834960937284063842, 0.5837402343534173754, 0.5838623046659229265, 0.5839233398221758131, 0.5839538574003022564, 0.5839691161893653115, 0.5839767455838968946, 0.5839843749784284777, 0.5849609374784705551, 0.5854492187284916493, 0.5856933593535021965, 0.5858154296660074145, 0.5858764648222599680, 0.5859069824003863003, 0.5859222411894494664, 0.5859298705839809385, 0.5859336852812467855, 0.5859355926298795980, 0.5859374999785124105, 0.5878906249786036708, 0.5898437499786948202, 0.5917968749787859695, 0.5927734374788314886, 0.5932617187288543592, 0.5935058593538656835, 0.5936279296663713456, 0.5936889648226242322, 0.5937194824007505645, 0.5937347411898138416, 0.5937423705843454247, 0.5937499999788770078, 0.5957031249789628280, 0.5976562499790486482, 0.5996093749791345795, 0.6005859374791774341, 0.6010742187291988614, 0.6013183593542096306, 0.6014404296667150707, 0.6015014648229677352, 0.6015319824010940675, 0.6015472411901572336, 0.6015548705846888167, 0.6015624999792203997, 0.6035156249793174332, 0.6044921874793659500, 0.6049804687293902639, 0.6052246093544023653, 0.6053466796669084715, 0.6054077148231615801, 0.6054382324012880234, 0.6054534911903513006, 0.6054611205848829947, 0.6054687499794146888, 0.6074218749795251560, 0.6083984374795803340, 0.6088867187296079786, 0.6091308593546217454, 0.6092529296671286287, 0.6093139648233820704, 0.6093444824015088468, 0.6093597411905722350, 0.6093749999796355121, 0.6113281249797379857, 0.6123046874797891670, 0.6127929687298147021, 0.6130371093548275807, 0.6131591796673340200, 0.6132202148235871286, 0.6132507324017136829, 0.6132659911907769601, 0.6132736205853086542, 0.6132812499798403483, 0.6152343749799318307, 0.6162109374799775718, 0.6166992187300004424, 0.6169433593550117667, 0.6170654296675175399, 0.6171264648237704264, 0.6171569824018967587, 0.6171722411909600359, 0.6171874999800233130, 0.6210937499802106077, 0.6230468749803044215, 0.6240234374803512729, 0.6245117187303745876, 0.6247558593553863560, 0.6248779296678921291, 0.6249389648241451267, 0.6249999999803982353, 0.6328124999807902551, 0.6406249999811823859, 0.6484374999815745166, 0.6523437499817704710, 0.6542968749818685037, 0.6552734374819175756, 0.6557617187319422225, 0.6560058593569544350, 0.6561279296694605412, 0.6561889648257135388, 0.6562194824038400931, 0.6562499999819665364, 0.6718749999827752228, 0.6796874999831795661, 0.6835937499833818487, 0.6855468749834829900, 0.6865234374835335052, 0.6870117187335589293, 0.6872558593585716968, 0.6873779296710780251, 0.6874389648273313558, 0.6874694824054579101, 0.6874999999835845754, 0.7187499999852486887, 0.7343749999860806899, 0.7421874999864966904, 0.7460937499867046352, 0.7480468749868086631, 0.7490234374868607325, 0.7495117187368869338, 0.7497558593618999234, 0.7498779296744064737, 0.7499999999869129130, 0.7812499999885803570, 0.8124999999902479120, 0.8437499999919154670, 0.8593749999927492444, 0.8671874999931661332, 0.8710937499933745221, 0.8730468749934786610, 0.8740234374935308415, 0.8745117187435570427, 0.8747558593685700323, 0.8748779296810765826, 0.8749389648373300243, 0.8749694824154565787, 0.8749999999935830219, 0.9062499999951872942, 0.9374999999967915665, 0.9687499999983957277, 1.000000000000000000 ),
 .UNSPECIFIED. ) ;
#65794 = EDGE_CURVE ( 'NONE', #72311, #22326, #100899, .T. ) ;
#65795 = CYLINDRICAL_SURFACE ( 'NONE', #97431, 7.499999999992679633 ) ;
#65796 = ORIENTED_EDGE ( 'NONE', *, *, #86440, .F. ) ;
#65797 = CARTESIAN_POINT ( 'NONE',  ( 61.32899078381009161, -49.91179946772914633, 80.89050486367615633 ) ) ;
#65798 = CARTESIAN_POINT ( 'NONE',  ( 9.498520115305538525, -51.35937410768142541, 30.13282173121349317 ) ) ;
#65799 = CARTESIAN_POINT ( 'NONE',  ( -8.772759641400078578, -5.000000000000000888, -16.83842667730707277 ) ) ;
#65801 = CARTESIAN_POINT ( 'NONE',  ( 15.75384615384615294, 1.411358822780289120E-15, 0.000000000000000000 ) ) ;
#65800 = CARTESIAN_POINT ( 'NONE',  ( -76.24902598065085613, -29.99999999995297273, 167.9309681516145361 ) ) ;
#65802 = CARTESIAN_POINT ( 'NONE',  ( -39.48063050920401906, 328.7742392842140475, 18.18155475394569365 ) ) ;
#65803 = CARTESIAN_POINT ( 'NONE',  ( 0.000000000000000000, 0.000000000000000000, 0.000000000000000000 ) ) ;
#65804 = CARTESIAN_POINT ( 'NONE',  ( 8.929771841637641927, 3.851859888774471706E-31, 5.000000000000001776 ) ) ;
#65805 = CARTESIAN_POINT ( 'NONE',  ( -1.469576158976823947E-15, -29.37499999999999645, 8.000000000000000000 ) ) ;
#65806 = VECTOR ( 'NONE', #97865, 1000.000000000000000 ) ;
#65807 = DIRECTION ( 'NONE',  ( 0.5735764363510466035, -0.8191520442889914655, 1.003171929053524500E-16 ) ) ;
#65808 = ORIENTED_EDGE ( 'NONE', *, *, #25322, .F. ) ;
#65809 = CARTESIAN_POINT ( 'NONE',  ( 84.78850302438281972, -28.94140559783478395, 170.4382928173611447 ) ) ;
#65810 = DIRECTION ( 'NONE',  ( 0.000000000000000000, -1.000000000000000000, 0.000000000000000000 ) ) ;
#65811 = PLANE ( 'NONE',  #40227 ) ;
#65812 = ORIENTED_EDGE ( 'NONE', *, *, #58723, .F. ) ;
#65813 = DIRECTION ( 'NONE',  ( 0.000000000000000000, -1.000000000000000000, 0.000000000000000000 ) ) ;
#65814 = DIRECTION ( 'NONE',  ( -1.000000000000000000, 0.000000000000000000, 0.000000000000000000 ) ) ;
#65815 = FACE_OUTER_BOUND ( 'NONE', #65406, .T. ) ;
#65816 = CARTESIAN_POINT ( 'NONE',  ( -1.590954574004046274, 50.00000000000000711, -73.00000000000002842 ) ) ;
#65817 = CARTESIAN_POINT ( 'NONE',  ( -43.48668509622026335, 41.44578431664083951, -50.71569214715880491 ) ) ;
#65818 = CARTESIAN_POINT ( 'NONE',  ( -28.46836751014381051, 13.00004364346765762, -40.55018863591808298 ) ) ;
#65819 = ADVANCED_FACE ( 'NONE', ( #58025 ), #90599, .T. ) ;
#65820 =( NAMED_UNIT ( * ) PLANE_ANGLE_UNIT ( ) SI_UNIT ( $, .RADIAN. ) );
#65821 = CARTESIAN_POINT ( 'NONE',  ( 6.826581433397953980, -2.695947255479825166, -6.331032031596339316 ) ) ;
#65822 = CARTESIAN_POINT ( 'NONE',  ( -4.999999999999993783, -46.27603786271895814, 102.2532056551910387 ) ) ;
#65823 = ADVANCED_FACE ( 'NONE', ( #49939, #7171 ), #22343, .T. ) ;
#65825 = CARTESIAN_POINT ( 'NONE',  ( -15.27610976668421650, 22.61015309965470976, 2.822488379715081486 ) ) ;
#65824 = CARTESIAN_POINT ( 'NONE',  ( -5.442530501874275117, -18.69205451546762475, 35.10612107872960053 ) ) ;
#65826 = CARTESIAN_POINT ( 'NONE',  ( -5.082755093536325042, -15.59375000204838635, -5.082755093536325930 ) ) ;
#65827 = CARTESIAN_POINT ( 'NONE',  ( -28.43253669899745617, 17.35855320307313221, -40.99008157358994708 ) ) ;
#65828 = FILL_AREA_STYLE_COLOUR ( '', #65569 ) ;
#65829 = VERTEX_POINT ( 'NONE', #55706 ) ;
#65830 = AXIS2_PLACEMENT_3D ( 'NONE', #56101, #30832, #14064 ) ;
#65831 = CARTESIAN_POINT ( 'NONE',  ( -19.03324747453609689, 49.57630456594476698, 61.85387798835519391 ) ) ;
#65832 = DIRECTION ( 'NONE',  ( 0.000000000000000000, 1.000000000000000000, 0.000000000000000000 ) ) ;
#65833 = PRESENTATION_LAYER_ASSIGNMENT (  '', '', ( #57193 ) ) ;
#65834 = CARTESIAN_POINT ( 'NONE',  ( 36.74148664940359765, 437.9559008978175143, 4.252305828303467372 ) ) ;
#65835 = CARTESIAN_POINT ( 'NONE',  ( -7.141975279369632723, -4.999999999999062972, -70.98863559356212249 ) ) ;
#65837 = CARTESIAN_POINT ( 'NONE',  ( 64.11807478814075978, -21.77010348245833526, -21.74840280664149716 ) ) ;
#65836 = DIRECTION ( 'NONE',  ( -1.000000000000000000, -0.000000000000000000, -0.000000000000000000 ) ) ;
#65838 = ADVANCED_FACE ( 'NONE', ( #79479 ), #68274, .T. ) ;
#65839 = ORIENTED_EDGE ( 'NONE', *, *, #56454, .F. ) ;
#65840 = CARTESIAN_POINT ( 'NONE',  ( -4.903871675326606727, -87.02085807301496345, -3.461400506969855684 ) ) ;
#65841 = CARTESIAN_POINT ( 'NONE',  ( -5.207109540145846260, 52.09997922571544393, 6.031152949374557259 ) ) ;
#65842 = ORIENTED_EDGE ( 'NONE', *, *, #69210, .F. ) ;
#65843 = ADVANCED_FACE ( 'NONE', ( #38002 ), #96738, .T. ) ;
#65844 = STYLED_ITEM ( 'NONE', ( #50033 ), #74710 ) ;
#65845 = B_SPLINE_CURVE_WITH_KNOTS ( 'NONE', 3,
 ( #68051, #58912, #59993, #19019 ),
 .UNSPECIFIED., .F., .F.,
 ( 4, 4 ),
 ( 3.469446951953614189E-18, 0.001748759895715563256 ),
 .UNSPECIFIED. ) ;
#65846 = CARTESIAN_POINT ( 'NONE',  ( -33.48012358427683921, 40.64846154899619535, -61.62971572559018796 ) ) ;
#65847 = CARTESIAN_POINT ( 'NONE',  ( -103.5524900213308683, -60.00000000000001421, 101.8145487315525770 ) ) ;
#65848 = DIRECTION ( 'NONE',  ( 0.000000000000000000, 0.000000000000000000, -1.000000000000000000 ) ) ;
#65849 = CARTESIAN_POINT ( 'NONE',  ( 43.52075891743746894, 484.7805561108181109, 4.063293749111048569 ) ) ;
#65850 = FACE_OUTER_BOUND ( 'NONE', #106749, .T. ) ;
#65852 = CARTESIAN_POINT ( 'NONE',  ( -32.85550102723723853, 465.7063702548733204, 11.00086562319487626 ) ) ;
#65851 =( REPRESENTATION_RELATIONSHIP ('NONE','NONE', #69581, #49395 ) REPRESENTATION_RELATIONSHIP_WITH_TRANSFORMATION ( #99916 )SHAPE_REPRESENTATION_RELATIONSHIP( ) );
#65854 = CARTESIAN_POINT ( 'NONE',  ( 5.290067270632321517, 52.08006895350504095, 6.031152949374479100 ) ) ;
#65853 = CARTESIAN_POINT ( 'NONE',  ( -6.145467200819251019, -5.000000000000002665, -77.00333157709852117 ) ) ;
#65855 = CARTESIAN_POINT ( 'NONE',  ( -83.53549352640362713, -39.47137158060975537, 174.7280617345839460 ) ) ;
#65856 = VERTEX_POINT ( 'NONE', #63846 ) ;
#65857 = PRESENTATION_STYLE_ASSIGNMENT (( #7601 ) ) ;
#65858 = EDGE_LOOP ( 'NONE', ( #67986, #61502, #32785, #64774, #93143 ) ) ;
#65859 = ORIENTED_EDGE ( 'NONE', *, *, #10204, .T. ) ;
#65860 = LINE ( 'NONE', #8683, #40491 ) ;
#65861 = ORIENTED_EDGE ( 'NONE', *, *, #910, .F. ) ;
#65862 =( GEOMETRIC_REPRESENTATION_CONTEXT ( 3 ) GLOBAL_UNCERTAINTY_ASSIGNED_CONTEXT ( ( #27011 ) ) GLOBAL_UNIT_ASSIGNED_CONTEXT ( ( #16054, #31736, #24709 ) ) REPRESENTATION_CONTEXT ( 'NONE', 'WORKASPACE' ) );
#65863 = CARTESIAN_POINT ( 'NONE',  ( 0.000000000000000000, 0.000000000000000000, 0.000000000000000000 ) ) ;
#65864 = FACE_BOUND ( 'NONE', #76768, .T. ) ;
#65865 = LINE ( 'NONE', #98745, #5909 ) ;
#65866 = CARTESIAN_POINT ( 'NONE',  ( -7.344361273354514275, -62.55439469411476239, -3.175733139645589898 ) ) ;
#65867 = AXIS2_PLACEMENT_3D ( 'NONE', #1691, #100396, #36774 ) ;
#65868 = DIRECTION ( 'NONE',  ( -1.000000000000000000, -1.224606353822377258E-16, -0.000000000000000000 ) ) ;
#65869 = CARTESIAN_POINT ( 'NONE',  ( -13.05378511524491536, -5.000000000000000000, -85.14608070245081706 ) ) ;
#65870 = CARTESIAN_POINT ( 'NONE',  ( 0.08224679563971280805, 6.145890662064650733, -5.355005115540897087 ) ) ;
#65871 = CARTESIAN_POINT ( 'NONE',  ( 106.7878191156923293, -14.21045842199435150, 165.8358245669431597 ) ) ;
#65872 = EDGE_CURVE ( 'NONE', #90932, #105278, #88116, .T. ) ;
#65873 = CARTESIAN_POINT ( 'NONE',  ( -114.2223820868815380, -59.99999999999997868, 162.1253058113985048 ) ) ;
#65874 = CARTESIAN_POINT ( 'NONE',  ( -64.00514404253527800, -29.05590673187525041, 77.96790845986099328 ) ) ;
#65875 = ORIENTED_EDGE ( 'NONE', *, *, #76707, .F. ) ;
#65876 = CARTESIAN_POINT ( 'NONE',  ( -43.70013511063233835, 484.4793062204365128, 2.436320700791212879 ) ) ;
#65877 = CARTESIAN_POINT ( 'NONE',  ( 109.6214308269799176, -59.99999999999999289, 124.0322540993774396 ) ) ;
#65878 = ORIENTED_EDGE ( 'NONE', *, *, #77865, .T. ) ;
#65879 = CARTESIAN_POINT ( 'NONE',  ( 1.023254973492224051, -60.35900083628900603, 33.94948343231720855 ) ) ;
#65880 = CARTESIAN_POINT ( 'NONE',  ( 2.977408999572652260, -10.81250000204838457, 7.188101187500000044 ) ) ;
#65881 = CARTESIAN_POINT ( 'NONE',  ( -8.641101172624390259, -5.000000000000000888, -72.37542516940096959 ) ) ;
#65882 = VERTEX_POINT ( 'NONE', #96214 ) ;
#65883 = CARTESIAN_POINT ( 'NONE',  ( 6.252586356923180766, -30.00000000000000000, 3.576699445452887094 ) ) ;
#65884 = ORIENTED_EDGE ( 'NONE', *, *, #28162, .F. ) ;
#65885 = DIRECTION ( 'NONE',  ( -1.000000000000000000, -0.000000000000000000, -0.000000000000000000 ) ) ;
#65886 = CARTESIAN_POINT ( 'NONE',  ( -94.37463078541230743, -59.99999999999994316, 202.5629720368760616 ) ) ;
#65887 = CARTESIAN_POINT ( 'NONE',  ( 2.977408999572650927, -22.25000000204839168, -7.188101187500001821 ) ) ;
#65888 = DIRECTION ( 'NONE',  ( -0.000000000000000000, -1.000000000000000000, -0.000000000000000000 ) ) ;
#65889 = CARTESIAN_POINT ( 'NONE',  ( -35.69355135759316511, 463.3819780847709922, 19.97922827668330470 ) ) ;
#65890 = DIRECTION ( 'NONE',  ( -1.000000000000000000, -0.000000000000000000, -0.000000000000000000 ) ) ;
#65891 = LINE ( 'NONE', #75028, #18498 ) ;
#65892 = SURFACE_SIDE_STYLE ('',( #32496 ) ) ;
#65893 = CARTESIAN_POINT ( 'NONE',  ( 15.43204163116762118, -5.423745131301086708, 13.99747994630663861 ) ) ;
#65894 = CARTESIAN_POINT ( 'NONE',  ( -23.38404382908472456, 27.34872606290121055, 33.19783523858075824 ) ) ;
#65895 = B_SPLINE_CURVE_WITH_KNOTS ( 'NONE', 3,
 ( #6889, #39810, #97480, #48404, #81294, #69272, #3460, #21271, #102145, #20761, #28298, #37989, #61723, #44996, #36404, #101626, #29363, #76800, #87049, #5053 ),
 .UNSPECIFIED., .F., .F.,
 ( 4, 2, 2, 2, 2, 2, 2, 2, 2, 4 ),
 ( 0.0009508909574247000930, 0.001455760884198634402, 0.001960630810972568278, 0.002465500737746502587, 0.002970370664520436896, 0.003475240591294370771, 0.003980110518068305514, 0.004232545481455271368, 0.004484980444842237221, 0.004989850371616175867 ),
 .UNSPECIFIED. ) ;
#65896 = ADVANCED_FACE ( 'NONE', ( #78947 ), #64888, .F. ) ;
#65897 = DIRECTION ( 'NONE',  ( 0.000000000000000000, -1.000000000000000000, 0.000000000000000000 ) ) ;
#65898 = CARTESIAN_POINT ( 'NONE',  ( -32.78616274675678710, -32.55822851310848876, 32.94897349368736172 ) ) ;
#65899 = CARTESIAN_POINT ( 'NONE',  ( -3.473068986402788383, -49.15491390339877142, 103.7454523020563499 ) ) ;
#65900 = CARTESIAN_POINT ( 'NONE',  ( 39.33871441765692367, -42.97318751769551426, 38.91929416661629659 ) ) ;
#65901 = DIRECTION ( 'NONE',  ( -1.000000000000000000, -0.000000000000000000, -0.000000000000000000 ) ) ;
#65902 = VERTEX_POINT ( 'NONE', #5590 ) ;
#65903 = EDGE_CURVE ( 'NONE', #6434, #102890, #39025, .T. ) ;
#65904 = CARTESIAN_POINT ( 'NONE',  ( -7.212408192734267587, 87.01517089320370246, -3.465038817813880012 ) ) ;
#65905 = EDGE_CURVE ( 'NONE', #59491, #48619, #41389, .T. ) ;
#65906 = CARTESIAN_POINT ( 'NONE',  ( -78.35849824112422368, -38.61718390855864413, 189.2875896208779523 ) ) ;
#65907 = ORIENTED_EDGE ( 'NONE', *, *, #72594, .T. ) ;
#65909 = CARTESIAN_POINT ( 'NONE',  ( -43.26971690803510029, 435.9072580013543643, 8.039630127097252554 ) ) ;
#65908 = DIRECTION ( 'NONE',  ( 0.000000000000000000, 0.000000000000000000, 1.000000000000000000 ) ) ;
#65910 = CARTESIAN_POINT ( 'NONE',  ( -12.27768440095290536, 5.728514393148000927, 8.474169079004697736 ) ) ;
#65911 = CARTESIAN_POINT ( 'NONE',  ( -48.76867190053926748, 8.289666503167254064, -16.61714170248003342 ) ) ;
#65912 = CARTESIAN_POINT ( 'NONE',  ( -7.109733192396788581, 41.69026681596732686, -59.69141549319190432 ) ) ;
#65913 = CARTESIAN_POINT ( 'NONE',  ( 6.836424187873526570, 40.92324844684119967, -70.97025588743883873 ) ) ;
#65914 = DIRECTION ( 'NONE',  ( -1.000000000000000000, -1.224606353822377258E-16, -0.000000000000000000 ) ) ;
#65916 = CARTESIAN_POINT ( 'NONE',  ( 5.727189096784633726, -88.57869875248739788, -1.806430436190347377 ) ) ;
#65915 = VECTOR ( 'NONE', #20040, 1000.000000000000000 ) ;
#65917 = CARTESIAN_POINT ( 'NONE',  ( 45.11650669486618881, 1.474610560812782335E-15, 0.000000000000000000 ) ) ;
#65918 = EDGE_CURVE ( 'NONE', #11369, #93666, #61485, .T. ) ;
#65919 = CARTESIAN_POINT ( 'NONE',  ( 106.0576547319784169, -60.00000000000000000, 116.7836318968619764 ) ) ;
#65921 = DIRECTION ( 'NONE',  ( -0.5735764363510494901, -0.8191520442889894671, 0.000000000000000000 ) ) ;
#65920 = AXIS2_PLACEMENT_3D ( 'NONE', #25260, #24724, #2004 ) ;
#65922 = EDGE_CURVE ( 'NONE', #21504, #23394, #66733, .T. ) ;
#65923 = CIRCLE ( 'NONE', #19464, 4.000000000000000000 ) ;
#65924 = FACE_OUTER_BOUND ( 'NONE', #80721, .T. ) ;
#65925 = ORIENTED_EDGE ( 'NONE', *, *, #55675, .F. ) ;
#65926 = CARTESIAN_POINT ( 'NONE',  ( -100.0418167452864537, -30.00000000000002132, 185.4816374921457225 ) ) ;
#65927 = ORIENTED_EDGE ( 'NONE', *, *, #68911, .T. ) ;
#65928 = DIRECTION ( 'NONE',  ( 0.000000000000000000, 0.000000000000000000, 1.000000000000000000 ) ) ;
#65929 = CARTESIAN_POINT ( 'NONE',  ( -7.500000000000006217, 152.0000000000000000, 0.000000000000000000 ) ) ;
#65930 = CARTESIAN_POINT ( 'NONE',  ( 9.518114776852277359, 142.5485589766093710, 0.000000000000000000 ) ) ;
#65931 = CARTESIAN_POINT ( 'NONE',  ( 30.17572460893185493, 323.8315592358100048, 14.85820515551728782 ) ) ;
#65932 = CARTESIAN_POINT ( 'NONE',  ( -6.231493956936421164, 147.8264543773111654, 0.000000000000000000 ) ) ;
#65933 = CARTESIAN_POINT ( 'NONE',  ( 5.082755093536324154, -24.21875000204838813, 5.082755093536326818 ) ) ;
#65934 = CARTESIAN_POINT ( 'NONE',  ( 6.162888688655344893, -3.752776749732565253, 6.499999999999999112 ) ) ;
#65935 = CARTESIAN_POINT ( 'NONE',  ( 7.245483083000110014, 40.92674623657338628, -70.53853222405051326 ) ) ;
#65936 = EDGE_LOOP ( 'NONE', ( #20843, #38408, #85109, #69874 ) ) ;
#65938 = ORIENTED_EDGE ( 'NONE', *, *, #95898, .F. ) ;
#65937 = CARTESIAN_POINT ( 'NONE',  ( 39.83349330513380693, 1.593028355512270567E-15, 0.000000000000000000 ) ) ;
#65939 = CARTESIAN_POINT ( 'NONE',  ( 82.46808697483727713, -25.62292026212021057, 146.0453604029042651 ) ) ;
#65940 = DIRECTION ( 'NONE',  ( 0.000000000000000000, 0.000000000000000000, -1.000000000000000000 ) ) ;
#65941 = ORIENTED_EDGE ( 'NONE', *, *, #61209, .F. ) ;
#65942 = PRESENTATION_STYLE_ASSIGNMENT (( #97764 ) ) ;
#65943 = CARTESIAN_POINT ( 'NONE',  ( -14.37299415487917109, 2.005565780251463259, -4.271091604483703286 ) ) ;
#65944 = CARTESIAN_POINT ( 'NONE',  ( -5.082755093536326818, -10.71875000204838457, 5.082755093536325042 ) ) ;
#65945 = CARTESIAN_POINT ( 'NONE',  ( 7.999912353029506207, 26.00017529396907179, -0.2691822806794995637 ) ) ;
#65946 = CYLINDRICAL_SURFACE ( 'NONE', #97245, 4.000000000000001776 ) ;
#65947 =( BOUNDED_CURVE ( )  B_SPLINE_CURVE ( 2, ( #99874, #33569, #49184, #15768, #40578, #58906, #90194, #17387, #48650 ),
 .UNSPECIFIED., .F., .F. ) 
 B_SPLINE_CURVE_WITH_KNOTS ( ( 3, 2, 2, 2, 3 ),
 ( 0.3088235294117646634, 0.3161764705882352255, 0.3235294117647058432, 0.3308823529411764053, 0.3382352941176470229 ),
 .UNSPECIFIED. ) 
 CURVE ( )  GEOMETRIC_REPRESENTATION_ITEM ( )  RATIONAL_B_SPLINE_CURVE ( ( 1.000000000000000666, 0.9238795325112861834, 1.000000000000000000, 0.9238795325112867385, 1.000000000000000000, 0.9238795325112867385, 1.000000000000000000, 0.9238795325112872936, 0.9999999999999994449 ) ) 
 REPRESENTATION_ITEM ( '' )  );
#65948 = CARTESIAN_POINT ( 'NONE',  ( -31.72650767699502339, 329.8019043314008059, 16.51996880882650132 ) ) ;
#65949 = ORIENTED_EDGE ( 'NONE', *, *, #100237, .F. ) ;
#65950 = PRESENTATION_LAYER_ASSIGNMENT (  '', '', ( #52162 ) ) ;
#65951 = CARTESIAN_POINT ( 'NONE',  ( 16.36650669486618881, -3.999999999999998224, 0.000000000000000000 ) ) ;
#65952 = LINE ( 'NONE', #73495, #39259 ) ;
#65953 = CARTESIAN_POINT ( 'NONE',  ( 86.31548406937289997, -57.42050482052351157, 193.3910388938697054 ) ) ;
#65954 = EDGE_CURVE ( 'NONE', #83820, #9879, #90667, .T. ) ;
#65955 = CARTESIAN_POINT ( 'NONE',  ( 0.000000000000000000, 0.000000000000000000, -5.710657142857142432 ) ) ;
#65956 = CARTESIAN_POINT ( 'NONE',  ( 7.188101187500001821, -31.06250000204838813, -2.977408999572650483 ) ) ;
#65957 = CARTESIAN_POINT ( 'NONE',  ( 36.55251058255094421, -36.29168913791675521, 45.74408343238721386 ) ) ;
#65958 =( LENGTH_UNIT ( ) NAMED_UNIT ( * ) SI_UNIT ( .MILLI., .METRE. ) );
#65959 = CARTESIAN_POINT ( 'NONE',  ( 7.483202312393204991, 52.00295125296706544, 3.437726841112358045 ) ) ;
#65960 = CARTESIAN_POINT ( 'NONE',  ( 35.54116392775497957, 439.5951022651032076, 24.01691468013297737 ) ) ;
#65961 = APPLICATION_PROTOCOL_DEFINITION ( 'draft international standard', 'automotive_design', 1998, #21797 ) ;
#65962 = CARTESIAN_POINT ( 'NONE',  ( 48.49185632690715408, 10.49696353563009410, 14.43858684427206640 ) ) ;
#65963 = ORIENTED_EDGE ( 'NONE', *, *, #16598, .F. ) ;
#65964 = CARTESIAN_POINT ( 'NONE',  ( 0.6460500001699683859, 43.23245175272156615, 18.58310964118233954 ) ) ;
#65965 = CARTESIAN_POINT ( 'NONE',  ( -17.49999999999997513, 45.00000000000000711, 100.0000000000000000 ) ) ;
#65966 = PRESENTATION_STYLE_ASSIGNMENT (( #33101 ) ) ;
#65967 = FACE_OUTER_BOUND ( 'NONE', #62609, .T. ) ;
#65968 = ORIENTED_EDGE ( 'NONE', *, *, #81751, .T. ) ;
#65969 = PRESENTATION_STYLE_ASSIGNMENT (( #8259 ) ) ;
#65970 = CARTESIAN_POINT ( 'NONE',  ( 107.8654790820937421, -57.67125328048376787, 115.6101856694811687 ) ) ;
#65971 = ADVANCED_FACE ( 'NONE', ( #89424 ), #23556, .T. ) ;
#65972 = CARTESIAN_POINT ( 'NONE',  ( 37.54237687664871004, 463.5961191363963962, 19.55587387186555048 ) ) ;
#65973 = DIRECTION ( 'NONE',  ( 0.000000000000000000, 1.224646799147352468E-16, 1.000000000000000000 ) ) ;
#65974 = FACE_OUTER_BOUND ( 'NONE', #85256, .T. ) ;
#65975 = CARTESIAN_POINT ( 'NONE',  ( 5.299999999999999822, 7.960204194457794491E-16, -6.499999999999999112 ) ) ;
#65976 = B_SPLINE_CURVE_WITH_KNOTS ( 'NONE', 3,
 ( #81672, #6202, #105960, #24033, #31069, #16429, #49310, #82221, #6745, #96315, #72541, #22443, #55284, #63947, #80097, #39141, #56338, #104929 ),
 .UNSPECIFIED., .F., .F.,
 ( 4, 2, 2, 2, 2, 2, 2, 2, 4 ),
 ( 0.5000000000000000000, 0.5625000000000000000, 0.6250000000000000000, 0.6875000000000000000, 0.7500000000000000000, 0.8125000000000000000, 0.8750000000000000000, 0.9375000000000000000, 1.000000000000000000 ),
 .UNSPECIFIED. ) ;
#65977 = CARTESIAN_POINT ( 'NONE',  ( -77.55662926993193196, -59.99999999999999289, 191.8679431246135891 ) ) ;
#65978 = CIRCLE ( 'NONE', #19541, 5.000000000000002665 ) ;
#65979 = DIRECTION ( 'NONE',  ( 0.000000000000000000, 0.000000000000000000, 1.000000000000000000 ) ) ;
#65980 =( LENGTH_UNIT ( ) NAMED_UNIT ( * ) SI_UNIT ( .MILLI., .METRE. ) );
#65981 = ORIENTED_EDGE ( 'NONE', *, *, #54490, .F. ) ;
#65982 = EDGE_CURVE ( 'NONE', #45532, #90027, #75180, .T. ) ;
#65983 = CARTESIAN_POINT ( 'NONE',  ( -42.09210974227526947, 317.4093497706929270, -4.557617623460385126 ) ) ;
#65984 = CARTESIAN_POINT ( 'NONE',  ( -86.02960737348817588, -28.37172899385929625, 182.1171066242029326 ) ) ;
#65985 = CIRCLE ( 'NONE', #10847, 4.250000000000000000 ) ;
#65986 = ORIENTED_EDGE ( 'NONE', *, *, #36887, .F. ) ;
#65987 = CARTESIAN_POINT ( 'NONE',  ( 20.24579557674105246, 304.8297271373347144, -10.00469232190991598 ) ) ;
#65988 = VECTOR ( 'NONE', #24097, 1000.000000000000000 ) ;
#65989 = ORIENTED_EDGE ( 'NONE', *, *, #80825, .T. ) ;
#65990 = DIRECTION ( 'NONE',  ( -1.000000000000000000, -1.224606353822377258E-16, -0.000000000000000000 ) ) ;
#65991 = CARTESIAN_POINT ( 'NONE',  ( -4.551587301587304957, -1.200583151104947843, 104.4018401814738155 ) ) ;
#65992 = CARTESIAN_POINT ( 'NONE',  ( -83.25973548172940752, -37.79105956807652689, -6.268593792199344428 ) ) ;
#65993 = CARTESIAN_POINT ( 'NONE',  ( 23.99113157947469332, 50.00000000000000000, -74.11764705882353610 ) ) ;
#65994 = DIRECTION ( 'NONE',  ( -1.000000000000000000, -1.224606353822377258E-16, -0.000000000000000000 ) ) ;
#65995 = VERTEX_POINT ( 'NONE', #14973 ) ;
#65996 =( GEOMETRIC_REPRESENTATION_CONTEXT ( 3 ) GLOBAL_UNCERTAINTY_ASSIGNED_CONTEXT ( ( #74109 ) ) GLOBAL_UNIT_ASSIGNED_CONTEXT ( ( #35582, #64095, #45248 ) ) REPRESENTATION_CONTEXT ( 'NONE', 'WORKASPACE' ) );
#65997 = CARTESIAN_POINT ( 'NONE',  ( 6.683837171061806082, 7.911893696991936231, -4.595687358162529387E-16 ) ) ;
#65998 = CARTESIAN_POINT ( 'NONE',  ( 5.363597346073513350, 41.33266196706048845, -58.39526881795627844 ) ) ;
#65999 = CARTESIAN_POINT ( 'NONE',  ( 4.453875240780039491, -1.734723475976807094E-15, 16.57301948837323380 ) ) ;
#66000 = CARTESIAN_POINT ( 'NONE',  ( -34.53029562237181693, 437.2884171348779887, 5.234332900502464803 ) ) ;
#66001 = CARTESIAN_POINT ( 'NONE',  ( -2.727034095388735757, -14.21045842199435860, -37.36840973699904822 ) ) ;
#66002 = CARTESIAN_POINT ( 'NONE',  ( -78.51742362413880016, -36.02766478407949080, 134.0155194058749260 ) ) ;
#66003 = ORIENTED_EDGE ( 'NONE', *, *, #11431, .T. ) ;
#66004 = CARTESIAN_POINT ( 'NONE',  ( 73.20367453073632191, -59.99999999999985789, 185.6239686060362146 ) ) ;
#66005 = DIRECTION ( 'NONE',  ( 0.000000000000000000, -1.000000000000000000, 0.000000000000000000 ) ) ;
#66006 = CARTESIAN_POINT ( 'NONE',  ( 94.29131450443634321, -57.67246088413772043, 24.29571120338738055 ) ) ;
#66007 = ORIENTED_EDGE ( 'NONE', *, *, #63924, .T. ) ;
#66008 = CARTESIAN_POINT ( 'NONE',  ( -43.00000000000000000, 461.6622277975412771, 10.18145404766302065 ) ) ;
#66009 = PLANE ( 'NONE',  #4662 ) ;
#66010 = ORIENTED_EDGE ( 'NONE', *, *, #62607, .T. ) ;
#66011 = CARTESIAN_POINT ( 'NONE',  ( 1.795343932601242143, 14.26861286782568072, -6.770400604484294149 ) ) ;
#66012 = CIRCLE ( 'NONE', #67796, 5.000000000000001776 ) ;
#66013 = CARTESIAN_POINT ( 'NONE',  ( 17.50000000000002842, 50.00000000000000000, 100.0000000000000000 ) ) ;
#66014 = LINE ( 'NONE', #24005, #81109 ) ;
#66015 = CARTESIAN_POINT ( 'NONE',  ( -7.188101187500001821, -21.50000000204839168, -2.977408999572651371 ) ) ;
#66016 = DIRECTION ( 'NONE',  ( -0.5735764363510459374, -0.8191520442889919096, 0.000000000000000000 ) ) ;
#66017 = CARTESIAN_POINT ( 'NONE',  ( 9.698972129396508990, 81.82370287258061126, -2.445345647270320999 ) ) ;
#66018 = DIRECTION ( 'NONE',  ( 0.000000000000000000, -1.000000000000000000, -0.000000000000000000 ) ) ;
#66019 = FACE_BOUND ( 'NONE', #15902, .T. ) ;
#66020 = CARTESIAN_POINT ( 'NONE',  ( 93.39999999999999147, 1.023464760207051730E-14, 0.000000000000000000 ) ) ;
#66021 = STYLED_ITEM ( 'NONE', ( #24473 ), #94875 ) ;
#66022 = ORIENTED_EDGE ( 'NONE', *, *, #12182, .T. ) ;
#66023 = EDGE_CURVE ( 'NONE', #56343, #19689, #66573, .T. ) ;
#66024 = CARTESIAN_POINT ( 'NONE',  ( -7.179418352514219670, 41.32597165265336514, -70.21788016059471715 ) ) ;
#66026 = CARTESIAN_POINT ( 'NONE',  ( 30.91344358666947656, -49.90441520833090294, 35.32657779368672379 ) ) ;
#66025 = FILL_AREA_STYLE ('',( #97857 ) ) ;
#66027 = CARTESIAN_POINT ( 'NONE',  ( 34.81143942477683595, 344.1812935971262277, 0.3927586600043628251 ) ) ;
#66028 = VERTEX_POINT ( 'NONE', #24181 ) ;
#66029 = EDGE_CURVE ( 'NONE', #40289, #32311, #106103, .T. ) ;
#66030 = FACE_OUTER_BOUND ( 'NONE', #21868, .T. ) ;
#66031 = ADVANCED_FACE ( 'NONE', ( #32251 ), #65133, .T. ) ;
#66032 = ORIENTED_EDGE ( 'NONE', *, *, #94959, .F. ) ;
#66034 = CARTESIAN_POINT ( 'NONE',  ( -8.716351559231869217, -5.000000000000000000, -5.062179317052287075 ) ) ;
#66033 = DIRECTION ( 'NONE',  ( 0.000000000000000000, -1.000000000000000000, 0.000000000000000000 ) ) ;
#66035 = DIRECTION ( 'NONE',  ( 0.000000000000000000, -1.000000000000000000, 0.000000000000000000 ) ) ;
#66036 = CARTESIAN_POINT ( 'NONE',  ( -13.41614109918367248, 302.5494791983582559, -10.06425368032961210 ) ) ;
#66037 = DIRECTION ( 'NONE',  ( 0.000000000000000000, 0.000000000000000000, 1.000000000000000000 ) ) ;
#66038 = CARTESIAN_POINT ( 'NONE',  ( 1.012362131619463090, 45.47537026410230254, 18.25126109922685558 ) ) ;
#66039 = FACE_OUTER_BOUND ( 'NONE', #75323, .T. ) ;
#66040 = ORIENTED_EDGE ( 'NONE', *, *, #74108, .F. ) ;
#66041 = CARTESIAN_POINT ( 'NONE',  ( 92.73814317491743964, -60.00000000000002132, -7.760776698426044007 ) ) ;
#66042 = CARTESIAN_POINT ( 'NONE',  ( 4.582575694955839829, 16.00000000000000000, 10.00000000000000000 ) ) ;
#66043 = DIRECTION ( 'NONE',  ( -1.000000000000000000, 0.000000000000000000, 0.000000000000000000 ) ) ;
#66044 = EDGE_CURVE ( 'NONE', #44948, #47033, #81823, .T. ) ;
#66045 = CARTESIAN_POINT ( 'NONE',  ( 6.953930663124324063, 304.7325910270068334, -10.02533923955978956 ) ) ;
#66046 = DIRECTION ( 'NONE',  ( 0.000000000000000000, 0.000000000000000000, 1.000000000000000000 ) ) ;
#66047 = ORIENTED_EDGE ( 'NONE', *, *, #18234, .T. ) ;
#66048 = CARTESIAN_POINT ( 'NONE',  ( 14.85284876471456350, 1.482358050883964840E-15, 0.000000000000000000 ) ) ;
#66049 = ORIENTED_EDGE ( 'NONE', *, *, #34779, .F. ) ;
#66050 = ORIENTED_EDGE ( 'NONE', *, *, #7452, .T. ) ;
#66051 = CARTESIAN_POINT ( 'NONE',  ( 1.217386590295936655, 53.94013396134795357, 8.674651084135625467 ) ) ;
#66052 = CARTESIAN_POINT ( 'NONE',  ( 39.23171889029396198, 39.86656303868996076, -53.99799529535449238 ) ) ;
#66053 = CARTESIAN_POINT ( 'NONE',  ( 29.83349330513380337, 4.000000000000002665, 0.000000000000000000 ) ) ;
#66054 = CARTESIAN_POINT ( 'NONE',  ( 31.02114370244065356, 322.6370389015594924, 14.80589093843013160 ) ) ;
#66055 = CARTESIAN_POINT ( 'NONE',  ( 85.33365913786940382, -52.71608586643078098, 1.351353659569916488 ) ) ;
#66056 = CARTESIAN_POINT ( 'NONE',  ( -42.63617128354209740, 336.9381626248995190, 8.123117897685229849 ) ) ;
#66057 = CARTESIAN_POINT ( 'NONE',  ( -6.112161658498984629, -61.81941831950287281, 14.40466291265888188 ) ) ;
#66058 = CARTESIAN_POINT ( 'NONE',  ( 12.50000000000000711, 39.79061977335776845, -65.15808776970733618 ) ) ;
#66059 = ORIENTED_EDGE ( 'NONE', *, *, #55109, .F. ) ;
#66060 = CARTESIAN_POINT ( 'NONE',  ( 30.80805190526341519, 8.074044156869311095, 41.40902236837642647 ) ) ;
#66061 = VERTEX_POINT ( 'NONE', #106644 ) ;
#66062 = CARTESIAN_POINT ( 'NONE',  ( 21.08349330513380693, 1.593028355512270962E-15, 0.000000000000000000 ) ) ;
#66063 = CARTESIAN_POINT ( 'NONE',  ( 7.093721425956736049, 304.7303285792975771, 9.911179277710184365 ) ) ;
#66064 = CARTESIAN_POINT ( 'NONE',  ( 3.713158817313909843, -48.94636994418067388, 103.2987150069879903 ) ) ;
#66065 = PRESENTATION_LAYER_ASSIGNMENT (  '', '', ( #12612 ) ) ;
#66067 = VERTEX_POINT ( 'NONE', #353 ) ;
#66066 = CARTESIAN_POINT ( 'NONE',  ( -28.97838153899067137, -60.00000000000000000, 36.30225964348677792 ) ) ;
#66068 = CARTESIAN_POINT ( 'NONE',  ( 68.22945241178948095, -25.58280432435164542, 88.38472783749070061 ) ) ;
#66069 = VECTOR ( 'NONE', #95440, 1000.000000000000000 ) ;
#66070 = VERTEX_POINT ( 'NONE', #98549 ) ;
#66071 = AXIS2_PLACEMENT_3D ( 'NONE', #19484, #35119, #67987 ) ;
#66072 = CARTESIAN_POINT ( 'NONE',  ( 5.082755093536325930, -29.46875000204838813, -5.082755093536325042 ) ) ;
#66073 = CARTESIAN_POINT ( 'NONE',  ( -91.67701774657527380, -57.66167918384760327, -19.87712626951747552 ) ) ;
#66074 = ORIENTED_EDGE ( 'NONE', *, *, #100184, .F. ) ;
#66075 = SURFACE_STYLE_USAGE ( .BOTH. , #49347 ) ;
#66076 = CARTESIAN_POINT ( 'NONE',  ( 23.21751746555303342, -1.200000000000000030E-05, 33.20617127781017075 ) ) ;
#66077 = CARTESIAN_POINT ( 'NONE',  ( -35.00874989808971094, 491.4345812359313186, 12.31435046935995281 ) ) ;
#66078 = ADVANCED_FACE ( 'NONE', ( #24700 ), #82376, .T. ) ;
#66079 = CARTESIAN_POINT ( 'NONE',  ( -10.00000000000000355, 15.00000000000000000, -10.00000000000000000 ) ) ;
#66080 = CARTESIAN_POINT ( 'NONE',  ( 8.000000000000000000, -21.59375000409677625, -3.313708498984761608 ) ) ;
#66081 = CARTESIAN_POINT ( 'NONE',  ( 43.47770857297122404, 484.8227827122696567, 4.253339224811428565 ) ) ;
#66082 = DIRECTION ( 'NONE',  ( -0.8660254037844389297, -3.039937634619675546E-16, 0.4999999999999995004 ) ) ;
#66083 = CARTESIAN_POINT ( 'NONE',  ( 14.29190075645216851, 12.99999999999999289, 0.000000000000000000 ) ) ;
#66084 = CARTESIAN_POINT ( 'NONE',  ( 48.02835407290414338, 14.94086294439859408, -16.85535821593631667 ) ) ;
#66085 = CARTESIAN_POINT ( 'NONE',  ( -3.587928128302542596, 304.8518027750386636, 9.936999415048941131 ) ) ;
#66086 = COLOUR_RGB ( '', 0.08235294, 0.09019608, 0.10196078) ;
#66087 = CARTESIAN_POINT ( 'NONE',  ( -4.034557488803232062, 15.07443463110226212, -9.151133496028503345 ) ) ;
#66088 = ORIENTED_EDGE ( 'NONE', *, *, #63054, .T. ) ;
#66089 = DIRECTION ( 'NONE',  ( -1.000000000000000000, -1.224606353822377258E-16, -0.000000000000000000 ) ) ;
#66090 = DIRECTION ( 'NONE',  ( -0.000000000000000000, -1.000000000000000000, -0.000000000000000000 ) ) ;
#66091 = CARTESIAN_POINT ( 'NONE',  ( 12.78947859897790629, -60.00000000000000000, 39.70829609032173835 ) ) ;
#66092 = VECTOR ( 'NONE', #102139, 1000.000000000000000 ) ;
#66093 = CARTESIAN_POINT ( 'NONE',  ( -91.95742184699108179, -30.00000000000000000, 190.8556395465993774 ) ) ;
#66094 = EDGE_CURVE ( 'NONE', #70045, #64296, #44180, .T. ) ;
#66095 =( GEOMETRIC_REPRESENTATION_CONTEXT ( 3 ) GLOBAL_UNCERTAINTY_ASSIGNED_CONTEXT ( ( #25196 ) ) GLOBAL_UNIT_ASSIGNED_CONTEXT ( ( #83193, #91307, #99354 ) ) REPRESENTATION_CONTEXT ( 'NONE', 'WORKASPACE' ) );
#66096 = AXIS2_PLACEMENT_3D ( 'NONE', #10339, #92854, #69138 ) ;
#66097 = AXIS2_PLACEMENT_3D ( 'NONE', #52400, #21157, #11405 ) ;
#66098 = CARTESIAN_POINT ( 'NONE',  ( 37.56673239365899519, 25.75719283951025318, -10.95617127780834998 ) ) ;
#66099 = CARTESIAN_POINT ( 'NONE',  ( 73.33207134919089754, -57.63936585033923876, 183.5250597598029287 ) ) ;
#66101 = CARTESIAN_POINT ( 'NONE',  ( -9.182222763132468657, 53.50083500536204184, 3.877122753022949730 ) ) ;
#66100 = CARTESIAN_POINT ( 'NONE',  ( 6.690415142086856726, 41.73276191905608812, -59.04972836783017698 ) ) ;
#66102 = CARTESIAN_POINT ( 'NONE',  ( 23.69903725379788284, -27.21825735636527455, -38.40810431224176114 ) ) ;
#66103 = CARTESIAN_POINT ( 'NONE',  ( -38.02740175685438828, 490.5688714813329057, 12.25042287455428180 ) ) ;
#66104 = CARTESIAN_POINT ( 'NONE',  ( -41.23432746627220524, -59.99999999999999289, 53.93406616075787952 ) ) ;
#66105 = CARTESIAN_POINT ( 'NONE',  ( 14.91270732344407257, 41.98564553269472555, -86.62216337287246404 ) ) ;
#66106 = ADVANCED_FACE ( 'NONE', ( #19306, #68334 ), #51056, .F. ) ;
#66107 = DIRECTION ( 'NONE',  ( -1.000000000000000000, 2.664535259100375697E-15, 0.000000000000000000 ) ) ;
#66108 = CARTESIAN_POINT ( 'NONE',  ( -86.80924175235543316, -20.64942504254944922, 185.6736228309295598 ) ) ;
#66109 = ORIENTED_EDGE ( 'NONE', *, *, #20690, .T. ) ;
#66110 = CARTESIAN_POINT ( 'NONE',  ( 19.50000000000160583, 49.99999999999990052, 59.86364615470513684 ) ) ;
#66111 = CARTESIAN_POINT ( 'NONE',  ( 6.125000000000095923, -15.62228920881129390, 14.41094225130415651 ) ) ;
#66112 = CARTESIAN_POINT ( 'NONE',  ( -10.23031279217029876, -35.99451456354128709, 29.89987121441171425 ) ) ;
#66113 = EDGE_CURVE ( 'NONE', #66259, #88304, #60786, .T. ) ;
#66115 = CARTESIAN_POINT ( 'NONE',  ( 4.291829500544997344, -67.75856037000218635, 13.66196629111150607 ) ) ;
#66114 = CARTESIAN_POINT ( 'NONE',  ( 0.000000000000000000, 0.000000000000000000, 0.000000000000000000 ) ) ;
#66116 = ORIENTED_EDGE ( 'NONE', *, *, #2098, .F. ) ;
#66118 = SURFACE_STYLE_USAGE ( .BOTH. , #16504 ) ;
#66117 = CIRCLE ( 'NONE', #105688, 3.309500000000001663 ) ;
#66119 = CARTESIAN_POINT ( 'NONE',  ( -6.109877454823899434, -4.349879335532910396, -16.82893417409533399 ) ) ;
#66120 = CARTESIAN_POINT ( 'NONE',  ( -7.002641335706727865, 31.05087262680831728, 3.868676264653293728 ) ) ;
#66121 = CARTESIAN_POINT ( 'NONE',  ( 33.54963988678932196, 300.7094765539930563, -0.6813154228844996441 ) ) ;
#66122 = DIRECTION ( 'NONE',  ( -1.000000000000000000, -1.224606353822377258E-16, -0.000000000000000000 ) ) ;
#66123 = CARTESIAN_POINT ( 'NONE',  ( -7.551892080562055298, -81.99012297460615173, 2.647003822403974471 ) ) ;
#66124 = CARTESIAN_POINT ( 'NONE',  ( -43.51517875623797948, 462.0595338174562130, 4.327785711300204952 ) ) ;
#66125 = CARTESIAN_POINT ( 'NONE',  ( 109.1953510978495956, -29.99999999999998934, 161.8808647345001646 ) ) ;
#66126 = CARTESIAN_POINT ( 'NONE',  ( -35.56416567029047116, 496.2909070316903239, -10.19064917708978335 ) ) ;
#66127 = EDGE_LOOP ( 'NONE', ( #92700, #41478, #61419, #103441 ) ) ;
#66128 = DIRECTION ( 'NONE',  ( 0.000000000000000000, 0.000000000000000000, 1.000000000000000000 ) ) ;
#66129 = DIRECTION ( 'NONE',  ( 0.000000000000000000, -1.000000000000000000, 0.000000000000000000 ) ) ;
#66130 = DIRECTION ( 'NONE',  ( 0.000000000000000000, -0.9540597841379422350, 0.2996163017772281445 ) ) ;
#66131 = COLOUR_RGB ( '', 0.31764706, 0.68627451, 0.89019608) ;
#66132 = CARTESIAN_POINT ( 'NONE',  ( -7.263825692932297962, -4.945657111639586212, -7.907570769506051533 ) ) ;
#66133 = CARTESIAN_POINT ( 'NONE',  ( 37.71362718402959047, 391.7064369608328320, 6.183124041103365442 ) ) ;
#66134 = DIRECTION ( 'NONE',  ( -1.000000000000000000, -1.224606353822377258E-16, -0.000000000000000000 ) ) ;
#66135 = ORIENTED_EDGE ( 'NONE', *, *, #79519, .T. ) ;
#66136 = CARTESIAN_POINT ( 'NONE',  ( -22.32457463498002426, 305.3822942928727002, 10.05158438472647475 ) ) ;
#66137 = ORIENTED_EDGE ( 'NONE', *, *, #56694, .F. ) ;
#66138 = CARTESIAN_POINT ( 'NONE',  ( 36.51457990505107887, 485.2739886279269399, -2.924107101145942522 ) ) ;
#66139 = SURFACE_STYLE_USAGE ( .BOTH. , #82859 ) ;
#66140 = CARTESIAN_POINT ( 'NONE',  ( 33.00540147335372865, 487.4196752801331058, 9.523982417621985164 ) ) ;
#66141 = ORIENTED_EDGE ( 'NONE', *, *, #78781, .T. ) ;
#66142 = FILL_AREA_STYLE_COLOUR ( '', #15219 ) ;
#66143 = CARTESIAN_POINT ( 'NONE',  ( 6.105464488512484245, -12.30761336975154308, 12.19688296867937538 ) ) ;
#66144 = CARTESIAN_POINT ( 'NONE',  ( -76.06031650297444457, -60.00000000000984812, 194.6114218367068815 ) ) ;
#66145 = FACE_OUTER_BOUND ( 'NONE', #77782, .T. ) ;
#66146 = ORIENTED_EDGE ( 'NONE', *, *, #37700, .F. ) ;
#66147 = CARTESIAN_POINT ( 'NONE',  ( 112.1408118161186991, -59.99999999999998579, 167.6738597471375840 ) ) ;
#66149 = CARTESIAN_POINT ( 'NONE',  ( 18.30455222202033738, -60.35759502867323079, 34.30908099980990755 ) ) ;
#66148 = CARTESIAN_POINT ( 'NONE',  ( -76.30486425386099825, -30.00000000000004619, 168.5691345232379206 ) ) ;
#66151 = CARTESIAN_POINT ( 'NONE',  ( 18.71440884245025416, 61.34242035161803841, -9.357204421225121749 ) ) ;
#66150 = UNCERTAINTY_MEASURE_WITH_UNIT (LENGTH_MEASURE( 1.000000000000000082E-05 ), #55188, 'distance_accuracy_value', 'NONE');
#66152 = CARTESIAN_POINT ( 'NONE',  ( -43.22159273586203199, -46.43894676989327763, 43.43051601094587966 ) ) ;
#66153 = CARTESIAN_POINT ( 'NONE',  ( -12.50000000000000711, 18.64303733123573537, -36.27143273323382999 ) ) ;
#66154 = EDGE_LOOP ( 'NONE', ( #8340, #50380, #1721, #58527 ) ) ;
#66155 =( LENGTH_UNIT ( ) NAMED_UNIT ( * ) SI_UNIT ( .MILLI., .METRE. ) );
#66156 = PLANE ( 'NONE',  #105922 ) ;
#66157 = CARTESIAN_POINT ( 'NONE',  ( 38.68218982724705057, 320.0845437455996603, 16.10279619727025135 ) ) ;
#66158 = FILL_AREA_STYLE_COLOUR ( '', #56084 ) ;
#66159 = DIRECTION ( 'NONE',  ( 0.000000000000000000, 0.000000000000000000, 1.000000000000000000 ) ) ;
#66160 = CARTESIAN_POINT ( 'NONE',  ( -29.99999999999437250, 487.0575442883997539, 5.835066518937727764 ) ) ;
#66161 = ORIENTED_EDGE ( 'NONE', *, *, #56000, .T. ) ;
#66162 = CARTESIAN_POINT ( 'NONE',  ( 4.792515968931522430, -47.29776092521730391, 102.4138677444059766 ) ) ;
#66163 = ORIENTED_EDGE ( 'NONE', *, *, #57435, .F. ) ;
#66164 = CARTESIAN_POINT ( 'NONE',  ( 81.56357004051291426, -30.00000000000010303, -4.949223632071581669 ) ) ;
#66165 = CARTESIAN_POINT ( 'NONE',  ( 17.73673397241445926, 41.93065142196708450, -82.77986825849473007 ) ) ;
#66166 = VECTOR ( 'NONE', #27944, 1000.000000000000114 ) ;
#66167 = DIRECTION ( 'NONE',  ( -1.000000000000000000, -1.224606353822377258E-16, -0.000000000000000000 ) ) ;
#66169 = ADVANCED_FACE ( 'NONE', ( #52662 ), #102284, .T. ) ;
#66168 = DIRECTION ( 'NONE',  ( 0.000000000000000000, 0.000000000000000000, 1.000000000000000000 ) ) ;
#66170 = CARTESIAN_POINT ( 'NONE',  ( 92.70324471557209733, -29.99999999999999645, 104.2926456640488055 ) ) ;
#66171 = AXIS2_PLACEMENT_3D ( 'NONE', #76405, #35468, #3607 ) ;
#66172 = ADVANCED_FACE ( 'NONE', ( #3600 ), #32101, .T. ) ;
#66173 = CARTESIAN_POINT ( 'NONE',  ( -42.10086803841218739, 435.6552064019005002, 19.95582312411058368 ) ) ;
#66174 = ORIENTED_EDGE ( 'NONE', *, *, #38172, .F. ) ;
#66175 =( GEOMETRIC_REPRESENTATION_CONTEXT ( 3 ) GLOBAL_UNCERTAINTY_ASSIGNED_CONTEXT ( ( #73703 ) ) GLOBAL_UNIT_ASSIGNED_CONTEXT ( ( #40480, #39962, #71774 ) ) REPRESENTATION_CONTEXT ( 'NONE', 'WORKASPACE' ) );
#66176 = VECTOR ( 'NONE', #13521, 1000.000000000000000 ) ;
#66177 = ORIENTED_EDGE ( 'NONE', *, *, #43638, .T. ) ;
#66178 = VERTEX_POINT ( 'NONE', #10084 ) ;
#66179 = LINE ( 'NONE', #17115, #71508 ) ;
#66180 = CARTESIAN_POINT ( 'NONE',  ( 22.88516029091543302, 26.05169045632067437, 30.73959371576558297 ) ) ;
#66181 = EDGE_CURVE ( 'NONE', #53932, #22177, #1059, .T. ) ;
#66182 = CARTESIAN_POINT ( 'NONE',  ( -41.87034742571102441, 465.6969385752248627, 15.30562829125321933 ) ) ;
#66183 = CARTESIAN_POINT ( 'NONE',  ( -30.93356169769148423, 332.2899936558947047, 16.85461323756102558 ) ) ;
#66184 = DIRECTION ( 'NONE',  ( 0.000000000000000000, -1.000000000000000000, 0.000000000000000000 ) ) ;
#66185 = VERTEX_POINT ( 'NONE', #59719 ) ;
#66186 = CARTESIAN_POINT ( 'NONE',  ( 9.165151389911679658, 105.0000000000000142, -4.000000000000001776 ) ) ;
#66187 = ORIENTED_EDGE ( 'NONE', *, *, #32373, .T. ) ;
#66188 = CARTESIAN_POINT ( 'NONE',  ( 32.99999999999999289, 439.7597899781498541, 24.16317522621305258 ) ) ;
#66189 = CARTESIAN_POINT ( 'NONE',  ( 77.60215982985106109, -38.52546103277521894, 186.8513230885473888 ) ) ;
#66190 = CARTESIAN_POINT ( 'NONE',  ( 23.58349330513380337, 4.000000000000002665, 0.000000000000000000 ) ) ;
#66191 = CARTESIAN_POINT ( 'NONE',  ( 31.35831589341289316, 299.6070351798090883, 11.00495117483204055 ) ) ;
#66192 = CARTESIAN_POINT ( 'NONE',  ( 6.249999999999998224, 8.000000000000000000, 0.000000000000000000 ) ) ;
#66193 = B_SPLINE_CURVE_WITH_KNOTS ( 'NONE', 3,
 ( #63391, #56303, #15340, #89242, #70926, #96803, #62852, #22411, #14800, #71443, #79544, #78481, #6174, #55772, #87127, #71986, #103305, #96286, #13204, #46644 ),
 .UNSPECIFIED., .F., .F.,
 ( 4, 2, 2, 2, 2, 2, 2, 2, 2, 4 ),
 ( 0.0009441224788332293989, 0.001448919914566972403, 0.001953717350300715732, 0.002458514786034458628, 0.002963312221768201957, 0.003468109657501945286, 0.003972907093235689482, 0.004225305811102561364, 0.004477704528969433245, 0.004982501964703170937 ),
 .UNSPECIFIED. ) ;
#66194 = CARTESIAN_POINT ( 'NONE',  ( 46.08349330513379982, -4.000000000000000888, 4.898587196589416773E-16 ) ) ;
#66195 = CARTESIAN_POINT ( 'NONE',  ( 42.76745897559497678, 409.8493022072242979, 19.95836708624130296 ) ) ;
#66196 = CYLINDRICAL_SURFACE ( 'NONE', #94547, 5.000000000000002665 ) ;
#66197 = AXIS2_PLACEMENT_3D ( 'NONE', #64967, #31572, #13751 ) ;
#66198 = SURFACE_STYLE_USAGE ( .BOTH. , #33328 ) ;
#66199 = VERTEX_POINT ( 'NONE', #51599 ) ;
#66200 = CARTESIAN_POINT ( 'NONE',  ( -22.37854104367661279, 303.2958516734515229, 10.03245274550628885 ) ) ;
#66201 = DIRECTION ( 'NONE',  ( 1.000000000000000000, 0.000000000000000000, 0.000000000000000000 ) ) ;
#66202 = CARTESIAN_POINT ( 'NONE',  ( -46.00000000000000000, 437.9690125970932968, 14.09127711025707796 ) ) ;
#66203 = CARTESIAN_POINT ( 'NONE',  ( -8.000000000000001776, -11.65624999999999289, 3.313708498984758943 ) ) ;
#66204 = CARTESIAN_POINT ( 'NONE',  ( 6.482941653187340947, -18.96218766594433092, 35.15061247569060043 ) ) ;
#66205 = CARTESIAN_POINT ( 'NONE',  ( 2.587364514240426239, 300.7566975493048176, 9.662361691355732418 ) ) ;
#66206 = EDGE_CURVE ( 'NONE', #43607, #9118, #84519, .T. ) ;
#66207 = MECHANICAL_DESIGN_GEOMETRIC_PRESENTATION_REPRESENTATION (  '', ( #48943 ), #33497 ) ;
#66208 = CIRCLE ( 'NONE', #61072, 4.000000000000007105 ) ;
#66209 = DIRECTION ( 'NONE',  ( 0.000000000000000000, -1.000000000000000000, 0.000000000000000000 ) ) ;
#66210 = CARTESIAN_POINT ( 'NONE',  ( 86.39342217817984704, -17.39602584710043587, 179.4229172789653717 ) ) ;
#66211 = CARTESIAN_POINT ( 'NONE',  ( -6.499999999999999112, -3.752776749732587902, -8.000000000000000000 ) ) ;
#66212 = B_SPLINE_CURVE_WITH_KNOTS ( 'NONE', 3,
 ( #86781, #70584, #96972, #96455 ),
 .UNSPECIFIED., .F., .F.,
 ( 4, 4 ),
 ( 0.000000000000000000, 0.001587725418201289037 ),
 .UNSPECIFIED. ) ;
#66213 = ORIENTED_EDGE ( 'NONE', *, *, #86303, .F. ) ;
#66214 = CARTESIAN_POINT ( 'NONE',  ( 93.08263284641110147, -57.65567480148813928, -17.01414318937586145 ) ) ;
#66215 = CARTESIAN_POINT ( 'NONE',  ( 0.000000000000000000, 56.87938524157181774, -0.6840402866513453084 ) ) ;
#66216 = CARTESIAN_POINT ( 'NONE',  ( -81.12945012041117820, -30.00000000000000711, 23.35381562080259954 ) ) ;
#66217 = EDGE_CURVE ( 'NONE', #28485, #25485, #78533, .T. ) ;
#66218 = B_SPLINE_CURVE_WITH_KNOTS ( 'NONE', 3,
 ( #96835, #22965, #14829, #9379, #50376, #34247, #19674, #42833, #41768, #91400, #17515, #74652, #8863, #60116, #76788, #2363, #100531, #26694, #52514, #84894, #10982, #101613, #10455, #68173, #738, #93529, #101070, #18590, #33703, #75730 ),
 .UNSPECIFIED., .F., .F.,
 ( 4, 2, 2, 2, 2, 2, 2, 2, 2, 2, 2, 2, 2, 2, 4 ),
 ( 0.004426540215027332387, 0.005358602402239606710, 0.005824633495845744739, 0.006290664589451882768, 0.006523680136254953951, 0.006756695683058026869, 0.006989711229861098052, 0.007222726776664170970, 0.007455742323467242152, 0.007688757870270314203, 0.008154788963876466110, 0.009086851151088764719, 0.01001891333830106506, 0.01095097552551336367, 0.01188303771272565881 ),
 .UNSPECIFIED. ) ;
#66219 = CARTESIAN_POINT ( 'NONE',  ( -85.15168385860675926, -37.99999999999996447, 183.5647360535557766 ) ) ;
#66220 = CARTESIAN_POINT ( 'NONE',  ( 0.000000000000000000, 0.000000000000000000, -12.27439246179028309 ) ) ;
#66221 = DIRECTION ( 'NONE',  ( 0.000000000000000000, 0.000000000000000000, -1.000000000000000000 ) ) ;
#66223 = LINE ( 'NONE', #91058, #79225 ) ;
#66222 = CARTESIAN_POINT ( 'NONE',  ( -33.00000000000000000, 439.7597899781497972, 24.16317522621304192 ) ) ;
#66224 = CARTESIAN_POINT ( 'NONE',  ( -17.49999999999997513, 49.32716648907489088, 64.00616971907881236 ) ) ;
#66225 = CARTESIAN_POINT ( 'NONE',  ( -28.43952395724186388, 17.90362770311683605, 40.70652153699781906 ) ) ;
#66226 = CARTESIAN_POINT ( 'NONE',  ( -15.56704895981947168, 43.91947438609057741, -6.064211335331039621 ) ) ;
#66227 = DIRECTION ( 'NONE',  ( 0.000000000000000000, 0.000000000000000000, 1.000000000000000000 ) ) ;
#66228 = CARTESIAN_POINT ( 'NONE',  ( -64.10993277136456925, -37.76178193452332010, -24.57515171481401595 ) ) ;
#66229 = DIRECTION ( 'NONE',  ( 0.000000000000000000, 0.000000000000000000, -1.000000000000000000 ) ) ;
#66230 = CARTESIAN_POINT ( 'NONE',  ( 32.93320410570996870, 485.0465637715138314, 1.208268278917676852 ) ) ;
#66231 = EDGE_CURVE ( 'NONE', #19129, #96664, #105214, .T. ) ;
#66232 = STYLED_ITEM ( 'NONE', ( #73636 ), #18657 ) ;
#66233 = ORIENTED_EDGE ( 'NONE', *, *, #20675, .F. ) ;
#66234 = CARTESIAN_POINT ( 'NONE',  ( 12.50000000000000355, -79.93083296558610584, -76.70843802411151557 ) ) ;
#66235 = SURFACE_SIDE_STYLE ('',( #926 ) ) ;
#66236 = CARTESIAN_POINT ( 'NONE',  ( -6.928203230275509661, 84.73520732746429474, 3.999999999999999112 ) ) ;
#66237 = CARTESIAN_POINT ( 'NONE',  ( -64.59904024412152523, -29.72015457327714572, -23.23336862644748990 ) ) ;
#66238 =( BOUNDED_SURFACE ( )  B_SPLINE_SURFACE ( 3, 2, ( 
 ( #62721, #62212, #53558 ),
 ( #86489, #12547, #95610 ),
 ( #61682, #96672, #95095 ),
 ( #54588, #21753, #22808 ) ),
 .UNSPECIFIED., .F., .F., .F. ) 
 B_SPLINE_SURFACE_WITH_KNOTS ( ( 4, 4 ),
 ( 3, 3 ),
 ( 1.682681771697502882E-16, 0.0002890157658755999155 ),
 ( 0.000000000000000000, 1.000000000000000000 ),
 .UNSPECIFIED. ) 
 GEOMETRIC_REPRESENTATION_ITEM ( )  RATIONAL_B_SPLINE_SURFACE ( (
 ( 1.000000000000000000, 0.7950530193018341407, 1.000000000000000000),
 ( 1.000000000000000000, 0.7968506399851618127, 1.000000000000000000),
 ( 1.000000000000000000, 0.7985582592109712330, 1.000000000000000000),
 ( 1.000000000000000000, 0.8001746426092147813, 1.000000000000000000) ) ) 
 REPRESENTATION_ITEM ( '' )  SURFACE ( )  );
#66239 = EDGE_CURVE ( 'NONE', #70163, #13347, #6224, .T. ) ;
#66241 = CARTESIAN_POINT ( 'NONE',  ( -72.01167074608865448, -21.77034257964697872, -18.48521213137105335 ) ) ;
#66240 = CARTESIAN_POINT ( 'NONE',  ( 37.06438722625302518, 6.123233995736772199E-16, -5.000000000000001776 ) ) ;
#66242 = PRODUCT_DEFINITION_FORMATION_WITH_SPECIFIED_SOURCE ( 'ANY', '', #19209, .NOT_KNOWN. ) ;
#66243 = ORIENTED_EDGE ( 'NONE', *, *, #24444, .T. ) ;
#66244 = AXIS2_PLACEMENT_3D ( 'NONE', #37733, #28566, #3738 ) ;
#66245 = CARTESIAN_POINT ( 'NONE',  ( 26.36650669486618881, 1.474610560812782335E-15, 0.000000000000000000 ) ) ;
#66246 = ORIENTED_EDGE ( 'NONE', *, *, #51090, .F. ) ;
#66247 = CARTESIAN_POINT ( 'NONE',  ( 41.75349605901003258, 461.8279235811430681, 2.915883750441165212 ) ) ;
#66248 = EDGE_CURVE ( 'NONE', #43166, #3450, #79613, .T. ) ;
#66249 = CARTESIAN_POINT ( 'NONE',  ( 11.36542776952655487, 43.57490045297072356, -13.50743829070831659 ) ) ;
#66250 = EDGE_CURVE ( 'NONE', #15279, #84521, #94202, .T. ) ;
#66251 = CARTESIAN_POINT ( 'NONE',  ( -52.47326062800689073, -60.00000000000000000, -37.40410650496403377 ) ) ;
#66253 = ADVANCED_FACE ( 'NONE', ( #21927 ), #45134, .T. ) ;
#66252 = ORIENTED_EDGE ( 'NONE', *, *, #44810, .F. ) ;
#66254 = CARTESIAN_POINT ( 'NONE',  ( 0.4037800551813712779, -4.058962678540093627, 5.969670414742685338 ) ) ;
#66255 = CARTESIAN_POINT ( 'NONE',  ( 15.43348245327038804, 2.792842261935781778, 2.002630087556611649 ) ) ;
#66256 = CARTESIAN_POINT ( 'NONE',  ( 102.8270117144912632, -60.17405004303049765, 193.1076501718758607 ) ) ;
#66258 = DIRECTION ( 'NONE',  ( -1.000000000000000000, 0.000000000000000000, 0.000000000000000000 ) ) ;
#66257 = CARTESIAN_POINT ( 'NONE',  ( 2.499999999999997780, -18.83380486180452706, 27.02532357426314036 ) ) ;
#66259 = VERTEX_POINT ( 'NONE', #79596 ) ;
#66260 = EDGE_LOOP ( 'NONE', ( #19411, #84781 ) ) ;
#66261 = EDGE_LOOP ( 'NONE', ( #79554, #99433 ) ) ;
#66262 = CARTESIAN_POINT ( 'NONE',  ( 29.72408284768632214, 326.8902487607700778, 14.35721078449378574 ) ) ;
#66263 = CARTESIAN_POINT ( 'NONE',  ( -6.019773438520521047, -12.68390881199314890, 12.80591459028008749 ) ) ;
#66264 = CARTESIAN_POINT ( 'NONE',  ( 9.180492345103683505, 53.50238668477037862, 3.869105311585077978 ) ) ;
#66265 = EDGE_LOOP ( 'NONE', ( #83750, #6184, #23737, #60056 ) ) ;
#66266 = AXIS2_PLACEMENT_3D ( 'NONE', #103455, #71606, #22576 ) ;
#66267 = CARTESIAN_POINT ( 'NONE',  ( -16.14595037822616419, 12.99999999999999289, 0.000000000000000000 ) ) ;
#66268 = CARTESIAN_POINT ( 'NONE',  ( -6.701893397842001221, 41.44328394191487774, -70.59544911652842814 ) ) ;
#66269 = CARTESIAN_POINT ( 'NONE',  ( -18.91791044776116237, 45.00000000000000711, 62.18611311450884926 ) ) ;
#66270 = CARTESIAN_POINT ( 'NONE',  ( -44.89949488402420030, -57.68324447995585302, 64.92693994880102082 ) ) ;
#66271 = CARTESIAN_POINT ( 'NONE',  ( 7.188101187500000044, -31.15625000204838813, 0.000000000000000000 ) ) ;
#66272 = CARTESIAN_POINT ( 'NONE',  ( -30.29489621385934228, 12.93001532776399642, 41.94819669044308341 ) ) ;
#66273 = CARTESIAN_POINT ( 'NONE',  ( -31.19792890532719198, 414.2215770364159084, 25.44228638033458623 ) ) ;
#66274 = DIRECTION ( 'NONE',  ( 1.000000000000000000, 0.000000000000000000, -0.000000000000000000 ) ) ;
#66275 = CARTESIAN_POINT ( 'NONE',  ( -25.62895382379538489, -60.00000000000000711, -43.76007060795225101 ) ) ;
#66276 = CARTESIAN_POINT ( 'NONE',  ( -34.17891763260271887, -14.21045842199440301, 38.95228509905292924 ) ) ;
#66277 = CARTESIAN_POINT ( 'NONE',  ( -51.71596078174152211, -25.65011578757576416, 48.87676497752350713 ) ) ;
#66278 = CARTESIAN_POINT ( 'NONE',  ( 3.463946997120229021, 19.86939720178062885, -6.085025630164112798 ) ) ;
#66279 = ORIENTED_EDGE ( 'NONE', *, *, #90808, .T. ) ;
#66280 = AXIS2_PLACEMENT_3D ( 'NONE', #63937, #30514, #55274 ) ;
#66281 = CARTESIAN_POINT ( 'NONE',  ( -97.64691574547987329, -37.71246555177214077, 192.6310394866860349 ) ) ;
#66282 = STYLED_ITEM ( 'NONE', ( #81746 ), #55770 ) ;
#66283 = AXIS2_PLACEMENT_3D ( 'NONE', #99563, #42942, #101180 ) ;
#66284 = CARTESIAN_POINT ( 'NONE',  ( -0.6398555294984749064, 296.1023409385620653, -10.00028515034555809 ) ) ;
#66285 = CARTESIAN_POINT ( 'NONE',  ( 10.11650669486618881, 4.000000000000003553, 4.898587196589414801E-16 ) ) ;
#66286 = EDGE_LOOP ( 'NONE', ( #68316, #54966, #64843, #18026 ) ) ;
#66287 = CARTESIAN_POINT ( 'NONE',  ( 4.472135954999578722, 249.9999999999999432, 4.000000000000002665 ) ) ;
#66288 = VECTOR ( 'NONE', #17232, 1000.000000000000000 ) ;
#66289 = CARTESIAN_POINT ( 'NONE',  ( 96.60812357626146252, -38.48423040734370204, 201.1678166273348722 ) ) ;
#66290 = DIRECTION ( 'NONE',  ( 0.000000000000000000, -1.000000000000000000, 0.000000000000000000 ) ) ;
#66291 = CARTESIAN_POINT ( 'NONE',  ( 0.000000000000000000, 0.000000000000000000, -5.000000000000000000 ) ) ;
#66292 = CARTESIAN_POINT ( 'NONE',  ( -20.97754405179124149, 294.8763868968453608, 9.942224931492244622 ) ) ;
#66293 = AXIS2_PLACEMENT_3D ( 'NONE', #103344, #54763, #104385 ) ;
#66294 = CARTESIAN_POINT ( 'NONE',  ( -2.912673042965788187E-14, 42.00000000000000000, -90.56128410203886858 ) ) ;
#66295 = CARTESIAN_POINT ( 'NONE',  ( 82.35949071855475268, -30.00000000000001066, 148.3810521812565923 ) ) ;
#66296 = CARTESIAN_POINT ( 'NONE',  ( 36.15790072655332921, 490.9284497187077818, 12.44298047260061679 ) ) ;
#66297 = FILL_AREA_STYLE_COLOUR ( '', #70325 ) ;
#66298 = EDGE_CURVE ( 'NONE', #45473, #66178, #2888, .T. ) ;
#66299 = DIRECTION ( 'NONE',  ( 0.000000000000000000, -1.000000000000000000, 0.000000000000000000 ) ) ;
#66300 = ORIENTED_EDGE ( 'NONE', *, *, #31133, .T. ) ;
#66301 = ORIENTED_EDGE ( 'NONE', *, *, #87735, .T. ) ;
#66302 = CARTESIAN_POINT ( 'NONE',  ( 52.62853896714921831, -32.57219741345102193, 52.90247569886912515 ) ) ;
#66303 = CARTESIAN_POINT ( 'NONE',  ( -5.644657432743346526, 301.6279981551656419, -10.01771144603109853 ) ) ;
#66304 = EDGE_CURVE ( 'NONE', #77351, #32439, #11404, .T. ) ;
#66305 = CARTESIAN_POINT ( 'NONE',  ( 36.57348720720209201, 28.18042387246633851, -11.44262404694478974 ) ) ;
#66306 = ORIENTED_EDGE ( 'NONE', *, *, #32522, .T. ) ;
#66307 = CARTESIAN_POINT ( 'NONE',  ( -90.59568090330395762, -38.34730571723916626, 12.65513652691200086 ) ) ;
#66308 = ORIENTED_EDGE ( 'NONE', *, *, #36515, .T. ) ;
#66309 = CARTESIAN_POINT ( 'NONE',  ( 14.83882035797480370, 4.620392632306892899, 5.701545570394880968 ) ) ;
#66310 = CARTESIAN_POINT ( 'NONE',  ( 99.34690486943590315, -38.35585097942631450, 84.62317533721636664 ) ) ;
#66311 = CARTESIAN_POINT ( 'NONE',  ( 12.53415426001211763, 20.77299430586604601, -6.330093763739077950 ) ) ;
#66312 = CARTESIAN_POINT ( 'NONE',  ( 84.82478036673688848, -37.84938749301726801, 44.26570419945227997 ) ) ;
#66313 = SURFACE_STYLE_FILL_AREA ( #41504 ) ;
#66314 = DIRECTION ( 'NONE',  ( 0.000000000000000000, -0.000000000000000000, 1.000000000000000000 ) ) ;
#66315 = CARTESIAN_POINT ( 'NONE',  ( -29.57614253651134106, 308.9699467501231993, -8.830034548758142421 ) ) ;
#66316 = CARTESIAN_POINT ( 'NONE',  ( 6.289572920342626716, 6.243622107253691489, -2.843693100100564308 ) ) ;
#66317 = CARTESIAN_POINT ( 'NONE',  ( 75.48311596653083200, -60.00000000000000711, 184.3857932157642949 ) ) ;
#66318 = STYLED_ITEM ( 'NONE', ( #10746 ), #98816 ) ;
#66319 = DIRECTION ( 'NONE',  ( 0.000000000000000000, 0.000000000000000000, 1.000000000000000000 ) ) ;
#66320 = ORIENTED_EDGE ( 'NONE', *, *, #37112, .F. ) ;
#66321 = CARTESIAN_POINT ( 'NONE',  ( 61.11682477142169034, -53.38749459719494439, 82.02260153653946873 ) ) ;
#66322 = CARTESIAN_POINT ( 'NONE',  ( -25.74471865176096230, 304.2941041679271166, -9.686096690486662553 ) ) ;
#66323 = ADVANCED_FACE ( 'NONE', ( #81691, #97898, #90885, #32673, #65541 ), #83883, .F. ) ;
#66324 = CARTESIAN_POINT ( 'NONE',  ( 13.09999999999999787, 1.533819458162526451E-15, 0.000000000000000000 ) ) ;
#66325 = PRODUCT_DEFINITION_FORMATION_WITH_SPECIFIED_SOURCE ( 'ANY', '', #70009, .NOT_KNOWN. ) ;
#66326 = CARTESIAN_POINT ( 'NONE',  ( -9.370229349454282541, -5.000000000000000000, -18.71807701186707362 ) ) ;
#66328 = CARTESIAN_POINT ( 'NONE',  ( -4.659670875555729452, 53.64098639941263258, 8.372684524479227619 ) ) ;
#66327 = CARTESIAN_POINT ( 'NONE',  ( -78.20651881317490961, -38.35596806284291915, -27.53224245461382935 ) ) ;
#66329 = CARTESIAN_POINT ( 'NONE',  ( -40.89628519196639189, 427.9551160164463113, 26.89233021404036705 ) ) ;
#66330 = CARTESIAN_POINT ( 'NONE',  ( -32.11963216114055797, 486.1305616887682390, 5.366014163932117498 ) ) ;
#66331 = CARTESIAN_POINT ( 'NONE',  ( -38.98358762946092781, 463.6566946817218877, 19.41660091132907695 ) ) ;
#66332 = CARTESIAN_POINT ( 'NONE',  ( 3.313708498984762496, -27.78124999999999289, 7.999999999999998224 ) ) ;
#66333 = ADVANCED_FACE ( 'NONE', ( #31091 ), #56300, .T. ) ;
#66334 = DIRECTION ( 'NONE',  ( -1.000000000000000000, 0.000000000000000000, 0.000000000000000000 ) ) ;
#66335 = ORIENTED_EDGE ( 'NONE', *, *, #17744, .F. ) ;
#66336 = CARTESIAN_POINT ( 'NONE',  ( 81.82114106837175882, -57.06932440951347729, 184.1247409842175387 ) ) ;
#66337 = CARTESIAN_POINT ( 'NONE',  ( 43.52075891743747604, 484.7805561108180541, 4.063293749110901132 ) ) ;
#66338 = CARTESIAN_POINT ( 'NONE',  ( -39.97975729992978700, 437.4435441785136049, 22.46871538407117441 ) ) ;
#66339 = VERTEX_POINT ( 'NONE', #96857 ) ;
#66340 = LINE ( 'NONE', #8099, #16941 ) ;
#66341 = CARTESIAN_POINT ( 'NONE',  ( 42.37751841893198446, 435.9440627571722757, 7.948837343527293875 ) ) ;
#66342 = CARTESIAN_POINT ( 'NONE',  ( -9.000000000000001776, -4.000000000000003553, 42.58845726811989607 ) ) ;
#66343 = CARTESIAN_POINT ( 'NONE',  ( 9.891797161801495264, -3.000000000000002665, -73.72381496649795452 ) ) ;
#66344 = CARTESIAN_POINT ( 'NONE',  ( -37.15195575618992763, 42.30491125877714609, -59.42450515948280554 ) ) ;
#66345 = EDGE_CURVE ( 'NONE', #60578, #86058, #22984, .T. ) ;
#66346 = CARTESIAN_POINT ( 'NONE',  ( 53.63423276373041659, -60.00000000000000000, 81.40523378288756362 ) ) ;
#66347 = CIRCLE ( 'NONE', #100759, 74.46152422706630603 ) ;
#66348 = CARTESIAN_POINT ( 'NONE',  ( 46.00000000000000000, 488.9831568219304927, 4.757012338623754388 ) ) ;
#66349 = CARTESIAN_POINT ( 'NONE',  ( 26.83690358097182482, -20.16800216920047006, 31.72032485502600352 ) ) ;
#66351 = CARTESIAN_POINT ( 'NONE',  ( -12.41941622641344622, 22.56916116445944454, -6.095008768951160505 ) ) ;
#66350 = CARTESIAN_POINT ( 'NONE',  ( -12.34912842698533986, -21.29189974538021701, 35.60347046151010630 ) ) ;
#66352 = VECTOR ( 'NONE', #88422, 1000.000000000000000 ) ;
#66353 = CARTESIAN_POINT ( 'NONE',  ( 5.082755093536324154, -11.84375000204838635, 5.082755093536326818 ) ) ;
#66354 = CARTESIAN_POINT ( 'NONE',  ( 1.000000000000000000, -69.59657292934913642, 12.76848391599222765 ) ) ;
#66355 = COLOUR_RGB ( '', 0.31764706, 0.68627451, 0.89019608) ;
#66356 = AXIS2_PLACEMENT_3D ( 'NONE', #66938, #59386, #99819 ) ;
#66357 = CONICAL_SURFACE ( 'NONE', #102559, 4.000000000000000000, 0.9599310885968912466 ) ;
#66358 = VERTEX_POINT ( 'NONE', #14853 ) ;
#66359 = CARTESIAN_POINT ( 'NONE',  ( -17.50000000000567368, 50.03761058180953825, 61.36442103424013794 ) ) ;
#66360 = DIRECTION ( 'NONE',  ( 0.000000000000000000, 0.000000000000000000, 1.000000000000000000 ) ) ;
#66361 = AXIS2_PLACEMENT_3D ( 'NONE', #78809, #13540, #46457 ) ;
#66362 = CARTESIAN_POINT ( 'NONE',  ( 37.71459991402549861, 437.7716825518404562, 4.505118785439984563 ) ) ;
#66363 = EDGE_CURVE ( 'NONE', #42192, #61003, #4606, .T. ) ;
#66365 = CARTESIAN_POINT ( 'NONE',  ( 41.98975166001473980, -60.22823911148290676, -33.55402375021320438 ) ) ;
#66364 = DIRECTION ( 'NONE',  ( 0.000000000000000000, -1.000000000000000000, 0.000000000000000000 ) ) ;
#66366 = ORIENTED_EDGE ( 'NONE', *, *, #255, .F. ) ;
#66367 = CARTESIAN_POINT ( 'NONE',  ( -5.382057749264594904, -87.99826798403947237, -2.659775980967107767 ) ) ;
#66368 = SURFACE_STYLE_USAGE ( .BOTH. , #18380 ) ;
#66369 = VERTEX_POINT ( 'NONE', #26714 ) ;
#66370 = EDGE_CURVE ( 'NONE', #7616, #3716, #67962, .T. ) ;
#66371 = DIRECTION ( 'NONE',  ( -0.000000000000000000, -1.000000000000000000, -0.000000000000000000 ) ) ;
#66372 = CARTESIAN_POINT ( 'NONE',  ( -33.00000000000000000, 500.0000000000002274, 0.000000000000000000 ) ) ;
#66373 = CARTESIAN_POINT ( 'NONE',  ( -33.10889724926384758, 40.69544138183375992, -62.12314050178786573 ) ) ;
#66374 = CARTESIAN_POINT ( 'NONE',  ( -95.53046091001213824, -60.00000000000000000, 52.81045404649977115 ) ) ;
#66375 = CARTESIAN_POINT ( 'NONE',  ( 28.79508601474799789, 15.38969543640854987, -41.74367987815723779 ) ) ;
#66376 = CARTESIAN_POINT ( 'NONE',  ( -16.14595037822607182, 6.785770140110558124, 6.193810554580664984 ) ) ;
#66377 = CARTESIAN_POINT ( 'NONE',  ( 23.95564068939877345, 305.6666757346319514, -9.824255363917307804 ) ) ;
#66378 = CARTESIAN_POINT ( 'NONE',  ( 35.59999999999999432, 1.533819458162526451E-15, 0.000000000000000000 ) ) ;
#66380 = CARTESIAN_POINT ( 'NONE',  ( 30.00000000000000355, 489.3008774416947517, 5.491695563546554304 ) ) ;
#66379 = CARTESIAN_POINT ( 'NONE',  ( 1.308996937480706890, -4.999999999999988454, -95.00000000000001421 ) ) ;
#66381 = CARTESIAN_POINT ( 'NONE',  ( -82.14756253037036515, -49.98515285713766332, 178.0770026145764291 ) ) ;
#66382 = ORIENTED_EDGE ( 'NONE', *, *, #99929, .T. ) ;
#66383 = CARTESIAN_POINT ( 'NONE',  ( 5.308064239167483045, 41.67430808361709182, -70.56675995020944470 ) ) ;
#66384 = ADVANCED_FACE ( 'NONE', ( #68193 ), #9811, .T. ) ;
#66385 = EDGE_LOOP ( 'NONE', ( #93910, #30553, #74869, #3237 ) ) ;
#66386 = VECTOR ( 'NONE', #58942, 1000.000000000000000 ) ;
#66387 = ORIENTED_EDGE ( 'NONE', *, *, #45110, .T. ) ;
#66388 = LINE ( 'NONE', #80967, #52661 ) ;
#66389 = CARTESIAN_POINT ( 'NONE',  ( 4.250000000000000000, 0.000000000000000000, -0.5505556536572887572 ) ) ;
#66390 = ORIENTED_EDGE ( 'NONE', *, *, #61722, .T. ) ;
#66391 = DIRECTION ( 'NONE',  ( 0.000000000000000000, -1.000000000000000000, 0.000000000000000000 ) ) ;
#66392 = CARTESIAN_POINT ( 'NONE',  ( -2.826893917877371987, -57.67120211504744987, -44.61186535421596489 ) ) ;
#66393 = DIRECTION ( 'NONE',  ( -1.000000000000000000, -1.224606353822377258E-16, -0.000000000000000000 ) ) ;
#66394 = CARTESIAN_POINT ( 'NONE',  ( -7.551560007654699369, -61.99089648193008628, -2.648022159607837267 ) ) ;
#66395 = CARTESIAN_POINT ( 'NONE',  ( -3.400000000000000355, 4.163799117101001052E-16, -3.852324522925831385 ) ) ;
#66396 = DIRECTION ( 'NONE',  ( 0.000000000000000000, -1.000000000000000000, 0.000000000000000000 ) ) ;
#66397 = CARTESIAN_POINT ( 'NONE',  ( 43.50377727019363050, 435.9167426301696082, 18.24083946424737590 ) ) ;
#66398 = CARTESIAN_POINT ( 'NONE',  ( 106.5496036037455809, -14.21045842199433373, 161.7522804960935900 ) ) ;
#66399 = CARTESIAN_POINT ( 'NONE',  ( -109.3240689110004524, -30.00000000000000355, 163.9542341103382057 ) ) ;
#66400 = CARTESIAN_POINT ( 'NONE',  ( -59.58922826906859171, -29.07209130795614271, 66.35028759016553579 ) ) ;
#66401 = ORIENTED_EDGE ( 'NONE', *, *, #106403, .T. ) ;
#66402 = CARTESIAN_POINT ( 'NONE',  ( -11.60300946697521063, 38.95405707135367379, 62.66999883219498457 ) ) ;
#66403 = CARTESIAN_POINT ( 'NONE',  ( 110.2524109620066355, -59.99999999998756550, 196.4786846540791316 ) ) ;
#66404 = ORIENTED_EDGE ( 'NONE', *, *, #87071, .T. ) ;
#66405 = CARTESIAN_POINT ( 'NONE',  ( 8.225526725709833897, -46.43474543944358857, 31.62224987670555976 ) ) ;
#66406 = CARTESIAN_POINT ( 'NONE',  ( -101.8692908878811352, -45.26559888734792025, 144.5090998712010162 ) ) ;
#66407 = CARTESIAN_POINT ( 'NONE',  ( -2.977408999572650039, -16.06250000204838457, -7.188101187500000933 ) ) ;
#66408 =( NAMED_UNIT ( * ) SI_UNIT ( $, .STERADIAN. ) SOLID_ANGLE_UNIT ( ) );
#66409 = CARTESIAN_POINT ( 'NONE',  ( 18.86650669486618881, 1.474610560812782335E-15, 0.000000000000000000 ) ) ;
#66410 = VERTEX_POINT ( 'NONE', #85449 ) ;
#66411 = CARTESIAN_POINT ( 'NONE',  ( 31.96671797320279396, 484.9925651024516355, 5.143045411173839732 ) ) ;
#66412 = CIRCLE ( 'NONE', #64649, 0.5000000000000004441 ) ;
#66413 = CARTESIAN_POINT ( 'NONE',  ( -74.49046798774418221, -60.00000000000002842, 177.0422497158886870 ) ) ;
#66414 =( NAMED_UNIT ( * ) SI_UNIT ( $, .STERADIAN. ) SOLID_ANGLE_UNIT ( ) );
#66415 = CARTESIAN_POINT ( 'NONE',  ( -2.977408999572650039, -19.06250000204838813, -7.188101187500001821 ) ) ;
#66416 = CARTESIAN_POINT ( 'NONE',  ( 32.45623693501995888, 464.7023894946350993, 16.04003527243817473 ) ) ;
#66417 = CARTESIAN_POINT ( 'NONE',  ( 0.000000000000000000, 3.000000000000002665, 12.00000000000003908 ) ) ;
#66418 = CARTESIAN_POINT ( 'NONE',  ( -10.93463539379134630, -4.991620506566409432, -12.57231523659326555 ) ) ;
#66419 = CARTESIAN_POINT ( 'NONE',  ( -32.18412820475297309, 464.7176420235863361, 10.95006602420806985 ) ) ;
#66420 = CARTESIAN_POINT ( 'NONE',  ( 21.09715123528542691, 1.340359594676612611E-15, 0.000000000000000000 ) ) ;
#66421 = CARTESIAN_POINT ( 'NONE',  ( -24.42584379203423950, 27.59191556861859596, 31.59852321640927642 ) ) ;
#66422 = EDGE_CURVE ( 'NONE', #58075, #36, #98890, .T. ) ;
#66423 = AXIS2_PLACEMENT_3D ( 'NONE', #3185, #26963, #76001 ) ;
#66424 = CARTESIAN_POINT ( 'NONE',  ( 104.7773608882266529, -59.99999999999998579, 148.0886741368902051 ) ) ;
#66425 = CARTESIAN_POINT ( 'NONE',  ( -33.27768848828844028, -36.02923593097368382, 33.82197891432520009 ) ) ;
#66426 = CARTESIAN_POINT ( 'NONE',  ( -2.228836330358908047, -49.81523274736686346, 102.4817230975880449 ) ) ;
#66427 = CARTESIAN_POINT ( 'NONE',  ( 43.39891897988977121, -53.34186061554017755, 45.35487243743281027 ) ) ;
#66428 = AXIS2_PLACEMENT_3D ( 'NONE', #100651, #44020, #75851 ) ;
#66429 = AXIS2_PLACEMENT_3D ( 'NONE', #50895, #27214, #84881 ) ;
#66430 =( NAMED_UNIT ( * ) SI_UNIT ( $, .STERADIAN. ) SOLID_ANGLE_UNIT ( ) );
#66431 = EDGE_LOOP ( 'NONE', ( #67745, #64375, #96565, #63283, #61427 ) ) ;
#66432 = EDGE_CURVE ( 'NONE', #14939, #1802, #20203, .T. ) ;
#66433 = CARTESIAN_POINT ( 'NONE',  ( 44.35776761200808238, 435.2162786697448382, 12.88191835534477647 ) ) ;
#66434 = CARTESIAN_POINT ( 'NONE',  ( -76.08373685344359671, -38.38310391996776616, 178.9727446662289481 ) ) ;
#66435 = PRESENTATION_LAYER_ASSIGNMENT (  '', '', ( #64749 ) ) ;
#66436 = VERTEX_POINT ( 'NONE', #93002 ) ;
#66438 = CARTESIAN_POINT ( 'NONE',  ( 40.73878142687892279, 503.7113041876743864, 10.19672445236252045 ) ) ;
#66437 = CARTESIAN_POINT ( 'NONE',  ( -33.00000000000000000, 450.0000000000002274, 13.20242257375370976 ) ) ;
#66439 = LINE ( 'NONE', #9782, #35463 ) ;
#66440 = FACE_OUTER_BOUND ( 'NONE', #94428, .T. ) ;
#66441 = CARTESIAN_POINT ( 'NONE',  ( -43.02661387979676988, 465.7449615347604208, 11.43319743843887082 ) ) ;
#66442 = CIRCLE ( 'NONE', #4459, 15.00000000000000711 ) ;
#66443 = DIRECTION ( 'NONE',  ( 0.000000000000000000, -1.000000000000000000, 0.000000000000000000 ) ) ;
#66444 = DIRECTION ( 'NONE',  ( -0.8191520442889884679, 1.003171929053520679E-16, 0.5735764363510508224 ) ) ;
#66445 = VECTOR ( 'NONE', #31407, 1000.000000000000000 ) ;
#66446 = CARTESIAN_POINT ( 'NONE',  ( -28.99999999999998934, 0.000000000000000000, 0.000000000000000000 ) ) ;
#66447 = CARTESIAN_POINT ( 'NONE',  ( 17.85237544995468895, 45.37579490857303455, 5.050174946722796321 ) ) ;
#66448 = CARTESIAN_POINT ( 'NONE',  ( 102.5207257002704608, -59.99999999999998579, 95.78292118410128353 ) ) ;
#66449 = CARTESIAN_POINT ( 'NONE',  ( 14.29190075645216851, 6.456385560668102208, -7.561819230143448145 ) ) ;
#66450 = AXIS2_PLACEMENT_3D ( 'NONE', #16943, #49820, #82725 ) ;
#66451 = AXIS2_PLACEMENT_3D ( 'NONE', #88638, #104822, #14730 ) ;
#66452 = FILL_AREA_STYLE_COLOUR ( '', #59445 ) ;
#66453 = ORIENTED_EDGE ( 'NONE', *, *, #78610, .F. ) ;
#66454 = EDGE_CURVE ( 'NONE', #29354, #33265, #40765, .T. ) ;
#66455 = CARTESIAN_POINT ( 'NONE',  ( -100.5402992199712600, -29.99999999999999289, 182.6301088287440848 ) ) ;
#66456 = ORIENTED_EDGE ( 'NONE', *, *, #41645, .F. ) ;
#66457 = CARTESIAN_POINT ( 'NONE',  ( 25.85844197703628211, 37.16340362582887025, -8.997040705657223469 ) ) ;
#66458 = DIRECTION ( 'NONE',  ( 1.000000000000000000, 0.000000000000000000, 0.000000000000000000 ) ) ;
#66459 = CARTESIAN_POINT ( 'NONE',  ( 22.36190337224704550, 304.3302339434704322, 10.03999859912378589 ) ) ;
#66460 = DIRECTION ( 'NONE',  ( 0.000000000000000000, 0.000000000000000000, 1.000000000000000000 ) ) ;
#66461 = CARTESIAN_POINT ( 'NONE',  ( 2.977408999572651815, -19.81250000204838813, 7.188101187500000933 ) ) ;
#66462 = CARTESIAN_POINT ( 'NONE',  ( 6.400000000000000355, 0.000000000000000000, 0.000000000000000000 ) ) ;
#66463 = CARTESIAN_POINT ( 'NONE',  ( 0.000000000000000000, 0.000000000000000000, -8.500000000000000000 ) ) ;
#66465 = ORIENTED_EDGE ( 'NONE', *, *, #381, .F. ) ;
#66464 = DIRECTION ( 'NONE',  ( 0.000000000000000000, 0.000000000000000000, 1.000000000000000000 ) ) ;
#66466 = CARTESIAN_POINT ( 'NONE',  ( 83.26732716159929737, -36.00583431519718403, 166.7925075315839365 ) ) ;
#66467 = SURFACE_STYLE_FILL_AREA ( #49750 ) ;
#66468 = DIRECTION ( 'NONE',  ( -1.000000000000000000, -1.224606353822377258E-16, -0.000000000000000000 ) ) ;
#66469 = ORIENTED_EDGE ( 'NONE', *, *, #105785, .F. ) ;
#66470 = CARTESIAN_POINT ( 'NONE',  ( -62.09744855146975340, 49.99999999999997868, -11.13337886142409694 ) ) ;
#66471 = CARTESIAN_POINT ( 'NONE',  ( -46.81357782755159747, 18.41089473351688000, 15.91307620878805018 ) ) ;
#66472 = CARTESIAN_POINT ( 'NONE',  ( 2.977408999572650927, -9.875000002048388126, -7.188101187500000933 ) ) ;
#66473 = DIRECTION ( 'NONE',  ( -1.000000000000000000, -0.000000000000000000, -0.000000000000000000 ) ) ;
#66474 = CARTESIAN_POINT ( 'NONE',  ( 10.59999999999999609, -3.309499999999999886, 0.000000000000000000 ) ) ;
#66475 = CARTESIAN_POINT ( 'NONE',  ( -31.83737891999024328, 331.2472356323341387, 16.85379648827611376 ) ) ;
#66476 = CARTESIAN_POINT ( 'NONE',  ( -32.82247836200028956, 434.5280635633159250, 16.69909682737922552 ) ) ;
#66477 = ORIENTED_EDGE ( 'NONE', *, *, #56749, .F. ) ;
#66478 = FILL_AREA_STYLE ('',( #33605 ) ) ;
#66479 = CARTESIAN_POINT ( 'NONE',  ( -1.317676211347249549, 302.2248989068114611, 9.913061446930983678 ) ) ;
#66480 = CARTESIAN_POINT ( 'NONE',  ( 36.90124019532461119, 18.64284798592713344, 10.73407659160235639 ) ) ;
#66481 = CARTESIAN_POINT ( 'NONE',  ( 86.96106181210527097, -35.41080976886706821, 188.0754270986170695 ) ) ;
#66482 = CARTESIAN_POINT ( 'NONE',  ( 0.7777704900234801988, 34.98030770577876325, -27.51796982157703297 ) ) ;
#66483 = CARTESIAN_POINT ( 'NONE',  ( -2.977408999572654480, -33.12500000204838813, 7.188101187499999156 ) ) ;
#66484 = DIRECTION ( 'NONE',  ( 0.5735764363510462704, 0.8191520442889915765, 0.000000000000000000 ) ) ;
#66485 = DIRECTION ( 'NONE',  ( 1.000000000000000000, 0.000000000000000000, 0.000000000000000000 ) ) ;
#66486 = CYLINDRICAL_SURFACE ( 'NONE', #49469, 4.000000000000000000 ) ;
#66487 = AXIS2_PLACEMENT_3D ( 'NONE', #5481, #97651, #4957 ) ;
#66488 = ITEM_DEFINED_TRANSFORMATION ( 'NONE', 'NONE', #4199,  #10728 ) ;
#66489 = CARTESIAN_POINT ( 'NONE',  ( 48.02835407290544367, 11.61227450977237829, 14.35535821593427386 ) ) ;
#66490 = ORIENTED_EDGE ( 'NONE', *, *, #103971, .T. ) ;
#66491 = CARTESIAN_POINT ( 'NONE',  ( -36.87655955837857391, 438.2068510013161244, 3.933030107424709598 ) ) ;
#66492 = CARTESIAN_POINT ( 'NONE',  ( 13.44208458454186150, 42.84831587751688886, -92.02018896800140624 ) ) ;
#66493 = CARTESIAN_POINT ( 'NONE',  ( -10.03463480799099550, 7.450536368003703558, -5.000000000000017764 ) ) ;
#66494 = DIRECTION ( 'NONE',  ( 0.000000000000000000, 0.000000000000000000, 1.000000000000000000 ) ) ;
#66495 = EDGE_CURVE ( 'NONE', #5468, #39998, #71786, .T. ) ;
#66496 = CIRCLE ( 'NONE', #26968, 3.309500000000007880 ) ;
#66497 = ORIENTED_EDGE ( 'NONE', *, *, #66503, .T. ) ;
#66498 = DIRECTION ( 'NONE',  ( 0.000000000000000000, 0.000000000000000000, -1.000000000000000000 ) ) ;
#66499 = CARTESIAN_POINT ( 'NONE',  ( -30.00000000000469669, 464.1479708722390001, 11.53751907632628360 ) ) ;
#66500 = CARTESIAN_POINT ( 'NONE',  ( -7.500000000000005329, 44.25000000000000000, -68.91429205785459544 ) ) ;
#66501 = CARTESIAN_POINT ( 'NONE',  ( 113.5519812807844033, -57.67142723623354073, 158.0961491198512476 ) ) ;
#66502 = MECHANICAL_DESIGN_GEOMETRIC_PRESENTATION_REPRESENTATION (  '', ( #75106 ), #94077 ) ;
#66503 = EDGE_CURVE ( 'NONE', #29837, #93080, #51075, .T. ) ;
#66504 = EDGE_CURVE ( 'NONE', #77823, #33833, #100021, .T. ) ;
#66505 = DIRECTION ( 'NONE',  ( 0.000000000000000000, -1.000000000000000000, 0.000000000000000000 ) ) ;
#66506 = CARTESIAN_POINT ( 'NONE',  ( 3.464434906260568603, 15.83682371743314476, 6.084749395801797078 ) ) ;
#66507 = CARTESIAN_POINT ( 'NONE',  ( 2.850615045022827587, -4.999999999999999112, -72.23577364510627774 ) ) ;
#66508 = AXIS2_PLACEMENT_3D ( 'NONE', #4653, #68868, #86652 ) ;
#66509 = CARTESIAN_POINT ( 'NONE',  ( 36.34557008114963139, 26.08151611875061349, 11.89035452524019476 ) ) ;
#66510 = CARTESIAN_POINT ( 'NONE',  ( -86.36548893003080707, -60.00000000000000711, 200.7376711920367143 ) ) ;
#66511 = AXIS2_PLACEMENT_3D ( 'NONE', #18450, #91271, #42699 ) ;
#66512 = AXIS2_PLACEMENT_3D ( 'NONE', #92403, #18551, #75693 ) ;
#66513 = DIRECTION ( 'NONE',  ( 0.000000000000000000, 0.000000000000000000, -1.000000000000000000 ) ) ;
#66514 = CARTESIAN_POINT ( 'NONE',  ( 89.99999999999997158, 500000.0000000000582, 196.0238439516549818 ) ) ;
#66515 = CARTESIAN_POINT ( 'NONE',  ( -24.37088254901632567, 295.3567874699774620, -9.892597027136796228 ) ) ;
#66516 = CARTESIAN_POINT ( 'NONE',  ( -84.33089495578791173, -42.97883097878487035, 183.3478449006408937 ) ) ;
#66517 = VERTEX_POINT ( 'NONE', #76807 ) ;
#66518 = CARTESIAN_POINT ( 'NONE',  ( 23.73340390206779560, 305.5981197995496927, -9.839287018817417518 ) ) ;
#66519 = AXIS2_PLACEMENT_3D ( 'NONE', #61067, #93962, #20112 ) ;
#66520 = EDGE_CURVE ( 'NONE', #86885, #45510, #83840, .T. ) ;
#66521 = CONICAL_SURFACE ( 'NONE', #97526, 4.172000000000001485, 0.9599310885968750373 ) ;
#66522 = ORIENTED_EDGE ( 'NONE', *, *, #68044, .T. ) ;
#66523 = CARTESIAN_POINT ( 'NONE',  ( -7.002641335706727865, -11.05087262680832971, 3.868676264653292396 ) ) ;
#66524 = CARTESIAN_POINT ( 'NONE',  ( 7.347880794884118356E-15, 0.000000000000000000, -60.00000000000000000 ) ) ;
#66525 = CARTESIAN_POINT ( 'NONE',  ( -83.21592982314025733, -37.80011021608530797, -4.677426421150369329 ) ) ;
#66526 = CARTESIAN_POINT ( 'NONE',  ( -4.698242434196084893, -14.20142765657231543, -8.220922734484002348 ) ) ;
#66527 = VECTOR ( 'NONE', #18335, 999.9999999999998863 ) ;
#66528 = CARTESIAN_POINT ( 'NONE',  ( -4.036417550650834407, 14.45404279547049065, -5.000000000000000888 ) ) ;
#66529 = DIRECTION ( 'NONE',  ( 0.000000000000000000, 1.000000000000000000, 0.000000000000000000 ) ) ;
#66530 = CARTESIAN_POINT ( 'NONE',  ( -32.28552837373661077, 464.7648866755938570, 15.30384310834759987 ) ) ;
#66531 = LINE ( 'NONE', #47677, #20968 ) ;
#66532 = CARTESIAN_POINT ( 'NONE',  ( -7.290763246116595115E-15, 7.666536031838887766, 59.53359981990485750 ) ) ;
#66533 = CARTESIAN_POINT ( 'NONE',  ( -36.14862957314523584, 438.2394791802965983, 3.891583768390257880 ) ) ;
#66534 = CARTESIAN_POINT ( 'NONE',  ( -55.21321105934377726, -60.00000000000002842, -39.23988760269474341 ) ) ;
#66535 = CARTESIAN_POINT ( 'NONE',  ( -76.67228451078059948, -32.55182850295351216, 122.5207825894436979 ) ) ;
#66536 = VERTEX_POINT ( 'NONE', #26192 ) ;
#66537 = CARTESIAN_POINT ( 'NONE',  ( 75.43375447319739635, -30.00000000000006395, 160.3035121353613306 ) ) ;
#66538 = CARTESIAN_POINT ( 'NONE',  ( 7.801642220026312025, 88.58796826149033166, 1.787233835843583973 ) ) ;
#66539 = CARTESIAN_POINT ( 'NONE',  ( 94.03892859735442755, -57.67587636535527906, 4.912622737924200678 ) ) ;
#66540 = VERTEX_POINT ( 'NONE', #51471 ) ;
#66541 = CARTESIAN_POINT ( 'NONE',  ( 7.465554980039875943, 52.17267064398219389, -2.153157956675398665 ) ) ;
#66542 = FACE_OUTER_BOUND ( 'NONE', #42187, .T. ) ;
#66543 = VERTEX_POINT ( 'NONE', #91422 ) ;
#66544 = CIRCLE ( 'NONE', #28710, 5.000000000000002665 ) ;
#66545 = CARTESIAN_POINT ( 'NONE',  ( 0.000000000000000000, 2.999999999999992450, 0.000000000000000000 ) ) ;
#66546 = DIRECTION ( 'NONE',  ( 1.000000000000000000, 1.224606353822377258E-16, 0.000000000000000000 ) ) ;
#66547 = CARTESIAN_POINT ( 'NONE',  ( 7.188101187500000044, -10.15625000204838457, 0.000000000000000000 ) ) ;
#66548 = CARTESIAN_POINT ( 'NONE',  ( -19.99999999999999289, -5.000000000000000000, 25.00000000000000000 ) ) ;
#66549 = CARTESIAN_POINT ( 'NONE',  ( 3.352941176470599860, -1.200583151104954061, 104.5794940929807524 ) ) ;
#66550 = CARTESIAN_POINT ( 'NONE',  ( 54.03872891708841308, 6.856755485862130937E-15, 0.000000000000000000 ) ) ;
#66551 = LINE ( 'NONE', #18017, #21026 ) ;
#66552 = CARTESIAN_POINT ( 'NONE',  ( 33.09999999999999432, 3.309500000000003439, 0.000000000000000000 ) ) ;
#66553 = DIRECTION ( 'NONE',  ( 0.000000000000000000, -1.000000000000000000, 0.000000000000000000 ) ) ;
#66554 = EDGE_CURVE ( 'NONE', #62246, #88153, #49378, .T. ) ;
#66555 = VERTEX_POINT ( 'NONE', #27787 ) ;
#66556 = CARTESIAN_POINT ( 'NONE',  ( -7.187173619203170993, 40.29457790443799325, -70.92326292136544907 ) ) ;
#66557 = CARTESIAN_POINT ( 'NONE',  ( 28.36086065759023001, -22.10831334729735431, 29.53362645638507544 ) ) ;
#66558 = CARTESIAN_POINT ( 'NONE',  ( 32.93903373786918110, 323.1113853486734797, -4.529746964764728823 ) ) ;
#66559 = ORIENTED_EDGE ( 'NONE', *, *, #90069, .F. ) ;
#66560 = EDGE_CURVE ( 'NONE', #100726, #88549, #60661, .T. ) ;
#66561 = EDGE_CURVE ( 'NONE', #93450, #97465, #76962, .T. ) ;
#66562 = CARTESIAN_POINT ( 'NONE',  ( -0.7710323107892651517, 18.23550529380447927, 49.51187434724097614 ) ) ;
#66563 = VERTEX_POINT ( 'NONE', #53601 ) ;
#66565 = CARTESIAN_POINT ( 'NONE',  ( -9.743117168496159053, -5.000000000000000000, -2.583982984173456288 ) ) ;
#66564 = CARTESIAN_POINT ( 'NONE',  ( 0.000000000000000000, 50.00000000000000000, 0.000000000000000000 ) ) ;
#66566 = CARTESIAN_POINT ( 'NONE',  ( 16.64348903516523848, 45.88445698070336221, 4.157797401561420081 ) ) ;
#66567 = DIRECTION ( 'NONE',  ( 0.000000000000000000, 1.000000000000000000, 0.000000000000000000 ) ) ;
#66568 = FACE_BOUND ( 'NONE', #90531, .T. ) ;
#66569 = DIRECTION ( 'NONE',  ( -0.9502668926229251856, 0.000000000000000000, 0.3114367235647877430 ) ) ;
#66570 = CARTESIAN_POINT ( 'NONE',  ( -35.20412044861406997, 463.4819191117596233, 19.77841787011475105 ) ) ;
#66571 = ORIENTED_EDGE ( 'NONE', *, *, #98111, .T. ) ;
#66572 = CARTESIAN_POINT ( 'NONE',  ( 86.86402307942935863, -60.00000000000000711, -22.80661258863997176 ) ) ;
#66573 = CIRCLE ( 'NONE', #94140, 9.000000000000000000 ) ;
#66574 = CARTESIAN_POINT ( 'NONE',  ( -11.53045486031949807, 45.53936973856495030, -13.95636496209362143 ) ) ;
#66575 = FILL_AREA_STYLE ('',( #74650 ) ) ;
#66576 = DIRECTION ( 'NONE',  ( 0.5735764363510440500, 0.8191520442889932418, 0.000000000000000000 ) ) ;
#66577 = ADVANCED_FACE ( 'NONE', ( #77888 ), #102689, .T. ) ;
#66578 =( BOUNDED_SURFACE ( )  B_SPLINE_SURFACE ( 3, 2, ( 
 ( #70251, #4446, #104193 ),
 ( #86980, #77815, #44385 ),
 ( #103152, #103675, #37390 ),
 ( #93474, #62186, #19624 ),
 ( #13050, #20696, #28775 ),
 ( #45455, #102073, #29820 ),
 ( #11459, #28234, #69725 ),
 ( #29298, #44930, #71301 ),
 ( #53004, #102617, #95072 ),
 ( #37919, #45980, #4988 ),
 ( #36335, #77280, #62698 ),
 ( #95590, #21726, #78859 ),
 ( #70780, #30337, #54568 ),
 ( #61654, #79394, #20154 ),
 ( #46500, #87504, #53534 ),
 ( #94544, #85926, #86464 ),
 ( #13584, #36857, #5511 ),
 ( #38435, #52457, #12522 ),
 ( #85374, #3392, #69204 ),
 ( #61106, #11998, #78330 ),
 ( #14639, #82034, #88033 ),
 ( #63230, #96122, #31928 ),
 ( #105266, #89620, #97161 ),
 ( #6026, #15183, #71827 ),
 ( #48604, #14113, #104731 ),
 ( #8158, #72877, #47547 ),
 ( #98229, #22785, #72362 ),
 ( #96650, #7609, #15718 ),
 ( #89088, #38949, #47016 ),
 ( #48072, #32468, #65338 ),
 ( #39487, #105789, #73948 ),
 ( #22254, #40005, #24384 ),
 ( #40528, #55103, #6553 ),
 ( #31413, #88558, #80973 ),
 ( #57225, #30882, #23309 ),
 ( #63760, #90144, #16247 ),
 ( #97688, #64806, #64290 ),
 ( #79918, #23852, #55621 ) ),
 .UNSPECIFIED., .F., .F., .F. ) 
 B_SPLINE_SURFACE_WITH_KNOTS ( ( 4, 2, 2, 2, 2, 2, 2, 2, 2, 2, 2, 2, 2, 2, 2, 2, 2, 2, 4 ),
 ( 3, 3 ),
 ( 0.06375477930561496143, 0.06591736287010036000, 0.06807994643458575856, 0.07240511356355655570, 0.07673028069252735284, 0.08105544782149814997, 0.08970578207943974425, 0.09835611633738133852, 0.1156567848532645271, 0.1329574533691477156, 0.1502581218850309042, 0.1675587904009140927, 0.1762091246588556870, 0.1848594589167972813, 0.1891846260457680784, 0.1935097931747388755, 0.1978349603037096727, 0.1999975438681950712, 0.2021601274326804976 ),
 ( 0.000000000000000000, 1.000000000000000000 ),
 .UNSPECIFIED. ) 
 GEOMETRIC_REPRESENTATION_ITEM ( )  RATIONAL_B_SPLINE_SURFACE ( (
 ( 1.000000000000000000, 0.7071067811865475727, 1.000000000000000000),
 ( 1.000000000000000000, 0.7071067811865475727, 1.000000000000000000),
 ( 1.000000000000000000, 0.7071067811865475727, 1.000000000000000000),
 ( 1.000000000000000000, 0.7071067811865475727, 1.000000000000000000),
 ( 1.000000000000000000, 0.7071067811865475727, 1.000000000000000000),
 ( 1.000000000000000000, 0.7071067811865475727, 1.000000000000000000),
 ( 1.000000000000000000, 0.7071067811865475727, 1.000000000000000000),
 ( 1.000000000000000000, 0.7071067811865475727, 1.000000000000000000),
 ( 1.000000000000000000, 0.7071067811865475727, 1.000000000000000000),
 ( 1.000000000000000000, 0.7071067811865475727, 1.000000000000000000),
 ( 1.000000000000000000, 0.7071067811865474617, 1.000000000000000000),
 ( 1.000000000000000000, 0.7071067811865474617, 1.000000000000000000),
 ( 1.000000000000000000, 0.7071067811865474617, 1.000000000000000000),
 ( 1.000000000000000000, 0.7071067811865474617, 1.000000000000000000),
 ( 1.000000000000000000, 0.7071067811865475727, 1.000000000000000000),
 ( 1.000000000000000000, 0.7071067811865475727, 1.000000000000000000),
 ( 1.000000000000000000, 0.7071067811865475727, 1.000000000000000000),
 ( 1.000000000000000000, 0.7071067811865475727, 1.000000000000000000),
 ( 1.000000000000000000, 0.7071067811865475727, 1.000000000000000000),
 ( 1.000000000000000000, 0.7071067811865475727, 1.000000000000000000),
 ( 1.000000000000000000, 0.7071067811865475727, 1.000000000000000000),
 ( 1.000000000000000000, 0.7071067811865475727, 1.000000000000000000),
 ( 1.000000000000000000, 0.7071067811865475727, 1.000000000000000000),
 ( 1.000000000000000000, 0.7071067811865475727, 1.000000000000000000),
 ( 1.000000000000000000, 0.7071067811865475727, 1.000000000000000000),
 ( 1.000000000000000000, 0.7071067811865475727, 1.000000000000000000),
 ( 1.000000000000000000, 0.7071067811865475727, 1.000000000000000000),
 ( 1.000000000000000000, 0.7071067811865475727, 1.000000000000000000),
 ( 1.000000000000000000, 0.7071067811865475727, 1.000000000000000000),
 ( 1.000000000000000000, 0.7071067811865475727, 1.000000000000000000),
 ( 1.000000000000000000, 0.7071067811865475727, 1.000000000000000000),
 ( 1.000000000000000000, 0.7071067811865475727, 1.000000000000000000),
 ( 1.000000000000000000, 0.7071067811865475727, 1.000000000000000000),
 ( 1.000000000000000000, 0.7071067811865475727, 1.000000000000000000),
 ( 1.000000000000000000, 0.7071067811865475727, 1.000000000000000000),
 ( 1.000000000000000000, 0.7071067811865475727, 1.000000000000000000),
 ( 1.000000000000000000, 0.7071067811865475727, 1.000000000000000000),
 ( 1.000000000000000000, 0.7071067811865475727, 1.000000000000000000) ) ) 
 REPRESENTATION_ITEM ( '' )  SURFACE ( )  );
#66579 = CARTESIAN_POINT ( 'NONE',  ( 24.63846153846153797, -4.171999999999999709, 5.616230220889763424E-16 ) ) ;
#66580 = ORIENTED_EDGE ( 'NONE', *, *, #82743, .T. ) ;
#66581 = AXIS2_PLACEMENT_3D ( 'NONE', #100181, #34952, #58123 ) ;
#66582 = EDGE_CURVE ( 'NONE', #29335, #78409, #97649, .T. ) ;
#66583 = CARTESIAN_POINT ( 'NONE',  ( -42.51195073777072508, 462.6463319774571232, 3.762330311937251981 ) ) ;
#66584 = ORIENTED_EDGE ( 'NONE', *, *, #39960, .F. ) ;
#66585 = EDGE_LOOP ( 'NONE', ( #96660, #10460, #42726, #103843 ) ) ;
#66586 = FACE_OUTER_BOUND ( 'NONE', #54969, .T. ) ;
#66587 = CARTESIAN_POINT ( 'NONE',  ( -15.52500069721948250, 34.97057647050228013, -22.76630647231286275 ) ) ;
#66588 = CARTESIAN_POINT ( 'NONE',  ( 83.19617777001812442, -37.83149000724398547, -4.129211925961556062 ) ) ;
#66589 = CARTESIAN_POINT ( 'NONE',  ( -33.34415954575715801, 315.0055737288411137, -7.094410410514097265 ) ) ;
#66590 = CARTESIAN_POINT ( 'NONE',  ( -13.58756192037751198, 304.5480426539326118, -9.064568272891900591 ) ) ;
#66591 = CARTESIAN_POINT ( 'NONE',  ( 12.50000000000000711, 27.21546065502551315, -44.75725117832055133 ) ) ;
#66592 = ORIENTED_EDGE ( 'NONE', *, *, #15113, .F. ) ;
#66593 = EDGE_CURVE ( 'NONE', #20213, #27454, #92430, .T. ) ;
#66594 = CARTESIAN_POINT ( 'NONE',  ( -9.040072111321892478, 43.92509090302731067, 14.03063673340002993 ) ) ;
#66595 = ORIENTED_EDGE ( 'NONE', *, *, #71867, .T. ) ;
#66596 = CARTESIAN_POINT ( 'NONE',  ( 9.797545558212032546, 51.31160919791983588, -2.589760350952462709 ) ) ;
#66597 = CONICAL_SURFACE ( 'NONE', #80359, 4.172000000000001485, 0.9599310885968750373 ) ;
#66598 = VECTOR ( 'NONE', #103153, 1000.000000000000000 ) ;
#66599 = EDGE_CURVE ( 'NONE', #91139, #93494, #35656, .T. ) ;
#66601 = ORIENTED_EDGE ( 'NONE', *, *, #13566, .F. ) ;
#66600 = CARTESIAN_POINT ( 'NONE',  ( 6.133952071448687704, 51.27085470495629949, 8.207115774551422049 ) ) ;
#66602 = CARTESIAN_POINT ( 'NONE',  ( 68.45974218760680685, -22.10775288249442383, 87.18709934866549816 ) ) ;
#66603 = VECTOR ( 'NONE', #90957, 1000.000000000000000 ) ;
#66604 = ORIENTED_EDGE ( 'NONE', *, *, #55218, .T. ) ;
#66605 = CARTESIAN_POINT ( 'NONE',  ( 17.50000000000002487, 49.38220963225677451, 64.00838255298897650 ) ) ;
#66606 = AXIS2_PLACEMENT_3D ( 'NONE', #22379, #5625, #5104 ) ;
#66607 = CARTESIAN_POINT ( 'NONE',  ( -1.320432766682874540E-15, -22.53125000204838457, 7.188101187500000044 ) ) ;
#66608 = CARTESIAN_POINT ( 'NONE',  ( -113.5594301016874539, -57.67117831481159840, 184.0234983118591856 ) ) ;
#66609 = VERTEX_POINT ( 'NONE', #62255 ) ;
#66610 = CARTESIAN_POINT ( 'NONE',  ( 6.394337469123802187, -7.552703473009535706, 4.547976812830884136E-16 ) ) ;
#66611 = CARTESIAN_POINT ( 'NONE',  ( 102.6967805458878047, -37.84840159047918462, 167.9561026369516128 ) ) ;
#66612 = CARTESIAN_POINT ( 'NONE',  ( -37.08530234603140485, 491.4084519804401907, 12.30481897466476049 ) ) ;
#66613 = LINE ( 'NONE', #16466, #5046 ) ;
#66614 = CARTESIAN_POINT ( 'NONE',  ( -8.000000000000001776, -26.84375000409676915, 3.313708498984758943 ) ) ;
#66615 = CARTESIAN_POINT ( 'NONE',  ( 43.03185303983483578, 485.3613526602390493, 6.073233449168488285 ) ) ;
#66616 = DIRECTION ( 'NONE',  ( -1.000000000000000000, -1.224606353822377258E-16, -0.000000000000000000 ) ) ;
#66617 = CIRCLE ( 'NONE', #56271, 4.000000000000000888 ) ;
#66618 = CARTESIAN_POINT ( 'NONE',  ( 9.176803346051508825, 30.52947155797438583, 3.973598758023531019 ) ) ;
#66619 = CARTESIAN_POINT ( 'NONE',  ( 6.943482370013978944, -9.471516297392756911, 3.973876482044364611 ) ) ;
#66620 = DIRECTION ( 'NONE',  ( 0.000000000000000000, 0.000000000000000000, 1.000000000000000000 ) ) ;
#66621 = CARTESIAN_POINT ( 'NONE',  ( -2.455962139888511420, 15.75268258782372754, -9.700350089084256666 ) ) ;
#66622 = ORIENTED_EDGE ( 'NONE', *, *, #30299, .T. ) ;
#66623 = CARTESIAN_POINT ( 'NONE',  ( 43.60098212335665124, 434.9832094534187377, 14.46717338012452458 ) ) ;
#66624 = DIRECTION ( 'NONE',  ( -1.000000000000000000, -0.000000000000000000, -0.000000000000000000 ) ) ;
#66625 = AXIS2_PLACEMENT_3D ( 'NONE', #68013, #10815, #100898 ) ;
#66626 = CARTESIAN_POINT ( 'NONE',  ( 9.217957586093081801, -59.99999999999999289, 39.64182104935679263 ) ) ;
#66627 = CARTESIAN_POINT ( 'NONE',  ( -98.33419151583822782, -30.00000000000000000, 190.1125085183297756 ) ) ;
#66628 = EDGE_CURVE ( 'NONE', #6033, #76952, #58005, .T. ) ;
#66629 = ORIENTED_EDGE ( 'NONE', *, *, #66593, .T. ) ;
#66630 = VERTEX_POINT ( 'NONE', #94066 ) ;
#66631 = DIRECTION ( 'NONE',  ( -1.000000000000000000, -0.000000000000000000, -0.000000000000000000 ) ) ;
#66632 = CARTESIAN_POINT ( 'NONE',  ( 71.38313853796425690, -57.68021046702090615, 165.8956670029349993 ) ) ;
#66633 = CARTESIAN_POINT ( 'NONE',  ( -6.088311765594377256, 4.652913962454959140, 5.000000000000019540 ) ) ;
#66634 = EDGE_CURVE ( 'NONE', #75817, #63451, #94224, .T. ) ;
#66635 = ADVANCED_FACE ( 'NONE', ( #3999 ), #68356, .F. ) ;
#66636 = CARTESIAN_POINT ( 'NONE',  ( 19.32074472756938022, -25.58899134302987122, -38.49253709561221370 ) ) ;
#66637 = CARTESIAN_POINT ( 'NONE',  ( -1.100143057407436675, 43.84113189085540085, 16.88562200540562941 ) ) ;
#66638 = CARTESIAN_POINT ( 'NONE',  ( -41.58908019493902231, 487.6887286007228681, 9.912025820238323348 ) ) ;
#66639 = CARTESIAN_POINT ( 'NONE',  ( -46.17444693964949920, -60.00000000000000711, 63.00263890028006131 ) ) ;
#66640 = MECHANICAL_DESIGN_GEOMETRIC_PRESENTATION_REPRESENTATION (  '', ( #77035 ), #56296 ) ;
#66641 = DIRECTION ( 'NONE',  ( -0.5735764363510494901, -0.8191520442889894671, 0.000000000000000000 ) ) ;
#66642 = CARTESIAN_POINT ( 'NONE',  ( 0.7784210542099400110, 45.39571455979881165, -18.48152473499649773 ) ) ;
#66643 = AXIS2_PLACEMENT_3D ( 'NONE', #102154, #13659, #45531 ) ;
#66644 = CARTESIAN_POINT ( 'NONE',  ( -86.97243100496625345, -42.77928646493604958, 189.9052986841667519 ) ) ;
#66645 = ORIENTED_EDGE ( 'NONE', *, *, #38414, .T. ) ;
#66646 = LINE ( 'NONE', #65051, #65988 ) ;
#66647 = CARTESIAN_POINT ( 'NONE',  ( -9.120514393641915518, -29.03121919898077863, 28.72967367393797389 ) ) ;
#66648 = ADVANCED_FACE ( 'NONE', ( #28304 ), #90753, .T. ) ;
#66649 = ADVANCED_FACE ( 'NONE', ( #37463 ), #104522, .T. ) ;
#66650 = CARTESIAN_POINT ( 'NONE',  ( -5.668939695963768344, 41.88723863199725628, -59.02759498664629945 ) ) ;
#66651 = CARTESIAN_POINT ( 'NONE',  ( 42.33349330513380693, 1.593028355512270567E-15, 0.000000000000000000 ) ) ;
#66653 = CARTESIAN_POINT ( 'NONE',  ( 5.053417956347306728, -64.34077225747144269, 13.91206720744365910 ) ) ;
#66652 = CARTESIAN_POINT ( 'NONE',  ( 4.574783636564311529, -5.228990388888064444, -6.171384342982683791 ) ) ;
#66654 = ORIENTED_EDGE ( 'NONE', *, *, #86669, .F. ) ;
#66655 = CARTESIAN_POINT ( 'NONE',  ( 26.78690032903771012, 34.58979447066111845, 10.02622625454039529 ) ) ;
#66656 = DIRECTION ( 'NONE',  ( -1.000000000000000000, -0.000000000000000000, -0.000000000000000000 ) ) ;
#66657 = CARTESIAN_POINT ( 'NONE',  ( -7.412906595240166929, 32.64188272852253903, 3.014362223629236670 ) ) ;
#66658 = AXIS2_PLACEMENT_3D ( 'NONE', #21577, #46874, #71154 ) ;
#66659 = CARTESIAN_POINT ( 'NONE',  ( 30.43355426543545406, 298.0544874283102104, -1.294920856760706673 ) ) ;
#66660 = LINE ( 'NONE', #32727, #67429 ) ;
#66661 = FACE_OUTER_BOUND ( 'NONE', #57953, .T. ) ;
#66662 = CARTESIAN_POINT ( 'NONE',  ( 32.13503062639011176, 486.0946171966414795, 5.282847667695620864 ) ) ;
#66663 = CARTESIAN_POINT ( 'NONE',  ( 106.6845404271915925, -14.21045842199438525, 180.1433801272770836 ) ) ;
#66664 = CARTESIAN_POINT ( 'NONE',  ( -81.94379596842044577, -39.49948281330256350, 160.0918886956195308 ) ) ;
#66665 = ORIENTED_EDGE ( 'NONE', *, *, #8078, .F. ) ;
#66666 = DIRECTION ( 'NONE',  ( 0.000000000000000000, 0.000000000000000000, -1.000000000000000000 ) ) ;
#66667 = DIRECTION ( 'NONE',  ( -1.000000000000000000, -1.224606353822377258E-16, -0.000000000000000000 ) ) ;
#66668 = STYLED_ITEM ( 'NONE', ( #6391 ), #58033 ) ;
#66669 = VECTOR ( 'NONE', #54312, 999.9999999999998863 ) ;
#66670 = CARTESIAN_POINT ( 'NONE',  ( -7.499940182180696802, -3.043015538681149934, -20.22995127276119476 ) ) ;
#66671 = CARTESIAN_POINT ( 'NONE',  ( 43.67907128098302394, 391.2096367011267262, 15.78583024887160136 ) ) ;
#66672 = CARTESIAN_POINT ( 'NONE',  ( 6.463344223170841119, -4.601472318010342732, 5.710032555828793654 ) ) ;
#66673 = EDGE_LOOP ( 'NONE', ( #47211, #30011, #9977, #96666 ) ) ;
#66674 = UNCERTAINTY_MEASURE_WITH_UNIT (LENGTH_MEASURE( 1.000000000000000082E-05 ), #91054, 'distance_accuracy_value', 'NONE');
#66675 = AXIS2_PLACEMENT_3D ( 'NONE', #69347, #102225, #61251 ) ;
#66677 = AXIS2_PLACEMENT_3D ( 'NONE', #7595, #55608, #74461 ) ;
#66676 = CARTESIAN_POINT ( 'NONE',  ( -19.83463548332446535, 303.8035096162419109, 9.926734387303330465 ) ) ;
#66678 = ORIENTED_EDGE ( 'NONE', *, *, #47857, .T. ) ;
#66679 = DIRECTION ( 'NONE',  ( -1.000000000000000000, -0.000000000000000000, -0.000000000000000000 ) ) ;
#66680 =( NAMED_UNIT ( * ) SI_UNIT ( $, .STERADIAN. ) SOLID_ANGLE_UNIT ( ) );
#66681 = DIRECTION ( 'NONE',  ( 0.000000000000000000, 0.000000000000000000, 1.000000000000000000 ) ) ;
#66682 = CARTESIAN_POINT ( 'NONE',  ( -63.03617022295203753, 48.00000000000000000, -16.93907820454660396 ) ) ;
#66683 = B_SPLINE_CURVE_WITH_KNOTS ( 'NONE', 3,
 ( #50005, #81816, #50520, #7942 ),
 .UNSPECIFIED., .F., .F.,
 ( 4, 4 ),
 ( 0.000000000000000000, 0.002170046543135659405 ),
 .UNSPECIFIED. ) ;
#66684 = CARTESIAN_POINT ( 'NONE',  ( 5.000000000000040856, -12.61682532716497640, 11.58371340991119958 ) ) ;
#66685 = CARTESIAN_POINT ( 'NONE',  ( 46.00000000000000000, 437.9173578870139636, 12.34179081168240799 ) ) ;
#66686 = ORIENTED_EDGE ( 'NONE', *, *, #62636, .F. ) ;
#66687 = CARTESIAN_POINT ( 'NONE',  ( 110.5157368889957610, -60.00000000000000000, 189.3796442602921672 ) ) ;
#66689 = CARTESIAN_POINT ( 'NONE',  ( 15.95816837728402149, -56.87732999964022440, 33.56976140312947621 ) ) ;
#66688 = CARTESIAN_POINT ( 'NONE',  ( -78.65018897216694427, -14.21045842199436571, 174.1869015730407000 ) ) ;
#66690 = CARTESIAN_POINT ( 'NONE',  ( 83.25561225319275138, -37.99999999999993605, -8.576613537955827482 ) ) ;
#66691 = CARTESIAN_POINT ( 'NONE',  ( -2.637755229554568666E-21, 53.39766064372320642, -10.24999999999999822 ) ) ;
#66692 = EDGE_CURVE ( 'NONE', #64398, #47413, #1167, .T. ) ;
#66693 = CARTESIAN_POINT ( 'NONE',  ( -41.45979221839193940, -46.43697368219972788, 41.56452721125755545 ) ) ;
#66694 = DIRECTION ( 'NONE',  ( -0.5735764363510494901, -0.8191520442889894671, 0.000000000000000000 ) ) ;
#66695 = EDGE_LOOP ( 'NONE', ( #6685, #20961, #18181, #15501, #18062 ) ) ;
#66696 = DIRECTION ( 'NONE',  ( 0.000000000000000000, -1.000000000000000000, 0.000000000000000000 ) ) ;
#66697 = CARTESIAN_POINT ( 'NONE',  ( 8.398900012642918966, 54.02103971888446665, 1.531152949374444239 ) ) ;
#66698 = CARTESIAN_POINT ( 'NONE',  ( 21.25502769577498796, 305.0480251235313176, 9.978840188629131802 ) ) ;
#66699 = CARTESIAN_POINT ( 'NONE',  ( -4.250000000000000000, 5.204748896376250699E-16, -9.078441367943003826 ) ) ;
#66700 = CARTESIAN_POINT ( 'NONE',  ( 4.898587196589412829E-16, -28.81250000409677270, -8.000000000000000000 ) ) ;
#66701 = CARTESIAN_POINT ( 'NONE',  ( -34.68355603894254813, 461.9758321905093226, 4.166121198602492193 ) ) ;
#66703 = ORIENTED_EDGE ( 'NONE', *, *, #48186, .T. ) ;
#66702 = STYLED_ITEM ( 'NONE', ( #48087 ), #29321 ) ;
#66704 = CARTESIAN_POINT ( 'NONE',  ( -45.30326460949155631, -38.31529918028564907, 58.49194340069017528 ) ) ;
#66705 = CARTESIAN_POINT ( 'NONE',  ( -9.999999999999982236, 7.499999999999973355, 0.000000000000000000 ) ) ;
#66706 = EDGE_LOOP ( 'NONE', ( #30409, #69760, #15842, #70813 ) ) ;
#66707 = CARTESIAN_POINT ( 'NONE',  ( 80.23011466839570005, -30.00000000000003197, -13.48167149206803295 ) ) ;
#66708 = CARTESIAN_POINT ( 'NONE',  ( 19.05374491087241751, 41.88689941110012427, -80.99294598599399819 ) ) ;
#66709 = UNCERTAINTY_MEASURE_WITH_UNIT (LENGTH_MEASURE( 1.000000000000000082E-05 ), #67286, 'distance_accuracy_value', 'NONE');
#66710 = DIRECTION ( 'NONE',  ( 0.000000000000000000, -1.000000000000000000, 0.000000000000000000 ) ) ;
#66711 = AXIS2_PLACEMENT_3D ( 'NONE', #55815, #14843, #80640 ) ;
#66712 = FACE_OUTER_BOUND ( 'NONE', #45909, .T. ) ;
#66713 = CARTESIAN_POINT ( 'NONE',  ( 81.06357478099751290, -29.99999999999999645, 22.11501143710179562 ) ) ;
#66714 = ADVANCED_FACE ( 'NONE', ( #38501, #30410 ), #41137, .T. ) ;
#66715 = CARTESIAN_POINT ( 'NONE',  ( 7.002641335706725201, 103.9491273731916294, 3.868676264653294172 ) ) ;
#66716 = ORIENTED_EDGE ( 'NONE', *, *, #88636, .T. ) ;
#66717 = ORIENTED_EDGE ( 'NONE', *, *, #41767, .T. ) ;
#66718 = ORIENTED_EDGE ( 'NONE', *, *, #43042, .F. ) ;
#66719 = CARTESIAN_POINT ( 'NONE',  ( -32.03720899075933204, 464.7921976803852999, 11.81820142136001728 ) ) ;
#66720 = CARTESIAN_POINT ( 'NONE',  ( -6.616218520611202081, 40.56071393578208273, -71.17595756557476250 ) ) ;
#66721 = DIRECTION ( 'NONE',  ( 1.000000000000000000, 1.224606353822377258E-16, 0.000000000000000000 ) ) ;
#66722 = CARTESIAN_POINT ( 'NONE',  ( -39.76451419608196858, 463.8702996273221402, 18.91610323218967693 ) ) ;
#66723 = CARTESIAN_POINT ( 'NONE',  ( -32.11440895090206027, 433.9874903900313257, 24.22985920295750617 ) ) ;
#66724 = LINE ( 'NONE', #18741, #27702 ) ;
#66725 = ORIENTED_EDGE ( 'NONE', *, *, #93426, .F. ) ;
#66726 = CARTESIAN_POINT ( 'NONE',  ( 42.60956082013381518, 435.9305394647374214, 18.66091589586977406 ) ) ;
#66727 = ORIENTED_EDGE ( 'NONE', *, *, #37586, .F. ) ;
#66728 = CARTESIAN_POINT ( 'NONE',  ( -16.14595037822608603, 7.274337365584598203, -6.616591826375523233 ) ) ;
#66729 = CARTESIAN_POINT ( 'NONE',  ( 72.82563136666954051, -38.32591977635656377, 151.2887102636987322 ) ) ;
#66730 = CARTESIAN_POINT ( 'NONE',  ( 0.000000000000000000, 0.000000000000000000, 4.000000000000000000 ) ) ;
#66731 = CARTESIAN_POINT ( 'NONE',  ( 31.19933698203508143, 299.4437075040892751, 10.96669800311853571 ) ) ;
#66732 = ADVANCED_FACE ( 'NONE', ( #30955 ), #28828, .T. ) ;
#66733 = LINE ( 'NONE', #99617, #85530 ) ;
#66734 = AXIS2_PLACEMENT_3D ( 'NONE', #86922, #21152, #20096 ) ;
#66735 = CARTESIAN_POINT ( 'NONE',  ( -28.09914318796796096, 34.19596624573215138, -9.569481124490501145 ) ) ;
#66736 = DIRECTION ( 'NONE',  ( 0.000000000000000000, 0.000000000000000000, -1.000000000000000000 ) ) ;
#66737 = DIRECTION ( 'NONE',  ( -1.000000000000000000, -1.224606353822377258E-16, -0.000000000000000000 ) ) ;
#66738 = CARTESIAN_POINT ( 'NONE',  ( -5.128020333435169498, 6.165036831253548399, 5.000000000000001776 ) ) ;
#66739 = ORIENTED_EDGE ( 'NONE', *, *, #81367, .T. ) ;
#66740 = CARTESIAN_POINT ( 'NONE',  ( -22.26224575421402463, 303.2621863394111870, 10.02517495966816874 ) ) ;
#66741 =( NAMED_UNIT ( * ) PLANE_ANGLE_UNIT ( ) SI_UNIT ( $, .RADIAN. ) );
#66742 = UNCERTAINTY_MEASURE_WITH_UNIT (LENGTH_MEASURE( 1.000000000000000082E-05 ), #64712, 'distance_accuracy_value', 'NONE');
#66743 = DIRECTION ( 'NONE',  ( -0.5735764363510512664, 0.8191520442889881348, 1.003171929053520309E-16 ) ) ;
#66744 = CARTESIAN_POINT ( 'NONE',  ( -6.484173630543650368, -4.916614646775412822, -7.642786413614080843 ) ) ;
#66745 = CIRCLE ( 'NONE', #15059, 6.499999999999999112 ) ;
#66747 = DIRECTION ( 'NONE',  ( 0.000000000000000000, -1.000000000000000000, 0.000000000000000000 ) ) ;
#66746 = AXIS2_PLACEMENT_3D ( 'NONE', #101012, #34727, #90811 ) ;
#66748 = SHAPE_REPRESENTATION ( '5. Joint', ( #10728 ), #47146 ) ;
#66749 = CARTESIAN_POINT ( 'NONE',  ( -7.344133061198929724, 102.5550560731942369, 3.176267128233874804 ) ) ;
#66750 = AXIS2_PLACEMENT_3D ( 'NONE', #30272, #98160, #55560 ) ;
#66751 = MECHANICAL_DESIGN_GEOMETRIC_PRESENTATION_REPRESENTATION (  '', ( #15071 ), #1272 ) ;
#66752 = CARTESIAN_POINT ( 'NONE',  ( 43.85205561063540358, 464.7392644987205585, 11.03676161964373570 ) ) ;
#66753 = MECHANICAL_DESIGN_GEOMETRIC_PRESENTATION_REPRESENTATION (  '', ( #25432 ), #39200 ) ;
#66754 = CARTESIAN_POINT ( 'NONE',  ( 85.28715672339788512, -42.92956674362846314, 186.5443997153789724 ) ) ;
#66755 = DIRECTION ( 'NONE',  ( 0.000000000000000000, -1.000000000000000000, 0.000000000000000000 ) ) ;
#66756 = DIRECTION ( 'NONE',  ( 0.5166563581656273829, 0.4014477553983911151, 0.7562446080816871419 ) ) ;
#66757 = ORIENTED_EDGE ( 'NONE', *, *, #25505, .T. ) ;
#66758 = CARTESIAN_POINT ( 'NONE',  ( 91.50964524610877504, -57.66228111830159975, -20.14352967758682311 ) ) ;
#66759 = DIRECTION ( 'NONE',  ( 0.000000000000000000, 0.000000000000000000, 1.000000000000000000 ) ) ;
#66760 = DIRECTION ( 'NONE',  ( 0.000000000000000000, -1.000000000000000000, 0.000000000000000000 ) ) ;
#66761 = AXIS2_PLACEMENT_3D ( 'NONE', #76495, #60870, #92687 ) ;
#66762 = CARTESIAN_POINT ( 'NONE',  ( -80.77720312678583525, -30.00000000000000000, 9.967219224732877692 ) ) ;
#66763 = B_SPLINE_CURVE_WITH_KNOTS ( 'NONE', 3,
 ( #63107, #103041, #12940, #28649 ),
 .UNSPECIFIED., .F., .F.,
 ( 4, 4 ),
 ( 3.898306166456212538E-17, 0.001587725418198030142 ),
 .UNSPECIFIED. ) ;
#66764 = VECTOR ( 'NONE', #27683, 1000.000000000000000 ) ;
#66765 = CARTESIAN_POINT ( 'NONE',  ( -30.00000000000000000, 500.0000000000002274, -12.00000000000000711 ) ) ;
#66766 = CARTESIAN_POINT ( 'NONE',  ( -7.125691916582566954, 41.67430808341742932, -69.26730091582949456 ) ) ;
#66767 = DIRECTION ( 'NONE',  ( -1.000000000000000000, -1.224606353822377258E-16, -0.000000000000000000 ) ) ;
#66768 = CARTESIAN_POINT ( 'NONE',  ( 18.09999999999999787, -3.309499999999999886, 4.475777889183790779E-16 ) ) ;
#66769 = ADVANCED_FACE ( 'NONE', ( #81555 ), #51222, .T. ) ;
#66770 = CARTESIAN_POINT ( 'NONE',  ( -28.94969860575643139, 18.87958371857672546, 39.84024749387425857 ) ) ;
#66771 = CARTESIAN_POINT ( 'NONE',  ( -35.17658899013244422, 491.5165241545290087, 12.37078523472847813 ) ) ;
#66772 = CARTESIAN_POINT ( 'NONE',  ( 5.476751506168961114, -81.83642877133006266, -2.461144630687910784 ) ) ;
#66773 = CARTESIAN_POINT ( 'NONE',  ( -51.00726465901860252, -36.03376012008488516, -27.78095564560482700 ) ) ;
#66774 = CARTESIAN_POINT ( 'NONE',  ( 41.47545032752432803, 461.4488756740975646, 2.700315731345424464 ) ) ;
#66775 = CARTESIAN_POINT ( 'NONE',  ( -98.14539993508641658, -37.99999999999994316, 192.4866759319958476 ) ) ;
#66776 = AXIS2_PLACEMENT_3D ( 'NONE', #21766, #5545, #72915 ) ;
#66777 = ORIENTED_EDGE ( 'NONE', *, *, #62328, .F. ) ;
#66778 = CARTESIAN_POINT ( 'NONE',  ( 5.763785242774020823, 12.46408377182749661, -3.972758706198394663 ) ) ;
#66779 = DIRECTION ( 'NONE',  ( 1.000000000000000000, 1.224606353822377258E-16, 0.000000000000000000 ) ) ;
#66780 = VECTOR ( 'NONE', #96462, 1000.000000000000000 ) ;
#66781 = CARTESIAN_POINT ( 'NONE',  ( -7.150931910075642328, 83.21374201477736676, -3.588457848165356623 ) ) ;
#66782 = EDGE_CURVE ( 'NONE', #35268, #64398, #7157, .T. ) ;
#66783 = CARTESIAN_POINT ( 'NONE',  ( -46.80132320916015232, -26.73529330813730454, -28.77368927080993188 ) ) ;
#66784 = EDGE_CURVE ( 'NONE', #28968, #29729, #74018, .T. ) ;
#66786 = CARTESIAN_POINT ( 'NONE',  ( 0.000000000000000000, 4.898587196589412829E-16, -4.000000000000000000 ) ) ;
#66785 = CARTESIAN_POINT ( 'NONE',  ( 7.500000000000006217, 152.0000000000000000, 0.000000000000000000 ) ) ;
#66787 = VERTEX_POINT ( 'NONE', #55693 ) ;
#66788 = CARTESIAN_POINT ( 'NONE',  ( 5.821900211247815093, 1.420906337218632798, -6.499999999999999112 ) ) ;
#66789 = EDGE_LOOP ( 'NONE', ( #37655, #14297 ) ) ;
#66790 = CARTESIAN_POINT ( 'NONE',  ( -26.16445804740967063, 35.04392636896330515, 7.979516327253138641 ) ) ;
#66791 = CIRCLE ( 'NONE', #18623, 3.400000000000000355 ) ;
#66792 = DIRECTION ( 'NONE',  ( -1.000000000000000000, 0.000000000000000000, 0.000000000000000000 ) ) ;
#66793 = CARTESIAN_POINT ( 'NONE',  ( 13.86650669486618881, 1.474610560812782335E-15, 0.000000000000000000 ) ) ;
#66794 = CARTESIAN_POINT ( 'NONE',  ( -83.65165148681774099, -60.00000000000000000, -25.56542375944041723 ) ) ;
#66795 = ORIENTED_EDGE ( 'NONE', *, *, #71487, .T. ) ;
#66796 = CARTESIAN_POINT ( 'NONE',  ( 89.06666666666666288, 4.172000000000019249, 0.000000000000000000 ) ) ;
#66797 = CARTESIAN_POINT ( 'NONE',  ( 55.26095113931063452, 6.856755485862130937E-15, 0.000000000000000000 ) ) ;
#66798 = CARTESIAN_POINT ( 'NONE',  ( 99.50318429255658259, -37.82977025964015638, 191.3434515804738112 ) ) ;
#66800 = DIRECTION ( 'NONE',  ( -1.000000000000000000, -1.224606353822377258E-16, -0.000000000000000000 ) ) ;
#66799 = CARTESIAN_POINT ( 'NONE',  ( 5.391112028019903413, 294.7725620969052329, -8.441341902468499470 ) ) ;
#66801 = ORIENTED_EDGE ( 'NONE', *, *, #18259, .F. ) ;
#66802 = ORIENTED_EDGE ( 'NONE', *, *, #58467, .F. ) ;
#66803 = ORIENTED_EDGE ( 'NONE', *, *, #5543, .T. ) ;
#66804 = CARTESIAN_POINT ( 'NONE',  ( 31.27225709781784957, 363.0917169579986989, 21.44302781083598930 ) ) ;
#66805 = CARTESIAN_POINT ( 'NONE',  ( -5.656854249492381470, -28.06249999999999645, 5.656854249492379694 ) ) ;
#66806 = LINE ( 'NONE', #50078, #62189 ) ;
#66807 = ORIENTED_EDGE ( 'NONE', *, *, #40082, .T. ) ;
#66808 = CARTESIAN_POINT ( 'NONE',  ( 16.02196273765584067, 46.08952128005080340, -4.311160109051586531 ) ) ;
#66809 = DIRECTION ( 'NONE',  ( -1.000000000000000000, -1.224606353822377258E-16, -0.000000000000000000 ) ) ;
#66810 = CARTESIAN_POINT ( 'NONE',  ( 0.3167204509598209872, -5.377136764700215288, -6.686525924292707757 ) ) ;
#66811 = CARTESIAN_POINT ( 'NONE',  ( -37.03244656124025624, -57.69633701093174949, 51.43040253561569131 ) ) ;
#66812 = CARTESIAN_POINT ( 'NONE',  ( -5.082755093536325042, -29.09375000204838813, -5.082755093536325930 ) ) ;
#66813 = DIRECTION ( 'NONE',  ( 0.000000000000000000, -1.000000000000000000, 0.000000000000000000 ) ) ;
#66814 = CARTESIAN_POINT ( 'NONE',  ( -21.25502769577498796, 305.0480251235313176, 9.978840188629131802 ) ) ;
#66815 = COLOUR_RGB ( '', 0.09019608, 0.27058824, 0.51372549) ;
#66816 = CARTESIAN_POINT ( 'NONE',  ( -6.706751634816551011, 41.66489468247179673, -58.91094301962639435 ) ) ;
#66817 = CARTESIAN_POINT ( 'NONE',  ( -89.66619014120909981, -60.00000000000001421, -23.31631894612182521 ) ) ;
#66818 = DIRECTION ( 'NONE',  ( -1.000000000000000000, -0.000000000000000000, -0.000000000000000000 ) ) ;
#66819 = EDGE_CURVE ( 'NONE', #11120, #46974, #31998, .T. ) ;
#66820 = CARTESIAN_POINT ( 'NONE',  ( -49.35531877875648377, -53.36885908633350795, 54.26204743392272434 ) ) ;
#66821 = DIRECTION ( 'NONE',  ( 0.000000000000000000, 0.000000000000000000, -1.000000000000000000 ) ) ;
#66822 = VERTEX_POINT ( 'NONE', #15790 ) ;
#66823 = PRESENTATION_LAYER_ASSIGNMENT (  '', '', ( #6518 ) ) ;
#66824 = DIRECTION ( 'NONE',  ( -1.000000000000000000, -0.000000000000000000, -0.000000000000000000 ) ) ;
#66825 = AXIS2_PLACEMENT_3D ( 'NONE', #10454, #83288, #43371 ) ;
#66826 = CARTESIAN_POINT ( 'NONE',  ( -8.823089264727318692, 295.7038567688371131, -10.03557449692967118 ) ) ;
#66827 = DIRECTION ( 'NONE',  ( -0.000000000000000000, -1.000000000000000000, -0.000000000000000000 ) ) ;
#66828 = ORIENTED_EDGE ( 'NONE', *, *, #67309, .F. ) ;
#66829 = CARTESIAN_POINT ( 'NONE',  ( 4.656390720430122698, 248.6835381403945178, 3.786082374785835203 ) ) ;
#66830 = CARTESIAN_POINT ( 'NONE',  ( 103.8938049727245669, -38.41582098933665890, 198.4886963997253133 ) ) ;
#66831 = DIRECTION ( 'NONE',  ( 0.000000000000000000, 1.000000000000000000, 0.000000000000000000 ) ) ;
#66832 = DIRECTION ( 'NONE',  ( 0.000000000000000000, 0.000000000000000000, -1.000000000000000000 ) ) ;
#66833 = CARTESIAN_POINT ( 'NONE',  ( 44.61777206441712451, 434.3429578869022976, 14.57557122161292362 ) ) ;
#66834 = CARTESIAN_POINT ( 'NONE',  ( 11.85444436799972934, 42.00000000000000000, 90.56128410203886858 ) ) ;
#66835 = CARTESIAN_POINT ( 'NONE',  ( 89.52544717665139729, -30.00000000000000355, 189.4090387211008419 ) ) ;
#66836 = CARTESIAN_POINT ( 'NONE',  ( 35.67925427713999653, 491.2490127027394351, 12.19183392504568531 ) ) ;
#66837 = ADVANCED_FACE ( 'NONE', ( #96721 ), #79987, .T. ) ;
#66838 = PRESENTATION_STYLE_ASSIGNMENT (( #33966 ) ) ;
#66839 = CARTESIAN_POINT ( 'NONE',  ( -3.840629472727446691E-14, -1.200000000000000030E-05, -27.25000000000000000 ) ) ;
#66840 = AXIS2_PLACEMENT_3D ( 'NONE', #41960, #91593, #43037 ) ;
#66841 = ORIENTED_EDGE ( 'NONE', *, *, #41943, .T. ) ;
#66842 = ORIENTED_EDGE ( 'NONE', *, *, #50187, .T. ) ;
#66843 = CARTESIAN_POINT ( 'NONE',  ( 52.52745653095553280, -49.90442938472995138, 59.15515806098346729 ) ) ;
#66844 = CARTESIAN_POINT ( 'NONE',  ( -33.72905809600837301, 464.0430918388251484, 18.49991514059377806 ) ) ;
#66845 = CARTESIAN_POINT ( 'NONE',  ( 9.999999999999998224, 0.000000000000000000, -9.999999999999998224 ) ) ;
#66846 = EDGE_LOOP ( 'NONE', ( #45326, #44858, #46870, #77664, #15095 ) ) ;
#66847 = CARTESIAN_POINT ( 'NONE',  ( -92.36008094370296817, -38.35495905226510160, 38.05242013568155812 ) ) ;
#66848 = AXIS2_PLACEMENT_3D ( 'NONE', #17368, #50240, #73975 ) ;
#66849 = ORIENTED_EDGE ( 'NONE', *, *, #47662, .F. ) ;
#66850 = CARTESIAN_POINT ( 'NONE',  ( 59.89460441624491693, -1.232595164407830946E-29, 4.000000000000007105 ) ) ;
#66851 = CARTESIAN_POINT ( 'NONE',  ( 109.9456817262660877, -38.35603827305180147, 154.1022712922482185 ) ) ;
#66852 = CARTESIAN_POINT ( 'NONE',  ( 14.20884251306467760, 21.14818849446572813, -5.803600968828524387 ) ) ;
#66853 = CARTESIAN_POINT ( 'NONE',  ( 89.51473135658183367, -45.28271082105466405, 67.81559373879049701 ) ) ;
#66854 = CARTESIAN_POINT ( 'NONE',  ( -16.80224347588841383, 43.42191715542256958, -6.657797401562048023 ) ) ;
#66855 = LINE ( 'NONE', #60377, #60257 ) ;
#66856 = CARTESIAN_POINT ( 'NONE',  ( -32.35276657115729648, 315.1152556236738178, -7.307750464049918904 ) ) ;
#66857 = CARTESIAN_POINT ( 'NONE',  ( 102.0666666666666629, 1.023464760207051730E-14, 0.000000000000000000 ) ) ;
#66858 = AXIS2_PLACEMENT_3D ( 'NONE', #106092, #57539, #57015 ) ;
#66859 = CARTESIAN_POINT ( 'NONE',  ( 75.45442456345966775, -60.00000000000002132, 184.2217590398179823 ) ) ;
#66860 = EDGE_CURVE ( 'NONE', #88074, #20995, #35740, .T. ) ;
#66861 = CARTESIAN_POINT ( 'NONE',  ( 41.08349330513380693, 4.000000000000003553, 0.000000000000000000 ) ) ;
#66862 = FACE_OUTER_BOUND ( 'NONE', #45646, .T. ) ;
#66863 = ORIENTED_EDGE ( 'NONE', *, *, #93290, .T. ) ;
#66864 = CARTESIAN_POINT ( 'NONE',  ( 61.37175430821151423, -60.33933855911503485, 86.28502804520786640 ) ) ;
#66865 = EDGE_CURVE ( 'NONE', #84992, #31964, #47613, .T. ) ;
#66866 = CARTESIAN_POINT ( 'NONE',  ( -25.80611886614622819, 295.7843487485618539, -9.799740642693116399 ) ) ;
#66867 = DIRECTION ( 'NONE',  ( 0.000000000000000000, -1.000000000000000000, 0.000000000000000000 ) ) ;
#66868 = DIRECTION ( 'NONE',  ( 1.000000000000000000, 0.000000000000000000, 0.000000000000000000 ) ) ;
#66869 = CARTESIAN_POINT ( 'NONE',  ( -4.036353419639556961, 54.13891293591672849, 7.153575984207336091 ) ) ;
#66870 = AXIS2_PLACEMENT_3D ( 'NONE', #25690, #59082, #33758 ) ;
#66871 = CARTESIAN_POINT ( 'NONE',  ( -33.06021938597559995, 369.5034847643744342, 23.69045737582667854 ) ) ;
#66872 = CARTESIAN_POINT ( 'NONE',  ( -38.64289892958222339, 25.32045246094368807, -11.54945401700677188 ) ) ;
#66873 = FILL_AREA_STYLE ('',( #74937 ) ) ;
#66874 = CARTESIAN_POINT ( 'NONE',  ( -5.656854249492379694, -25.43749999999999645, -5.656854249492380582 ) ) ;
#66875 = LINE ( 'NONE', #32932, #105347 ) ;
#66876 = CIRCLE ( 'NONE', #1395, 8.000000000000000000 ) ;
#66877 = CARTESIAN_POINT ( 'NONE',  ( 15.89150943383949333, 43.76196850971604846, -6.419014916071676957 ) ) ;
#66878 = AXIS2_PLACEMENT_3D ( 'NONE', #28110, #11331, #62574 ) ;
#66879 = VERTEX_POINT ( 'NONE', #104806 ) ;
#66880 = CARTESIAN_POINT ( 'NONE',  ( 86.13882259233811567, -18.34482622158760989, 167.7275104523019991 ) ) ;
#66881 = CARTESIAN_POINT ( 'NONE',  ( 43.51067860848610991, 485.4417974898067314, 3.909400899861634304 ) ) ;
#66882 = EDGE_CURVE ( 'NONE', #21082, #57829, #855, .T. ) ;
#66883 = AXIS2_PLACEMENT_3D ( 'NONE', #50166, #60417, #75500 ) ;
#66884 = DIRECTION ( 'NONE',  ( -1.000000000000000000, -1.224606353822377258E-16, -0.000000000000000000 ) ) ;
#66885 = ORIENTED_EDGE ( 'NONE', *, *, #62637, .F. ) ;
#66886 = DIRECTION ( 'NONE',  ( -1.000000000000000000, -0.000000000000000000, -0.000000000000000000 ) ) ;
#66887 = EDGE_CURVE ( 'NONE', #27782, #21120, #63971, .T. ) ;
#66888 = CARTESIAN_POINT ( 'NONE',  ( 0.000000000000000000, 303.8518027762758038, 9.936999415352289589 ) ) ;
#66889 = CARTESIAN_POINT ( 'NONE',  ( -13.57428064878229890, -23.62732209985536969, -38.53619311655949531 ) ) ;
#66890 = CARTESIAN_POINT ( 'NONE',  ( -6.148597574911479846, -3.030260368802259463E-15, 18.77664127325637011 ) ) ;
#66891 =( BOUNDED_SURFACE ( )  B_SPLINE_SURFACE ( 3, 2, ( 
 ( #78274, #77756, #69147 ),
 ( #102014, #28175, #4390 ),
 ( #77220, #79334, #3868 ),
 ( #12993, #37329, #5455 ) ),
 .UNSPECIFIED., .F., .F., .F. ) 
 B_SPLINE_SURFACE_WITH_KNOTS ( ( 4, 4 ),
 ( 3, 3 ),
 ( -1.214306433183764966E-17, 0.003677210556161270016 ),
 ( 0.000000000000000000, 1.000000000000000000 ),
 .UNSPECIFIED. ) 
 GEOMETRIC_REPRESENTATION_ITEM ( )  RATIONAL_B_SPLINE_SURFACE ( (
 ( 1.000000000000000000, 0.7874655377940259493, 1.000000000000000000),
 ( 1.000000000000000000, 0.7709584336437038665, 1.000000000000000000),
 ( 1.000000000000000000, 0.7542748649868507016, 1.000000000000000000),
 ( 1.000000000000000000, 0.7370557512816398038, 1.000000000000000000) ) ) 
 REPRESENTATION_ITEM ( '' )  SURFACE ( )  );
#66892 = B_SPLINE_CURVE_WITH_KNOTS ( 'NONE', 3,
 ( #54331, #105562, #105046, #7387, #47843, #31187, #64072, #96947 ),
 .UNSPECIFIED., .F., .F.,
 ( 4, 2, 2, 4 ),
 ( 0.000000000000000000, 0.002052176099994375801, 0.003078264149991564568, 0.004104352199988753336 ),
 .UNSPECIFIED. ) ;
#66893 = CARTESIAN_POINT ( 'NONE',  ( 49.28483115600248965, -60.00000000000000000, 70.03155139212616120 ) ) ;
#66894 = STYLED_ITEM ( 'NONE', ( #88179 ), #60953 ) ;
#66895 = VECTOR ( 'NONE', #33787, 1000.000000000000000 ) ;
#66896 = CARTESIAN_POINT ( 'NONE',  ( 6.928203230275507885, 105.0000000000000000, -4.000000000000001776 ) ) ;
#66897 = CARTESIAN_POINT ( 'NONE',  ( 19.21337042771324377, -16.78003050461148504, 31.49141766188020242 ) ) ;
#66898 = VECTOR ( 'NONE', #48533, 1000.000000000000000 ) ;
#66900 = CARTESIAN_POINT ( 'NONE',  ( -13.55991250221987166, 24.71331123137162677, 1.199625589988368768 ) ) ;
#66899 = CARTESIAN_POINT ( 'NONE',  ( -7.580914931690657887, -19.30281391077188147, 35.20923601663831448 ) ) ;
#66901 = CARTESIAN_POINT ( 'NONE',  ( -9.989435848181784650, 88.97380292528423240, -0.5278651953175997891 ) ) ;
#66902 = CARTESIAN_POINT ( 'NONE',  ( 2.977408999572651815, -14.93750000204838457, 7.188101187500000933 ) ) ;
#66903 = CYLINDRICAL_SURFACE ( 'NONE', #85427, 15.00000000000001421 ) ;
#66904 = CIRCLE ( 'NONE', #70370, 5.000000000000010658 ) ;
#66905 = CARTESIAN_POINT ( 'NONE',  ( 26.08349330513380337, 4.000000000000002665, 0.000000000000000000 ) ) ;
#66906 = ORIENTED_EDGE ( 'NONE', *, *, #82986, .T. ) ;
#66907 = CARTESIAN_POINT ( 'NONE',  ( -18.97029851426740521, 49.42830426956749790, 61.97293826772175152 ) ) ;
#66908 = CARTESIAN_POINT ( 'NONE',  ( 103.5111111111111057, -4.171999999999998820, 5.616230220889773285E-16 ) ) ;
#66909 = DIRECTION ( 'NONE',  ( -0.5735764363510510444, -0.8191520442889883569, 0.000000000000000000 ) ) ;
#66910 = EDGE_CURVE ( 'NONE', #47934, #2138, #48144, .T. ) ;
#66912 = CARTESIAN_POINT ( 'NONE',  ( 16.18283418694998588, -60.22807642560611896, -36.38454838023258731 ) ) ;
#66911 = DIRECTION ( 'NONE',  ( -1.000000000000000000, -1.224606353822377258E-16, -0.000000000000000000 ) ) ;
#66913 = B_SPLINE_CURVE_WITH_KNOTS ( 'NONE', 3,
 ( #88471, #80348, #6461, #33430, #23756, #106208, #15621, #25903, #58209, #461, #91134, #66303, #73312, #32371, #99184, #90583, #32902, #65777 ),
 .UNSPECIFIED., .F., .F.,
 ( 4, 2, 2, 2, 2, 2, 2, 2, 4 ),
 ( -1.788854398705523621E-05, 0.003356281543241195105, 0.005043366586855251542, 0.006730451630469307112, 0.007573994152276390841, 0.008417536674083472836, 0.01010462171769764377, 0.01179170676131181296, 0.01347879180492598215 ),
 .UNSPECIFIED. ) ;
#66914 = ORIENTED_EDGE ( 'NONE', *, *, #17517, .T. ) ;
#66915 = AXIS2_PLACEMENT_3D ( 'NONE', #42098, #8669, #58285 ) ;
#66916 = CARTESIAN_POINT ( 'NONE',  ( 0.000000000000000000, 0.000000000000000000, 0.000000000000000000 ) ) ;
#66917 = CARTESIAN_POINT ( 'NONE',  ( -4.524258892669210219, 51.56515624534051057, 8.282099392949428207 ) ) ;
#66918 = EDGE_LOOP ( 'NONE', ( #92192, #49940, #74537, #45343, #45790, #91363 ) ) ;
#66919 = ADVANCED_FACE ( 'NONE', ( #105336 ), #32252, .T. ) ;
#66920 = FACE_OUTER_BOUND ( 'NONE', #23304, .T. ) ;
#66921 = VECTOR ( 'NONE', #32892, 1000.000000000000000 ) ;
#66922 = CARTESIAN_POINT ( 'NONE',  ( 30.25640691047251707, 12.05011699928722102, -39.73625916528182245 ) ) ;
#66923 = CIRCLE ( 'NONE', #103039, 5.000000000000002665 ) ;
#66924 = CARTESIAN_POINT ( 'NONE',  ( -33.14954961147306278, 40.69031475660899133, -62.06908864790394631 ) ) ;
#66925 = CARTESIAN_POINT ( 'NONE',  ( -101.5459148796837212, -60.00000000000000000, 90.09389878889895442 ) ) ;
#66926 = CARTESIAN_POINT ( 'NONE',  ( -11.80096911583921404, 304.5943216053429410, -9.054726665033207667 ) ) ;
#66927 = CARTESIAN_POINT ( 'NONE',  ( 30.24427031855517711, 312.0196691915732004, -8.325478004009855937 ) ) ;
#66928 = CARTESIAN_POINT ( 'NONE',  ( 41.02721008360133226, 460.5398098099298636, 2.518281297459247448 ) ) ;
#66930 = CARTESIAN_POINT ( 'NONE',  ( -15.05785784214257461, 3.824195276785042896, 4.604276673521232155 ) ) ;
#66929 = CARTESIAN_POINT ( 'NONE',  ( -9.999999999999996447, -3.000000000000002665, -86.30899693747677759 ) ) ;
#66931 = CARTESIAN_POINT ( 'NONE',  ( -81.78828991020175465, -53.49607135933386814, 179.9890600379855243 ) ) ;
#66932 = ORIENTED_EDGE ( 'NONE', *, *, #4912, .T. ) ;
#66933 = LINE ( 'NONE', #34594, #105630 ) ;
#66934 = EDGE_LOOP ( 'NONE', ( #94744, #37198, #20800, #17503, #6520, #61730 ) ) ;
#66935 = ORIENTED_EDGE ( 'NONE', *, *, #88247, .F. ) ;
#66936 = FACE_OUTER_BOUND ( 'NONE', #69755, .T. ) ;
#66937 = ADVANCED_FACE ( 'NONE', ( #622 ), #34672, .F. ) ;
#66938 = CARTESIAN_POINT ( 'NONE',  ( 41.50669491856072568, 1.482358050883964840E-15, 0.000000000000000000 ) ) ;
#66939 = ORIENTED_EDGE ( 'NONE', *, *, #2625, .T. ) ;
#66940 = DIRECTION ( 'NONE',  ( 0.000000000000000000, -1.000000000000000000, 0.000000000000000000 ) ) ;
#66941 = DIRECTION ( 'NONE',  ( 0.000000000000000000, -0.000000000000000000, 1.000000000000000000 ) ) ;
#66942 = CARTESIAN_POINT ( 'NONE',  ( -6.815830331203685866, -0.6619522098568515478, -6.171384342982615401 ) ) ;
#66943 = AXIS2_PLACEMENT_3D ( 'NONE', #49384, #31652, #82293 ) ;
#66944 = CARTESIAN_POINT ( 'NONE',  ( -6.944371705245971249, -64.46100308575449844, -3.972324460300566962 ) ) ;
#66945 = CARTESIAN_POINT ( 'NONE',  ( 43.72105821076075927, 464.5236242685676871, 7.250473608341952314 ) ) ;
#66946 = CARTESIAN_POINT ( 'NONE',  ( -13.38090213880806800, -53.73814761577546051, 31.11721482942555994 ) ) ;
#66947 = CARTESIAN_POINT ( 'NONE',  ( -16.91657744243853045, 36.34978592707986422, -24.30698433968596461 ) ) ;
#66948 = CARTESIAN_POINT ( 'NONE',  ( 89.52590460267296635, -30.00000000000006395, 22.04891038916446888 ) ) ;
#66949 = CARTESIAN_POINT ( 'NONE',  ( -106.5495191435086468, -14.21045842199437992, 161.7519935124221604 ) ) ;
#66950 = ADVANCED_FACE ( 'NONE', ( #76677 ), #55825, .T. ) ;
#66951 = CARTESIAN_POINT ( 'NONE',  ( -58.77187156240383814, -29.07515625515527447, 64.41617457802827573 ) ) ;
#66952 = EDGE_LOOP ( 'NONE', ( #78968, #104495, #69066, #17905 ) ) ;
#66953 = CARTESIAN_POINT ( 'NONE',  ( 72.11682663846713126, 4.898587196589294500E-16, -4.000000000000007105 ) ) ;
#66954 = CARTESIAN_POINT ( 'NONE',  ( 112.7988352096499369, -60.00000000000001421, 189.9832682156421129 ) ) ;
#66955 = ORIENTED_EDGE ( 'NONE', *, *, #65903, .F. ) ;
#66956 = CARTESIAN_POINT ( 'NONE',  ( 4.060351201658883191, -42.95350087791473470, 31.04114541283799156 ) ) ;
#66957 = CARTESIAN_POINT ( 'NONE',  ( -104.6405814182722480, -60.15514485569779879, 146.7656546127498984 ) ) ;
#66958 = CARTESIAN_POINT ( 'NONE',  ( -7.188101187500000933, -12.87500000204838813, -2.977408999572651371 ) ) ;
#66959 = FILL_AREA_STYLE_COLOUR ( '', #95963 ) ;
#66961 = DIRECTION ( 'NONE',  ( 0.000000000000000000, 0.000000000000000000, -1.000000000000000000 ) ) ;
#66960 = CIRCLE ( 'NONE', #92740, 4.000000000000001776 ) ;
#66962 = ORIENTED_EDGE ( 'NONE', *, *, #9820, .F. ) ;
#66964 = B_SPLINE_CURVE_WITH_KNOTS ( 'NONE', 3,
 ( #30318, #39467, #63745, #22235, #46485, #89068, #31396, #46999, #48053, #105767, #95057, #13032, #45959, #78841, #21708, #4969, #37899, #70759, #54545, #5496, #99253, #57733, #82563, #25974, #106282, #65846, #73385, #32448, #66924, #91729, #90124, #66373, #8667, #73926, #8132, #58834, #7, #25425, #32976, #42630, #58283, #74981, #1072, #41570, #57205, #23834, #48584, #99804, #65320, #91209, #56678, #17316, #74456, #49655, #90657, #50191, #31908, #98725, #24361, #7589, #34047, #83093, #536, #17847, #33496, #50697, #9186, #83612, #9716, #42095 ),
 .UNSPECIFIED., .F., .F.,
 ( 4, 2, 2, 2, 1, 1, 1, 1, 1, 2, 2, 2, 2, 2, 2, 1, 1, 1, 1, 1, 2, 2, 2, 2, 2, 2, 1, 1, 1, 1, 1, 1, 2, 2, 2, 2, 2, 2, 1, 1, 1, 1, 2, 2, 4 ),
 ( 0.000000000000000000, 0.1250000000002316758, 0.1875000000003474998, 0.2187500000004056477, 0.2343750000004347356, 0.2421875000004492517, 0.2460937500004567458, 0.2480468750004604095, 0.2490234375004621026, 0.2495117187504630463, 0.2500000000004640177, 0.3750000000006326606, 0.4375000000007171486, 0.4687500000007595036, 0.4843750000007807088, 0.4921875000007913670, 0.4960937500007965850, 0.4980468750007990830, 0.4990234375008003043, 0.4995117187508010814, 0.4997558593758013035, 0.5000000000008014700, 0.6250000000008512080, 0.6875000000008759660, 0.7187500000008880674, 0.7343750000008941736, 0.7421875000008971712, 0.7460937500008987255, 0.7480468750008993917, 0.7490234375008996137, 0.7495117187508999468, 0.7497558593759003909, 0.7498779296884003909, 0.7500000000009003909, 0.8125000000007255307, 0.8437500000006383782, 0.8593750000005944134, 0.8671875000005724310, 0.8710937500005613288, 0.8730468750005559997, 0.8740234375005532241, 0.8745117187505518919, 0.8747558593755512257, 0.8750000000005505596, 1.000000000000000000 ),
 .UNSPECIFIED. ) ;
#66963 = CARTESIAN_POINT ( 'NONE',  ( 37.33349330513379982, -3.851859888774471706E-31, 4.000000000000001776 ) ) ;
#66965 = CARTESIAN_POINT ( 'NONE',  ( -72.42031090680902139, -60.00000000000001421, 157.4287250850663895 ) ) ;
#66966 = CARTESIAN_POINT ( 'NONE',  ( 36.57304083009643136, 26.05215988785383630, -11.44320818231313730 ) ) ;
#66967 = CARTESIAN_POINT ( 'NONE',  ( 7.188101187500000044, -18.03125000204838457, 0.000000000000000000 ) ) ;
#66968 = CARTESIAN_POINT ( 'NONE',  ( 0.000000000000000000, 23.58303312036771615, 0.000000000000000000 ) ) ;
#66969 = CARTESIAN_POINT ( 'NONE',  ( -1.060159942579158798, 21.71876410358088805, -6.924198097909567196 ) ) ;
#66970 = LINE ( 'NONE', #56174, #30586 ) ;
#66971 = DIRECTION ( 'NONE',  ( 0.5735764363510442720, -0.8191520442889930198, 1.003171929053526349E-16 ) ) ;
#66972 = CARTESIAN_POINT ( 'NONE',  ( 7.576662914407418015, -12.42162669466707570, 8.412646887033078613 ) ) ;
#66973 = ADVANCED_FACE ( 'NONE', ( #17404 ), #101138, .T. ) ;
#66974 = CARTESIAN_POINT ( 'NONE',  ( -24.32770621568460001, 27.33676458719045144, 32.55389746325912625 ) ) ;
#66975 = CARTESIAN_POINT ( 'NONE',  ( 86.14605752652843762, -59.99999999999999289, 15.79010570469148789 ) ) ;
#66976 = CARTESIAN_POINT ( 'NONE',  ( -32.30820442022806560, -46.43510695185953807, 35.30439282640345056 ) ) ;
#66977 = FILL_AREA_STYLE ('',( #26030 ) ) ;
#66978 = CARTESIAN_POINT ( 'NONE',  ( 41.39420356405966572, -18.78398962539201733, 34.98631649356083528 ) ) ;
#66979 = FACE_OUTER_BOUND ( 'NONE', #70404, .T. ) ;
#66980 = ORIENTED_EDGE ( 'NONE', *, *, #29370, .F. ) ;
#66981 = VECTOR ( 'NONE', #17135, 1000.000000000000000 ) ;
#66982 = CARTESIAN_POINT ( 'NONE',  ( 44.28914958154554427, 435.2230000814673758, 14.00302124382064761 ) ) ;
#66983 = CARTESIAN_POINT ( 'NONE',  ( -76.90211361482964492, -38.44896177797908621, 183.8811321853390552 ) ) ;
#66984 = ORIENTED_EDGE ( 'NONE', *, *, #68784, .T. ) ;
#66986 =( NAMED_UNIT ( * ) SI_UNIT ( $, .STERADIAN. ) SOLID_ANGLE_UNIT ( ) );
#66985 = DIRECTION ( 'NONE',  ( 0.000000000000000000, -1.000000000000000000, 0.000000000000000000 ) ) ;
#66987 = CARTESIAN_POINT ( 'NONE',  ( 77.37879385987021408, -60.00000000000004263, 150.9693798004460348 ) ) ;
#66988 = CARTESIAN_POINT ( 'NONE',  ( -48.28061695858873748, 9.217865022612228287, -16.83796839065926676 ) ) ;
#66989 = CARTESIAN_POINT ( 'NONE',  ( 42.50679667589145794, 460.9583926513302004, 2.954705527089782624 ) ) ;
#66990 = VECTOR ( 'NONE', #42062, 1000.000000000000000 ) ;
#66991 = CARTESIAN_POINT ( 'NONE',  ( -3.594029361870008099, -9.531975552773349847, 6.225090491531444670 ) ) ;
#66992 = LINE ( 'NONE', #60509, #18914 ) ;
#66993 = CARTESIAN_POINT ( 'NONE',  ( 5.000000000000000000, -46.02075056256854424, 5.909823871114814331 ) ) ;
#66994 = CARTESIAN_POINT ( 'NONE',  ( 16.80328583523077768, 45.82802980027266671, 4.157797401561413864 ) ) ;
#66995 = CARTESIAN_POINT ( 'NONE',  ( 105.7023782531532134, -60.00000000000000000, 114.6129108351607044 ) ) ;
#66996 = DIRECTION ( 'NONE',  ( 1.000000000000000000, 1.224606353822377258E-16, 0.000000000000000000 ) ) ;
#66997 = DIRECTION ( 'NONE',  ( -1.000000000000000000, -1.224606353822377258E-16, -0.000000000000000000 ) ) ;
#66998 = ORIENTED_EDGE ( 'NONE', *, *, #40335, .F. ) ;
#66999 = ADVANCED_FACE ( 'NONE', ( #67544 ), #84249, .T. ) ;
#67000 =( GEOMETRIC_REPRESENTATION_CONTEXT ( 3 ) GLOBAL_UNCERTAINTY_ASSIGNED_CONTEXT ( ( #80788 ) ) GLOBAL_UNIT_ASSIGNED_CONTEXT ( ( #50578, #67854, #84581 ) ) REPRESENTATION_CONTEXT ( 'NONE', 'WORKASPACE' ) );
#67001 = CARTESIAN_POINT ( 'NONE',  ( -85.72047231801046507, -29.99999999999986855, 176.6773169481917591 ) ) ;
#67002 = ORIENTED_EDGE ( 'NONE', *, *, #91993, .T. ) ;
#67003 = DIRECTION ( 'NONE',  ( 0.8191520442889884679, 0.000000000000000000, 0.5735764363510509334 ) ) ;
#67004 = CARTESIAN_POINT ( 'NONE',  ( 30.47402504887697106, 326.6747004222083888, 15.54443406114438453 ) ) ;
#67005 = FILL_AREA_STYLE_COLOUR ( '', #26577 ) ;
#67006 = VECTOR ( 'NONE', #80270, 1000.000000000000000 ) ;
#67007 = CARTESIAN_POINT ( 'NONE',  ( -1.320432766682874540E-15, -19.90625000204838457, 7.188101187500000044 ) ) ;
#67008 = EDGE_CURVE ( 'NONE', #97780, #62139, #56377, .T. ) ;
#67009 = ADVANCED_FACE ( 'NONE', ( #46446 ), #104589, .T. ) ;
#67010 = CIRCLE ( 'NONE', #84164, 4.000000000000001776 ) ;
#67011 = FACE_OUTER_BOUND ( 'NONE', #74262, .T. ) ;
#67012 = COLOUR_RGB ( '', 0.40784314, 0.44705882, 0.49803922) ;
#67013 = EDGE_LOOP ( 'NONE', ( #73572, #76066, #105094, #77827 ) ) ;
#67014 = CARTESIAN_POINT ( 'NONE',  ( 84.47855945016070223, -18.66665705232763983, 151.2491824433281522 ) ) ;
#67015 = CARTESIAN_POINT ( 'NONE',  ( -62.01418705506001317, 38.95383793061829891, 16.66584972140498166 ) ) ;
#67016 = VECTOR ( 'NONE', #50767, 1000.000000000000000 ) ;
#67017 = VERTEX_POINT ( 'NONE', #28706 ) ;
#67018 = EDGE_CURVE ( 'NONE', #4022, #59703, #61049, .T. ) ;
#67019 = DIRECTION ( 'NONE',  ( 0.000000000000000000, 1.000000000000000000, 0.000000000000000000 ) ) ;
#67020 = CARTESIAN_POINT ( 'NONE',  ( -7.188101187500000044, -9.406250002048384573, -8.802885111219163269E-16 ) ) ;
#67021 = DIRECTION ( 'NONE',  ( 0.000000000000000000, -1.000000000000000000, 0.000000000000000000 ) ) ;
#67022 = DIRECTION ( 'NONE',  ( 0.000000000000000000, 0.000000000000000000, -1.000000000000000000 ) ) ;
#67023 = CARTESIAN_POINT ( 'NONE',  ( -24.97496876848101977, 304.5750556681570629, 10.31800315847969429 ) ) ;
#67024 = SURFACE_STYLE_USAGE ( .BOTH. , #49220 ) ;
#67025 = ORIENTED_EDGE ( 'NONE', *, *, #27425, .F. ) ;
#67026 =( GEOMETRIC_REPRESENTATION_CONTEXT ( 3 ) GLOBAL_UNCERTAINTY_ASSIGNED_CONTEXT ( ( #11090 ) ) GLOBAL_UNIT_ASSIGNED_CONTEXT ( ( #10002, #11049, #1356 ) ) REPRESENTATION_CONTEXT ( 'NONE', 'WORKASPACE' ) );
#67027 = CARTESIAN_POINT ( 'NONE',  ( 4.000000000000000000, 17.85270131633358304, -5.744562646538043715 ) ) ;
#67028 = CIRCLE ( 'NONE', #48049, 65.00000000000000000 ) ;
#67029 = CARTESIAN_POINT ( 'NONE',  ( -5.000000000000000000, -66.75623614760699809, 15.74601422014960583 ) ) ;
#67030 = CARTESIAN_POINT ( 'NONE',  ( 14.87694226783599838, 23.07857475180312434, -1.005178106818441996 ) ) ;
#67031 = DIRECTION ( 'NONE',  ( 0.000000000000000000, 0.000000000000000000, 1.000000000000000000 ) ) ;
#67032 = CARTESIAN_POINT ( 'NONE',  ( -7.188101187500002709, -33.31250000204838813, 2.977408999572648707 ) ) ;
#67033 = DIRECTION ( 'NONE',  ( -0.000000000000000000, 1.000000000000000000, -0.000000000000000000 ) ) ;
#67034 = CARTESIAN_POINT ( 'NONE',  ( -4.466912950640278268E-14, -7.505553499465147382, -0.7999999999999977129 ) ) ;
#67035 = VECTOR ( 'NONE', #44902, 999.9999999999998863 ) ;
#67036 = PRESENTATION_STYLE_ASSIGNMENT (( #19591 ) ) ;
#67037 = CONTEXT_DEPENDENT_SHAPE_REPRESENTATION ( #52149, #103512 ) ;
#67039 = ORIENTED_EDGE ( 'NONE', *, *, #23124, .F. ) ;
#67038 = B_SPLINE_CURVE_WITH_KNOTS ( 'NONE', 3,
 ( #52133, #75340, #26325, #85051, #102289, #42451 ),
 .UNSPECIFIED., .F., .F.,
 ( 4, 2, 4 ),
 ( 2.380729204634966319E-07, 0.003943479449179620316, 0.007886720825438776200 ),
 .UNSPECIFIED. ) ;
#67040 = CARTESIAN_POINT ( 'NONE',  ( 0.1699708769753489057, 44.08204242029594866, 16.25877257701097989 ) ) ;
#67041 = CARTESIAN_POINT ( 'NONE',  ( 95.70911704725124025, 1.016364837396684119E-14, 0.000000000000000000 ) ) ;
#67042 = CARTESIAN_POINT ( 'NONE',  ( -6.446543223214487917, 3.857628234704938652, -5.000000000000000000 ) ) ;
#67043 = DIRECTION ( 'NONE',  ( 0.000000000000000000, -1.000000000000000000, 0.000000000000000000 ) ) ;
#67044 = EDGE_CURVE ( 'NONE', #51009, #98690, #72895, .T. ) ;
#67045 = ORIENTED_EDGE ( 'NONE', *, *, #104735, .F. ) ;
#67046 = CARTESIAN_POINT ( 'NONE',  ( -30.00000000002245315, 464.1822223165869445, 13.92818874393521966 ) ) ;
#67047 = CARTESIAN_POINT ( 'NONE',  ( -14.11595029531626722, 2.410436752329290222, 5.024000119293328126 ) ) ;
#67048 = CARTESIAN_POINT ( 'NONE',  ( 113.4126431804666311, -57.67118003651737723, 185.0856980667289235 ) ) ;
#67049 = ORIENTED_EDGE ( 'NONE', *, *, #51361, .F. ) ;
#67050 = AXIS2_PLACEMENT_3D ( 'NONE', #53218, #46187, #45142 ) ;
#67051 = ADVANCED_FACE ( 'NONE', ( #85314 ), #66891, .F. ) ;
#67052 = PLANE ( 'NONE',  #59224 ) ;
#67053 = CARTESIAN_POINT ( 'NONE',  ( -8.720250784003027889, 51.50345487123529864, -4.031152949374509298 ) ) ;
#67054 = DIRECTION ( 'NONE',  ( 0.000000000000000000, 0.000000000000000000, -1.000000000000000000 ) ) ;
#67055 = CARTESIAN_POINT ( 'NONE',  ( 19.96162532426522773, 302.8116070918645164, 9.928455558879880627 ) ) ;
#67056 = CARTESIAN_POINT ( 'NONE',  ( -89.92895766737007079, -60.00000000000002842, 201.9442179873481678 ) ) ;
#67057 = AXIS2_PLACEMENT_3D ( 'NONE', #48046, #13563, #47525 ) ;
#67058 = FACE_OUTER_BOUND ( 'NONE', #18309, .T. ) ;
#67059 = CARTESIAN_POINT ( 'NONE',  ( 37.96538461538461462, -4.171999999999999709, 0.000000000000000000 ) ) ;
#67060 = CARTESIAN_POINT ( 'NONE',  ( -82.99502123910362172, -60.92268927480029816, 190.5952502046357324 ) ) ;
#67061 = ORIENTED_EDGE ( 'NONE', *, *, #62568, .T. ) ;
#67062 = CARTESIAN_POINT ( 'NONE',  ( -4.524249911684786518, 53.69361481913332312, -8.281779686802252627 ) ) ;
#67063 = VERTEX_POINT ( 'NONE', #11940 ) ;
#67064 = CARTESIAN_POINT ( 'NONE',  ( -7.550180524134850302, -13.00559247213187497, 2.651855549982494509 ) ) ;
#67065 = CARTESIAN_POINT ( 'NONE',  ( 0.9999999999999997780, -32.36379547066533036, -3.982563152093286263 ) ) ;
#67066 = CARTESIAN_POINT ( 'NONE',  ( -86.65482536451017381, -60.23408797249618374, -11.84100989679749816 ) ) ;
#67067 = AXIS2_PLACEMENT_3D ( 'NONE', #17062, #99551, #25727 ) ;
#67068 = CARTESIAN_POINT ( 'NONE',  ( -3.783418949173940504, -11.62946060510804180, -10.57964823094830464 ) ) ;
#67069 = CARTESIAN_POINT ( 'NONE',  ( -15.51658955605313217, 44.08192631113433890, 4.860327001126657720 ) ) ;
#67070 = CARTESIAN_POINT ( 'NONE',  ( -43.47770857297121694, 484.8227827122652229, 4.253339224812703101 ) ) ;
#67071 = CARTESIAN_POINT ( 'NONE',  ( 28.20029758590857227, 36.30545350850469077, -9.433058495126838139 ) ) ;
#67072 = DIRECTION ( 'NONE',  ( 0.000000000000000000, -1.000000000000000000, 0.000000000000000000 ) ) ;
#67073 = CARTESIAN_POINT ( 'NONE',  ( 45.38117173420300787, -14.21045842199442077, 49.92181071548740334 ) ) ;
#67074 = CARTESIAN_POINT ( 'NONE',  ( -35.30457612798088718, 437.1674308734259284, 5.430039551431026901 ) ) ;
#67075 = CARTESIAN_POINT ( 'NONE',  ( -60.75193363616918418, -14.21045842199437281, -29.98592940458554779 ) ) ;
#67076 = CARTESIAN_POINT ( 'NONE',  ( -67.99944868274178589, -29.05959306063812519, 89.58447443812319477 ) ) ;
#67077 = ORIENTED_EDGE ( 'NONE', *, *, #51724, .T. ) ;
#67078 = CARTESIAN_POINT ( 'NONE',  ( 76.85420403038403947, -14.21045842199429288, 149.6289235591555666 ) ) ;
#67079 = SURFACE_STYLE_USAGE ( .BOTH. , #75142 ) ;
#67080 = CARTESIAN_POINT ( 'NONE',  ( 93.88541012961576371, -57.67354554259142674, 15.96172296223697806 ) ) ;
#67081 = ORIENTED_EDGE ( 'NONE', *, *, #94297, .T. ) ;
#67082 = CARTESIAN_POINT ( 'NONE',  ( 7.576405003894376655, 51.95174893343489231, -3.569492037579363952 ) ) ;
#67083 = COLOUR_RGB ( '', 0.72549020, 0.75294118, 0.79215686) ;
#67084 = DIRECTION ( 'NONE',  ( -1.000000000000000000, -0.000000000000000000, -0.000000000000000000 ) ) ;
#67085 = ORIENTED_EDGE ( 'NONE', *, *, #36033, .T. ) ;
#67086 = CARTESIAN_POINT ( 'NONE',  ( 2.649531230271432225, 14.84514140904274981, -6.482209702755499237 ) ) ;
#67087 = DIRECTION ( 'NONE',  ( -1.000000000000000000, -0.000000000000000000, -0.000000000000000000 ) ) ;
#67088 = FACE_BOUND ( 'NONE', #46038, .T. ) ;
#67089 = CARTESIAN_POINT ( 'NONE',  ( 7.188101187500001821, -14.56250000204838457, -2.977408999572650483 ) ) ;
#67090 = CARTESIAN_POINT ( 'NONE',  ( -49.07662235626727920, 14.00107037724450798, 14.92012541985352669 ) ) ;
#67091 = CARTESIAN_POINT ( 'NONE',  ( 1.570694327390588674, -0.05369876004218275545, 101.7856530012106759 ) ) ;
#67092 = LINE ( 'NONE', #31166, #92457 ) ;
#67093 = DIRECTION ( 'NONE',  ( 0.000000000000000000, 0.000000000000000000, 1.000000000000000000 ) ) ;
#67094 = CARTESIAN_POINT ( 'NONE',  ( 18.09999999999999787, -3.309499999999999886, 0.000000000000000000 ) ) ;
#67095 = UNCERTAINTY_MEASURE_WITH_UNIT (LENGTH_MEASURE( 1.000000000000000082E-05 ), #4598, 'distance_accuracy_value', 'NONE');
#67096 = ORIENTED_EDGE ( 'NONE', *, *, #26052, .T. ) ;
#67097 = CARTESIAN_POINT ( 'NONE',  ( -7.312789287434840801, 41.37363159257076006, -69.62136469306526010 ) ) ;
#67099 = CARTESIAN_POINT ( 'NONE',  ( 31.99307667142880263, -29.08164122046728295, 31.97780603565110980 ) ) ;
#67098 = CARTESIAN_POINT ( 'NONE',  ( -4.073826509765688719, -48.95212347009508846, 104.5376934966490694 ) ) ;
#67100 = CARTESIAN_POINT ( 'NONE',  ( 35.51708561081854754, 413.1995985843952894, 6.943723052262567919 ) ) ;
#67101 = ORIENTED_EDGE ( 'NONE', *, *, #18382, .T. ) ;
#67102 = CARTESIAN_POINT ( 'NONE',  ( -0.2947874284240592502, 18.79274386076835768, 49.28318674568507873 ) ) ;
#67103 = CIRCLE ( 'NONE', #41222, 7.999999999999994671 ) ;
#67104 = EDGE_LOOP ( 'NONE', ( #12010, #21408, #33447, #20264 ) ) ;
#67106 = CARTESIAN_POINT ( 'NONE',  ( -1.309314578950586894, -5.000000000000000888, 10.00000000000000178 ) ) ;
#67105 = CARTESIAN_POINT ( 'NONE',  ( -13.00000000000003730, -10.00000000000000888, 4.000000000000000000 ) ) ;
#67107 = CARTESIAN_POINT ( 'NONE',  ( 9.970195021754669540, 302.6460196488382053, -10.04373974541433689 ) ) ;
#67108 = CARTESIAN_POINT ( 'NONE',  ( -11.51023648311793934, 294.5990937745008864, -2.053736347526041506 ) ) ;
#67109 = DIRECTION ( 'NONE',  ( -0.000000000000000000, -0.000000000000000000, 1.000000000000000000 ) ) ;
#67110 = CARTESIAN_POINT ( 'NONE',  ( 32.78378308087458493, 465.0370457078494155, 14.48673668603556663 ) ) ;
#67111 = CARTESIAN_POINT ( 'NONE',  ( 0.9887502050300159828, 17.70131422926374398, -49.73213769803840023 ) ) ;
#67112 = ORIENTED_EDGE ( 'NONE', *, *, #100888, .T. ) ;
#67113 = CARTESIAN_POINT ( 'NONE',  ( 91.74875941113400302, -59.99999999999999289, -14.85367483812130551 ) ) ;
#67114 = CARTESIAN_POINT ( 'NONE',  ( 3.855937557716788584E-14, -1.200000000000000030E-05, 27.25000000000000000 ) ) ;
#67115 = FACE_OUTER_BOUND ( 'NONE', #42091, .T. ) ;
#67116 = DIRECTION ( 'NONE',  ( -1.000000000000000000, -1.224606353822377258E-16, -0.000000000000000000 ) ) ;
#67117 = VERTEX_POINT ( 'NONE', #37862 ) ;
#67118 = ADVANCED_FACE ( 'NONE', ( #38376 ), #86400, .F. ) ;
#67119 = B_SPLINE_CURVE_WITH_KNOTS ( 'NONE', 3,
 ( #14286, #32640, #64977, #80088, #89790, #81663, #64463, #48245 ),
 .UNSPECIFIED., .F., .F.,
 ( 4, 2, 2, 4 ),
 ( 0.000000000000000000, 0.2500000000000000000, 0.5000000000000000000, 1.000000000000000000 ),
 .UNSPECIFIED. ) ;
#67120 = EDGE_CURVE ( 'NONE', #42272, #6505, #59812, .T. ) ;
#67121 = DIRECTION ( 'NONE',  ( 0.000000000000000000, -1.000000000000000000, 0.000000000000000000 ) ) ;
#67122 = ORIENTED_EDGE ( 'NONE', *, *, #23603, .T. ) ;
#67123 = ORIENTED_EDGE ( 'NONE', *, *, #93201, .F. ) ;
#67124 = CARTESIAN_POINT ( 'NONE',  ( 7.550180524134852966, 81.99440752786813391, 2.651855549982491400 ) ) ;
#67125 = DIRECTION ( 'NONE',  ( 0.000000000000000000, -1.000000000000000000, 0.000000000000000000 ) ) ;
#67126 = DIRECTION ( 'NONE',  ( 0.9135154255863047190, -0.3026456445944416540, -0.2718366807917715344 ) ) ;
#67127 = CARTESIAN_POINT ( 'NONE',  ( 85.74599729795382075, -52.74913451446589363, -7.705021881710077736 ) ) ;
#67128 = CARTESIAN_POINT ( 'NONE',  ( -36.02170868991535002, 304.0253897065642263, 0.1122103735631282684 ) ) ;
#67129 = CARTESIAN_POINT ( 'NONE',  ( -6.818939631097694409, 304.7371852070875775, -9.024366697556562400 ) ) ;
#67130 = CIRCLE ( 'NONE', #103318, 0.5000000000000004441 ) ;
#67131 = ORIENTED_EDGE ( 'NONE', *, *, #25141, .F. ) ;
#67133 = EDGE_CURVE ( 'NONE', #19635, #21082, #80747, .T. ) ;
#67132 = CARTESIAN_POINT ( 'NONE',  ( -6.499999999999999112, -1.336926445781680739, -6.054363369342814494 ) ) ;
#67134 = ORIENTED_EDGE ( 'NONE', *, *, #70072, .F. ) ;
#67135 = CARTESIAN_POINT ( 'NONE',  ( 8.876331957793322402, 51.71967626501947279, -1.561720172594562195 ) ) ;
#67136 = CARTESIAN_POINT ( 'NONE',  ( 11.31153846153846132, 1.411358822780289120E-15, 0.000000000000000000 ) ) ;
#67137 = B_SPLINE_CURVE_WITH_KNOTS ( 'NONE', 3,
 ( #26882, #100193, #27421, #27956, #11166, #44094, #85624, #44636, #60820, #92096, #93172, #18237 ),
 .UNSPECIFIED., .F., .F.,
 ( 4, 2, 2, 2, 2, 4 ),
 ( 0.000000000000000000, 0.001850948747980105200, 0.002776423121970204855, 0.003701897495960304943, 0.005552846243940486905, 0.007403794991920670601 ),
 .UNSPECIFIED. ) ;
#67138 = EDGE_CURVE ( 'NONE', #49495, #102339, #40854, .T. ) ;
#67139 =( GEOMETRIC_REPRESENTATION_CONTEXT ( 3 ) GLOBAL_UNCERTAINTY_ASSIGNED_CONTEXT ( ( #83013 ) ) GLOBAL_UNIT_ASSIGNED_CONTEXT ( ( #44311, #68600, #51317 ) ) REPRESENTATION_CONTEXT ( 'NONE', 'WORKASPACE' ) );
#67141 = ORIENTED_EDGE ( 'NONE', *, *, #58663, .T. ) ;
#67140 = CARTESIAN_POINT ( 'NONE',  ( 6.509970471953121951, 51.36724606752097344, 7.565900303448065856 ) ) ;
#67142 = CARTESIAN_POINT ( 'NONE',  ( 72.65174976871776380, -46.43323079597204384, 115.6298787946136599 ) ) ;
#67143 = EDGE_LOOP ( 'NONE', ( #63487, #103639, #103422, #82496 ) ) ;
#67144 = EDGE_CURVE ( 'NONE', #3167, #93228, #32809, .T. ) ;
#67145 = CARTESIAN_POINT ( 'NONE',  ( -14.91271302809441401, 41.98564543112699710, -86.62215342991694911 ) ) ;
#67146 = CARTESIAN_POINT ( 'NONE',  ( 7.188101187500000044, -22.15625000204838457, 0.000000000000000000 ) ) ;
#67147 = CARTESIAN_POINT ( 'NONE',  ( -85.55066431120862092, -57.67066120584623690, -26.59325976709777706 ) ) ;
#67148 = ORIENTED_EDGE ( 'NONE', *, *, #96759, .F. ) ;
#67149 = CARTESIAN_POINT ( 'NONE',  ( 6.289692432696784685, 1.244805614057421469E-13, 6.828989928337167115 ) ) ;
#67150 = AXIS2_PLACEMENT_3D ( 'NONE', #82804, #8905, #776 ) ;
#67151 = CARTESIAN_POINT ( 'NONE',  ( 102.4821652698666270, -37.84834387798020572, 163.3383496542420801 ) ) ;
#67152 = CONICAL_SURFACE ( 'NONE', #87863, 5.000000000000001776, 0.9599310885968803664 ) ;
#67153 = DIRECTION ( 'NONE',  ( -0.000000000000000000, 1.000000000000000000, 0.000000000000000000 ) ) ;
#67154 = CARTESIAN_POINT ( 'NONE',  ( 7.500000000000000888, -4.999999999999999112, -20.99851272547259384 ) ) ;
#67155 = CARTESIAN_POINT ( 'NONE',  ( 5.656854249492378806, -21.87500000409676915, 5.656854249492381470 ) ) ;
#67156 = LINE ( 'NONE', #100041, #79561 ) ;
#67157 = CARTESIAN_POINT ( 'NONE',  ( 58.67238219402268840, 6.975173280561618775E-15, 0.000000000000000000 ) ) ;
#67158 = AXIS2_PLACEMENT_3D ( 'NONE', #59160, #82890, #102121 ) ;
#67159 = DIRECTION ( 'NONE',  ( 0.000000000000000000, 0.000000000000000000, 1.000000000000000000 ) ) ;
#67160 = B_SPLINE_CURVE_WITH_KNOTS ( 'NONE', 3,
 ( #49971, #75850, #7914, #82880, #8977, #73710, #34368, #1946, #41880, #65099, #97996, #24149, #847, #16015, #99579, #48895, #40817, #106614, #61823, #26810, #77452, #2481 ),
 .UNSPECIFIED., .F., .F.,
 ( 4, 2, 2, 2, 2, 2, 2, 2, 2, 2, 4 ),
 ( 2.161454313166970184E-17, 0.001055301598474675008, 0.001582952397712002537, 0.002110603196949330067, 0.002638253996186657596, 0.003165904795423985126, 0.004221206393898647991, 0.005276507992373309988, 0.006331809590847972853, 0.007387111189322636585, 0.008442412787797297716 ),
 .UNSPECIFIED. ) ;
#67161 = FACE_OUTER_BOUND ( 'NONE', #11867, .T. ) ;
#67162 = B_SPLINE_CURVE_WITH_KNOTS ( 'NONE', 3,
 ( #199, #25072, #2354, #74643, #100522, #33163, #92423, #27216, #19132, #67107 ),
 .UNSPECIFIED., .F., .F.,
 ( 4, 2, 2, 2, 4 ),
 ( -5.999999998189896673E-08, 0.001316581415853271785, 0.002633222831706525432, 0.005266505663413042701, 0.01053307132682607290 ),
 .UNSPECIFIED. ) ;
#67163 = DIRECTION ( 'NONE',  ( -0.000000000000000000, -1.000000000000000000, -0.000000000000000000 ) ) ;
#67164 = CARTESIAN_POINT ( 'NONE',  ( -0.9670823471685771056, 546.5234784715379419, 200.1325441657795068 ) ) ;
#67165 = DIRECTION ( 'NONE',  ( 0.000000000000000000, -1.000000000000000000, 0.000000000000000000 ) ) ;
#67166 = ORIENTED_EDGE ( 'NONE', *, *, #105785, .T. ) ;
#67167 = CARTESIAN_POINT ( 'NONE',  ( -5.461524205193410531, 41.98576152084350355, -59.47047328349175643 ) ) ;
#67168 = DIRECTION ( 'NONE',  ( 1.000000000000000000, 0.000000000000000000, 0.000000000000000000 ) ) ;
#67169 = CARTESIAN_POINT ( 'NONE',  ( -4.999999999999999112, -53.41520084899324416, 9.165069380062005777 ) ) ;
#67170 = CIRCLE ( 'NONE', #36177, 4.000000000000000000 ) ;
#67171 = CARTESIAN_POINT ( 'NONE',  ( -84.30164704855529578, -30.00000000000000000, 163.7302190737703711 ) ) ;
#67172 = ADVANCED_FACE ( 'NONE', ( #56507 ), #11580, .T. ) ;
#67173 = ORIENTED_EDGE ( 'NONE', *, *, #80679, .F. ) ;
#67175 = B_SPLINE_CURVE_WITH_KNOTS ( 'NONE', 3,
 ( #8346, #98935, #73603, #59044, #41782, #33715, #41250, #66058, #106507, #15914, #75197, #91414, #25095, #18061, #33188, #24573, #223, #82774, #17527, #90335, #16442, #49326, #50919, #1293, #83831, #57952, #42847, #9940, #16990, #49868, #34795, #1838, #48792, #7807, #82233, #66591, #99472, #25646, #9391, #58510, #50390 ),
 .UNSPECIFIED., .F., .F.,
 ( 4, 1, 1, 1, 1, 1, 1, 1, 1, 2, 2, 1, 1, 1, 1, 1, 1, 1, 1, 2, 2, 1, 1, 1, 1, 1, 1, 1, 1, 1, 2, 2, 4 ),
 ( 0.000000000000000000, 0.1249999999999719946, 0.1874999999999580336, 0.2187499999999505951, 0.2343749999999464040, 0.2421874999999438782, 0.2460937499999431288, 0.2480468749999432398, 0.2490234374999432954, 0.2495117187499428235, 0.2499999999999423517, 0.3749999999998880340, 0.4374999999998607225, 0.4687499999998471223, 0.4843749999998406275, 0.4921874999998376854, 0.4960937499998361866, 0.4980468749998355205, 0.4990234374998349098, 0.4995117187498344657, 0.4999999999998340217, 0.6249999999998132605, 0.6874999999998030464, 0.7187499999997978284, 0.7343749999997949418, 0.7421874999997936095, 0.7460937499997929434, 0.7480468749997928324, 0.7490234374997926103, 0.7495117187497924993, 0.7497558593747926103, 0.7499999999997927214, 1.000000000000000000 ),
 .UNSPECIFIED. ) ;
#67174 = CIRCLE ( 'NONE', #103367, 5.000000000000000000 ) ;
#67176 = CARTESIAN_POINT ( 'NONE',  ( 1.957257541017970892, -49.88613852985599095, 44.76450653543791702 ) ) ;
#67177 = CARTESIAN_POINT ( 'NONE',  ( 70.41017571245976114, -57.68249222584282165, 157.3648689374751370 ) ) ;
#67179 = DIRECTION ( 'NONE',  ( 0.5735764363510468256, 0.8191520442889913545, 0.000000000000000000 ) ) ;
#67178 = CARTESIAN_POINT ( 'NONE',  ( -14.89969599197564065, 1.346844969880335308, -1.740400043373642402 ) ) ;
#67180 = EDGE_CURVE ( 'NONE', #54015, #1507, #49487, .T. ) ;
#67181 = EDGE_CURVE ( 'NONE', #73038, #92082, #87368, .T. ) ;
#67183 = CARTESIAN_POINT ( 'NONE',  ( 37.43042651949708954, -32.13357833424133503, -37.68003761008185393 ) ) ;
#67182 = STYLED_ITEM ( 'NONE', ( #22954 ), #72138 ) ;
#67184 = CARTESIAN_POINT ( 'NONE',  ( -1.101319585913861587, 43.39549463643071192, 18.11240750576352809 ) ) ;
#67185 = CARTESIAN_POINT ( 'NONE',  ( -43.21801493131978589, 434.4543138596390008, 16.17410598222931029 ) ) ;
#67186 = CARTESIAN_POINT ( 'NONE',  ( -47.26077543882751542, -59.99999999999999289, 65.36119327807321611 ) ) ;
#67187 = LINE ( 'NONE', #11578, #58895 ) ;
#67188 = AXIS2_PLACEMENT_3D ( 'NONE', #105908, #159, #84180 ) ;
#67189 = CARTESIAN_POINT ( 'NONE',  ( 37.56208910883223240, 463.3609840191073772, 20.02047205468278790 ) ) ;
#67190 = CARTESIAN_POINT ( 'NONE',  ( -86.71692066761134754, -24.38214587370727671, 185.1863996357423900 ) ) ;
#67191 = VERTEX_POINT ( 'NONE', #91040 ) ;
#67192 = CARTESIAN_POINT ( 'NONE',  ( -42.76313255036283323, 461.1833584523140530, 3.199811539384791459 ) ) ;
#67193 = CARTESIAN_POINT ( 'NONE',  ( -9.152872775044887277, -32.51284889757581453, 29.31026127488318167 ) ) ;
#67194 = CARTESIAN_POINT ( 'NONE',  ( -5.420469775605653240, 41.88321586335170821, -59.04137891894602319 ) ) ;
#67195 = DIRECTION ( 'NONE',  ( -1.000000000000000000, -1.224606353822377258E-16, -0.000000000000000000 ) ) ;
#67197 = CARTESIAN_POINT ( 'NONE',  ( 5.146676080590609104, -67.38655984587389014, 13.97995438629998155 ) ) ;
#67196 = CARTESIAN_POINT ( 'NONE',  ( -38.64834039627831430, 312.1053154204562929, 6.072046802107182728 ) ) ;
#67198 = ORIENTED_EDGE ( 'NONE', *, *, #10031, .T. ) ;
#67199 = EDGE_CURVE ( 'NONE', #72931, #106311, #57562, .T. ) ;
#67200 = CARTESIAN_POINT ( 'NONE',  ( 5.041270396327364622, 41.82074884801023984, -70.25592674792672199 ) ) ;
#67201 = B_SPLINE_CURVE_WITH_KNOTS ( 'NONE', 3,
 ( #27245, #25649, #91417, #1296, #51995, #50392, #59583, #42850, #83304, #34797 ),
 .UNSPECIFIED., .F., .F.,
 ( 4, 2, 2, 2, 4 ),
 ( 0.009353627468483458399, 0.01031000219096075976, 0.01126637691343805939, 0.01222275163591535901, 0.01317912635839266038 ),
 .UNSPECIFIED. ) ;
#67202 = CARTESIAN_POINT ( 'NONE',  ( 40.34715123528543046, 1.340359594676612611E-15, 0.000000000000000000 ) ) ;
#67203 = CARTESIAN_POINT ( 'NONE',  ( -30.63590201688455750, 10.93049107008196330, -40.03749794393677774 ) ) ;
#67204 = AXIS2_PLACEMENT_3D ( 'NONE', #29388, #78956, #44482 ) ;
#67205 = CARTESIAN_POINT ( 'NONE',  ( 26.15475286542767819, 304.5035472506963856, -9.639477703573707146 ) ) ;
#67206 = DIRECTION ( 'NONE',  ( -0.5735764363510459374, -0.8191520442889919096, 0.000000000000000000 ) ) ;
#67207 = EDGE_CURVE ( 'NONE', #24536, #80654, #25387, .T. ) ;
#67208 = FACE_OUTER_BOUND ( 'NONE', #88783, .T. ) ;
#67209 = CARTESIAN_POINT ( 'NONE',  ( 109.0818019194042847, -30.00000000000000355, 182.6293461004923131 ) ) ;
#67210 = CARTESIAN_POINT ( 'NONE',  ( -83.35807197383493872, -25.61544833356139250, 152.1595157485745347 ) ) ;
#67211 = ORIENTED_EDGE ( 'NONE', *, *, #83714, .F. ) ;
#67212 = PLANE ( 'NONE',  #87781 ) ;
#67213 = DIRECTION ( 'NONE',  ( 0.000000000000000000, 0.000000000000000000, -1.000000000000000000 ) ) ;
#67214 = CARTESIAN_POINT ( 'NONE',  ( -5.656854249492381470, -20.75000000409676915, 5.656854249492379694 ) ) ;
#67215 = CARTESIAN_POINT ( 'NONE',  ( -7.101747359475742982, -4.047770588416829796, -17.37629258578624203 ) ) ;
#67216 = EDGE_CURVE ( 'NONE', #41081, #88535, #97363, .T. ) ;
#67217 = CARTESIAN_POINT ( 'NONE',  ( -42.09158233638504498, 465.7816406625409513, 14.79318349170026892 ) ) ;
#67218 = LINE ( 'NONE', #82315, #90641 ) ;
#67219 = VERTEX_POINT ( 'NONE', #78027 ) ;
#67220 = CARTESIAN_POINT ( 'NONE',  ( -22.85358936945000252, 305.5818686480074575, 9.095431853656572585 ) ) ;
#67221 = ORIENTED_EDGE ( 'NONE', *, *, #13288, .T. ) ;
#67222 = CARTESIAN_POINT ( 'NONE',  ( 34.14275462543660922, 484.1047237107248407, 0.7219141280516476744 ) ) ;
#67223 =( BOUNDED_CURVE ( )  B_SPLINE_CURVE ( 2, ( #26934, #101321, #9625, #60349, #27471, #75970, #93225, #19914, #19387 ),
 .UNSPECIFIED., .F., .F. ) 
 B_SPLINE_CURVE_WITH_KNOTS ( ( 3, 2, 2, 2, 3 ),
 ( 0.8382352941176473005, 0.8455882352941177516, 0.8529411764705883137, 0.8602941176470588758, 0.8676470588235294379 ),
 .UNSPECIFIED. ) 
 CURVE ( )  GEOMETRIC_REPRESENTATION_ITEM ( )  RATIONAL_B_SPLINE_CURVE ( ( 0.9999999999999976685, 0.9238795325112890700, 1.000000000000000000, 0.9238795325112867385, 1.000000000000000000, 0.9238795325112867385, 1.000000000000000000, 0.9238795325112867385, 1.000000000000000000 ) ) 
 REPRESENTATION_ITEM ( '' )  );
#67224 = DIRECTION ( 'NONE',  ( -1.000000000000000000, 1.224646799147351482E-16, 0.000000000000000000 ) ) ;
#67225 = CARTESIAN_POINT ( 'NONE',  ( 32.00986601473097437, 486.4616239121639296, 6.105527853532677796 ) ) ;
#67226 = CARTESIAN_POINT ( 'NONE',  ( -50.18984356160270011, 50.00000000000000000, 38.51389699557558544 ) ) ;
#67227 = CARTESIAN_POINT ( 'NONE',  ( 5.000000000000000000, -14.43521912202222524, 12.17944458656167583 ) ) ;
#67228 = CIRCLE ( 'NONE', #15463, 7.000000000000000000 ) ;
#67229 = CARTESIAN_POINT ( 'NONE',  ( 44.23810852895211809, 435.1998687191861563, 14.01156801387538309 ) ) ;
#67230 = ORIENTED_EDGE ( 'NONE', *, *, #33, .T. ) ;
#67231 = CARTESIAN_POINT ( 'NONE',  ( 112.0559613019898535, -60.00000000000000000, 178.9342536578935210 ) ) ;
#67233 = CARTESIAN_POINT ( 'NONE',  ( 21.50664772083280951, -46.43444599742699808, 32.33001467109113491 ) ) ;
#67232 = CARTESIAN_POINT ( 'NONE',  ( -97.13635602990564166, -30.00000000000002842, 199.9106954788804842 ) ) ;
#67235 = CARTESIAN_POINT ( 'NONE',  ( 0.000000000000000000, 0.000000000000000000, 0.000000000000000000 ) ) ;
#67234 = PRODUCT_DEFINITION_CONTEXT ( 'detailed design', #72768, 'design' ) ;
#67236 = CARTESIAN_POINT ( 'NONE',  ( 0.000000000000000000, 5.629165124598848102, 3.250000000000005329 ) ) ;
#67237 = AXIS2_PLACEMENT_3D ( 'NONE', #35912, #60692, #4033 ) ;
#67238 = CARTESIAN_POINT ( 'NONE',  ( -40.62314756017665474, -49.89205973216389367, 41.58854808969374517 ) ) ;
#67239 = CARTESIAN_POINT ( 'NONE',  ( -8.719137237811853680, 53.63217708511133708, -4.031152949374852135 ) ) ;
#67240 = EDGE_LOOP ( 'NONE', ( #90640, #71686, #61141, #80745, #8456 ) ) ;
#67241 = CARTESIAN_POINT ( 'NONE',  ( 51.01037695545453232, 500.0000000000002274, 0.000000000000000000 ) ) ;
#67242 = FACE_OUTER_BOUND ( 'NONE', #4824, .T. ) ;
#67243 = CARTESIAN_POINT ( 'NONE',  ( 40.93435977689158989, 414.3154843149413296, 27.72243992809649527 ) ) ;
#67244 = FACE_OUTER_BOUND ( 'NONE', #62206, .T. ) ;
#67245 = CARTESIAN_POINT ( 'NONE',  ( -1.469576158976823947E-15, -23.37499999999999289, 8.000000000000000000 ) ) ;
#67246 = ORIENTED_EDGE ( 'NONE', *, *, #57181, .F. ) ;
#67247 = DIRECTION ( 'NONE',  ( 0.000000000000000000, 1.000000000000000000, 0.000000000000000000 ) ) ;
#67248 = EDGE_LOOP ( 'NONE', ( #52215, #79643 ) ) ;
#67249 = CARTESIAN_POINT ( 'NONE',  ( 81.59257212631717948, -30.00000000000000711, -7.373243558649345886 ) ) ;
#67250 = CARTESIAN_POINT ( 'NONE',  ( 47.07447497471061126, 13.47837589781632950, 14.79567547011555995 ) ) ;
#67252 = CARTESIAN_POINT ( 'NONE',  ( 24.17890427073063009, 25.18054377835295909, -32.75958092602339633 ) ) ;
#67251 = AXIS2_PLACEMENT_3D ( 'NONE', #96569, #87947, #7523 ) ;
#67253 = CARTESIAN_POINT ( 'NONE',  ( -8.000000000000000000, 9.797174393178825657E-16, -13.00000000000000000 ) ) ;
#67254 = CARTESIAN_POINT ( 'NONE',  ( 83.46915891402045418, -30.00000000000000000, 46.60997905724752144 ) ) ;
#67255 = CIRCLE ( 'NONE', #86200, 5.000000000000000000 ) ;
#67256 = ORIENTED_EDGE ( 'NONE', *, *, #38291, .T. ) ;
#67257 = B_SPLINE_CURVE_WITH_KNOTS ( 'NONE', 3,
 ( #19135, #22836, #105835, #40050, #71878, #96699 ),
 .UNSPECIFIED., .F., .F.,
 ( 4, 2, 4 ),
 ( 2.380731629580637688E-07, 0.002336973833157565076, 0.004673709593152172194 ),
 .UNSPECIFIED. ) ;
#67258 = ADVANCED_FACE ( 'NONE', ( #34943 ), #59200, .T. ) ;
#67259 = CIRCLE ( 'NONE', #70713, 4.000000000000000888 ) ;
#67260 = ORIENTED_EDGE ( 'NONE', *, *, #71996, .F. ) ;
#67261 = VERTEX_POINT ( 'NONE', #3074 ) ;
#67262 = CARTESIAN_POINT ( 'NONE',  ( -46.79842100651292469, 13.68672532571791400, -15.36912611011954510 ) ) ;
#67263 = FACE_BOUND ( 'NONE', #101298, .T. ) ;
#67264 = CARTESIAN_POINT ( 'NONE',  ( -36.31400481676831760, 26.07308277780756711, -12.05999164150846070 ) ) ;
#67265 = CARTESIAN_POINT ( 'NONE',  ( 4.472135954999580498, -10.00000000000000888, 4.000000000000000000 ) ) ;
#67266 = CARTESIAN_POINT ( 'NONE',  ( 5.819846122303830249, 4.937269551422757807, -4.448398286272981395 ) ) ;
#67267 = EDGE_CURVE ( 'NONE', #71589, #40596, #15131, .T. ) ;
#67268 = ORIENTED_EDGE ( 'NONE', *, *, #2418, .F. ) ;
#67270 = ADVANCED_FACE ( 'NONE', ( #43540 ), #27188, .T. ) ;
#67269 = CARTESIAN_POINT ( 'NONE',  ( -9.739726766104316980, 49.99999999999999289, -87.61747884499031613 ) ) ;
#67271 = AXIS2_PLACEMENT_3D ( 'NONE', #25848, #81349, #7461 ) ;
#67272 = EDGE_LOOP ( 'NONE', ( #69995, #102586, #40975, #45717 ) ) ;
#67273 = CARTESIAN_POINT ( 'NONE',  ( 61.26180592153973237, -38.34168193138184222, 100.4494290447654663 ) ) ;
#67274 = LINE ( 'NONE', #66730, #40341 ) ;
#67275 = CARTESIAN_POINT ( 'NONE',  ( 33.80977330536913428, 301.4714739734875479, 3.439059217111231082 ) ) ;
#67276 = EDGE_CURVE ( 'NONE', #46183, #11885, #51071, .T. ) ;
#67277 = CARTESIAN_POINT ( 'NONE',  ( -5.911778709945829213, 246.1333816058341881, 1.058844270818183109 ) ) ;
#67278 = ORIENTED_EDGE ( 'NONE', *, *, #90254, .F. ) ;
#67279 = ADVANCED_FACE ( 'NONE', ( #10096, #19319 ), #43007, .F. ) ;
#67280 = CARTESIAN_POINT ( 'NONE',  ( 17.86532138382082024, 45.30096510830348677, -5.720552158557850930 ) ) ;
#67281 = CARTESIAN_POINT ( 'NONE',  ( 35.65344923961711032, 304.2588450519185699, 4.111980580341269231 ) ) ;
#67282 = FACE_OUTER_BOUND ( 'NONE', #42965, .T. ) ;
#67283 = VERTEX_POINT ( 'NONE', #18766 ) ;
#67284 = CARTESIAN_POINT ( 'NONE',  ( -22.56879301375676050, 303.3526548909255780, 10.04479196209192615 ) ) ;
#67285 = CARTESIAN_POINT ( 'NONE',  ( 8.399605801963765828, 54.02078684658069108, -1.531152949374517291 ) ) ;
#67286 =( LENGTH_UNIT ( ) NAMED_UNIT ( * ) SI_UNIT ( .MILLI., .METRE. ) );
#67287 = CARTESIAN_POINT ( 'NONE',  ( -5.656854249492379694, -11.93749999999999289, -5.656854249492380582 ) ) ;
#67288 = CARTESIAN_POINT ( 'NONE',  ( 32.33349330513379982, 4.898587196589405926E-16, -4.000000000000001776 ) ) ;
#67289 = VECTOR ( 'NONE', #101913, 1000.000000000000000 ) ;
#67290 = DIRECTION ( 'NONE',  ( 1.000000000000000000, 0.000000000000000000, 0.000000000000000000 ) ) ;
#67291 = STYLED_ITEM ( 'NONE', ( #79184 ), #102995 ) ;
#67292 = CARTESIAN_POINT ( 'NONE',  ( 46.00000000000000000, 461.8824355614426054, 11.41562375511947458 ) ) ;
#67293 = APPLICATION_CONTEXT ( 'automotive_design' ) ;
#67294 = CARTESIAN_POINT ( 'NONE',  ( 85.68501797939430276, -39.26251600558322963, 186.0341779385333894 ) ) ;
#67295 = CARTESIAN_POINT ( 'NONE',  ( 17.74039601254145637, 36.76373445370536075, -22.27539783717256228 ) ) ;
#67296 = CARTESIAN_POINT ( 'NONE',  ( -8.309329435532722741, 32.78459446883342565, 5.000000000001270095 ) ) ;
#67297 = ORIENTED_EDGE ( 'NONE', *, *, #30809, .T. ) ;
#67298 = CARTESIAN_POINT ( 'NONE',  ( 93.17075602859650019, -57.65531965366547240, -16.78974746904759741 ) ) ;
#67299 = LINE ( 'NONE', #73769, #31529 ) ;
#67300 = CARTESIAN_POINT ( 'NONE',  ( 15.73368388934906470, 35.06301254113061105, -22.31274010331293312 ) ) ;
#67301 = CARTESIAN_POINT ( 'NONE',  ( -94.04704852291118300, -29.99999999999999645, 112.2487365680688782 ) ) ;
#67302 = AXIS2_PLACEMENT_3D ( 'NONE', #80880, #62086, #53948 ) ;
#67303 = CONICAL_SURFACE ( 'NONE', #19147, 8.000000000000000000, 0.9599310885968911355 ) ;
#67304 = SURFACE_STYLE_FILL_AREA ( #68367 ) ;
#67305 = DIRECTION ( 'NONE',  ( -0.000000000000000000, -0.000000000000000000, 1.000000000000000000 ) ) ;
#67306 = DIRECTION ( 'NONE',  ( 0.000000000000000000, 1.000000000000000000, 0.000000000000000000 ) ) ;
#67308 = CARTESIAN_POINT ( 'NONE',  ( 92.53532739719321398, 1.030564683017419500E-14, 0.000000000000000000 ) ) ;
#67307 = CARTESIAN_POINT ( 'NONE',  ( 106.4000000000000057, 5.109226446042757607E-16, -4.171999999999999709 ) ) ;
#67309 = EDGE_CURVE ( 'NONE', #10763, #14964, #40826, .T. ) ;
#67310 = SURFACE_STYLE_USAGE ( .BOTH. , #40895 ) ;
#67311 = CARTESIAN_POINT ( 'NONE',  ( -32.09911992168218831, 438.9232547152092252, 23.66653216045979491 ) ) ;
#67312 = CARTESIAN_POINT ( 'NONE',  ( -11.28790243858421150, -9.071383756617100502, -0.5355294694855911031 ) ) ;
#67313 = CARTESIAN_POINT ( 'NONE',  ( 4.503026011213025370, -84.45658137716684166, 3.965236350746919047 ) ) ;
#67314 = DIRECTION ( 'NONE',  ( -1.000000000000000000, -0.000000000000000000, -0.000000000000000000 ) ) ;
#67315 = LINE ( 'NONE', #9048, #89071 ) ;
#67316 = CARTESIAN_POINT ( 'NONE',  ( 19.76895601567771266, -18.47386612047070997, -33.76156256446066095 ) ) ;
#67317 = CARTESIAN_POINT ( 'NONE',  ( -25.87975877140922520, -18.61425406802221261, 28.34855765540077499 ) ) ;
#67318 = AXIS2_PLACEMENT_3D ( 'NONE', #76795, #8873, #59577 ) ;
#67319 = ORIENTED_EDGE ( 'NONE', *, *, #96766, .F. ) ;
#67320 = CARTESIAN_POINT ( 'NONE',  ( 7.000111909206518490, 8.999804158740396076, 0.1284026198027884424 ) ) ;
#67321 = FACE_OUTER_BOUND ( 'NONE', #70010, .T. ) ;
#67322 = CARTESIAN_POINT ( 'NONE',  ( -7.344133061198930612, 82.55505607319422268, 3.176267128233873471 ) ) ;
#67323 = CARTESIAN_POINT ( 'NONE',  ( -66.26923848658640281, -29.83372399135324571, -22.51683101449095759 ) ) ;
#67324 = AXIS2_PLACEMENT_3D ( 'NONE', #61301, #69392, #11119 ) ;
#67325 = LINE ( 'NONE', #66786, #99928 ) ;
#67326 = EDGE_LOOP ( 'NONE', ( #20488, #82599 ) ) ;
#67327 = CIRCLE ( 'NONE', #93115, 4.000000000000000888 ) ;
#67328 = DIRECTION ( 'NONE',  ( 5.329070518200750605E-15, 0.000000000000000000, -1.000000000000000000 ) ) ;
#67329 = VERTEX_POINT ( 'NONE', #11142 ) ;
#67330 = CARTESIAN_POINT ( 'NONE',  ( -25.88320034774018907, 35.08514486786264541, 8.494208376200145238 ) ) ;
#67331 = AXIS2_PLACEMENT_3D ( 'NONE', #22728, #24322, #47488 ) ;
#67332 =( LENGTH_UNIT ( ) NAMED_UNIT ( * ) SI_UNIT ( .MILLI., .METRE. ) );
#67333 = CARTESIAN_POINT ( 'NONE',  ( -87.91896268344133603, -59.99999999999997868, -21.67466428380060250 ) ) ;
#67334 = B_SPLINE_CURVE_WITH_KNOTS ( 'NONE', 3,
 ( #39028, #70331, #6103, #88107, #63308, #104272, #30960, #21278, #95146, #22861, #21804, #78410, #46056, #71910, #54116, #56224, #30415, #104811, #4524, #55698, #103750, #79470, #103229, #39565, #63836, #88629, #54643, #37469, #78941, #79994, #38507, #29372, #47092, #5063, #96205, #95665, #62261, #6638, #22334, #14719, #55181 ),
 .UNSPECIFIED., .F., .F.,
 ( 4, 1, 1, 1, 1, 1, 1, 1, 1, 1, 2, 2, 1, 1, 1, 1, 1, 1, 1, 1, 2, 2, 1, 1, 1, 1, 1, 1, 1, 1, 2, 2, 4 ),
 ( 0.000000000000000000, 0.1250000000000022482, 0.1875000000000033029, 0.2187500000000036915, 0.2343750000000039413, 0.2421875000000038858, 0.2460937500000036637, 0.2480468750000034694, 0.2490234375000036360, 0.2495117187500037470, 0.2497558593750039968, 0.2500000000000042188, 0.3750000000000879297, 0.4375000000001293410, 0.4687500000001500466, 0.4843750000001602052, 0.4921875000001652567, 0.4960937500001676437, 0.4980468750001689759, 0.4990234375001694755, 0.4995117187501696976, 0.5000000000001699751, 0.6250000000002530198, 0.6875000000002948752, 0.7187500000003157474, 0.7343750000003267386, 0.7421875000003321787, 0.7460937500003348433, 0.7480468750003361755, 0.7490234375003363976, 0.7495117187503365086, 0.7500000000003367306, 1.000000000000000000 ),
 .UNSPECIFIED. ) ;
#67335 = ORIENTED_EDGE ( 'NONE', *, *, #56410, .F. ) ;
#67336 = DIRECTION ( 'NONE',  ( 0.000000000000000000, 0.000000000000000000, -1.000000000000000000 ) ) ;
#67337 = CARTESIAN_POINT ( 'NONE',  ( -5.385569124936798957, 294.7724401061256572, -8.430686591128788265 ) ) ;
#67338 = CARTESIAN_POINT ( 'NONE',  ( 101.8255536633035092, -60.21687307657023069, 194.3872987722783137 ) ) ;
#67339 = CARTESIAN_POINT ( 'NONE',  ( -3.910135399454920169, -1.060349490810097439, 104.5757312272370427 ) ) ;
#67340 = EDGE_CURVE ( 'NONE', #9861, #37699, #40922, .T. ) ;
#67341 = EDGE_LOOP ( 'NONE', ( #99689, #29859, #83665, #4292 ) ) ;
#67342 = VERTEX_POINT ( 'NONE', #62916 ) ;
#67343 = EDGE_LOOP ( 'NONE', ( #8210, #44339, #94257, #106342, #46850 ) ) ;
#67344 = CARTESIAN_POINT ( 'NONE',  ( 30.72323423254651686, 348.3287414960516912, 19.95724199425579570 ) ) ;
#67345 = CARTESIAN_POINT ( 'NONE',  ( -13.50000000000000355, 3.304540750553675021, -12.77799806994943310 ) ) ;
#67346 = CARTESIAN_POINT ( 'NONE',  ( 9.170976460981439260, 53.73491031865484047, 1.679364399482070391 ) ) ;
#67347 = ORIENTED_EDGE ( 'NONE', *, *, #5600, .F. ) ;
#67348 = CARTESIAN_POINT ( 'NONE',  ( 0.000000000000000000, 47.00000000000000000, -56.99999999999999289 ) ) ;
#67349 = CARTESIAN_POINT ( 'NONE',  ( 26.08349330513380337, 1.593028355512270567E-15, 0.000000000000000000 ) ) ;
#67350 = CARTESIAN_POINT ( 'NONE',  ( 12.21253585067004543, -5.000000000000000000, 0.000000000000000000 ) ) ;
#67352 = CARTESIAN_POINT ( 'NONE',  ( -30.75663703201544408, -57.68613454458090217, 45.71164565728040685 ) ) ;
#67351 = CONICAL_SURFACE ( 'NONE', #34660, 8.000000000000000000, 1.047197551196600296 ) ;
#67353 = CARTESIAN_POINT ( 'NONE',  ( -29.77344787310991947, 13.34785391060250959, 42.10535821593509098 ) ) ;
#67354 = DIRECTION ( 'NONE',  ( -1.000000000000000000, -0.000000000000000000, -0.000000000000000000 ) ) ;
#67355 = FACE_OUTER_BOUND ( 'NONE', #86766, .T. ) ;
#67356 = CARTESIAN_POINT ( 'NONE',  ( -82.54102867968215662, -60.00000000000007105, -29.20875881225653004 ) ) ;
#67357 = CYLINDRICAL_SURFACE ( 'NONE', #1682, 1.250000000000001110 ) ;
#67358 = ADVANCED_FACE ( 'NONE', ( #45665 ), #87452, .T. ) ;
#67359 = CARTESIAN_POINT ( 'NONE',  ( -52.40382998801522518, -22.17894777271752460, 48.78687196755927857 ) ) ;
#67360 = CIRCLE ( 'NONE', #91458, 4.000000000000001776 ) ;
#67361 = CARTESIAN_POINT ( 'NONE',  ( -1.058190070889937440, 21.71930410792606025, 6.924500316192023774 ) ) ;
#67362 = VERTEX_POINT ( 'NONE', #47233 ) ;
#67363 = CARTESIAN_POINT ( 'NONE',  ( 0.000000000000000000, 4.898587196589413815E-16, -4.000000000000000888 ) ) ;
#67364 = CARTESIAN_POINT ( 'NONE',  ( -9.659964574194615849, 294.6522956596209610, -2.587254427031161264 ) ) ;
#67365 = CARTESIAN_POINT ( 'NONE',  ( 11.59943540149712504, -1.679055970110489460, 20.57194209593012957 ) ) ;
#67366 = ORIENTED_EDGE ( 'NONE', *, *, #76842, .T. ) ;
#67367 = CARTESIAN_POINT ( 'NONE',  ( 79.42188716763993739, -38.73604089626370950, 191.9100328722365418 ) ) ;
#67368 = FILL_AREA_STYLE_COLOUR ( '', #53719 ) ;
#67369 = CARTESIAN_POINT ( 'NONE',  ( 0.000000000000000000, 0.000000000000000000, -13.00000000000000000 ) ) ;
#67370 = CARTESIAN_POINT ( 'NONE',  ( -12.39854599882999153, -8.430153398135473708, -12.16137996778341268 ) ) ;
#67371 = FILL_AREA_STYLE_COLOUR ( '', #29098 ) ;
#67372 = CARTESIAN_POINT ( 'NONE',  ( 87.77046421779371599, -29.99999999999999645, 186.1866013582121298 ) ) ;
#67373 = CYLINDRICAL_SURFACE ( 'NONE', #90617, 3.400000000000000355 ) ;
#67374 = CARTESIAN_POINT ( 'NONE',  ( 18.91791044776121211, 44.85000000000000853, 62.18611311450882795 ) ) ;
#67375 = DIRECTION ( 'NONE',  ( 0.000000000000000000, 0.000000000000000000, -1.000000000000000000 ) ) ;
#67376 = AXIS2_PLACEMENT_3D ( 'NONE', #86233, #103449, #12306 ) ;
#67377 = ADVANCED_FACE ( 'NONE', ( #21939 ), #53746, .F. ) ;
#67378 = ORIENTED_EDGE ( 'NONE', *, *, #53965, .T. ) ;
#67379 = ORIENTED_EDGE ( 'NONE', *, *, #49507, .F. ) ;
#67380 = CARTESIAN_POINT ( 'NONE',  ( 51.22218799938233502, -60.30135857894056528, 60.32169156076044203 ) ) ;
#67381 = CARTESIAN_POINT ( 'NONE',  ( 6.263553873705014041, 41.61160258182582083, -58.64895314702076945 ) ) ;
#67382 = FACE_OUTER_BOUND ( 'NONE', #80246, .T. ) ;
#67383 =( BOUNDED_SURFACE ( )  B_SPLINE_SURFACE ( 3, 2, ( 
 ( #10502, #92482, #28321 ),
 ( #19184, #18632, #101113 ),
 ( #83861, #3489, #61198 ),
 ( #76297, #93022, #9973 ) ),
 .UNSPECIFIED., .F., .F., .F. ) 
 B_SPLINE_SURFACE_WITH_KNOTS ( ( 4, 4 ),
 ( 3, 3 ),
 ( 6.938893903907228378E-18, 0.001025706331908567614 ),
 ( 0.000000000000000000, 1.000000000000000000 ),
 .UNSPECIFIED. ) 
 GEOMETRIC_REPRESENTATION_ITEM ( )  RATIONAL_B_SPLINE_SURFACE ( (
 ( 1.000000000000000000, 0.9153908114178146427, 1.000000000000000000),
 ( 1.000000000000000000, 0.9167125567853761092, 1.000000000000000000),
 ( 1.000000000000000000, 0.9180307555289068944, 1.000000000000000000),
 ( 1.000000000000000000, 0.9193453746270491278, 1.000000000000000000) ) ) 
 REPRESENTATION_ITEM ( '' )  SURFACE ( )  );
#67384 = EDGE_CURVE ( 'NONE', #41440, #19817, #92594, .T. ) ;
#67385 = ORIENTED_EDGE ( 'NONE', *, *, #11882, .F. ) ;
#67386 = CARTESIAN_POINT ( 'NONE',  ( -92.65791048185651846, -38.35495741458606034, 40.59163175469802809 ) ) ;
#67387 = ORIENTED_EDGE ( 'NONE', *, *, #44202, .F. ) ;
#67388 = SURFACE_STYLE_USAGE ( .BOTH. , #100794 ) ;
#67389 = CARTESIAN_POINT ( 'NONE',  ( 110.2552427511137267, -38.35601349421322226, 184.2954527649220893 ) ) ;
#67390 = CARTESIAN_POINT ( 'NONE',  ( 12.60415904244543484, 22.93641037622941070, -5.610498527788345235 ) ) ;
#67391 = CARTESIAN_POINT ( 'NONE',  ( 87.11640230159049736, -52.71607002794502250, 42.63259187033803954 ) ) ;
#67392 = CARTESIAN_POINT ( 'NONE',  ( 5.075566108724594017, -4.332661967060489339, -17.09624963492156269 ) ) ;
#67393 = CARTESIAN_POINT ( 'NONE',  ( -21.14633401031152360, 303.9368958959844917, -9.981912898654558219 ) ) ;
#67394 = CARTESIAN_POINT ( 'NONE',  ( 0.000000000000000000, 0.000000000000000000, 4.000000000000000000 ) ) ;
#67395 =( BOUNDED_SURFACE ( )  B_SPLINE_SURFACE ( 3, 2, ( 
 ( #79862, #15132, #96067 ),
 ( #87979, #64756, #38900 ),
 ( #104676, #80925, #88507 ),
 ( #97110, #30827, #54509 ),
 ( #71243, #48015, #80389 ),
 ( #22198, #104141, #62645 ),
 ( #56643, #89562, #6498 ),
 ( #78802, #39435, #46963 ),
 ( #95529, #71764, #63712 ),
 ( #7036, #96600, #4934 ),
 ( #37866, #21675, #75489 ),
 ( #98172, #41531, #100296 ),
 ( #26458, #81975, #34011 ),
 ( #66338, #58797, #8630 ),
 ( #59323, #17278, #49077 ),
 ( #8097, #65281, #495 ),
 ( #90624, #16190, #16730 ),
 ( #50656, #41007, #24843 ) ),
 .UNSPECIFIED., .F., .F., .F. ) 
 B_SPLINE_SURFACE_WITH_KNOTS ( ( 4, 2, 2, 2, 2, 2, 2, 2, 4 ),
 ( 3, 3 ),
 ( 0.0001601145914732075891, 0.001714143494069139120, 0.002491157945367104831, 0.003268172396665070759, 0.004822201299261002182, 0.006376230201856934038, 0.007930259104452865027, 0.009484288007048796015, 0.01259234581224065973 ),
 ( 0.000000000000000000, 1.000000000000000000 ),
 .UNSPECIFIED. ) 
 GEOMETRIC_REPRESENTATION_ITEM ( )  RATIONAL_B_SPLINE_SURFACE ( (
 ( 1.000000000000000000, 0.9028401456532980651, 1.000000000000000000),
 ( 1.000000000000000000, 0.9067333287510357387, 1.000000000000000000),
 ( 1.000000000000000000, 0.9090942099086769534, 1.000000000000000000),
 ( 1.000000000000000000, 0.9101952033055793478, 1.000000000000000000),
 ( 1.000000000000000000, 0.9101526397032935201, 1.000000000000000000),
 ( 1.000000000000000000, 0.9092257979258016043, 1.000000000000000000),
 ( 1.000000000000000000, 0.9083503838810818021, 1.000000000000000000),
 ( 1.000000000000000000, 0.9045634707242991013, 1.000000000000000000),
 ( 1.000000000000000000, 0.9004851055695014539, 1.000000000000000000),
 ( 1.000000000000000000, 0.8895482392855161846, 1.000000000000000000),
 ( 1.000000000000000000, 0.8828580819741439489, 1.000000000000000000),
 ( 1.000000000000000000, 0.8675505019241241955, 1.000000000000000000),
 ( 1.000000000000000000, 0.8588864831504116060, 1.000000000000000000),
 ( 1.000000000000000000, 0.8401763864807653137, 1.000000000000000000),
 ( 1.000000000000000000, 0.8302671801042916799, 1.000000000000000000),
 ( 1.000000000000000000, 0.7996378488151107966, 1.000000000000000000),
 ( 1.000000000000000000, 0.7777557150150771204, 1.000000000000000000),
 ( 1.000000000000000000, 0.7583909709667374655, 1.000000000000000000) ) ) 
 REPRESENTATION_ITEM ( '' )  SURFACE ( )  );
#67396 = CARTESIAN_POINT ( 'NONE',  ( -33.67444716837063368, 489.3309112354450008, 10.55021651976771757 ) ) ;
#67397 = MECHANICAL_DESIGN_GEOMETRIC_PRESENTATION_REPRESENTATION (  '', ( #51818 ), #26090 ) ;
#67398 = VECTOR ( 'NONE', #12985, 1000.000000000000000 ) ;
#67399 = ADVANCED_FACE ( 'NONE', ( #54249 ), #61673, .T. ) ;
#67400 = DIRECTION ( 'NONE',  ( 1.000000000000000000, -0.000000000000000000, -0.000000000000000000 ) ) ;
#67401 = VERTEX_POINT ( 'NONE', #5722 ) ;
#67402 = CARTESIAN_POINT ( 'NONE',  ( 60.36974275104975618, -29.06706137689814540, 68.28589426947422680 ) ) ;
#67403 = EDGE_CURVE ( 'NONE', #66609, #33845, #5207, .T. ) ;
#67404 = CARTESIAN_POINT ( 'NONE',  ( 0.000000000000000000, -99.99999999999997158, 0.000000000000000000 ) ) ;
#67405 = LINE ( 'NONE', #92723, #2259 ) ;
#67406 = AXIS2_PLACEMENT_3D ( 'NONE', #1064, #66911, #7580 ) ;
#67407 = FACE_OUTER_BOUND ( 'NONE', #89414, .T. ) ;
#67408 = EDGE_CURVE ( 'NONE', #35550, #88549, #75411, .T. ) ;
#67409 = CARTESIAN_POINT ( 'NONE',  ( -42.70310427752711746, 433.3420030442914594, 18.58178892519891079 ) ) ;
#67410 = CARTESIAN_POINT ( 'NONE',  ( -6.874999999999999112, -4.690970937165719334, -7.298562697733108173 ) ) ;
#67411 = DIRECTION ( 'NONE',  ( 0.05555555555555551084, 0.000000000000000000, -0.9984555975339683975 ) ) ;
#67412 = CARTESIAN_POINT ( 'NONE',  ( -3.313708498984760720, -25.53124999999999645, -8.000000000000000000 ) ) ;
#67413 = AXIS2_PLACEMENT_3D ( 'NONE', #100633, #34877, #66681 ) ;
#67414 =( GEOMETRIC_REPRESENTATION_CONTEXT ( 3 ) GLOBAL_UNCERTAINTY_ASSIGNED_CONTEXT ( ( #26789 ) ) GLOBAL_UNIT_ASSIGNED_CONTEXT ( ( #72703, #47884, #5842 ) ) REPRESENTATION_CONTEXT ( 'NONE', 'WORKASPACE' ) );
#67415 = CARTESIAN_POINT ( 'NONE',  ( -20.00000000000000000, 12.99999999999999289, 0.000000000000000000 ) ) ;
#67416 = ORIENTED_EDGE ( 'NONE', *, *, #71716, .F. ) ;
#67417 = CARTESIAN_POINT ( 'NONE',  ( 84.39719784251927592, -39.41516335604673316, 180.8079987764798489 ) ) ;
#67418 =( NAMED_UNIT ( * ) SI_UNIT ( $, .STERADIAN. ) SOLID_ANGLE_UNIT ( ) );
#67419 = CARTESIAN_POINT ( 'NONE',  ( 32.94021323899734455, 485.0599191339525191, 5.361609822540892800 ) ) ;
#67420 = ORIENTED_EDGE ( 'NONE', *, *, #100197, .F. ) ;
#67421 = CARTESIAN_POINT ( 'NONE',  ( 0.000000000000000000, -19.99999999999998934, 0.000000000000000000 ) ) ;
#67422 = LINE ( 'NONE', #18353, #52717 ) ;
#67423 = DIRECTION ( 'NONE',  ( 0.000000000000000000, -0.000000000000000000, 1.000000000000000000 ) ) ;
#67424 = CARTESIAN_POINT ( 'NONE',  ( 21.08349330513380693, 1.593028355512270962E-15, 0.000000000000000000 ) ) ;
#67425 = CARTESIAN_POINT ( 'NONE',  ( -9.920059540012950094, -3.000000000000003109, -96.33176891503234174 ) ) ;
#67426 = CARTESIAN_POINT ( 'NONE',  ( -23.44733519253580667, -27.12328492395885604, -38.41448460140718169 ) ) ;
#67427 = CARTESIAN_POINT ( 'NONE',  ( -8.390648120624151218, -0.1953587718301813270, 19.49430943995808008 ) ) ;
#67428 =( NAMED_UNIT ( * ) PLANE_ANGLE_UNIT ( ) SI_UNIT ( $, .RADIAN. ) );
#67429 = VECTOR ( 'NONE', #90946, 1000.000000000000000 ) ;
#67430 = CARTESIAN_POINT ( 'NONE',  ( 53.73123005835647348, -60.00000000000000711, 81.67570342333168298 ) ) ;
#67431 = CIRCLE ( 'NONE', #46785, 5.000000000000000888 ) ;
#67432 = CARTESIAN_POINT ( 'NONE',  ( 7.003653396366579464, 106.0570620555967594, -3.866846144092870752 ) ) ;
#67433 = CARTESIAN_POINT ( 'NONE',  ( 20.28983781531179531, -17.22150327053471486, 31.47367925788013210 ) ) ;
#67435 = CARTESIAN_POINT ( 'NONE',  ( -12.87067482339596758, 21.40376567796203133, -5.445097966235947773 ) ) ;
#67434 = CARTESIAN_POINT ( 'NONE',  ( -2.499999999981197707, -21.99834632368703069, -30.53960193249073640 ) ) ;
#67436 = ADVANCED_FACE ( 'NONE', ( #70992, #72053 ), #12746, .T. ) ;
#67437 = VECTOR ( 'NONE', #52296, 999.9999999999998863 ) ;
#67438 = CARTESIAN_POINT ( 'NONE',  ( -10.00005432054556742, 89.00013580137914460, 0.2621623937322776765 ) ) ;
#67439 = CARTESIAN_POINT ( 'NONE',  ( 22.20318009218133071, 295.0333587257888439, 9.975590323731541531 ) ) ;
#67440 = DIRECTION ( 'NONE',  ( 1.096832036894112098E-16, -0.000000000000000000, 1.000000000000000000 ) ) ;
#67441 = VERTEX_POINT ( 'NONE', #46195 ) ;
#67442 = CARTESIAN_POINT ( 'NONE',  ( 23.15769230769230802, 4.172000000000003261, 5.109226446042759579E-16 ) ) ;
#67443 = CARTESIAN_POINT ( 'NONE',  ( -17.49999999999995381, 48.00000000000000000, 62.61753806507839215 ) ) ;
#67444 = CARTESIAN_POINT ( 'NONE',  ( -15.95159607370372967, -2.671900693682740080, 14.76216555840736255 ) ) ;
#67445 = CARTESIAN_POINT ( 'NONE',  ( -40.62988512551102360, 465.1694420659723619, 17.16838584799783973 ) ) ;
#67446 = ADVANCED_FACE ( 'NONE', ( #30555 ), #35813, .F. ) ;
#67448 = CARTESIAN_POINT ( 'NONE',  ( 32.37152068336183675, -60.22820715367447519, -34.89893449057208130 ) ) ;
#67447 = DIRECTION ( 'NONE',  ( 0.000000000000000000, 0.000000000000000000, 1.000000000000000000 ) ) ;
#67449 = B_SPLINE_CURVE_WITH_KNOTS ( 'NONE', 3,
 ( #12755, #54261, #36560, #87204, #71002 ),
 .UNSPECIFIED., .F., .F.,
 ( 4, 1, 4 ),
 ( 0.000000000000000000, 0.003752776749732565295, 0.007505553499465130590 ),
 .UNSPECIFIED. ) ;
#67450 = ORIENTED_EDGE ( 'NONE', *, *, #58280, .F. ) ;
#67451 = CARTESIAN_POINT ( 'NONE',  ( -5.192560085536412906, -87.64305442631243181, 3.013051918867554413 ) ) ;
#67452 = CARTESIAN_POINT ( 'NONE',  ( 42.98746414932995208, 1.482358050883964840E-15, 0.000000000000000000 ) ) ;
#67453 = ORIENTED_EDGE ( 'NONE', *, *, #92182, .F. ) ;
#67454 = CARTESIAN_POINT ( 'NONE',  ( 46.00000000000000000, 459.9277931459794786, 6.461582622334601567 ) ) ;
#67455 = CARTESIAN_POINT ( 'NONE',  ( 30.87917441950755659, 8.312254468506253602, -41.23121050640295238 ) ) ;
#67456 =( LENGTH_UNIT ( ) NAMED_UNIT ( * ) SI_UNIT ( .MILLI., .METRE. ) );
#67457 = CARTESIAN_POINT ( 'NONE',  ( -103.7243948980324006, -60.00000000000000000, 102.8245780598074077 ) ) ;
#67458 = DIRECTION ( 'NONE',  ( -0.8902151594054030781, 0.000000000000000000, 0.4555403055326856521 ) ) ;
#67459 = FACE_OUTER_BOUND ( 'NONE', #79692, .T. ) ;
#67460 = DIRECTION ( 'NONE',  ( 0.5735764363510466035, -0.8191520442889914655, 1.003171929053524500E-16 ) ) ;
#67461 = CARTESIAN_POINT ( 'NONE',  ( 40.54048956546203897, 460.8805895396365031, 2.213361020664811996 ) ) ;
#67463 = SURFACE_STYLE_FILL_AREA ( #11860 ) ;
#67462 = CARTESIAN_POINT ( 'NONE',  ( -33.92709525147871830, 435.0559456452657514, 11.89085117398056113 ) ) ;
#67464 = EDGE_CURVE ( 'NONE', #23419, #43519, #25501, .T. ) ;
#67465 = CARTESIAN_POINT ( 'NONE',  ( -85.49467086792562043, -21.96977942738778822, 166.0364208305039426 ) ) ;
#67466 = ORIENTED_EDGE ( 'NONE', *, *, #48504, .F. ) ;
#67467 = CIRCLE ( 'NONE', #100178, 5.000000000000011546 ) ;
#67468 = ORIENTED_EDGE ( 'NONE', *, *, #84026, .T. ) ;
#67469 = ORIENTED_EDGE ( 'NONE', *, *, #101045, .T. ) ;
#67470 = FACE_OUTER_BOUND ( 'NONE', #77470, .T. ) ;
#67471 = ADVANCED_FACE ( 'NONE', ( #62389 ), #20914, .T. ) ;
#67472 = ORIENTED_EDGE ( 'NONE', *, *, #90865, .T. ) ;
#67473 = CARTESIAN_POINT ( 'NONE',  ( -72.61817094705909881, -45.32535816143199270, -22.56079433717181715 ) ) ;
#67474 = CARTESIAN_POINT ( 'NONE',  ( 4.000000000000000000, 4.898587196589412829E-16, -3.432199999999999918 ) ) ;
#67475 = DIRECTION ( 'NONE',  ( 1.000000000000000000, 0.000000000000000000, 0.000000000000000000 ) ) ;
#67476 = CARTESIAN_POINT ( 'NONE',  ( -1.793778237424737965, 14.26790010547893495, 6.770782475500216613 ) ) ;
#67477 = CARTESIAN_POINT ( 'NONE',  ( 35.11650669486618170, 4.898587196589411843E-16, -4.000000000000000888 ) ) ;
#67478 =( NAMED_UNIT ( * ) SI_UNIT ( $, .STERADIAN. ) SOLID_ANGLE_UNIT ( ) );
#67479 = DIRECTION ( 'NONE',  ( 1.150791560227848051E-16, -0.3420201433256733758, 0.9396926207859066515 ) ) ;
#67480 = MECHANICAL_DESIGN_GEOMETRIC_PRESENTATION_REPRESENTATION (  '', ( #72616 ), #58936 ) ;
#67481 = CARTESIAN_POINT ( 'NONE',  ( 89.32114860119857269, -29.99999999999995026, 17.89867789164953393 ) ) ;
#67482 = CARTESIAN_POINT ( 'NONE',  ( -106.7759996721837297, -60.00000000000014211, 200.9056163170290858 ) ) ;
#67483 = CARTESIAN_POINT ( 'NONE',  ( -57.95451485573907746, -29.07822120235440622, 62.48206156589100857 ) ) ;
#67484 = VERTEX_POINT ( 'NONE', #31102 ) ;
#67485 = CARTESIAN_POINT ( 'NONE',  ( 47.44000135571184273, -60.00000000002890488, -40.81002596378207414 ) ) ;
#67486 = ORIENTED_EDGE ( 'NONE', *, *, #48128, .T. ) ;
#67487 = CARTESIAN_POINT ( 'NONE',  ( 7.205507455416617191, -49.91572346798661641, 32.19931394973104233 ) ) ;
#67488 = CARTESIAN_POINT ( 'NONE',  ( -106.2891245437193675, -60.15515527080706448, 179.7497780154444058 ) ) ;
#67489 =( NAMED_UNIT ( * ) PLANE_ANGLE_UNIT ( ) SI_UNIT ( $, .RADIAN. ) );
#67490 = FACE_OUTER_BOUND ( 'NONE', #72631, .T. ) ;
#67491 = DIRECTION ( 'NONE',  ( -0.000000000000000000, -1.000000000000000000, -0.000000000000000000 ) ) ;
#67492 = ORIENTED_EDGE ( 'NONE', *, *, #54343, .T. ) ;
#67493 = CARTESIAN_POINT ( 'NONE',  ( 19.49642740850473999, 49.99975891507487091, 59.99140731955566963 ) ) ;
#67494 = EDGE_CURVE ( 'NONE', #4517, #104615, #104412, .T. ) ;
#67495 = CARTESIAN_POINT ( 'NONE',  ( -79.40048706246868448, -60.00000000000001421, 195.2207880595982772 ) ) ;
#67496 = CARTESIAN_POINT ( 'NONE',  ( 36.62728554792472124, 26.04043489851655480, -11.37739872878407255 ) ) ;
#67497 = CARTESIAN_POINT ( 'NONE',  ( -2.977408999572650039, -23.56250000204839168, -7.188101187500001821 ) ) ;
#67498 = LINE ( 'NONE', #77176, #20736 ) ;
#67499 = CARTESIAN_POINT ( 'NONE',  ( 13.52487676486885348, 0.000000000000000000, 10.38441970551129501 ) ) ;
#67500 = CARTESIAN_POINT ( 'NONE',  ( -11.47300386045560749, -4.941189186712652059, -12.56866361833190915 ) ) ;
#67501 = CARTESIAN_POINT ( 'NONE',  ( 0.000000000000000000, 0.000000000000000000, 4.000000000000000000 ) ) ;
#67502 = CARTESIAN_POINT ( 'NONE',  ( 9.778942110939100374, -12.74542388620636757, 16.96968632615047667 ) ) ;
#67503 = SURFACE_STYLE_USAGE ( .BOTH. , #34636 ) ;
#67504 = CARTESIAN_POINT ( 'NONE',  ( -5.243676916559595114, 9.267627703000917094, -29.53296413887904848 ) ) ;
#67505 = UNCERTAINTY_MEASURE_WITH_UNIT (LENGTH_MEASURE( 1.000000000000000082E-05 ), #27572, 'distance_accuracy_value', 'NONE');
#67506 = CARTESIAN_POINT ( 'NONE',  ( -30.53886170152374291, -18.65827435953780977, 29.53940708261786341 ) ) ;
#67507 = AXIS2_PLACEMENT_3D ( 'NONE', #39367, #57107, #97562 ) ;
#67508 = CARTESIAN_POINT ( 'NONE',  ( 44.33516561222944574, -60.24910389432578484, 48.28984989065179434 ) ) ;
#67509 = CIRCLE ( 'NONE', #41702, 14.00000000000000178 ) ;
#67510 = CARTESIAN_POINT ( 'NONE',  ( 0.000000000000000000, 45.00000000000000711, 59.50000000000000000 ) ) ;
#67511 = ORIENTED_EDGE ( 'NONE', *, *, #63103, .T. ) ;
#67512 = CARTESIAN_POINT ( 'NONE',  ( -7.551437640244098581, 88.00872462522912087, -2.648272645923386293 ) ) ;
#67513 = VECTOR ( 'NONE', #35375, 1000.000000000000000 ) ;
#67514 = CARTESIAN_POINT ( 'NONE',  ( -81.68379548809339497, -38.84189794985886124, 195.5063719952446775 ) ) ;
#67515 = VERTEX_POINT ( 'NONE', #13270 ) ;
#67517 = CARTESIAN_POINT ( 'NONE',  ( 40.85254446136673323, 441.7500193615117610, 25.53625856138344474 ) ) ;
#67516 = FACE_OUTER_BOUND ( 'NONE', #47070, .T. ) ;
#67518 = CARTESIAN_POINT ( 'NONE',  ( 34.59539548351714444, -59.99999999999999289, 38.98399512715914028 ) ) ;
#67519 = FACE_OUTER_BOUND ( 'NONE', #8524, .T. ) ;
#67520 = CARTESIAN_POINT ( 'NONE',  ( -7.081808430652881903, 41.46696591259760112, -58.88886595218312436 ) ) ;
#67521 = FACE_OUTER_BOUND ( 'NONE', #98355, .T. ) ;
#67522 = DIRECTION ( 'NONE',  ( -0.000000000000000000, -1.000000000000000000, -0.000000000000000000 ) ) ;
#67523 = CARTESIAN_POINT ( 'NONE',  ( -23.21474708200883796, 305.7582702134220085, 9.134669239329348045 ) ) ;
#67524 = CARTESIAN_POINT ( 'NONE',  ( 6.928203230275508773, -85.00000000000000000, 4.000000000000001776 ) ) ;
#67525 = CARTESIAN_POINT ( 'NONE',  ( 106.3113036129748821, -60.00000000000000711, 118.3450711846818422 ) ) ;
#67526 = DIRECTION ( 'NONE',  ( 0.5000000000000006661, -0.8660254037844382635, 0.000000000000000000 ) ) ;
#67527 = ADVANCED_FACE ( 'NONE', ( #87192 ), #9972, .T. ) ;
#67528 =( BOUNDED_SURFACE ( )  B_SPLINE_SURFACE ( 3, 3, ( 
 ( #88157, #14240, #104868, #80040 ),
 ( #31011, #33643, #56280, #23443 ),
 ( #90270, #81103, #90809, #42236 ),
 ( #66524, #57884, #97821, #23984 ) ),
 .UNSPECIFIED., .F., .F., .F. ) 
 B_SPLINE_SURFACE_WITH_KNOTS ( ( 4, 4 ),
 ( 4, 4 ),
 ( 0.000000000000000000, 1.000000000000000000 ),
 ( 0.000000000000000000, 1.000000000000000000 ),
 .UNSPECIFIED. ) 
 GEOMETRIC_REPRESENTATION_ITEM ( )  RATIONAL_B_SPLINE_SURFACE ( (
 ( 1.000000000000000000, 0.3333333333333334259, 0.3333333333333334259, 1.000000000000000000),
 ( 1.000000000000000000, 0.3333333333333334259, 0.3333333333333334259, 1.000000000000000000),
 ( 1.000000000000000000, 0.3333333333333334259, 0.3333333333333334259, 1.000000000000000000),
 ( 1.000000000000000000, 0.3333333333333334259, 0.3333333333333334259, 1.000000000000000000) ) ) 
 REPRESENTATION_ITEM ( '' )  SURFACE ( )  );
#67529 = CARTESIAN_POINT ( 'NONE',  ( 13.69330508143927538, 6.123233995736770227E-16, -5.000000000000002665 ) ) ;
#67530 = ORIENTED_EDGE ( 'NONE', *, *, #61234, .T. ) ;
#67531 = EDGE_CURVE ( 'NONE', #35344, #40074, #70270, .T. ) ;
#67532 = CARTESIAN_POINT ( 'NONE',  ( 1.993516955649288214, -49.88337200126083815, 102.1895970170251644 ) ) ;
#67533 = CARTESIAN_POINT ( 'NONE',  ( -97.95549896524885014, -29.99999999999989342, 190.5752664689312894 ) ) ;
#67534 = EDGE_LOOP ( 'NONE', ( #215, #103926, #82184, #9517 ) ) ;
#67535 = CARTESIAN_POINT ( 'NONE',  ( 26.35426118683261620, 36.89205985873699944, -9.819161256584076014 ) ) ;
#67536 = CARTESIAN_POINT ( 'NONE',  ( 43.27198366478697267, 461.7520071969412925, 3.865882560854753347 ) ) ;
#67537 = CARTESIAN_POINT ( 'NONE',  ( 26.98763868050856729, 309.1593988222194866, 11.18671119439325956 ) ) ;
#67538 = LINE ( 'NONE', #100418, #104043 ) ;
#67539 = CARTESIAN_POINT ( 'NONE',  ( 7.188101187500000044, -19.53125000204838457, 0.000000000000000000 ) ) ;
#67541 = EDGE_CURVE ( 'NONE', #54844, #99696, #88248, .T. ) ;
#67540 = CARTESIAN_POINT ( 'NONE',  ( -9.596002107492989097, -5.000000000000002665, -77.62543935900905012 ) ) ;
#67542 = UNCERTAINTY_MEASURE_WITH_UNIT (LENGTH_MEASURE( 1.000000000000000082E-05 ), #6910, 'distance_accuracy_value', 'NONE');
#67543 = CARTESIAN_POINT ( 'NONE',  ( 0.000000000000000000, 2.999999999999993339, 0.000000000000000000 ) ) ;
#67545 = VERTEX_POINT ( 'NONE', #39172 ) ;
#67544 = FACE_OUTER_BOUND ( 'NONE', #68646, .T. ) ;
#67546 = CARTESIAN_POINT ( 'NONE',  ( 80.67535997844298379, -49.91147864860721484, 164.5085625698619936 ) ) ;
#67547 = CARTESIAN_POINT ( 'NONE',  ( -46.00000000000000000, 460.8575856737582512, 7.929402417978877793 ) ) ;
#67548 = VERTEX_POINT ( 'NONE', #56908 ) ;
#67549 = AXIS2_PLACEMENT_3D ( 'NONE', #69936, #18760, #84530 ) ;
#67550 = CARTESIAN_POINT ( 'NONE',  ( 11.36650669486618881, -3.999999999999998224, 0.000000000000000000 ) ) ;
#67551 = CARTESIAN_POINT ( 'NONE',  ( -4.852941176470586093, 40.00000000000132871, -70.80672828634229177 ) ) ;
#67552 = CARTESIAN_POINT ( 'NONE',  ( -2.977408999572650039, -9.687500002048384573, -7.188101187500000933 ) ) ;
#67553 = CARTESIAN_POINT ( 'NONE',  ( 30.00000000000000355, 488.7759232733317845, 4.253593570494768272 ) ) ;
#67554 = MECHANICAL_DESIGN_GEOMETRIC_PRESENTATION_REPRESENTATION (  '', ( #86516 ), #420 ) ;
#67555 = SURFACE_STYLE_USAGE ( .BOTH. , #10355 ) ;
#67556 = CARTESIAN_POINT ( 'NONE',  ( -33.16832880629362279, 391.4582360920214796, 25.60486106200601952 ) ) ;
#67557 = CARTESIAN_POINT ( 'NONE',  ( -32.48507062769438392, 435.0120188477415581, 18.09005837372713899 ) ) ;
#67558 = EDGE_LOOP ( 'NONE', ( #51248, #65241, #5502, #42848, #104944, #4029 ) ) ;
#67559 = FILL_AREA_STYLE_COLOUR ( '', #59189 ) ;
#67561 = DIRECTION ( 'NONE',  ( -1.000000000000000000, -1.224606353822377258E-16, -0.000000000000000000 ) ) ;
#67560 = STYLED_ITEM ( 'NONE', ( #39661 ), #20554 ) ;
#67562 = CARTESIAN_POINT ( 'NONE',  ( 28.08715220166955007, 18.64284798592788306, 26.23039857546442732 ) ) ;
#67563 = CARTESIAN_POINT ( 'NONE',  ( 87.26958111220818637, -50.07308097134770719, 192.1704676255311881 ) ) ;
#67564 = CONICAL_SURFACE ( 'NONE', #282, 9.000000000000000000, 0.7853981633974509435 ) ;
#67565 = CARTESIAN_POINT ( 'NONE',  ( 1.093552547293052069, 34.39704201091980451, -29.11089208678710705 ) ) ;
#67566 = EDGE_CURVE ( 'NONE', #23677, #13857, #37598, .T. ) ;
#67567 = CARTESIAN_POINT ( 'NONE',  ( 2.977408999572650927, -27.87500000204838457, -7.188101187500001821 ) ) ;
#67568 = CARTESIAN_POINT ( 'NONE',  ( -31.96161004470367928, 465.6201165449651285, 10.43791023679821883 ) ) ;
#67569 = CARTESIAN_POINT ( 'NONE',  ( 7.578119713073430574, 51.95084648887009848, 3.571665354261504888 ) ) ;
#67570 = ADVANCED_FACE ( 'NONE', ( #65551 ), #77915, .F. ) ;
#67571 = CARTESIAN_POINT ( 'NONE',  ( 31.08349330513380693, 1.593028355512270962E-15, 0.000000000000000000 ) ) ;
#67572 = EDGE_LOOP ( 'NONE', ( #10998, #81441, #59352, #80297, #63402, #41451 ) ) ;
#67573 = CARTESIAN_POINT ( 'NONE',  ( -35.07439070119946933, 437.8544070495365759, 4.397851634058751458 ) ) ;
#67574 =( NAMED_UNIT ( * ) SI_UNIT ( $, .STERADIAN. ) SOLID_ANGLE_UNIT ( ) );
#67575 = CARTESIAN_POINT ( 'NONE',  ( -9.995757844555885896, 7.506119843332723640, 0.000000000000000000 ) ) ;
#67576 = EDGE_CURVE ( 'NONE', #91282, #91423, #81865, .T. ) ;
#67577 = DIRECTION ( 'NONE',  ( -0.000000000000000000, 1.000000000000000000, -0.000000000000000000 ) ) ;
#67578 = AXIS2_PLACEMENT_3D ( 'NONE', #80727, #56446, #105027 ) ;
#67579 = ORIENTED_EDGE ( 'NONE', *, *, #43802, .T. ) ;
#67580 = DIRECTION ( 'NONE',  ( 0.000000000000000000, 1.000000000000000000, -0.000000000000000000 ) ) ;
#67581 = CYLINDRICAL_SURFACE ( 'NONE', #72023, 1.250000000000000222 ) ;
#67582 = AXIS2_PLACEMENT_3D ( 'NONE', #66437, #17379, #26039 ) ;
#67583 = CARTESIAN_POINT ( 'NONE',  ( 32.39555719572166481, 435.1515357145120220, 14.91598548009360670 ) ) ;
#67584 = CIRCLE ( 'NONE', #53783, 4.000000000000007105 ) ;
#67585 = B_SPLINE_CURVE_WITH_KNOTS ( 'NONE', 3,
 ( #92582, #106217, #32381, #65253, #59171, #92052, #18736, #18185, #98143, #26833, #10593, #57144, #67264, #100142, #51044, #42981, #10069, #28973, #37583, #77999, #79059, #5179 ),
 .UNSPECIFIED., .F., .F.,
 ( 4, 2, 2, 2, 2, 2, 2, 2, 2, 2, 4 ),
 ( 0.003005601947361117611, 0.003258126653066766108, 0.003510651358772414604, 0.003763176064478062667, 0.004015700770183711597, 0.004520750181594991243, 0.005025799593006271757, 0.005530849004417552270, 0.006035898415828832783, 0.006540947827240112429, 0.007045997238651392942 ),
 .UNSPECIFIED. ) ;
#67586 = DIRECTION ( 'NONE',  ( 0.5735764363510490460, 0.8191520442889896891, 0.000000000000000000 ) ) ;
#67587 = CARTESIAN_POINT ( 'NONE',  ( 16.83213728180786362, 302.5742751247036040, 9.878299632764496963 ) ) ;
#67588 = CARTESIAN_POINT ( 'NONE',  ( -79.77917837913028620, -60.00000000000000711, 195.7066188485981399 ) ) ;
#67590 = AXIS2_PLACEMENT_3D ( 'NONE', #80629, #15373, #41243 ) ;
#67589 = CARTESIAN_POINT ( 'NONE',  ( -7.500000000000006217, 39.99999999999122480, -59.88032989330939415 ) ) ;
#67591 = CYLINDRICAL_SURFACE ( 'NONE', #87328, 4.000000000000000888 ) ;
#67592 = CARTESIAN_POINT ( 'NONE',  ( -84.32939227294266971, -46.57010899852983243, 185.7296267468632607 ) ) ;
#67593 = ORIENTED_EDGE ( 'NONE', *, *, #103917, .F. ) ;
#67594 =( LENGTH_UNIT ( ) NAMED_UNIT ( * ) SI_UNIT ( .MILLI., .METRE. ) );
#67595 = VERTEX_POINT ( 'NONE', #42329 ) ;
#67596 = CARTESIAN_POINT ( 'NONE',  ( 95.42421628608209971, -5.000000000000000000, 6.123233995736778115E-16 ) ) ;
#67597 = EDGE_CURVE ( 'NONE', #76425, #106028, #60159, .T. ) ;
#67598 = CARTESIAN_POINT ( 'NONE',  ( 3.718188220751057926, -1.049015004457080957, 104.2423402216923733 ) ) ;
#67599 = CARTESIAN_POINT ( 'NONE',  ( -85.16386424983127768, -52.70345752972548325, 3.865554627149779154 ) ) ;
#67600 = FACE_OUTER_BOUND ( 'NONE', #4086, .T. ) ;
#67601 = CARTESIAN_POINT ( 'NONE',  ( -30.00000000000000000, 461.8163627757383551, 11.11111419091028729 ) ) ;
#67602 = CARTESIAN_POINT ( 'NONE',  ( -14.31840793639504383, -7.983782706452587696, 12.70197556375779513 ) ) ;
#67603 = CARTESIAN_POINT ( 'NONE',  ( -6.125000000000002665, -15.62228920881133654, 14.41094225130411211 ) ) ;
#67604 = CARTESIAN_POINT ( 'NONE',  ( 79.13121736040859844, 42.00000000000000000, -45.60838156035022450 ) ) ;
#67605 = DIRECTION ( 'NONE',  ( 0.000000000000000000, -1.000000000000000000, 0.000000000000000000 ) ) ;
#67606 = CARTESIAN_POINT ( 'NONE',  ( 58.28796150060976089, -14.21045842199433729, 78.47796032183087789 ) ) ;
#67607 = CARTESIAN_POINT ( 'NONE',  ( -36.28420329444977455, 437.5777248398061374, 4.256696328374294680 ) ) ;
#67608 = CARTESIAN_POINT ( 'NONE',  ( -85.44375122223560481, -14.21045842199445630, -16.44937377337592466 ) ) ;
#67609 = CARTESIAN_POINT ( 'NONE',  ( -68.69079975540086025, -18.63268183060117877, 85.99216174777282617 ) ) ;
#67610 = EDGE_LOOP ( 'NONE', ( #32733, #14180, #62436, #67885 ) ) ;
#67611 = CARTESIAN_POINT ( 'NONE',  ( 69.85392978727392688, -60.00000000000004263, 155.8703566448706113 ) ) ;
#67612 = CARTESIAN_POINT ( 'NONE',  ( -5.921510830615929422, 40.83857583775533584, 64.79874045254685200 ) ) ;
#67613 = CARTESIAN_POINT ( 'NONE',  ( 44.68316001078914468, -60.00000000001960387, 65.34536827560972938 ) ) ;
#67614 = EDGE_CURVE ( 'NONE', #105135, #16697, #8207, .T. ) ;
#67615 = ORIENTED_EDGE ( 'NONE', *, *, #82333, .T. ) ;
#67616 = CARTESIAN_POINT ( 'NONE',  ( 7.306651344440208362, 52.17319877359566505, -2.637493225739738101 ) ) ;
#67617 = CARTESIAN_POINT ( 'NONE',  ( 5.082755093536324154, -22.71875000204838457, 5.082755093536326818 ) ) ;
#67618 = AXIS2_PLACEMENT_3D ( 'NONE', #105920, #23999, #7228 ) ;
#67619 = CARTESIAN_POINT ( 'NONE',  ( -0.6458819410170080211, 27.35549314424027756, -40.58326240071404811 ) ) ;
#67620 = VERTEX_POINT ( 'NONE', #60672 ) ;
#67621 = CARTESIAN_POINT ( 'NONE',  ( 0.000000000000000000, 0.000000000000000000, -1.446714285714285841 ) ) ;
#67622 = CARTESIAN_POINT ( 'NONE',  ( 1.432382586635896571, 14.11565467677096564, -6.853004900836180191 ) ) ;
#67623 = CARTESIAN_POINT ( 'NONE',  ( 47.44867487729116817, 16.35164899989712239, -16.71951642917279202 ) ) ;
#67624 = CARTESIAN_POINT ( 'NONE',  ( 30.07110509900797268, 309.7455132721622135, -8.642324552508243940 ) ) ;
#67625 = CARTESIAN_POINT ( 'NONE',  ( 5.082755093536325930, -14.46875000204838457, -5.082755093536325042 ) ) ;
#67626 = CARTESIAN_POINT ( 'NONE',  ( -49.26579422795270347, 13.23794831108498649, 15.39367580924676560 ) ) ;
#67627 = CIRCLE ( 'NONE', #53827, 11.00000000000001066 ) ;
#67628 = CARTESIAN_POINT ( 'NONE',  ( 3.301565691951519721, -4.285714285714296246, -25.05982991920904723 ) ) ;
#67629 = CYLINDRICAL_SURFACE ( 'NONE', #35766, 1.249999999999999334 ) ;
#67630 = CARTESIAN_POINT ( 'NONE',  ( -9.999999999999989342, 49.99999999999999289, -83.69100306251235111 ) ) ;
#67631 = CYLINDRICAL_SURFACE ( 'NONE', #49017, 4.000000000000000888 ) ;
#67632 = DIRECTION ( 'NONE',  ( -1.000000000000000000, -1.224606353822377258E-16, -0.000000000000000000 ) ) ;
#67633 = CONICAL_SURFACE ( 'NONE', #95196, 5.000000000000010658, 0.9599310885968697082 ) ;
#67634 = ORIENTED_EDGE ( 'NONE', *, *, #78576, .T. ) ;
#67635 = CARTESIAN_POINT ( 'NONE',  ( -7.316989450287470831, 41.06054039135568701, -70.27554050036877697 ) ) ;
#67636 = PRESENTATION_LAYER_ASSIGNMENT (  '', '', ( #7314 ) ) ;
#67637 = CARTESIAN_POINT ( 'NONE',  ( 30.53703330449200237, -18.65834619125411109, 29.53878724365041464 ) ) ;
#67638 = CARTESIAN_POINT ( 'NONE',  ( -4.036265570123655166, 52.01079393774872983, -7.152884558231209056 ) ) ;
#67639 = VERTEX_POINT ( 'NONE', #93015 ) ;
#67640 = CARTESIAN_POINT ( 'NONE',  ( -3.312116827214752676E-14, 12.91535575336970965, 51.75000000000017764 ) ) ;
#67641 = ORIENTED_EDGE ( 'NONE', *, *, #46788, .T. ) ;
#67643 = CARTESIAN_POINT ( 'NONE',  ( -6.318250223874061420E-16, 9.147862274876551680, -8.047472243342934206 ) ) ;
#67642 = FACE_OUTER_BOUND ( 'NONE', #89488, .T. ) ;
#67644 = DIRECTION ( 'NONE',  ( 0.000000000000000000, 0.000000000000000000, -1.000000000000000000 ) ) ;
#67645 = CARTESIAN_POINT ( 'NONE',  ( -33.52832263806441659, 435.4519723258069348, 9.506607217394984488 ) ) ;
#67646 = DIRECTION ( 'NONE',  ( 0.000000000000000000, 0.000000000000000000, 1.000000000000000000 ) ) ;
#67647 = CARTESIAN_POINT ( 'NONE',  ( -37.54559764570110048, 464.1143081516183884, 19.43664670202764100 ) ) ;
#67648 = EDGE_LOOP ( 'NONE', ( #39793, #28102, #102763, #42113, #44621, #22052 ) ) ;
#67649 = CARTESIAN_POINT ( 'NONE',  ( 81.12437216259647244, -59.99999999999999289, -27.26058583151750270 ) ) ;
#67650 = FACE_OUTER_BOUND ( 'NONE', #46148, .T. ) ;
#67651 =( NAMED_UNIT ( * ) PLANE_ANGLE_UNIT ( ) SI_UNIT ( $, .RADIAN. ) );
#67652 = CARTESIAN_POINT ( 'NONE',  ( -7.922281120364393914, 4.573931137438267847, -8.047472243342932430 ) ) ;
#67653 = FACE_BOUND ( 'NONE', #88518, .T. ) ;
#67654 = VERTEX_POINT ( 'NONE', #101645 ) ;
#67655 = EDGE_CURVE ( 'NONE', #14445, #36519, #85762, .T. ) ;
#67656 = DIRECTION ( 'NONE',  ( -1.000000000000000000, -0.000000000000000000, 0.000000000000000000 ) ) ;
#67657 = ORIENTED_EDGE ( 'NONE', *, *, #50054, .F. ) ;
#67658 = EDGE_LOOP ( 'NONE', ( #89593, #22162 ) ) ;
#67659 = CARTESIAN_POINT ( 'NONE',  ( 6.928203230275506996, 84.73069070304462969, -4.000000000000000888 ) ) ;
#67660 = CARTESIAN_POINT ( 'NONE',  ( 12.33349330513380337, 1.593028355512270567E-15, 0.000000000000000000 ) ) ;
#67661 = CARTESIAN_POINT ( 'NONE',  ( 85.85151669601329161, -60.21672556079247585, -14.42664014460055988 ) ) ;
#67662 = CARTESIAN_POINT ( 'NONE',  ( -37.41669077972581192, 304.6406083910922007, -7.749892281362566138 ) ) ;
#67663 = CARTESIAN_POINT ( 'NONE',  ( -11.86976244332121233, 303.5920063884646538, -10.05522024194447539 ) ) ;
#67665 = ADVANCED_FACE ( 'NONE', ( #1316 ), #34278, .F. ) ;
#67664 = FILL_AREA_STYLE_COLOUR ( '', #74304 ) ;
#67666 = ORIENTED_EDGE ( 'NONE', *, *, #95044, .F. ) ;
#67667 = DIRECTION ( 'NONE',  ( -1.000000000000000000, 0.000000000000000000, 0.000000000000000000 ) ) ;
#67668 = ORIENTED_EDGE ( 'NONE', *, *, #47973, .T. ) ;
#67669 = CARTESIAN_POINT ( 'NONE',  ( 8.559508646656349029, 51.83514083332403999, -1.531152949374623873 ) ) ;
#67670 = CARTESIAN_POINT ( 'NONE',  ( -8.559508646656370345, -1.200000000000000030E-05, 2.781152949374564365 ) ) ;
#67672 = ORIENTED_EDGE ( 'NONE', *, *, #5986, .T. ) ;
#67671 = CARTESIAN_POINT ( 'NONE',  ( 5.383907448094620740, 41.54392475608550939, -58.58678525159944428 ) ) ;
#67673 = CARTESIAN_POINT ( 'NONE',  ( 72.21471659750817196, -22.11717074490460178, 98.80210365957880470 ) ) ;
#67674 = ORIENTED_EDGE ( 'NONE', *, *, #17342, .T. ) ;
#67675 = CARTESIAN_POINT ( 'NONE',  ( 4.585277158900029626, -47.79285414227015139, 43.04040780539905597 ) ) ;
#67676 = CARTESIAN_POINT ( 'NONE',  ( 82.42421628608209971, 1.030564683017419500E-14, 0.000000000000000000 ) ) ;
#67677 = CARTESIAN_POINT ( 'NONE',  ( -7.188101187500002709, -27.31250000204838457, 2.977408999572647819 ) ) ;
#67678 = CARTESIAN_POINT ( 'NONE',  ( -92.76317396897962908, -57.65703681568646743, -17.81073576277876569 ) ) ;
#67679 = EDGE_CURVE ( 'NONE', #96995, #68089, #67769, .T. ) ;
#67680 = VERTEX_POINT ( 'NONE', #19707 ) ;
#67681 = FILL_AREA_STYLE_COLOUR ( '', #76328 ) ;
#67682 = CARTESIAN_POINT ( 'NONE',  ( 4.000000000000000888, 0.000000000000000000, 3.469446951953614189E-15 ) ) ;
#67683 = CARTESIAN_POINT ( 'NONE',  ( 103.1592532910830471, -45.28273945504021469, 184.6164784094243032 ) ) ;
#67684 = CARTESIAN_POINT ( 'NONE',  ( -36.31544203073882215, 28.19121493635761766, -12.14374965612692669 ) ) ;
#67685 = DIRECTION ( 'NONE',  ( 0.000000000000000000, -1.000000000000000000, 0.000000000000000000 ) ) ;
#67686 = ADVANCED_FACE ( 'NONE', ( #44475 ), #34818, .T. ) ;
#67687 = CARTESIAN_POINT ( 'NONE',  ( 3.313708498984762052, -21.40625000409677270, -8.000000000000000000 ) ) ;
#67688 = CARTESIAN_POINT ( 'NONE',  ( -17.49999999999999645, -2.499999999999999556, 25.00000000000000000 ) ) ;
#67689 = CARTESIAN_POINT ( 'NONE',  ( -36.64357978206631117, 25.84195196822051344, 13.05277382008214282 ) ) ;
#67690 = CIRCLE ( 'NONE', #103865, 4.999999999999993783 ) ;
#67691 = CARTESIAN_POINT ( 'NONE',  ( 46.84999999999999432, 1.533819458162526451E-15, 0.000000000000000000 ) ) ;
#67692 = CARTESIAN_POINT ( 'NONE',  ( 5.367391215540106231, 43.24496486319787181, -60.11082976391321608 ) ) ;
#67693 = CARTESIAN_POINT ( 'NONE',  ( -10.28624191511829977, 46.12099395432375104, -12.90779740156156841 ) ) ;
#67694 = AXIS2_PLACEMENT_3D ( 'NONE', #100179, #18776, #66759 ) ;
#67695 = DIRECTION ( 'NONE',  ( -1.894296555319105934E-20, 0.4412131870756565988, 0.8974023197822377229 ) ) ;
#67696 = CARTESIAN_POINT ( 'NONE',  ( -4.397168787612410590, 15.00000000000000000, -9.999999999999998224 ) ) ;
#67697 = EDGE_LOOP ( 'NONE', ( #68479, #73052 ) ) ;
#67698 = CARTESIAN_POINT ( 'NONE',  ( 32.85155332502863956, 463.8111683108725174, 7.359358840565810134 ) ) ;
#67699 = DIRECTION ( 'NONE',  ( -1.000000000000000000, -0.000000000000000000, -0.000000000000000000 ) ) ;
#67700 = PRESENTATION_LAYER_ASSIGNMENT (  '', '', ( #22989 ) ) ;
#67701 = CARTESIAN_POINT ( 'NONE',  ( -7.000000000000000000, 8.572527594031473190E-16, -4.425378966781146950 ) ) ;
#67702 = CARTESIAN_POINT ( 'NONE',  ( -85.49926595847192345, -30.00000000000000000, 174.8177305309835674 ) ) ;
#67703 = EDGE_CURVE ( 'NONE', #15011, #54845, #17724, .T. ) ;
#67704 = ORIENTED_EDGE ( 'NONE', *, *, #83537, .F. ) ;
#67705 = CARTESIAN_POINT ( 'NONE',  ( 38.33084065836750653, 25.24363705771616750, -13.20929050494120993 ) ) ;
#67706 = AXIS2_PLACEMENT_3D ( 'NONE', #95381, #38749, #103469 ) ;
#67707 = CARTESIAN_POINT ( 'NONE',  ( 71.51784493620726835, -57.67947522968200502, 167.2032557688225154 ) ) ;
#67709 = CARTESIAN_POINT ( 'NONE',  ( 44.83349330513380693, 1.593028355512270567E-15, 0.000000000000000000 ) ) ;
#67708 = FACE_OUTER_BOUND ( 'NONE', #67013, .T. ) ;
#67710 = CARTESIAN_POINT ( 'NONE',  ( 47.36551243866970395, -34.95418281838176711, -36.56030574305207637 ) ) ;
#67711 =( NAMED_UNIT ( * ) PLANE_ANGLE_UNIT ( ) SI_UNIT ( $, .RADIAN. ) );
#67712 = CARTESIAN_POINT ( 'NONE',  ( -48.61603543328580912, -60.00000000000000711, 68.43586388735928949 ) ) ;
#67713 = SURFACE_SIDE_STYLE ('',( #68242 ) ) ;
#67714 = CARTESIAN_POINT ( 'NONE',  ( -86.83128596798019316, -35.43248611210681531, 187.7796440410022853 ) ) ;
#67715 = ORIENTED_EDGE ( 'NONE', *, *, #48504, .T. ) ;
#67716 = DIRECTION ( 'NONE',  ( 0.000000000000000000, -1.000000000000000000, 0.000000000000000000 ) ) ;
#67717 = CARTESIAN_POINT ( 'NONE',  ( -3.081151406350138178, -56.88415668120669721, 33.36504120651643746 ) ) ;
#67718 = CARTESIAN_POINT ( 'NONE',  ( -6.676660803729373761, 41.76849044449239301, -59.12256534660619423 ) ) ;
#67719 = CARTESIAN_POINT ( 'NONE',  ( -1.560773912800800467, -49.96204304796045648, 101.5963399667048748 ) ) ;
#67721 = CARTESIAN_POINT ( 'NONE',  ( 2.538204850144155866, -70.38324806241240594, 13.23000886114773422 ) ) ;
#67720 = CARTESIAN_POINT ( 'NONE',  ( -41.66331289688267958, 334.8661377240072738, 11.59565765669084847 ) ) ;
#67722 = ADVANCED_FACE ( 'NONE', ( #102702 ), #92873, .T. ) ;
#67723 = ORIENTED_EDGE ( 'NONE', *, *, #106332, .T. ) ;
#67724 = CARTESIAN_POINT ( 'NONE',  ( 1.249391989912810752, 27.86128073807352834, 39.17855071985294302 ) ) ;
#67725 = DIRECTION ( 'NONE',  ( 0.9745656835855589506, 0.000000000000000000, 0.2241020490254661268 ) ) ;
#67726 = COLOUR_RGB ( '', 0.08235294, 0.09019608, 0.10196078) ;
#67727 = CARTESIAN_POINT ( 'NONE',  ( 17.50000000000002842, 50.00000000000000000, 63.82142195508322402 ) ) ;
#67728 = CARTESIAN_POINT ( 'NONE',  ( 41.58649125062324003, 315.0454808444952732, -5.157136739128146630 ) ) ;
#67729 = EDGE_CURVE ( 'NONE', #56748, #49838, #7011, .T. ) ;
#67730 = DIRECTION ( 'NONE',  ( 0.000000000000000000, 1.000000000000000000, 0.000000000000000000 ) ) ;
#67731 = DIRECTION ( 'NONE',  ( 1.000000000000000000, 1.224606353822377258E-16, 0.000000000000000000 ) ) ;
#67732 = CARTESIAN_POINT ( 'NONE',  ( 106.2140667560022536, -14.21045842199435860, 184.2067176257025380 ) ) ;
#67733 = CARTESIAN_POINT ( 'NONE',  ( -80.49898587717534326, -42.97031838899095391, 153.3002156829724356 ) ) ;
#67734 = ORIENTED_EDGE ( 'NONE', *, *, #24419, .F. ) ;
#67735 = CYLINDRICAL_SURFACE ( 'NONE', #30989, 4.000000000000000000 ) ;
#67736 = CARTESIAN_POINT ( 'NONE',  ( 0.000000000000000000, 22.97884757028485225, -55.94820918777160301 ) ) ;
#67737 = LINE ( 'NONE', #34339, #30057 ) ;
#67738 = DIRECTION ( 'NONE',  ( 0.000000000000000000, 0.000000000000000000, -1.000000000000000000 ) ) ;
#67739 = CARTESIAN_POINT ( 'NONE',  ( 2.849088235197433594, 81.66451978571728887, -5.000000000000000000 ) ) ;
#67740 = DIRECTION ( 'NONE',  ( 0.000000000000000000, 0.000000000000000000, 1.000000000000000000 ) ) ;
#67741 = ORIENTED_EDGE ( 'NONE', *, *, #56675, .T. ) ;
#67742 = UNCERTAINTY_MEASURE_WITH_UNIT (LENGTH_MEASURE( 1.000000000000000082E-05 ), #44110, 'distance_accuracy_value', 'NONE');
#67743 = EDGE_CURVE ( 'NONE', #48515, #35853, #74567, .T. ) ;
#67744 = CARTESIAN_POINT ( 'NONE',  ( 30.99921441447351356, 438.8475427232315838, 22.05400630073976131 ) ) ;
#67745 = ORIENTED_EDGE ( 'NONE', *, *, #98167, .T. ) ;
#67746 = CARTESIAN_POINT ( 'NONE',  ( 28.86650669486618881, 4.000000000000003553, 4.898587196589414801E-16 ) ) ;
#67747 = CARTESIAN_POINT ( 'NONE',  ( 0.000000000000000000, 0.000000000000000000, 0.000000000000000000 ) ) ;
#67748 = CARTESIAN_POINT ( 'NONE',  ( 39.04923757937011430, 50.00000000002003731, 52.30342408740191473 ) ) ;
#67749 = CARTESIAN_POINT ( 'NONE',  ( 19.83349330513380693, -4.000000000000000000, 4.898587196589415787E-16 ) ) ;
#67750 = DIRECTION ( 'NONE',  ( 0.000000000000000000, -1.000000000000000000, 0.000000000000000000 ) ) ;
#67751 = ORIENTED_EDGE ( 'NONE', *, *, #64272, .F. ) ;
#67752 = CARTESIAN_POINT ( 'NONE',  ( 109.7201212107555222, -60.00000000000001421, 141.0713185866662798 ) ) ;
#67754 = CARTESIAN_POINT ( 'NONE',  ( 22.90497520565338618, -53.39364463476709233, 33.72890349766722551 ) ) ;
#67753 = CARTESIAN_POINT ( 'NONE',  ( -86.50885295532998498, -60.00000000000009237, 203.5147570966663011 ) ) ;
#67755 =( NAMED_UNIT ( * ) PLANE_ANGLE_UNIT ( ) SI_UNIT ( $, .RADIAN. ) );
#67756 = DIRECTION ( 'NONE',  ( 0.000000000000000000, -1.000000000000000000, 0.000000000000000000 ) ) ;
#67757 = CARTESIAN_POINT ( 'NONE',  ( -42.14242943275500153, -39.52740482707008596, 40.59973544904098475 ) ) ;
#67758 = DIRECTION ( 'NONE',  ( 0.000000000000000000, -1.000000000000000000, 0.000000000000000000 ) ) ;
#67759 = UNCERTAINTY_MEASURE_WITH_UNIT (LENGTH_MEASURE( 1.000000000000000082E-05 ), #50239, 'distance_accuracy_value', 'NONE');
#67760 = ORIENTED_EDGE ( 'NONE', *, *, #78975, .T. ) ;
#67761 =( LENGTH_UNIT ( ) NAMED_UNIT ( * ) SI_UNIT ( .MILLI., .METRE. ) );
#67762 = LINE ( 'NONE', #85009, #81818 ) ;
#67763 = CARTESIAN_POINT ( 'NONE',  ( -43.71335306921091046, 464.5235014653455323, 7.258763594085895221 ) ) ;
#67764 = LINE ( 'NONE', #93102, #50937 ) ;
#67765 = CARTESIAN_POINT ( 'NONE',  ( 5.975663821521244756, 4.257391242883541871, 5.625982059626890575 ) ) ;
#67766 = CARTESIAN_POINT ( 'NONE',  ( -35.61495859169594524, 461.3395811758602463, 3.370444927184965689 ) ) ;
#67767 = ORIENTED_EDGE ( 'NONE', *, *, #78695, .T. ) ;
#67768 = ORIENTED_EDGE ( 'NONE', *, *, #49451, .F. ) ;
#67769 = B_SPLINE_CURVE_WITH_KNOTS ( 'NONE', 3,
 ( #9965, #59064, #100037, #11016, #69292, #9413, #100567, #26204, #91950, #75766, #67684, #27801, #102165, #50409, #35887, #83321, #93559, #1860, #52544, #68765 ),
 .UNSPECIFIED., .F., .F.,
 ( 4, 2, 2, 2, 2, 2, 2, 2, 2, 4 ),
 ( 0.003063312233486976607, 0.003568397869495329531, 0.004073483505503682454, 0.004578569141512035812, 0.004831111959516212057, 0.005083654777520388302, 0.005588740413528742526, 0.006093826049537097618, 0.006598911685545452710, 0.007103997321553806935 ),
 .UNSPECIFIED. ) ;
#67770 = CARTESIAN_POINT ( 'NONE',  ( 59.42959829229317847, -29.99999999993401900, 90.05551113897882942 ) ) ;
#67771 = CARTESIAN_POINT ( 'NONE',  ( 24.97083012527267343, 41.55031761159468573, -72.99854779811836636 ) ) ;
#67772 = CIRCLE ( 'NONE', #43735, 7.499999999992679633 ) ;
#67773 = UNCERTAINTY_MEASURE_WITH_UNIT (LENGTH_MEASURE( 1.000000000000000082E-05 ), #35883, 'distance_accuracy_value', 'NONE');
#67774 = CARTESIAN_POINT ( 'NONE',  ( 23.21751746555220564, 25.98869614573808917, -30.70617127781077116 ) ) ;
#67775 = CARTESIAN_POINT ( 'NONE',  ( 86.61642755793405968, -30.00000000000000355, 68.10716385505197934 ) ) ;
#67776 = CARTESIAN_POINT ( 'NONE',  ( -26.34324959015004453, 307.8500962193381270, 10.86395315858437804 ) ) ;
#67777 = EDGE_LOOP ( 'NONE', ( #29114, #12921, #54881, #97893, #4618, #105591 ) ) ;
#67778 = ADVANCED_FACE ( 'NONE', ( #98322 ), #3058, .T. ) ;
#67779 = ORIENTED_EDGE ( 'NONE', *, *, #101045, .F. ) ;
#67780 = ORIENTED_EDGE ( 'NONE', *, *, #105111, .T. ) ;
#67781 = CARTESIAN_POINT ( 'NONE',  ( -32.78378308081553882, 465.0370457077456194, 14.48673668605084153 ) ) ;
#67782 = FACE_OUTER_BOUND ( 'NONE', #33931, .T. ) ;
#67783 = CARTESIAN_POINT ( 'NONE',  ( 70.89460441624491693, 6.975173280561618775E-15, 0.000000000000000000 ) ) ;
#67784 = CARTESIAN_POINT ( 'NONE',  ( 4.904566723942686224, -12.02242702470747382, 3.460360782932700552 ) ) ;
#67785 = CARTESIAN_POINT ( 'NONE',  ( -31.12255084532423055, 439.8601387403313652, 23.32256247975105978 ) ) ;
#67786 = EDGE_CURVE ( 'NONE', #45306, #97178, #65952, .T. ) ;
#67787 = ORIENTED_EDGE ( 'NONE', *, *, #37366, .F. ) ;
#67788 = CARTESIAN_POINT ( 'NONE',  ( -9.596002107488990518, 50.00000000000000000, -92.37456064098950037 ) ) ;
#67789 = B_SPLINE_CURVE_WITH_KNOTS ( 'NONE', 3,
 ( #66222, #99108, #25270, #91057 ),
 .UNSPECIFIED., .F., .F.,
 ( 4, 4 ),
 ( 0.000000000000000000, 0.0001235227585948107888 ),
 .UNSPECIFIED. ) ;
#67790 = VERTEX_POINT ( 'NONE', #23943 ) ;
#67791 = LINE ( 'NONE', #33316, #29518 ) ;
#67792 = CARTESIAN_POINT ( 'NONE',  ( 75.45753799503356163, -38.35118960347601558, 173.8236108886823956 ) ) ;
#67793 = CARTESIAN_POINT ( 'NONE',  ( 6.289692432696767810, 6.589071317540668993, -2.245373559998994129 ) ) ;
#67794 = CARTESIAN_POINT ( 'NONE',  ( 36.42984981315670723, 305.7557014711401848, 4.481287940851245821 ) ) ;
#67795 = CARTESIAN_POINT ( 'NONE',  ( -4.590682673078520182, 248.9320824268784520, 3.864023243754614700 ) ) ;
#67796 = AXIS2_PLACEMENT_3D ( 'NONE', #55963, #14449, #32265 ) ;
#67797 = ORIENTED_EDGE ( 'NONE', *, *, #102858, .F. ) ;
#67798 = CARTESIAN_POINT ( 'NONE',  ( 17.89653557359968872, 45.30873500717390101, -5.550246105160208110 ) ) ;
#67799 = DIRECTION ( 'NONE',  ( 0.000000000000000000, -1.000000000000000000, 0.000000000000000000 ) ) ;
#67800 = CIRCLE ( 'NONE', #81538, 4.000000000000001776 ) ;
#67801 = CARTESIAN_POINT ( 'NONE',  ( 16.36650669486618881, 4.000000000000003553, 4.898587196589414801E-16 ) ) ;
#67802 = EDGE_CURVE ( 'NONE', #24664, #70585, #20046, .T. ) ;
#67803 =( GEOMETRIC_REPRESENTATION_CONTEXT ( 3 ) GLOBAL_UNCERTAINTY_ASSIGNED_CONTEXT ( ( #100642 ) ) GLOBAL_UNIT_ASSIGNED_CONTEXT ( ( #62140, #61604, #103628 ) ) REPRESENTATION_CONTEXT ( 'NONE', 'WORKASPACE' ) );
#67804 = CARTESIAN_POINT ( 'NONE',  ( 15.29454505947262177, 3.501281615901158162, 3.973654925238538027 ) ) ;
#67806 = VERTEX_POINT ( 'NONE', #99910 ) ;
#67805 = AXIS2_PLACEMENT_3D ( 'NONE', #39055, #56797, #14745 ) ;
#67807 = CARTESIAN_POINT ( 'NONE',  ( 30.00000000000000000, 461.8163627757383551, 11.11111419091032460 ) ) ;
#67808 = CARTESIAN_POINT ( 'NONE',  ( -4.999999999999993783, -4.000000000000003553, 102.2532056551910387 ) ) ;
#67809 = PLANE ( 'NONE',  #55670 ) ;
#67810 = CARTESIAN_POINT ( 'NONE',  ( -1.060314165523204677, -8.048081368954012049, -7.659344964962870428 ) ) ;
#67811 = AXIS2_PLACEMENT_3D ( 'NONE', #4270, #10222, #60924 ) ;
#67812 = DIRECTION ( 'NONE',  ( 0.000000000000000000, 0.000000000000000000, 1.000000000000000000 ) ) ;
#67813 = ADVANCED_FACE ( 'NONE', ( #34152 ), #76694, .T. ) ;
#67814 = CARTESIAN_POINT ( 'NONE',  ( -7.213352437320216914, 102.9816352699231743, -3.463014597543483397 ) ) ;
#67815 = CARTESIAN_POINT ( 'NONE',  ( 13.58349330513380160, 4.000000000000002665, 0.000000000000000000 ) ) ;
#67816 = CARTESIAN_POINT ( 'NONE',  ( 84.74699022287541084, -50.18978294560194797, 188.7071310768435524 ) ) ;
#67817 = CARTESIAN_POINT ( 'NONE',  ( 0.7018335428337041382, 15.23280014800325510, -9.981531048852462007 ) ) ;
#67818 = CARTESIAN_POINT ( 'NONE',  ( -3.147946884150642610, 111.7483634657347551, 5.000000000000000000 ) ) ;
#67819 = ORIENTED_EDGE ( 'NONE', *, *, #78805, .F. ) ;
#67820 = DIRECTION ( 'NONE',  ( -0.000000000000000000, 1.000000000000000000, -0.000000000000000000 ) ) ;
#67821 = CARTESIAN_POINT ( 'NONE',  ( 83.86866073052654258, 1.030564683017419500E-14, 0.000000000000000000 ) ) ;
#67822 = CARTESIAN_POINT ( 'NONE',  ( 4.999999999999993783, -46.00000000000000000, 102.2532056551910387 ) ) ;
#67823 = CARTESIAN_POINT ( 'NONE',  ( 0.000000000000000000, 0.000000000000000000, 0.000000000000000000 ) ) ;
#67824 = CARTESIAN_POINT ( 'NONE',  ( -85.87820296494453487, -30.00000000000000000, 63.41064199202992313 ) ) ;
#67825 = FACE_OUTER_BOUND ( 'NONE', #9409, .T. ) ;
#67826 = CARTESIAN_POINT ( 'NONE',  ( 22.57731121199973856, 28.20557510165626880, -30.87924556879413984 ) ) ;
#67827 = LINE ( 'NONE', #50035, #89322 ) ;
#67828 = CARTESIAN_POINT ( 'NONE',  ( -9.483056940782047306, 247.5561220989341962, -3.177305548492608711 ) ) ;
#67829 = CARTESIAN_POINT ( 'NONE',  ( -51.84566471874714466, -38.00000000000001421, 53.44666163652544100 ) ) ;
#67830 = CYLINDRICAL_SURFACE ( 'NONE', #77293, 15.00000000000001243 ) ;
#67831 = CARTESIAN_POINT ( 'NONE',  ( 5.799999999999999822, 8.000000000000000000, 0.000000000000000000 ) ) ;
#67832 = CARTESIAN_POINT ( 'NONE',  ( 0.2578475836320727188, -6.890627091270376425, -1.065083781909170302 ) ) ;
#67833 = CIRCLE ( 'NONE', #5843, 4.000000000000000888 ) ;
#67834 = CARTESIAN_POINT ( 'NONE',  ( 41.91057518544140947, -25.42445561657448394, -29.89054115698944969 ) ) ;
#67835 = CIRCLE ( 'NONE', #55718, 3.500000000000000000 ) ;
#67836 = CARTESIAN_POINT ( 'NONE',  ( -26.36605410305137909, -46.43802873313279633, 33.26382985736353248 ) ) ;
#67837 = ORIENTED_EDGE ( 'NONE', *, *, #74743, .F. ) ;
#67838 = CARTESIAN_POINT ( 'NONE',  ( -17.45941954208535307, -18.58880440242212018, 27.26036603235977296 ) ) ;
#67839 = AXIS2_PLACEMENT_3D ( 'NONE', #73956, #37, #98755 ) ;
#67840 = CARTESIAN_POINT ( 'NONE',  ( -54.44869668617586456, -28.39263527606577853, -26.74396193234344565 ) ) ;
#67841 =( BOUNDED_SURFACE ( )  B_SPLINE_SURFACE ( 2, 3, ( 
 ( #77325, #4496, #44431, #37433 ),
 ( #3438, #95114, #79439, #44974 ),
 ( #52502, #11503, #3969, #28277 ) ),
 .UNSPECIFIED., .F., .F., .F. ) 
 B_SPLINE_SURFACE_WITH_KNOTS ( ( 3, 3 ),
 ( 4, 4 ),
 ( 0.000000000000000000, 1.000000000000000000 ),
 ( -0.05487404235502676975, -0.006958263022644777668 ),
 .UNSPECIFIED. ) 
 GEOMETRIC_REPRESENTATION_ITEM ( )  RATIONAL_B_SPLINE_SURFACE ( (
 ( 1.000000000000000000, 1.000000000000000000, 1.000000000000000000, 1.000000000000000000),
 ( 1.857142857142858317, 1.857142857142858317, 1.857142857142858317, 1.857142857142858317),
 ( 1.000000000000000000, 1.000000000000000000, 1.000000000000000000, 1.000000000000000000) ) ) 
 REPRESENTATION_ITEM ( '' )  SURFACE ( )  );
#67843 = CARTESIAN_POINT ( 'NONE',  ( 0.000000000000000000, 0.000000000000000000, 0.000000000000000000 ) ) ;
#67842 = CARTESIAN_POINT ( 'NONE',  ( -14.33580413386536812, 42.00000000000000000, -89.41414995615788541 ) ) ;
#67844 = ADVANCED_FACE ( 'NONE', ( #35210 ), #62798, .T. ) ;
#67845 = ORIENTED_EDGE ( 'NONE', *, *, #99775, .T. ) ;
#67846 = CARTESIAN_POINT ( 'NONE',  ( 91.37578371391791165, 1.016364837396684119E-14, 0.000000000000000000 ) ) ;
#67847 = ORIENTED_EDGE ( 'NONE', *, *, #525, .T. ) ;
#67848 =( NAMED_UNIT ( * ) PLANE_ANGLE_UNIT ( ) SI_UNIT ( $, .RADIAN. ) );
#67849 = ADVANCED_FACE ( 'NONE', ( #11955 ), #25572, .T. ) ;
#67850 = CARTESIAN_POINT ( 'NONE',  ( 16.02335565827205599, 4.077236164005316965, 2.242500883998115757 ) ) ;
#67851 = B_SPLINE_CURVE_WITH_KNOTS ( 'NONE', 3,
 ( #86954, #79361, #5482, #70221 ),
 .UNSPECIFIED., .F., .F.,
 ( 4, 4 ),
 ( 0.000000000000000000, 1.000000000000000000 ),
 .UNSPECIFIED. ) ;
#67852 = CARTESIAN_POINT ( 'NONE',  ( -3.313708498984765161, -23.65625000409677625, 7.999999999999998224 ) ) ;
#67853 = EDGE_LOOP ( 'NONE', ( #52576, #69393, #89161, #50980, #90456, #54071, #99067, #42022 ) ) ;
#67854 =( NAMED_UNIT ( * ) PLANE_ANGLE_UNIT ( ) SI_UNIT ( $, .RADIAN. ) );
#67855 = CARTESIAN_POINT ( 'NONE',  ( -2.808418600359145145, 294.8278116980254708, -9.614630257155971194 ) ) ;
#67856 = CARTESIAN_POINT ( 'NONE',  ( 102.7294937518374098, -60.17726499089666703, 193.2519588841914810 ) ) ;
#67858 = CARTESIAN_POINT ( 'NONE',  ( -7.151597709147949011, -8.210707349477859296, 3.587174531012140122 ) ) ;
#67857 = CARTESIAN_POINT ( 'NONE',  ( 4.000000000000001776, 0.000000000000000000, -25.03750572909317285 ) ) ;
#67859 = EDGE_LOOP ( 'NONE', ( #44127, #8885, #7156, #12977, #100955 ) ) ;
#67860 = EDGE_CURVE ( 'NONE', #41106, #59573, #20434, .T. ) ;
#67861 = VERTEX_POINT ( 'NONE', #36295 ) ;
#67862 = ORIENTED_EDGE ( 'NONE', *, *, #84338, .T. ) ;
#67863 = CARTESIAN_POINT ( 'NONE',  ( 28.48717193686734106, 313.7474573396027040, 12.33990598094187341 ) ) ;
#67864 = VECTOR ( 'NONE', #14321, 1000.000000000000000 ) ;
#67865 = CARTESIAN_POINT ( 'NONE',  ( -13.50000000000000533, 6.533945317241111717, -12.15804109017022405 ) ) ;
#67866 = CARTESIAN_POINT ( 'NONE',  ( 8.559508646656407649, 53.68473964988125857, 4.031152949374444461 ) ) ;
#67867 = ORIENTED_EDGE ( 'NONE', *, *, #69048, .F. ) ;
#67868 = CARTESIAN_POINT ( 'NONE',  ( 0.000000000000000000, 0.000000000000000000, -11.82492182392400437 ) ) ;
#67869 =( NAMED_UNIT ( * ) SI_UNIT ( $, .STERADIAN. ) SOLID_ANGLE_UNIT ( ) );
#67870 = CONICAL_SURFACE ( 'NONE', #43773, 4.172000000000001485, 0.9599310885968750373 ) ;
#67871 = DIRECTION ( 'NONE',  ( -0.5735764363510497121, 0.8191520442889892450, 1.003171929053521665E-16 ) ) ;
#67872 = CARTESIAN_POINT ( 'NONE',  ( -40.46187072321335165, -57.69130470027779012, 56.40641529803505705 ) ) ;
#67873 = CARTESIAN_POINT ( 'NONE',  ( 7.045755811259132528, -66.30341603013553708, 3.790843699961856217 ) ) ;
#67874 = CARTESIAN_POINT ( 'NONE',  ( -33.63427961064055438, 325.9154870834976236, -4.827994974213513757 ) ) ;
#67875 = DIRECTION ( 'NONE',  ( -1.000000000000000000, 0.000000000000000000, 0.000000000000000000 ) ) ;
#67876 = CARTESIAN_POINT ( 'NONE',  ( -95.23228170574914486, -59.99999999999995737, 30.92731164540345645 ) ) ;
#67877 = SURFACE_STYLE_FILL_AREA ( #59268 ) ;
#67878 = CARTESIAN_POINT ( 'NONE',  ( -49.37788450122778983, -36.05643262852323261, 48.61507133927151614 ) ) ;
#67879 = VERTEX_POINT ( 'NONE', #69163 ) ;
#67880 = CARTESIAN_POINT ( 'NONE',  ( 96.86866073052655679, 5.000000000000021316, 0.000000000000000000 ) ) ;
#67881 = ORIENTED_EDGE ( 'NONE', *, *, #78967, .T. ) ;
#67882 = CARTESIAN_POINT ( 'NONE',  ( 9.833493305133805151, 1.593028355512270962E-15, 0.000000000000000000 ) ) ;
#67883 = LINE ( 'NONE', #42535, #63329 ) ;
#67884 = CARTESIAN_POINT ( 'NONE',  ( 9.877159628591359208, -2.620207910158452336, 15.38486787623552665 ) ) ;
#67885 = ORIENTED_EDGE ( 'NONE', *, *, #77241, .T. ) ;
#67887 = B_SPLINE_CURVE_WITH_KNOTS ( 'NONE', 3,
 ( #853, #39905, #105685, #47968, #72263, #14537, #8983, #31824, #31312, #80877 ),
 .UNSPECIFIED., .F., .F.,
 ( 4, 2, 2, 2, 4 ),
 ( 1.651718721987238896E-28, 0.01019698562015586112, 0.01529547843023379254, 0.01784472483527275305, 0.02039397124031171182 ),
 .UNSPECIFIED. ) ;
#67886 = CARTESIAN_POINT ( 'NONE',  ( 5.383284837158151426, 246.9995065648421928, 2.657356347551702580 ) ) ;
#67888 = CARTESIAN_POINT ( 'NONE',  ( 75.89775319832926925, -38.36850784122120928, 177.7196282691413103 ) ) ;
#67889 = CARTESIAN_POINT ( 'NONE',  ( 0.000000000000000000, -79.93083296558610584, -85.00000000000000000 ) ) ;
#67890 = DIRECTION ( 'NONE',  ( -1.000000000000000000, 0.000000000000000000, 0.000000000000000000 ) ) ;
#67891 = CARTESIAN_POINT ( 'NONE',  ( -7.322849800245839980, -11.36060796471280376, -12.99999999999999467 ) ) ;
#67892 = CARTESIAN_POINT ( 'NONE',  ( 79.13121736037263076, 42.00000000000000000, 45.60838156036771096 ) ) ;
#67893 = CARTESIAN_POINT ( 'NONE',  ( 90.32749040348188885, -30.00000000000000000, 190.1148432507463610 ) ) ;
#67894 = B_SPLINE_SURFACE_WITH_KNOTS ( 'NONE', 3, 3, ( 
 ( #33404, #9089, #74878, #84059, #10160, #100758, #41999, #75962 ),
 ( #17741, #26927, #59800, #2594, #68419, #18834, #101313, #51678 ),
 ( #84599, #966, #66816, #99705, #25876, #58732, #50601, #91631 ),
 ( #83516, #9616, #28511, #93215, #13335, #61395, #68958, #93751 ),
 ( #4738, #45214, #86736, #78088, #30095, #4207, #11743, #12811 ),
 ( #94284, #54313, #19903, #20450, #102903, #53291, #19379, #85123 ),
 ( #44680, #20973, #37136, #70539, #103949, #45725, #52210, #86212 ),
 ( #37677, #87260, #46261, #78607, #38198, #103430, #3682, #79147 ),
 ( #29067, #29579, #61937, #11207, #52746, #62451, #94827, #71058 ),
 ( #95342, #70002, #27994, #12284, #53807, #101829, #21478, #5273 ) ),
 .UNSPECIFIED., .F., .F., .F.,
 ( 4, 2, 2, 2, 4 ),
 ( 4, 2, 2, 4 ),
 ( 0.000000000000000000, 0.1250000000000000000, 0.2500000000000000000, 0.5000000000000000000, 1.000000000000000000 ),
 ( 0.000000000000000000, 0.2500000000000000000, 0.5000000000000000000, 1.000000000000000000 ),
 .UNSPECIFIED. ) ;
#67895 = CARTESIAN_POINT ( 'NONE',  ( -11.51402452371067042, 43.27676821513870209, -14.44504951838048967 ) ) ;
#67896 = EDGE_CURVE ( 'NONE', #44531, #80759, #92661, .T. ) ;
#67897 = AXIS2_PLACEMENT_3D ( 'NONE', #42153, #23887, #75036 ) ;
#67898 = ORIENTED_EDGE ( 'NONE', *, *, #79650, .T. ) ;
#67899 = EDGE_LOOP ( 'NONE', ( #17204, #84753, #79052, #23694, #6002, #24480 ) ) ;
#67900 = CARTESIAN_POINT ( 'NONE',  ( 51.44370365268617462, -53.36997065266968576, 58.22489762912441336 ) ) ;
#67901 = CARTESIAN_POINT ( 'NONE',  ( 6.810575959914616284, 41.35122729146528542, -58.50275608815579176 ) ) ;
#67902 = CARTESIAN_POINT ( 'NONE',  ( -5.500000000000007994, 42.00000000000000000, -72.67206406577980715 ) ) ;
#67903 = EDGE_CURVE ( 'NONE', #43534, #22641, #51381, .T. ) ;
#67904 = ORIENTED_EDGE ( 'NONE', *, *, #90112, .F. ) ;
#67905 = CARTESIAN_POINT ( 'NONE',  ( -86.58581895693029651, -38.36255730625217808, -21.30046015158363204 ) ) ;
#67906 = EDGE_LOOP ( 'NONE', ( #29909, #96204, #89776, #65989, #32003 ) ) ;
#67907 = DIRECTION ( 'NONE',  ( 0.000000000000000000, 0.000000000000000000, -1.000000000000000000 ) ) ;
#67908 = CARTESIAN_POINT ( 'NONE',  ( 108.8405169039002658, -38.35664350992961147, 190.6511209365205559 ) ) ;
#67909 = CARTESIAN_POINT ( 'NONE',  ( 12.79009255231004971, 21.25547159246564277, -5.667716523303968579 ) ) ;
#67910 = CARTESIAN_POINT ( 'NONE',  ( 93.88942621708076786, -52.71697813123014953, 86.64237755783022976 ) ) ;
#67911 = CARTESIAN_POINT ( 'NONE',  ( -1.719443193057841768, -4.999999999999999112, -17.47055129847369770 ) ) ;
#67912 = CARTESIAN_POINT ( 'NONE',  ( -24.81120153453596799, 306.0655852089439577, -9.736014901624853835 ) ) ;
#67913 = PRESENTATION_LAYER_ASSIGNMENT (  '', '', ( #61073 ) ) ;
#67914 = CARTESIAN_POINT ( 'NONE',  ( 1.000000000000000000, -5.000000000000016875, -14.14213562373094746 ) ) ;
#67915 = CARTESIAN_POINT ( 'NONE',  ( -24.46186824438995799, 25.41025174371402784, -31.75584039582438933 ) ) ;
#67916 = AXIS2_PLACEMENT_3D ( 'NONE', #24117, #41853, #66130 ) ;
#67917 = CYLINDRICAL_SURFACE ( 'NONE', #11278, 1.000000000000000888 ) ;
#67918 = CARTESIAN_POINT ( 'NONE',  ( 3.836994546497918268, 134.0493965400703189, 5.000000000000000888 ) ) ;
#67919 = ORIENTED_EDGE ( 'NONE', *, *, #78523, .F. ) ;
#67920 = DIRECTION ( 'NONE',  ( 0.000000000000000000, -1.000000000000000000, 0.000000000000000000 ) ) ;
#67921 = ADVANCED_BREP_SHAPE_REPRESENTATION ( '', ( #90584, #10728 ), #83338 ) ;
#67922 = EDGE_CURVE ( 'NONE', #82432, #85998, #32484, .T. ) ;
#67923 = DIRECTION ( 'NONE',  ( -0.000000000000000000, -1.000000000000000000, -0.000000000000000000 ) ) ;
#67924 = ORIENTED_EDGE ( 'NONE', *, *, #30573, .F. ) ;
#67925 = CARTESIAN_POINT ( 'NONE',  ( -34.40608992613577044, 484.1267599597962317, 0.1303963904809097296 ) ) ;
#67926 = CARTESIAN_POINT ( 'NONE',  ( -40.85805974307315580, 440.2633714685022710, 25.57337624204853199 ) ) ;
#67927 = DIRECTION ( 'NONE',  ( 0.000000000000000000, -1.000000000000000000, 0.000000000000000000 ) ) ;
#67928 = CARTESIAN_POINT ( 'NONE',  ( 5.656854249492380582, -22.81249999999999289, -5.656854249492379694 ) ) ;
#67929 = CARTESIAN_POINT ( 'NONE',  ( 8.000000000000000000, -24.40624999999999645, -3.313708498984761608 ) ) ;
#67930 = CARTESIAN_POINT ( 'NONE',  ( 46.68287061863885867, -28.88195831521701962, 41.82624838710184889 ) ) ;
#67931 = EDGE_CURVE ( 'NONE', #98370, #26898, #44484, .T. ) ;
#67932 = B_SPLINE_CURVE_WITH_KNOTS ( 'NONE', 3,
 ( #2634, #35580, #42036, #91668, #10196, #9652, #75996, #26436 ),
 .UNSPECIFIED., .F., .F.,
 ( 4, 2, 2, 4 ),
 ( 0.000000000000000000, 0.003573659743918579813, 0.005360489615877896824, 0.007147319487837215136 ),
 .UNSPECIFIED. ) ;
#67933 = CARTESIAN_POINT ( 'NONE',  ( 15.88274348574180195, 44.00148148787235414, -4.401868159917717627 ) ) ;
#67934 = EDGE_LOOP ( 'NONE', ( #1069, #15667, #204, #17378, #11866 ) ) ;
#67935 = CARTESIAN_POINT ( 'NONE',  ( 84.60774502086400162, -35.87429910332870975, 178.5856127707324958 ) ) ;
#67936 = EDGE_CURVE ( 'NONE', #18077, #4192, #28197, .T. ) ;
#67937 = DIRECTION ( 'NONE',  ( -1.000000000000000000, -0.000000000000000000, -0.000000000000000000 ) ) ;
#67938 = CARTESIAN_POINT ( 'NONE',  ( -15.42941528477439306, 46.21391461311945648, 5.098611828030516158 ) ) ;
#67939 = ORIENTED_EDGE ( 'NONE', *, *, #37892, .F. ) ;
#67940 = CARTESIAN_POINT ( 'NONE',  ( 23.09999999999999432, 3.309500000000003439, 0.000000000000000000 ) ) ;
#67941 = CIRCLE ( 'NONE', #21460, 1.000000000000000888 ) ;
#67942 = FACE_OUTER_BOUND ( 'NONE', #3210, .T. ) ;
#67943 = DIRECTION ( 'NONE',  ( -1.000000000000000000, -1.224606353822377258E-16, -0.000000000000000000 ) ) ;
#67944 = CARTESIAN_POINT ( 'NONE',  ( -5.499265899526136536, -3.000000000000002665, -99.22427370006747083 ) ) ;
#67945 = CARTESIAN_POINT ( 'NONE',  ( -12.57956330988036164, -3.000000000000003109, -93.28077019085830557 ) ) ;
#67946 = CARTESIAN_POINT ( 'NONE',  ( -36.53758404866636766, -31.84355814719485522, -37.75376796106051103 ) ) ;
#67947 = MECHANICAL_DESIGN_GEOMETRIC_PRESENTATION_REPRESENTATION (  '', ( #83417 ), #38700 ) ;
#67948 = AXIS2_PLACEMENT_3D ( 'NONE', #93568, #93024, #67695 ) ;
#67949 = AXIS2_PLACEMENT_3D ( 'NONE', #36668, #22057, #62507 ) ;
#67950 = CARTESIAN_POINT ( 'NONE',  ( 51.50689545266209279, -59.99999999999999289, 75.64874100463009654 ) ) ;
#67951 = CARTESIAN_POINT ( 'NONE',  ( 27.11672592962718653, -30.49100857079985261, 39.11945417788622592 ) ) ;
#67952 = LINE ( 'NONE', #26999, #101297 ) ;
#67953 = CARTESIAN_POINT ( 'NONE',  ( 5.701534300459289994, -12.96799601469463958, 32.08129232778961182 ) ) ;
#67955 = CARTESIAN_POINT ( 'NONE',  ( -13.56142784925484968, 22.61021997758750146, -2.795891692239694137 ) ) ;
#67954 = CARTESIAN_POINT ( 'NONE',  ( -29.17202919767179026, -31.89494080154250355, 40.11040161891606459 ) ) ;
#67956 = CARTESIAN_POINT ( 'NONE',  ( 9.398978598878366952, 294.6597737643559185, -3.429745804602678305 ) ) ;
#67957 = CARTESIAN_POINT ( 'NONE',  ( 29.07128654445882887, 296.9339959557834163, -9.548856946221640385 ) ) ;
#67958 = CARTESIAN_POINT ( 'NONE',  ( 0.000000000000000000, 0.000000000000000000, 0.000000000000000000 ) ) ;
#67959 = CARTESIAN_POINT ( 'NONE',  ( 28.09999999999999787, 3.309500000000003439, 0.000000000000000000 ) ) ;
#67960 = ORIENTED_EDGE ( 'NONE', *, *, #99080, .T. ) ;
#67961 = CARTESIAN_POINT ( 'NONE',  ( -21.51569398614863715, 294.9107018935607130, -9.987480606144506723 ) ) ;
#67962 = B_SPLINE_CURVE_WITH_KNOTS ( 'NONE', 3,
 ( #2916, #43395, #99479, #50396, #76278, #19696, #66600, #50926, #17536, #83309, #67140, #18068, #52000, #52530, #93548, #35332, #754, #43919, #33721, #35872, #2386, #1845 ),
 .UNSPECIFIED., .F., .F.,
 ( 4, 2, 2, 2, 2, 2, 2, 2, 2, 2, 4 ),
 ( 0.002311503593064429506, 0.002814959816865062261, 0.003066687928765378639, 0.003318416040665695017, 0.003821872264466328641, 0.004073600376366644585, 0.004325328488266960529, 0.005332240935868233847, 0.005835697159668867470, 0.006087425271569182547, 0.006339153383469499359 ),
 .UNSPECIFIED. ) ;
#67963 = UNCERTAINTY_MEASURE_WITH_UNIT (LENGTH_MEASURE( 1.000000000000000082E-05 ), #23645, 'distance_accuracy_value', 'NONE');
#67964 = CARTESIAN_POINT ( 'NONE',  ( 0.000000000000000000, 0.000000000000000000, 8.000000000000000000 ) ) ;
#67965 = DIRECTION ( 'NONE',  ( 0.5735764363510554853, 0.8191520442889852482, 0.000000000000000000 ) ) ;
#67966 = CARTESIAN_POINT ( 'NONE',  ( 18.93998220273022071, -34.58964014173281498, -31.89241200920337604 ) ) ;
#67967 = ADVANCED_FACE ( 'NONE', ( #20655 ), #78876, .T. ) ;
#67968 = CIRCLE ( 'NONE', #59361, 4.000000000000001776 ) ;
#67969 = ORIENTED_EDGE ( 'NONE', *, *, #14860, .T. ) ;
#67970 = CARTESIAN_POINT ( 'NONE',  ( 28.10294377376055053, 36.32212184348568229, 9.577882736625975113 ) ) ;
#67971 = EDGE_LOOP ( 'NONE', ( #98541, #85041, #106270, #56622, #94707, #28542 ) ) ;
#67972 = ADVANCED_FACE ( 'NONE', ( #77772 ), #11725, .T. ) ;
#67973 = FACE_BOUND ( 'NONE', #106710, .T. ) ;
#67974 = EDGE_CURVE ( 'NONE', #57566, #10346, #103663, .T. ) ;
#67975 = CARTESIAN_POINT ( 'NONE',  ( 30.75967547141102187, 7.962001144779974560, -41.50359925574515785 ) ) ;
#67976 = CARTESIAN_POINT ( 'NONE',  ( 0.000000000000000000, 4.898587196589412829E-16, -4.000000000000000000 ) ) ;
#67977 = CONICAL_SURFACE ( 'NONE', #81657, 8.000000000000000000, 1.047197551196600296 ) ;
#67978 = CARTESIAN_POINT ( 'NONE',  ( -91.89192752807107922, -59.99999999999999289, 9.067612356765010873 ) ) ;
#67979 = CARTESIAN_POINT ( 'NONE',  ( -8.000000000000000000, -25.24999999999999289, -9.797174393178825657E-16 ) ) ;
#67980 = AXIS2_PLACEMENT_3D ( 'NONE', #76233, #36365, #99430 ) ;
#67981 = DIRECTION ( 'NONE',  ( -1.000000000000000000, -1.224606353822377258E-16, -0.000000000000000000 ) ) ;
#67982 = CIRCLE ( 'NONE', #11146, 5.000000000000002665 ) ;
#67983 = CARTESIAN_POINT ( 'NONE',  ( 0.000000000000000000, 0.000000000000000000, 5.000000000000000000 ) ) ;
#67984 =( LENGTH_UNIT ( ) NAMED_UNIT ( * ) SI_UNIT ( .MILLI., .METRE. ) );
#67985 = CARTESIAN_POINT ( 'NONE',  ( -81.36484122651633299, -57.00091329419471009, 181.4273748944744113 ) ) ;
#67986 = ORIENTED_EDGE ( 'NONE', *, *, #81028, .F. ) ;
#67987 = DIRECTION ( 'NONE',  ( 0.000000000000000000, 0.000000000000000000, 1.000000000000000000 ) ) ;
#67988 = EDGE_CURVE ( 'NONE', #54873, #6732, #15671, .T. ) ;
#67989 = ORIENTED_EDGE ( 'NONE', *, *, #79449, .F. ) ;
#67990 = CIRCLE ( 'NONE', #31821, 61.50000000000000000 ) ;
#67991 = ORIENTED_EDGE ( 'NONE', *, *, #63694, .T. ) ;
#67992 = CARTESIAN_POINT ( 'NONE',  ( 10.00000000000000000, -15.00000000000000000, 10.00000000000000178 ) ) ;
#67993 = SURFACE_STYLE_USAGE ( .BOTH. , #98361 ) ;
#67994 = CARTESIAN_POINT ( 'NONE',  ( 43.03357534759661718, 463.2291678140137492, 4.675918524166122303 ) ) ;
#67995 = VERTEX_POINT ( 'NONE', #30839 ) ;
#67996 = CARTESIAN_POINT ( 'NONE',  ( 32.20528583231335062, 488.0688772979464716, 8.922366577023394640 ) ) ;
#67997 = CARTESIAN_POINT ( 'NONE',  ( 19.00000000000000711, 4.000000000000000888, 25.00000000000000000 ) ) ;
#67998 = CARTESIAN_POINT ( 'NONE',  ( 7.801642220026312025, -13.58796826149033166, 1.787233835843577534 ) ) ;
#67999 = CARTESIAN_POINT ( 'NONE',  ( -8.000113193197771366, -60.99977361354140015, -0.2613481123984653931 ) ) ;
#68000 = DIRECTION ( 'NONE',  ( -1.000000000000000000, -1.224606353822377258E-16, -0.000000000000000000 ) ) ;
#68001 = CARTESIAN_POINT ( 'NONE',  ( 68.70539558375507738, -4.000000000000000000, 0.000000000000000000 ) ) ;
#68002 = CARTESIAN_POINT ( 'NONE',  ( 88.10210802036469602, -14.21045842199426090, 36.33415240954661840 ) ) ;
#68003 =( BOUNDED_SURFACE ( )  B_SPLINE_SURFACE ( 2, 3, ( 
 ( #44485, #67692, #45024, #13681, #61745, #20786, #62790, #46074, #77909, #4017 ),
 ( #80010, #88128, #21825, #54662, #30977, #70874, #46591, #103244, #78422, #79490 ),
 ( #78957, #71386, #6120, #5601, #14209, #21294, #102710, #38524, #104286, #29389 ) ),
 .UNSPECIFIED., .F., .F., .F. ) 
 B_SPLINE_SURFACE_WITH_KNOTS ( ( 3, 3 ),
 ( 4, 2, 2, 2, 4 ),
 ( 0.000000000000000000, 1.000000000000000000 ),
 ( 0.2013554496957829509, 0.2052093776119387758, 0.2375733647630427492, 0.2537553583385947498, 0.2699373519141466948 ),
 .UNSPECIFIED. ) 
 GEOMETRIC_REPRESENTATION_ITEM ( )  RATIONAL_B_SPLINE_SURFACE ( (
 ( 1.000000000000000000, 1.000000000000000000, 1.000000000000000000, 1.000000000000000000, 1.000000000000000000, 1.000000000000000000, 1.000000000000000000, 1.000000000000000000, 1.000000000000000000, 1.000000000000000000),
 ( 1.857142857142858317, 1.857142857142858317, 1.857142857142858317, 1.857142857142858317, 1.857142857142858317, 1.857142857142858317, 1.857142857142857428, 1.857142857142857428, 1.857142857142858317, 1.857142857142858317),
 ( 1.000000000000000000, 1.000000000000000000, 1.000000000000000000, 1.000000000000000000, 1.000000000000000000, 1.000000000000000000, 1.000000000000000000, 1.000000000000000000, 1.000000000000000000, 1.000000000000000000) ) ) 
 REPRESENTATION_ITEM ( '' )  SURFACE ( )  );
#68004 = CARTESIAN_POINT ( 'NONE',  ( -101.7136998165503883, -14.21045842199435150, 195.4607583018654395 ) ) ;
#68005 = CARTESIAN_POINT ( 'NONE',  ( -58.40069796809858360, -36.02129440492078061, 66.61610187002420957 ) ) ;
#68006 = VERTEX_POINT ( 'NONE', #49631 ) ;
#68007 = SURFACE_STYLE_USAGE ( .BOTH. , #84724 ) ;
#68008 = ORIENTED_EDGE ( 'NONE', *, *, #103113, .F. ) ;
#68009 = CARTESIAN_POINT ( 'NONE',  ( -103.9973128897120915, -45.26549305579687399, 174.9173151977936982 ) ) ;
#68010 = CARTESIAN_POINT ( 'NONE',  ( 30.11650669486618881, -3.851859888774471706E-31, 4.000000000000000888 ) ) ;
#68011 = DIRECTION ( 'NONE',  ( 0.000000000000000000, -1.000000000000000000, 0.000000000000000000 ) ) ;
#68012 = EDGE_LOOP ( 'NONE', ( #60777, #37052, #6422, #59806 ) ) ;
#68013 = CARTESIAN_POINT ( 'NONE',  ( 11.08349330513380515, 1.593028355512270962E-15, 0.000000000000000000 ) ) ;
#68014 = CARTESIAN_POINT ( 'NONE',  ( -67.11354318489686932, -59.99999999999998579, 126.9389420720010122 ) ) ;
#68015 = CARTESIAN_POINT ( 'NONE',  ( -3.365451957726517840, -0.9314134953371686620, 104.1992105446095422 ) ) ;
#68016 = CARTESIAN_POINT ( 'NONE',  ( -1.320432766682874540E-15, -22.90625000204838457, 7.188101187500000044 ) ) ;
#68017 = CARTESIAN_POINT ( 'NONE',  ( 63.07777777777777573, 6.915964383211875250E-15, 0.000000000000000000 ) ) ;
#68018 = CARTESIAN_POINT ( 'NONE',  ( 80.40000000000000568, 4.172000000000019249, 5.109226446042768454E-16 ) ) ;
#68019 =( GEOMETRIC_REPRESENTATION_CONTEXT ( 3 ) GLOBAL_UNCERTAINTY_ASSIGNED_CONTEXT ( ( #18990 ) ) GLOBAL_UNIT_ASSIGNED_CONTEXT ( ( #69023, #33743, #49353 ) ) REPRESENTATION_CONTEXT ( 'NONE', 'WORKASPACE' ) );
#68020 = DIRECTION ( 'NONE',  ( -1.000000000000000000, -1.224606353822377258E-16, -0.000000000000000000 ) ) ;
#68021 = CARTESIAN_POINT ( 'NONE',  ( -26.54817876223620488, 310.6276912632132507, 11.31208242866018132 ) ) ;
#68022 = CARTESIAN_POINT ( 'NONE',  ( 7.372535033043513764, -14.99112640172484490, 15.08559782546382166 ) ) ;
#68023 =( LENGTH_UNIT ( ) NAMED_UNIT ( * ) SI_UNIT ( .MILLI., .METRE. ) );
#68024 = CARTESIAN_POINT ( 'NONE',  ( -31.41190527934607246, -60.32878540294149872, 37.39027770532391770 ) ) ;
#68025 = CARTESIAN_POINT ( 'NONE',  ( -18.99999999999999645, 5.000000000000000888, -1.500000000000000000 ) ) ;
#68026 = CARTESIAN_POINT ( 'NONE',  ( 43.50297803938072860, -22.24728821975209669, 37.57093068451706586 ) ) ;
#68027 = CARTESIAN_POINT ( 'NONE',  ( -32.10528697966002198, 486.1671898930082421, 5.449875171704826826 ) ) ;
#68028 = CARTESIAN_POINT ( 'NONE',  ( -0.1693524243964244225, 45.30391365246044444, 18.74999999999999645 ) ) ;
#68029 = ADVANCED_FACE ( 'NONE', ( #90633 ), #47648, .F. ) ;
#68030 = CARTESIAN_POINT ( 'NONE',  ( -87.31462566429209460, -38.58291539573046691, 199.6787966471005404 ) ) ;
#68031 = ORIENTED_EDGE ( 'NONE', *, *, #64030, .F. ) ;
#68033 = CARTESIAN_POINT ( 'NONE',  ( -42.80559098684942398, 434.8801202232389187, 8.726134940843630616 ) ) ;
#68032 = CARTESIAN_POINT ( 'NONE',  ( -16.10155864910909074, 21.86284619731855372, 0.4346306502030854446 ) ) ;
#68034 = CARTESIAN_POINT ( 'NONE',  ( 51.91349542570045372, -60.00000000000000711, 61.65172145578477370 ) ) ;
#68035 = CARTESIAN_POINT ( 'NONE',  ( -49.10020235979911973, 7.817788915495857083, -16.25178062802477186 ) ) ;
#68036 = CARTESIAN_POINT ( 'NONE',  ( -7.500000000000007105, 40.28750026290749275, -59.87155394325278479 ) ) ;
#68037 = CARTESIAN_POINT ( 'NONE',  ( 7.696567030444234644E-14, -1.200000000000000030E-05, 38.25000000000000000 ) ) ;
#68038 = FACE_OUTER_BOUND ( 'NONE', #68900, .T. ) ;
#68039 = CARTESIAN_POINT ( 'NONE',  ( -26.52730633476061683, 310.2711082345475120, 10.22138833121726442 ) ) ;
#68040 = DIRECTION ( 'NONE',  ( -1.000000000000000000, -0.000000000000000000, -0.000000000000000000 ) ) ;
#68041 = CARTESIAN_POINT ( 'NONE',  ( 107.2905653249216300, -60.00000000000000711, 196.7157100397594149 ) ) ;
#68042 = CARTESIAN_POINT ( 'NONE',  ( 0.2573354458087829810, 4.368923434677195239, 5.432802636760776238 ) ) ;
#68043 = CARTESIAN_POINT ( 'NONE',  ( 34.42407431220851066, 1.340359594676612611E-15, 0.000000000000000000 ) ) ;
#68044 = EDGE_CURVE ( 'NONE', #94625, #67191, #72835, .T. ) ;
#68045 = ORIENTED_EDGE ( 'NONE', *, *, #81129, .T. ) ;
#68046 = CARTESIAN_POINT ( 'NONE',  ( 0.9999999999999940048, -50.00000000000000000, 101.0455488498966758 ) ) ;
#68047 = VECTOR ( 'NONE', #11924, 1000.000000000000000 ) ;
#68048 = CARTESIAN_POINT ( 'NONE',  ( -81.26072837970858131, -30.00000000000007816, -10.92579196702281408 ) ) ;
#68049 = VERTEX_POINT ( 'NONE', #31372 ) ;
#68051 = CARTESIAN_POINT ( 'NONE',  ( 42.20041562234358423, 435.2369744135583574, 7.788607701745475786 ) ) ;
#68050 =( LENGTH_UNIT ( ) NAMED_UNIT ( * ) SI_UNIT ( .MILLI., .METRE. ) );
#68052 = DIRECTION ( 'NONE',  ( 0.000000000000000000, 1.000000000000000000, 0.000000000000000000 ) ) ;
#68053 = CARTESIAN_POINT ( 'NONE',  ( -34.12349128637492157, 490.8027302422244134, 11.84948222508912252 ) ) ;
#68054 = CARTESIAN_POINT ( 'NONE',  ( -7.188101187500002709, -20.18750000204838457, 2.977408999572648707 ) ) ;
#68055 = CARTESIAN_POINT ( 'NONE',  ( -4.403473400622100797, -6.117907484625871639, -6.860966872759830380E-15 ) ) ;
#68057 = B_SPLINE_CURVE_WITH_KNOTS ( 'NONE', 3,
 ( #103312, #21357, #103828, #101709, #77438, #102774, #45087, #77966, #29458, #19255, #93084, #52084, #53167, #84997, #62330, #4081 ),
 .UNSPECIFIED., .F., .F.,
 ( 4, 2, 2, 2, 2, 2, 2, 4 ),
 ( 0.000000000000000000, 0.001828028632607115985, 0.003656057265214231970, 0.005484085897821349039, 0.007312114530428463939, 0.01096817179564269808, 0.01279620042824981992, 0.01462422906085693829 ),
 .UNSPECIFIED. ) ;
#68056 = CIRCLE ( 'NONE', #30128, 4.000000000000007105 ) ;
#68058 = AXIS2_PLACEMENT_3D ( 'NONE', #55397, #31694, #48894 ) ;
#68059 = AXIS2_PLACEMENT_3D ( 'NONE', #24896, #49127, #98223 ) ;
#68060 = FACE_OUTER_BOUND ( 'NONE', #31009, .T. ) ;
#68061 = EDGE_CURVE ( 'NONE', #37759, #71772, #93364, .T. ) ;
#68063 = ORIENTED_EDGE ( 'NONE', *, *, #57027, .F. ) ;
#68062 = CARTESIAN_POINT ( 'NONE',  ( -41.51027609766077120, 460.7143792095437220, 2.893824450528216019 ) ) ;
#68064 = CARTESIAN_POINT ( 'NONE',  ( 81.31836778682512090, -46.44211778139398206, 165.0976634020017855 ) ) ;
#68065 = ADVANCED_FACE ( 'NONE', ( #508 ), #33475, .F. ) ;
#68066 = CARTESIAN_POINT ( 'NONE',  ( -3.866514940531297295, -1.181881931264997077, 103.9726926151897715 ) ) ;
#68067 = AXIS2_PLACEMENT_3D ( 'NONE', #105161, #32360, #6982 ) ;
#68068 = CARTESIAN_POINT ( 'NONE',  ( 9.918512371096300129, 88.79282992270555042, -1.297150762882697261 ) ) ;
#68069 = EDGE_LOOP ( 'NONE', ( #4786, #78202, #15915, #6629 ) ) ;
#68070 = CARTESIAN_POINT ( 'NONE',  ( -80.00000000000000000, -60.00000000000000000, -21.09707704303352926 ) ) ;
#68071 = CARTESIAN_POINT ( 'NONE',  ( -46.97732051764550931, 17.75298140206600905, 16.28617214199123353 ) ) ;
#68072 = DIRECTION ( 'NONE',  ( 1.000000000000000000, 0.000000000000000000, 0.000000000000000000 ) ) ;
#68073 = CARTESIAN_POINT ( 'NONE',  ( 4.898587196589412829E-16, -24.12499999999999289, -8.000000000000000000 ) ) ;
#68074 = MECHANICAL_DESIGN_GEOMETRIC_PRESENTATION_REPRESENTATION (  '', ( #83602 ), #28535 ) ;
#68075 = LINE ( 'NONE', #66474, #43971 ) ;
#68076 = CARTESIAN_POINT ( 'NONE',  ( 0.8433544674962375476, 13.67115454006535558, 51.42600440392107686 ) ) ;
#68077 = CARTESIAN_POINT ( 'NONE',  ( 5.385673916453011856, -2.602085213965210642E-15, 18.57417562100670949 ) ) ;
#68078 = ORIENTED_EDGE ( 'NONE', *, *, #77516, .F. ) ;
#68079 = SURFACE_STYLE_USAGE ( .BOTH. , #2258 ) ;
#68080 = DIRECTION ( 'NONE',  ( -0.5735764363510494901, -0.8191520442889894671, 0.000000000000000000 ) ) ;
#68081 =( NAMED_UNIT ( * ) SI_UNIT ( $, .STERADIAN. ) SOLID_ANGLE_UNIT ( ) );
#68082 = CARTESIAN_POINT ( 'NONE',  ( 86.87595582856886267, -20.64717089365305824, 186.0002144904201202 ) ) ;
#68083 = DIRECTION ( 'NONE',  ( -0.5735764363510497121, 0.8191520442889892450, 1.003171929053521665E-16 ) ) ;
#68084 = CARTESIAN_POINT ( 'NONE',  ( 7.188101187500000044, -25.15625000204838813, 0.000000000000000000 ) ) ;
#68085 = LINE ( 'NONE', #27138, #14723 ) ;
#68086 = CARTESIAN_POINT ( 'NONE',  ( -17.49999999999999645, -2.499999999999999556, 0.000000000000000000 ) ) ;
#68087 = CARTESIAN_POINT ( 'NONE',  ( 18.71538461538461462, 1.411358822780289120E-15, 0.000000000000000000 ) ) ;
#68088 = CONTEXT_DEPENDENT_SHAPE_REPRESENTATION ( #96279, #64115 ) ;
#68089 = VERTEX_POINT ( 'NONE', #58811 ) ;
#68090 = DIRECTION ( 'NONE',  ( -0.5735764363510494901, -0.8191520442889894671, 0.000000000000000000 ) ) ;
#68091 = CARTESIAN_POINT ( 'NONE',  ( 35.59999999999999432, 3.309500000000003439, 0.000000000000000000 ) ) ;
#68092 = CARTESIAN_POINT ( 'NONE',  ( -9.998567040921154003, 7.502056690377623127, -4.999999999999999112 ) ) ;
#68093 = ORIENTED_EDGE ( 'NONE', *, *, #54343, .F. ) ;
#68094 = CYLINDRICAL_SURFACE ( 'NONE', #10216, 4.000000000000000000 ) ;
#68095 = CARTESIAN_POINT ( 'NONE',  ( -7.500000000000005329, -5.250000000000004441, -68.91429205785459544 ) ) ;
#68096 = CARTESIAN_POINT ( 'NONE',  ( 32.48450373119614198, 435.0129692059579156, 18.09237844440232124 ) ) ;
#68097 = CARTESIAN_POINT ( 'NONE',  ( -8.717757428195424652, 51.77844298770122577, -1.531152949373723482 ) ) ;
#68098 = CARTESIAN_POINT ( 'NONE',  ( 16.07917213302812698, 5.118112109469847404, -4.258304778695102932 ) ) ;
#68099 = CARTESIAN_POINT ( 'NONE',  ( 36.48965585550728719, 25.91808176478719616, 12.86142835070472223 ) ) ;
#68100 = CARTESIAN_POINT ( 'NONE',  ( -88.14079865277417980, -60.00000000000000711, 201.4458585072254664 ) ) ;
#68101 = CARTESIAN_POINT ( 'NONE',  ( 18.92174722983540391, 48.90933038775173003, 62.13887004286578275 ) ) ;
#68102 = CARTESIAN_POINT ( 'NONE',  ( -45.48126212248870814, 413.7349014071057240, 8.309231847991947362 ) ) ;
#68103 = DIRECTION ( 'NONE',  ( -0.000000000000000000, -0.09744402424476124314, -0.9952410070626042105 ) ) ;
#68104 = DIRECTION ( 'NONE',  ( 0.000000000000000000, 0.000000000000000000, -1.000000000000000000 ) ) ;
#68105 = CARTESIAN_POINT ( 'NONE',  ( -82.72409333703991763, -60.87321690922112083, 189.9861444112082438 ) ) ;
#68106 = AXIS2_PLACEMENT_3D ( 'NONE', #14215, #47118, #42214 ) ;
#68107 = CARTESIAN_POINT ( 'NONE',  ( -4.652092900574788636, 54.30645573760831724, -6.202889689747271618 ) ) ;
#68108 = EDGE_CURVE ( 'NONE', #23629, #44644, #90990, .T. ) ;
#68109 = EDGE_LOOP ( 'NONE', ( #4760, #3319, #68343, #49823, #103478 ) ) ;
#68110 = CARTESIAN_POINT ( 'NONE',  ( -9.045746190732444347, 45.90313006749668290, -14.51680462862712062 ) ) ;
#68111 = EDGE_CURVE ( 'NONE', #74596, #29512, #25950, .T. ) ;
#68112 = DIRECTION ( 'NONE',  ( -1.000000000000000000, -1.224606353822377258E-16, -0.000000000000000000 ) ) ;
#68113 = CARTESIAN_POINT ( 'NONE',  ( -82.55444755025907000, -37.83384472315690772, 6.159036853484627372 ) ) ;
#68115 = B_SPLINE_CURVE_WITH_KNOTS ( 'NONE', 3,
 ( #72653, #39250, #64059, #55907, #98516, #24145, #73707, #80735, #96422, #23069, #32215, #97443, #97992, #48370, #88844, #105552, #106609, #56455, #14938, #82340, #65632, #106066 ),
 .UNSPECIFIED., .F., .F.,
 ( 4, 2, 2, 2, 2, 2, 2, 2, 2, 2, 4 ),
 ( 0.007334634194406657905, 0.007586619625986230908, 0.007838605057565803044, 0.008342575920724945582, 0.008846546783884086385, 0.009350517647043227187, 0.01035845937336151053, 0.01061044480494107919, 0.01086243023652064786, 0.01111441566810021826, 0.01136640109967978693 ),
 .UNSPECIFIED. ) ;
#68114 = CARTESIAN_POINT ( 'NONE',  ( -5.000000000000000000, -15.63336956925501653, -6.409577599286857996 ) ) ;
#68116 = CARTESIAN_POINT ( 'NONE',  ( -30.24427031855517711, 312.0196691915732004, -8.325478004009855937 ) ) ;
#68117 = CARTESIAN_POINT ( 'NONE',  ( -5.850740358028501120, 4.708522909031559678, -4.999999999999999112 ) ) ;
#68118 = AXIS2_PLACEMENT_3D ( 'NONE', #10052, #76370, #848 ) ;
#68119 = COLOUR_RGB ( '', 0.40784314, 0.44705882, 0.49803922) ;
#68120 = CARTESIAN_POINT ( 'NONE',  ( -12.31099551388335556, -10.27527576804327936, 10.93729666877207585 ) ) ;
#68121 = CARTESIAN_POINT ( 'NONE',  ( -5.973896061805169744, -13.10340519129065839, 13.28276905619559400 ) ) ;
#68122 = CARTESIAN_POINT ( 'NONE',  ( 3.348006310196415480, -1.091696481258594975, 104.4601921234425390 ) ) ;
#68123 = CARTESIAN_POINT ( 'NONE',  ( 70.85242353449750397, -59.99999999999999289, 164.3672743468505359 ) ) ;
#68124 = DIRECTION ( 'NONE',  ( -1.000000000000000000, 0.000000000000000000, 0.000000000000000000 ) ) ;
#68125 = CARTESIAN_POINT ( 'NONE',  ( -86.84190767202800032, -14.21045842199442788, 3.676479754794546473 ) ) ;
#68126 = CARTESIAN_POINT ( 'NONE',  ( -70.72062100957347752, -42.96379174276994917, 106.3028856496189292 ) ) ;
#68127 = PRESENTATION_LAYER_ASSIGNMENT (  '', '', ( #2601 ) ) ;
#68128 = ORIENTED_EDGE ( 'NONE', *, *, #21556, .T. ) ;
#68129 = CARTESIAN_POINT ( 'NONE',  ( 59.93162491489189847, -30.00000000000002842, 91.51739161628221098 ) ) ;
#68130 = CARTESIAN_POINT ( 'NONE',  ( 55.21757201740613397, 40.83935004233791943, 34.80653877613059421 ) ) ;
#68131 = CARTESIAN_POINT ( 'NONE',  ( 2.811255222305522938, -57.67120193607534162, -44.61186864502481342 ) ) ;
#68132 = AXIS2_PLACEMENT_3D ( 'NONE', #24550, #48243, #81144 ) ;
#68134 = ORIENTED_EDGE ( 'NONE', *, *, #9145, .F. ) ;
#68133 = CIRCLE ( 'NONE', #28599, 2.999999999999999112 ) ;
#68135 = CARTESIAN_POINT ( 'NONE',  ( 7.337993220704071007, 52.18301828126001141, -2.466490591092684870 ) ) ;
#68136 = CARTESIAN_POINT ( 'NONE',  ( -5.082755093536325042, -26.46875000204838813, -5.082755093536325930 ) ) ;
#68137 = DIRECTION ( 'NONE',  ( 0.000000000000000000, -1.000000000000000000, 0.000000000000000000 ) ) ;
#68138 = ORIENTED_EDGE ( 'NONE', *, *, #67896, .F. ) ;
#68139 = PRODUCT_DEFINITION_SHAPE ( 'NONE', 'NONE',  #30479 ) ;
#68141 = ORIENTED_EDGE ( 'NONE', *, *, #42627, .F. ) ;
#68140 = CIRCLE ( 'NONE', #7837, 6.500000000000000888 ) ;
#68142 = DIRECTION ( 'NONE',  ( -0.5735764363510497121, 0.8191520442889892450, 1.003171929053521665E-16 ) ) ;
#68143 = CARTESIAN_POINT ( 'NONE',  ( -38.72040230558515361, -59.99999999998055955, 54.32356401625951037 ) ) ;
#68144 = DIRECTION ( 'NONE',  ( 1.000000000000000000, 1.224606353822377258E-16, 0.000000000000000000 ) ) ;
#68145 = CARTESIAN_POINT ( 'NONE',  ( 5.082755093536324154, -11.84375000204838635, 5.082755093536326818 ) ) ;
#68146 = CARTESIAN_POINT ( 'NONE',  ( -48.76595811598829755, 13.46359178982173255, 16.61915017902422420 ) ) ;
#68147 = CONICAL_SURFACE ( 'NONE', #85400, 4.172000000000001485, 0.9599310885968750373 ) ;
#68148 =( BOUNDED_SURFACE ( )  B_SPLINE_SURFACE ( 3, 2, ( 
 ( #63973, #29507, #14856 ),
 ( #104399, #15393, #21930 ),
 ( #89300, #47750, #70982 ),
 ( #104953, #54781, #81180 ),
 ( #23525, #79599, #80649 ),
 ( #6772, #56362, #87710 ),
 ( #87182, #80123, #39692 ),
 ( #22467, #46184, #13792 ),
 ( #79076, #72567, #48279 ),
 ( #7291, #46703, #38126 ),
 ( #5711, #38636, #71500 ),
 ( #30548, #63446, #96341 ) ),
 .UNSPECIFIED., .F., .F., .F. ) 
 B_SPLINE_SURFACE_WITH_KNOTS ( ( 4, 2, 2, 2, 2, 4 ),
 ( 3, 3 ),
 ( 8.673617379884035472E-18, 0.001890581228128788115, 0.002835871842193177835, 0.003781162456257567556, 0.005671743684386346997, 0.007562324912515126438 ),
 ( 0.000000000000000000, 1.000000000000000000 ),
 .UNSPECIFIED. ) 
 GEOMETRIC_REPRESENTATION_ITEM ( )  RATIONAL_B_SPLINE_SURFACE ( (
 ( 1.000000000000000000, 0.7560596356357117687, 1.000000000000000000),
 ( 1.000000000000000000, 0.7675942737806970007, 1.000000000000000000),
 ( 1.000000000000000000, 0.7799842945909555292, 1.000000000000000000),
 ( 1.000000000000000000, 0.7988124055279367530, 1.000000000000000000),
 ( 1.000000000000000000, 0.8051313863604262488, 1.000000000000000000),
 ( 1.000000000000000000, 0.8177136313173961613, 1.000000000000000000),
 ( 1.000000000000000000, 0.8240064671659272921, 1.000000000000000000),
 ( 1.000000000000000000, 0.8422864973116017673, 1.000000000000000000),
 ( 1.000000000000000000, 0.8537348782016001003, 1.000000000000000000),
 ( 1.000000000000000000, 0.8743527270674196217, 1.000000000000000000),
 ( 1.000000000000000000, 0.8835747495209320679, 1.000000000000000000),
 ( 1.000000000000000000, 0.8909749942926241673, 1.000000000000000000) ) ) 
 REPRESENTATION_ITEM ( '' )  SURFACE ( )  );
#68149 = CARTESIAN_POINT ( 'NONE',  ( 1.057603710517943441, -3.557244269805818156E-15, 101.1178170116175181 ) ) ;
#68150 = DIRECTION ( 'NONE',  ( 0.000000000000000000, -0.8267102254948328621, 0.5626279437268314476 ) ) ;
#68151 = CARTESIAN_POINT ( 'NONE',  ( -6.145467200818548470, 49.99999999999999289, -77.00333157709850695 ) ) ;
#68152 = CARTESIAN_POINT ( 'NONE',  ( 7.715274834628325378E-15, 2.000000000000000000, -63.00000000000000000 ) ) ;
#68153 = UNCERTAINTY_MEASURE_WITH_UNIT (LENGTH_MEASURE( 1.000000000000000082E-05 ), #106514, 'distance_accuracy_value', 'NONE');
#68154 = ORIENTED_EDGE ( 'NONE', *, *, #37050, .T. ) ;
#68155 = FILL_AREA_STYLE_COLOUR ( '', #7600 ) ;
#68156 = CARTESIAN_POINT ( 'NONE',  ( 30.90820517067947648, -25.60289659773413362, 30.93734601537375184 ) ) ;
#68157 = CARTESIAN_POINT ( 'NONE',  ( 3.088855081073062209E-15, -4.285714285714286476, 25.22241582816893413 ) ) ;
#68158 = ORIENTED_EDGE ( 'NONE', *, *, #64772, .T. ) ;
#68159 = CARTESIAN_POINT ( 'NONE',  ( -22.89219133817175589, 25.33230817006059965, -33.16583220086505435 ) ) ;
#68160 = EDGE_CURVE ( 'NONE', #88131, #19669, #43149, .T. ) ;
#68161 = VERTEX_POINT ( 'NONE', #42603 ) ;
#68163 = FACE_OUTER_BOUND ( 'NONE', #69870, .T. ) ;
#68162 = CARTESIAN_POINT ( 'NONE',  ( -26.35037284168458527, 34.99717245364579554, -7.807171992874543776 ) ) ;
#68164 = DIRECTION ( 'NONE',  ( 0.000000000000000000, -1.000000000000000000, 0.000000000000000000 ) ) ;
#68165 = CARTESIAN_POINT ( 'NONE',  ( -43.71297783477844234, 485.1278128289774827, -1.116606130290715981 ) ) ;
#68166 = SURFACE_SIDE_STYLE ('',( #42286 ) ) ;
#68167 = FACE_OUTER_BOUND ( 'NONE', #78716, .T. ) ;
#68168 = CARTESIAN_POINT ( 'NONE',  ( 13.58349330513380515, -4.000000000000000000, 4.898587196589415787E-16 ) ) ;
#68169 = VERTEX_POINT ( 'NONE', #2128 ) ;
#68170 = CARTESIAN_POINT ( 'NONE',  ( 86.04389369610818505, -60.00000000000000711, -23.60500139439278655 ) ) ;
#68171 = CARTESIAN_POINT ( 'NONE',  ( 32.94994279514033053, 464.9549361168423047, 15.12478419437801946 ) ) ;
#68172 = AXIS2_PLACEMENT_3D ( 'NONE', #75381, #25275, #8520 ) ;
#68173 = CARTESIAN_POINT ( 'NONE',  ( -47.14583847125333449, 17.20522387600227532, -16.50112645798017041 ) ) ;
#68174 = ADVANCED_FACE ( 'NONE', ( #9161 ), #84122, .T. ) ;
#68175 = ORIENTED_EDGE ( 'NONE', *, *, #53030, .T. ) ;
#68176 = CARTESIAN_POINT ( 'NONE',  ( -86.77091681052317540, -30.00000000002323119, 198.1326347201452336 ) ) ;
#68177 = ORIENTED_EDGE ( 'NONE', *, *, #71650, .T. ) ;
#68178 = MECHANICAL_DESIGN_GEOMETRIC_PRESENTATION_REPRESENTATION (  '', ( #81374 ), #83740 ) ;
#68179 = ORIENTED_EDGE ( 'NONE', *, *, #40286, .F. ) ;
#68180 = CARTESIAN_POINT ( 'NONE',  ( 6.928203230275510549, 85.00000000000000000, 4.000000000000000000 ) ) ;
#68181 = CARTESIAN_POINT ( 'NONE',  ( 38.86638200451619696, 5.000000000000004441, 6.123233995736770227E-16 ) ) ;
#68182 = CARTESIAN_POINT ( 'NONE',  ( -16.58598004038824314, 34.29213908405171196, -24.29859534253508713 ) ) ;
#68183 = PRESENTATION_STYLE_ASSIGNMENT (( #10465 ) ) ;
#68184 = CARTESIAN_POINT ( 'NONE',  ( 83.26455805995850312, -37.81343560710378426, -7.281846265020657682 ) ) ;
#68185 = CARTESIAN_POINT ( 'NONE',  ( -33.42633708788835634, 315.2810023977556284, -7.024978449121026536 ) ) ;
#68186 = CARTESIAN_POINT ( 'NONE',  ( -17.53271835666959788, 45.00000000000000711, 63.43174741287191409 ) ) ;
#68187 = LINE ( 'NONE', #2379, #57354 ) ;
#68188 = ORIENTED_EDGE ( 'NONE', *, *, #2642, .T. ) ;
#68189 = DIRECTION ( 'NONE',  ( -1.734723475976807094E-16, 0.000000000000000000, -1.000000000000000000 ) ) ;
#68190 = ORIENTED_EDGE ( 'NONE', *, *, #100235, .F. ) ;
#68191 = CARTESIAN_POINT ( 'NONE',  ( 48.02835407290503866, 11.61227450977245468, -14.35535821593549954 ) ) ;
#68192 = SURFACE_STYLE_USAGE ( .BOTH. , #35330 ) ;
#68194 = ORIENTED_EDGE ( 'NONE', *, *, #56637, .T. ) ;
#68193 = FACE_OUTER_BOUND ( 'NONE', #41555, .T. ) ;
#68195 = CARTESIAN_POINT ( 'NONE',  ( 78.52207915638700797, -22.14163466735898211, 122.4742839152309557 ) ) ;
#68196 = EDGE_CURVE ( 'NONE', #33037, #27928, #58243, .T. ) ;
#68197 = CONICAL_SURFACE ( 'NONE', #35501, 5.000000000000010658, 0.9599310885968697082 ) ;
#68198 = VERTEX_POINT ( 'NONE', #59878 ) ;
#68199 = CARTESIAN_POINT ( 'NONE',  ( 2.041386142727035224, -49.95395470777400249, 40.93797071785119357 ) ) ;
#68200 = DIRECTION ( 'NONE',  ( -0.02699252395738975518, -0.001721171576548164101, 0.9996341536876447442 ) ) ;
#68201 = CARTESIAN_POINT ( 'NONE',  ( -1.320432766682874540E-15, -27.03125000204838813, 7.188101187500000044 ) ) ;
#68202 = CARTESIAN_POINT ( 'NONE',  ( -94.10527518209565301, -57.67545334945994995, 3.926124123639501029 ) ) ;
#68203 = EDGE_CURVE ( 'NONE', #85895, #101318, #37661, .T. ) ;
#68204 = EDGE_LOOP ( 'NONE', ( #19093, #9928, #70632, #30836 ) ) ;
#68205 = SURFACE_STYLE_FILL_AREA ( #10489 ) ;
#68206 = CARTESIAN_POINT ( 'NONE',  ( 32.42271565838718317, 438.8719799267125268, 23.74906467565527635 ) ) ;
#68207 = AXIS2_PLACEMENT_3D ( 'NONE', #23609, #56461, #89392 ) ;
#68208 = CARTESIAN_POINT ( 'NONE',  ( 105.1856413884972596, -52.71711923733968064, 177.3383578302138233 ) ) ;
#68209 = EDGE_CURVE ( 'NONE', #7953, #57657, #67952, .T. ) ;
#68210 = CARTESIAN_POINT ( 'NONE',  ( -9.176803346051510601, 84.47052844202561062, 3.973598758023530131 ) ) ;
#68211 = CARTESIAN_POINT ( 'NONE',  ( 48.26904874857434180, 16.21976735686757110, -14.37315625587818069 ) ) ;
#68212 = B_SPLINE_CURVE_WITH_KNOTS ( 'NONE', 3,
 ( #102314, #4160, #11694, #77517, #20398, #95826, #95297, #38150 ),
 .UNSPECIFIED., .F., .F.,
 ( 4, 2, 2, 4 ),
 ( 2.459764731290589165E-07, 0.001920659145285759243, 0.002880865729692073940, 0.003841072314098388854 ),
 .UNSPECIFIED. ) ;
#68213 = CARTESIAN_POINT ( 'NONE',  ( -1.469576158976823947E-15, -20.56250000409676915, 8.000000000000000000 ) ) ;
#68214 = EDGE_CURVE ( 'NONE', #36374, #66061, #42769, .T. ) ;
#68215 = AXIS2_PLACEMENT_3D ( 'NONE', #50765, #91791, #9783 ) ;
#68216 = CARTESIAN_POINT ( 'NONE',  ( -36.23827446154780318, -24.64368107998518553, 33.97573338550268573 ) ) ;
#68217 = AXIS2_PLACEMENT_3D ( 'NONE', #72377, #54052, #105283 ) ;
#68218 = CARTESIAN_POINT ( 'NONE',  ( 9.221346651730858213, 248.9516597993166158, -3.869102247876035072 ) ) ;
#68219 = CIRCLE ( 'NONE', #2767, 8.000000000000000000 ) ;
#68220 = CARTESIAN_POINT ( 'NONE',  ( 23.21751746555220564, -1.200000000000000030E-05, -31.95617127781077116 ) ) ;
#68221 = CARTESIAN_POINT ( 'NONE',  ( 9.165151389911677882, 30.26710781282912777, -4.000000000000000888 ) ) ;
#68222 = DIRECTION ( 'NONE',  ( -1.000000000000000000, -0.000000000000000000, -0.000000000000000000 ) ) ;
#68224 = EDGE_CURVE ( 'NONE', #94742, #37271, #13682, .T. ) ;
#68223 = CARTESIAN_POINT ( 'NONE',  ( 51.88291765283138091, 397.1183258646378249, 267.1969486012846460 ) ) ;
#68225 = CARTESIAN_POINT ( 'NONE',  ( 1.155400528493880197, -30.00000000000000711, -7.642489478904992417 ) ) ;
#68226 = ORIENTED_EDGE ( 'NONE', *, *, #94916, .F. ) ;
#68227 = CARTESIAN_POINT ( 'NONE',  ( 43.58619280597250167, 434.9882623928570524, 14.52865984557897860 ) ) ;
#68228 = DIRECTION ( 'NONE',  ( 0.000000000000000000, 0.000000000000000000, 1.000000000000000000 ) ) ;
#68229 = DIRECTION ( 'NONE',  ( -0.000000000000000000, 1.000000000000000000, -0.000000000000000000 ) ) ;
#68230 = CARTESIAN_POINT ( 'NONE',  ( -89.02034635566286624, -29.99999999999999645, 188.7318756114235896 ) ) ;
#68231 = ORIENTED_EDGE ( 'NONE', *, *, #62636, .T. ) ;
#68232 = AXIS2_PLACEMENT_3D ( 'NONE', #77209, #27642, #93405 ) ;
#68233 = CARTESIAN_POINT ( 'NONE',  ( 15.17407431220850533, 1.340359594676612611E-15, 0.000000000000000000 ) ) ;
#68234 = CARTESIAN_POINT ( 'NONE',  ( 81.41097500085039940, -57.51647407579447702, 200.0635567779065411 ) ) ;
#68236 = CARTESIAN_POINT ( 'NONE',  ( 9.999999999999998224, 47.99999999999999289, -86.30899693899574743 ) ) ;
#68235 = CARTESIAN_POINT ( 'NONE',  ( -14.99524476912838367, 1.250852691628805857, 0.4434096853180573006 ) ) ;
#68237 = ORIENTED_EDGE ( 'NONE', *, *, #32944, .F. ) ;
#68238 = CARTESIAN_POINT ( 'NONE',  ( 69.34622291710002173, -38.18775354531572930, -31.40869740071274663 ) ) ;
#68239 = CARTESIAN_POINT ( 'NONE',  ( -14.77017712487166534, 22.74518112338312648, -2.603937284893117710 ) ) ;
#68240 = CARTESIAN_POINT ( 'NONE',  ( -41.86260695335467830, 487.3392455165196111, 9.527470086611755207 ) ) ;
#68241 = CARTESIAN_POINT ( 'NONE',  ( -41.40363853713615327, -59.99999999999999289, 54.19992334669975520 ) ) ;
#68242 = SURFACE_STYLE_FILL_AREA ( #93047 ) ;
#68243 = CARTESIAN_POINT ( 'NONE',  ( 28.89099332390834363, 48.00000000000000000, 58.53034795347323893 ) ) ;
#68244 = CIRCLE ( 'NONE', #6241, 4.000000000000001776 ) ;
#68245 = CARTESIAN_POINT ( 'NONE',  ( -86.60038770626319149, -39.13859030795514826, 188.3081612211328206 ) ) ;
#68246 = ORIENTED_EDGE ( 'NONE', *, *, #32033, .T. ) ;
#68247 = LINE ( 'NONE', #60704, #38457 ) ;
#68248 = CARTESIAN_POINT ( 'NONE',  ( -1.023259250014928456, -60.36594246766334493, 33.95064037087961850 ) ) ;
#68249 = CIRCLE ( 'NONE', #69954, 4.000000000000000888 ) ;
#68250 = CARTESIAN_POINT ( 'NONE',  ( -6.346112372205309882, 41.86049372390779411, -59.13213685944749898 ) ) ;
#68251 = CARTESIAN_POINT ( 'NONE',  ( 32.62730128615243785, 485.2399689022752796, 2.794144060394053497 ) ) ;
#68253 = CARTESIAN_POINT ( 'NONE',  ( -8.398775527966902743, 54.02108431962560786, 1.531152949374565475 ) ) ;
#68252 = CARTESIAN_POINT ( 'NONE',  ( -32.42769167400230401, 299.9084148736556017, 3.070043388578370891 ) ) ;
#68254 = EDGE_CURVE ( 'NONE', #71639, #43184, #82350, .T. ) ;
#68255 = ORIENTED_EDGE ( 'NONE', *, *, #41943, .F. ) ;
#68257 = CARTESIAN_POINT ( 'NONE',  ( -36.74062794522055952, 396.3876241540195906, 6.156540521676369337 ) ) ;
#68256 = B_SPLINE_CURVE_WITH_KNOTS ( 'NONE', 3,
 ( #89410, #17116, #73185, #16033, #7934, #98539, #74265, #14960, #340, #73730, #49992, #16572, #106091, #33308, #41375, #40313 ),
 .UNSPECIFIED., .F., .F.,
 ( 4, 2, 2, 2, 2, 2, 2, 4 ),
 ( -2.482109357202701380E-05, 0.001810221378381205153, 0.003645263850334437561, 0.007315348794240897172, 0.009150391266194126544, 0.01098543373814735505, 0.01282047621010058355, 0.01465551868205381206 ),
 .UNSPECIFIED. ) ;
#68258 = CARTESIAN_POINT ( 'NONE',  ( -5.309984767906265724, -5.000000000000680345, -15.43787989249558734 ) ) ;
#68259 = CARTESIAN_POINT ( 'NONE',  ( -30.93386089602973499, 8.839832930400778110, -40.91297150549259953 ) ) ;
#68260 = CARTESIAN_POINT ( 'NONE',  ( 22.26102485043540824, 295.0200461295465857, -1.964238772177369530 ) ) ;
#68261 = ADVANCED_FACE ( 'NONE', ( #85197 ), #13938, .T. ) ;
#68262 = CARTESIAN_POINT ( 'NONE',  ( 27.47093694407817210, 296.2799286419132727, -9.692114557244172701 ) ) ;
#68263 = DIRECTION ( 'NONE',  ( 0.000000000000000000, 1.000000000000000000, 0.000000000000000000 ) ) ;
#68264 = CARTESIAN_POINT ( 'NONE',  ( 108.2372837266210297, -59.99999999999997868, 115.4707114838127211 ) ) ;
#68265 = CARTESIAN_POINT ( 'NONE',  ( -78.02770516898169717, -60.31600362760740808, 156.3356691730190846 ) ) ;
#68266 = VERTEX_POINT ( 'NONE', #63050 ) ;
#68267 = DIRECTION ( 'NONE',  ( -1.000000000000000000, -1.224606353822377258E-16, -0.000000000000000000 ) ) ;
#68268 = CARTESIAN_POINT ( 'NONE',  ( 5.477432325710311467, 253.1647953557046833, 2.459915882346695337 ) ) ;
#68269 = CARTESIAN_POINT ( 'NONE',  ( 9.923022100475872520, -57.67120321077532452, 41.61848498758426729 ) ) ;
#68270 = DIRECTION ( 'NONE',  ( -1.000000000000000000, -1.224606353822377258E-16, -0.000000000000000000 ) ) ;
#68271 = CARTESIAN_POINT ( 'NONE',  ( 34.37399270670962181, 318.9891659766902876, -6.087815582663091085 ) ) ;
#68272 = CARTESIAN_POINT ( 'NONE',  ( 43.64002961914448520, 465.1123652286975698, 8.841020312837930106 ) ) ;
#68273 = ORIENTED_EDGE ( 'NONE', *, *, #17565, .F. ) ;
#68274 = TOROIDAL_SURFACE ( 'NONE', #64795, 60.50000000000000000, 0.5000000000000000000 ) ;
#68275 = CARTESIAN_POINT ( 'NONE',  ( -17.08544069068336668, 304.5690947107618740, -10.06009145438460983 ) ) ;
#68276 = CARTESIAN_POINT ( 'NONE',  ( 31.35125168101714976, 439.1949078441656980, 22.91632451326402631 ) ) ;
#68277 = ORIENTED_EDGE ( 'NONE', *, *, #16596, .F. ) ;
#68278 =( LENGTH_UNIT ( ) NAMED_UNIT ( * ) SI_UNIT ( .MILLI., .METRE. ) );
#68279 = CARTESIAN_POINT ( 'NONE',  ( -8.331345277524542681, 1.020295532671184640E-15, -7.381345277524544279 ) ) ;
#68280 = CARTESIAN_POINT ( 'NONE',  ( 6.996268247851322286, 41.79455473942780230, -69.25931863577100955 ) ) ;
#68281 = ADVANCED_FACE ( 'NONE', ( #53877 ), #95869, .T. ) ;
#68282 = AXIS2_PLACEMENT_3D ( 'NONE', #42882, #35358, #58547 ) ;
#68283 = CARTESIAN_POINT ( 'NONE',  ( -62.91825180719953892, 50.00000000000000000, 6.605622457240398759 ) ) ;
#68284 = CARTESIAN_POINT ( 'NONE',  ( 4.999999999999960032, -13.06782935463053796, 12.36551185560477784 ) ) ;
#68285 = CARTESIAN_POINT ( 'NONE',  ( -10.00000000000000355, 85.00000000000000000, 0.000000000000000000 ) ) ;
#68286 = ORIENTED_EDGE ( 'NONE', *, *, #83882, .F. ) ;
#68287 = CARTESIAN_POINT ( 'NONE',  ( 90.78097007041577626, -59.99999999999997868, -17.40510296751067187 ) ) ;
#68288 = AXIS2_PLACEMENT_3D ( 'NONE', #70728, #103622, #29770 ) ;
#68290 = CARTESIAN_POINT ( 'NONE',  ( 21.99398094262454606, -22.07632118128579535, 28.30098176883504735 ) ) ;
#68289 = CARTESIAN_POINT ( 'NONE',  ( -102.9006728679688365, -30.00000000000001421, 197.6531887663732618 ) ) ;
#68292 = CARTESIAN_POINT ( 'NONE',  ( 2.892604062750769184E-15, 60.76237703744687479, -11.80995232570204045 ) ) ;
#68291 = PRODUCT_DEFINITION_CONTEXT ( 'detailed design', #39724, 'design' ) ;
#68293 = FACE_OUTER_BOUND ( 'NONE', #8808, .T. ) ;
#68294 = CARTESIAN_POINT ( 'NONE',  ( -35.80230656125740296, -60.29385515264787898, 39.79296061328858514 ) ) ;
#68295 = ADVANCED_FACE ( 'NONE', ( #65701 ), #60053, .T. ) ;
#68296 = CARTESIAN_POINT ( 'NONE',  ( -23.07257312862554599, 18.64284798593020298, 30.73399254005029135 ) ) ;
#68297 = UNCERTAINTY_MEASURE_WITH_UNIT (LENGTH_MEASURE( 1.000000000000000082E-05 ), #102024, 'distance_accuracy_value', 'NONE');
#68298 = EDGE_LOOP ( 'NONE', ( #99666, #22713, #16806, #38856, #39340 ) ) ;
#68299 = CONICAL_SURFACE ( 'NONE', #99286, 5.000000000000001776, 0.9599310885968803664 ) ;
#68300 = FACE_OUTER_BOUND ( 'NONE', #5699, .T. ) ;
#68301 = CARTESIAN_POINT ( 'NONE',  ( -13.45079846400082957, -54.26579227026637398, 23.11721482942554573 ) ) ;
#68302 = CIRCLE ( 'NONE', #18421, 4.000000000000000888 ) ;
#68303 = CARTESIAN_POINT ( 'NONE',  ( 6.222742520105473574, 7.673830019007162662, -0.2914634815676393487 ) ) ;
#68304 = FILL_AREA_STYLE ('',( #79043 ) ) ;
#68305 = ORIENTED_EDGE ( 'NONE', *, *, #70058, .T. ) ;
#68306 = CARTESIAN_POINT ( 'NONE',  ( 30.00000000000000000, 0.000000000000000000, 0.000000000000000000 ) ) ;
#68307 = ORIENTED_EDGE ( 'NONE', *, *, #20482, .T. ) ;
#68308 = CARTESIAN_POINT ( 'NONE',  ( 95.54086597314230289, -30.00000000000007461, 191.3283643440866513 ) ) ;
#68309 = CARTESIAN_POINT ( 'NONE',  ( 43.89937922080078891, 39.34350223877356001, -47.75665600345389805 ) ) ;
#68310 = CARTESIAN_POINT ( 'NONE',  ( -5.725989721596477899, -81.42322888743538556, 1.809923354557187336 ) ) ;
#68311 = CONICAL_SURFACE ( 'NONE', #7995, 4.000000000000007105, 0.9599310885968835860 ) ;
#68312 = CARTESIAN_POINT ( 'NONE',  ( 81.08533849400782856, -30.00000000000000000, 22.49689936057352568 ) ) ;
#68313 = CARTESIAN_POINT ( 'NONE',  ( -30.60088410313775853, 328.0742987498344405, 15.87722222682625173 ) ) ;
#68314 = EDGE_CURVE ( 'NONE', #100791, #80953, #70347, .T. ) ;
#68315 = ORIENTED_EDGE ( 'NONE', *, *, #41419, .T. ) ;
#68316 = ORIENTED_EDGE ( 'NONE', *, *, #50687, .F. ) ;
#68317 = VERTEX_POINT ( 'NONE', #34959 ) ;
#68318 = VECTOR ( 'NONE', #53470, 1000.000000000000000 ) ;
#68320 = ORIENTED_EDGE ( 'NONE', *, *, #70142, .F. ) ;
#68319 = CARTESIAN_POINT ( 'NONE',  ( -32.07495350396642664, 464.7631673202369598, 11.47102835347554617 ) ) ;
#68321 = DIRECTION ( 'NONE',  ( 0.000000000000000000, 0.000000000000000000, 1.000000000000000000 ) ) ;
#68322 = CARTESIAN_POINT ( 'NONE',  ( 5.656854249492380582, -15.31249999999999289, -5.656854249492379694 ) ) ;
#68323 = CARTESIAN_POINT ( 'NONE',  ( 4.813668318631101783, -11.79513229826687493, 3.583991016754772829 ) ) ;
#68324 = CARTESIAN_POINT ( 'NONE',  ( -30.61827153859606909, 339.8037943721997181, 17.27484252342313198 ) ) ;
#68325 = CARTESIAN_POINT ( 'NONE',  ( 12.13034742782427955, 48.00000000000000000, -93.82352941176471006 ) ) ;
#68326 = VERTEX_POINT ( 'NONE', #34435 ) ;
#68327 = CARTESIAN_POINT ( 'NONE',  ( -10.48543666094594684, 50.00000000000000000, -78.95657223723274853 ) ) ;
#68328 = ORIENTED_EDGE ( 'NONE', *, *, #64924, .T. ) ;
#68329 = CARTESIAN_POINT ( 'NONE',  ( -3.826931552919423662, 16.00000000000000000, -9.246279647933182133 ) ) ;
#68330 = CARTESIAN_POINT ( 'NONE',  ( 74.24161930812724108, -38.32798603758613609, 162.4564917793205439 ) ) ;
#68331 = CARTESIAN_POINT ( 'NONE',  ( 67.22793774957824553, -4.000000000000000888, 4.898587196589422689E-16 ) ) ;
#68332 = CARTESIAN_POINT ( 'NONE',  ( 34.06798233701722012, 303.3571279571132209, 11.90485029882048806 ) ) ;
#68333 = CIRCLE ( 'NONE', #59784, 1.000000000000000000 ) ;
#68334 = FACE_OUTER_BOUND ( 'NONE', #891, .T. ) ;
#68335 = ORIENTED_EDGE ( 'NONE', *, *, #98698, .F. ) ;
#68336 = CARTESIAN_POINT ( 'NONE',  ( 0.000000000000000000, 0.000000000000000000, 1.734723475976807094E-15 ) ) ;
#68337 = CONICAL_SURFACE ( 'NONE', #63180, 3.309500000000001663, 0.9599310885968770357 ) ;
#68338 = CARTESIAN_POINT ( 'NONE',  ( 17.84510959215113601, 45.37789619860912183, -5.053583809357707679 ) ) ;
#68339 = CARTESIAN_POINT ( 'NONE',  ( 10.59999999999999609, 1.533819458162526451E-15, 0.000000000000000000 ) ) ;
#68340 = DIRECTION ( 'NONE',  ( -1.000000000000000000, 0.000000000000000000, 0.000000000000000000 ) ) ;
#68341 = EDGE_CURVE ( 'NONE', #81898, #91293, #85739, .T. ) ;
#68342 = CARTESIAN_POINT ( 'NONE',  ( 4.898587196589412829E-16, -21.12499999999999289, -8.000000000000000000 ) ) ;
#68343 = ORIENTED_EDGE ( 'NONE', *, *, #42361, .T. ) ;
#68344 = CARTESIAN_POINT ( 'NONE',  ( 7.619135598915496743, -88.17305367784679504, 2.449260492474795825 ) ) ;
#68345 = CARTESIAN_POINT ( 'NONE',  ( 16.75187969033515145, -1.200000000000000030E-05, -21.80698433968624528 ) ) ;
#68346 = DIRECTION ( 'NONE',  ( 0.000000000000000000, 0.000000000000000000, -1.000000000000000000 ) ) ;
#68347 = DIRECTION ( 'NONE',  ( 0.000000000000000000, 0.000000000000000000, -1.000000000000000000 ) ) ;
#68348 = FACE_OUTER_BOUND ( 'NONE', #51274, .T. ) ;
#68349 = EDGE_CURVE ( 'NONE', #101881, #49122, #90502, .T. ) ;
#68350 = EDGE_CURVE ( 'NONE', #32259, #14808, #39479, .T. ) ;
#68351 = EDGE_LOOP ( 'NONE', ( #79858, #27904 ) ) ;
#68352 = CARTESIAN_POINT ( 'NONE',  ( 0.000000000000000000, 0.000000000000000000, 0.000000000000000000 ) ) ;
#68353 = CARTESIAN_POINT ( 'NONE',  ( 86.41301712325638107, -46.49206446395204040, 190.1341371302563346 ) ) ;
#68354 = AXIS2_PLACEMENT_3D ( 'NONE', #78423, #70875, #46592 ) ;
#68355 =( NAMED_UNIT ( * ) SI_UNIT ( $, .STERADIAN. ) SOLID_ANGLE_UNIT ( ) );
#68356 = CONICAL_SURFACE ( 'NONE', #59736, 8.000000000000000000, 0.9599310885968798113 ) ;
#68357 = CARTESIAN_POINT ( 'NONE',  ( -3.981089209424774733, 136.6339151386011110, 4.999999999999997335 ) ) ;
#68358 = ORIENTED_EDGE ( 'NONE', *, *, #73524, .T. ) ;
#68359 = CARTESIAN_POINT ( 'NONE',  ( 74.56127108291157413, 4.000000000000013323, 0.000000000000000000 ) ) ;
#68360 = EDGE_CURVE ( 'NONE', #76274, #76519, #58678, .T. ) ;
#68361 = EDGE_CURVE ( 'NONE', #17308, #91520, #13508, .T. ) ;
#68362 = DIRECTION ( 'NONE',  ( -0.000000000000000000, 1.000000000000000000, 0.000000000000000000 ) ) ;
#68363 = DIRECTION ( 'NONE',  ( 0.000000000000000000, -1.000000000000000000, 0.000000000000000000 ) ) ;
#68364 = SURFACE_STYLE_USAGE ( .BOTH. , #93162 ) ;
#68365 = CARTESIAN_POINT ( 'NONE',  ( -94.05936093215517246, -29.99999999999999645, 112.3224062120655304 ) ) ;
#68366 = CONICAL_SURFACE ( 'NONE', #4620, 4.172000000000009479, 0.9599310885968813656 ) ;
#68367 = FILL_AREA_STYLE ('',( #19332 ) ) ;
#68368 = STYLED_ITEM ( 'NONE', ( #45059 ), #59647 ) ;
#68369 = CARTESIAN_POINT ( 'NONE',  ( -6.625705691649441675, 5.306270977113046960, -7.795653906408888112 ) ) ;
#68371 =( NAMED_UNIT ( * ) PLANE_ANGLE_UNIT ( ) SI_UNIT ( $, .RADIAN. ) );
#68370 = CARTESIAN_POINT ( 'NONE',  ( 35.44957237873525457, 490.5771127895677637, 12.28211989808393589 ) ) ;
#68372 = PLANE ( 'NONE',  #43616 ) ;
#68373 = CYLINDRICAL_SURFACE ( 'NONE', #23973, 7.500000000001509015 ) ;
#68374 = SURFACE_SIDE_STYLE ('',( #20406 ) ) ;
#68375 = CARTESIAN_POINT ( 'NONE',  ( 0.000000000000000000, 4.000000000000000000, -2.000000000000000888 ) ) ;
#68376 = COLOUR_RGB ( '', 0.72549020, 0.75294118, 0.79215686) ;
#68377 = VECTOR ( 'NONE', #12766, 1000.000000000000000 ) ;
#68378 = CONICAL_SURFACE ( 'NONE', #57961, 4.000000000000007105, 0.9599310885968835860 ) ;
#68379 = CONICAL_SURFACE ( 'NONE', #75278, 0.6840402866513453084, 1.221730476396026610 ) ;
#68380 = CARTESIAN_POINT ( 'NONE',  ( 50.21954304836901173, -27.54177712049025928, -27.91686790315894839 ) ) ;
#68381 = CARTESIAN_POINT ( 'NONE',  ( -22.19868783087845898, -29.03752594377393592, 29.50702968582816865 ) ) ;
#68382 = ORIENTED_EDGE ( 'NONE', *, *, #76027, .F. ) ;
#68383 = DIRECTION ( 'NONE',  ( 0.000000000000000000, -1.000000000000000000, 0.000000000000000000 ) ) ;
#68384 = CARTESIAN_POINT ( 'NONE',  ( -9.165151389911681434, 105.2631950629488387, 4.000000000000004441 ) ) ;
#68385 = AXIS2_PLACEMENT_3D ( 'NONE', #8673, #97674, #7076 ) ;
#68386 = CARTESIAN_POINT ( 'NONE',  ( -19.33192182939703230, -53.40145674591138913, 33.25391692593370863 ) ) ;
#68387 = CARTESIAN_POINT ( 'NONE',  ( 0.000000000000000000, 50.89575828009192549, 0.000000000000000000 ) ) ;
#68389 = CARTESIAN_POINT ( 'NONE',  ( 1.099490667017193335, 36.97155732390793048, -27.88395719433528086 ) ) ;
#68388 = CARTESIAN_POINT ( 'NONE',  ( -1.219336931563358206, 27.86033604905912142, 39.18213164352511058 ) ) ;
#68390 = EDGE_CURVE ( 'NONE', #27731, #14520, #41957, .T. ) ;
#68391 = ORIENTED_EDGE ( 'NONE', *, *, #90254, .T. ) ;
#68392 = CARTESIAN_POINT ( 'NONE',  ( -35.81652876273700770, 437.2229768147630580, 4.496326601633259479 ) ) ;
#68393 = ORIENTED_EDGE ( 'NONE', *, *, #37112, .T. ) ;
#68394 = CARTESIAN_POINT ( 'NONE',  ( 0.000000000000000000, -8.673617379884035472E-16, -22.23822744035697241 ) ) ;
#68395 = EDGE_CURVE ( 'NONE', #82223, #11941, #50551, .T. ) ;
#68396 = CARTESIAN_POINT ( 'NONE',  ( 21.36650669486618881, -3.851859888774471706E-31, 4.000000000000000888 ) ) ;
#68397 = ORIENTED_EDGE ( 'NONE', *, *, #20611, .T. ) ;
#68398 = CYLINDRICAL_SURFACE ( 'NONE', #89405, 5.000000000000002665 ) ;
#68399 = CARTESIAN_POINT ( 'NONE',  ( 62.59428447264396311, -4.000000000000000000, 0.000000000000000000 ) ) ;
#68400 = CARTESIAN_POINT ( 'NONE',  ( 99.57218404754800645, -45.27071417153299393, 192.9608328712945706 ) ) ;
#68402 = CARTESIAN_POINT ( 'NONE',  ( -6.928203230275509661, -10.00000000000000888, 4.000000000000000000 ) ) ;
#68401 = CARTESIAN_POINT ( 'NONE',  ( 0.5742487732211798424, 294.8518027760915743, -10.00000000000000533 ) ) ;
#68403 = CIRCLE ( 'NONE', #13320, 4.000000000000000888 ) ;
#68404 = ORIENTED_EDGE ( 'NONE', *, *, #77541, .F. ) ;
#68405 = ORIENTED_EDGE ( 'NONE', *, *, #17948, .F. ) ;
#68406 = VECTOR ( 'NONE', #86772, 999.9999999999998863 ) ;
#68407 = VERTEX_POINT ( 'NONE', #10113 ) ;
#68408 = CARTESIAN_POINT ( 'NONE',  ( 25.40751943109334121, 308.2109744773123339, 10.71449383779814113 ) ) ;
#68409 = CARTESIAN_POINT ( 'NONE',  ( 0.000000000000000000, 0.000000000000000000, -6.123524522925831270 ) ) ;
#68410 = CARTESIAN_POINT ( 'NONE',  ( 0.000000000000000000, -30.00000000000000000, 8.000000000000000000 ) ) ;
#68411 = ORIENTED_EDGE ( 'NONE', *, *, #16740, .T. ) ;
#68412 = EDGE_CURVE ( 'NONE', #54043, #93508, #75912, .T. ) ;
#68413 = FACE_OUTER_BOUND ( 'NONE', #54119, .T. ) ;
#68414 = CARTESIAN_POINT ( 'NONE',  ( -6.764423789826284228, 41.48989065997112391, -70.49176070234911151 ) ) ;
#68415 = DIRECTION ( 'NONE',  ( -0.000000000000000000, 1.000000000000000000, -0.000000000000000000 ) ) ;
#68416 = CARTESIAN_POINT ( 'NONE',  ( -53.08864208271962326, -59.99999999998543387, -39.69027889185369418 ) ) ;
#68417 = CARTESIAN_POINT ( 'NONE',  ( 23.86650669486618881, 4.000000000000003553, 4.898587196589414801E-16 ) ) ;
#68418 = CARTESIAN_POINT ( 'NONE',  ( -29.01988888469873018, 321.8047804620298393, 14.12772110426748284 ) ) ;
#68419 = CARTESIAN_POINT ( 'NONE',  ( -6.873632436824210323, 41.52279939058548308, -58.77795267647356781 ) ) ;
#68420 = CARTESIAN_POINT ( 'NONE',  ( -86.55941870227799484, -14.21045842199434439, 7.758091717749037386 ) ) ;
#68421 = DIRECTION ( 'NONE',  ( -1.000000000000000000, 0.000000000000000000, 0.000000000000000000 ) ) ;
#68422 = CARTESIAN_POINT ( 'NONE',  ( -51.52612014391598194, -32.58135107158835808, 50.96622865610893172 ) ) ;
#68423 = ORIENTED_EDGE ( 'NONE', *, *, #69598, .T. ) ;
#68424 = DIRECTION ( 'NONE',  ( 0.000000000000000000, 0.000000000000000000, 1.000000000000000000 ) ) ;
#68425 = ORIENTED_EDGE ( 'NONE', *, *, #82201, .T. ) ;
#68426 = CARTESIAN_POINT ( 'NONE',  ( -94.65235043456101494, -37.67961520111438745, 193.0070918200965480 ) ) ;
#68427 = AXIS2_PLACEMENT_3D ( 'NONE', #47908, #39324, #31763 ) ;
#68428 = DIRECTION ( 'NONE',  ( 0.000000000000000000, 1.000000000000000000, 0.000000000000000000 ) ) ;
#68429 = CARTESIAN_POINT ( 'NONE',  ( 6.692649838135032780, 4.003395468798079726, 6.852343244299697211 ) ) ;
#68430 = ORIENTED_EDGE ( 'NONE', *, *, #58041, .F. ) ;
#68431 = DIRECTION ( 'NONE',  ( -1.000000000000000000, -0.000000000000000000, -0.000000000000000000 ) ) ;
#68432 = VECTOR ( 'NONE', #98818, 1000.000000000000227 ) ;
#68433 = CARTESIAN_POINT ( 'NONE',  ( 86.98911389379702541, -30.00000000000125411, -18.62703500237973842 ) ) ;
#68434 = CARTESIAN_POINT ( 'NONE',  ( 49.24259736700050638, 13.36037099747072077, 15.29523612018071965 ) ) ;
#68435 = CARTESIAN_POINT ( 'NONE',  ( 3.769311339736628241, -48.92514534113568914, 104.1674216685381396 ) ) ;
#68436 = DIRECTION ( 'NONE',  ( 0.4165977904505316354, 1.053856448911994735E-15, -0.9090909090909087276 ) ) ;
#68437 = CARTESIAN_POINT ( 'NONE',  ( -19.32152200341433357, 18.64316884707570310, 33.52312678237270660 ) ) ;
#68438 = CARTESIAN_POINT ( 'NONE',  ( 90.09437403127707000, -30.00000000000000355, 189.9480191965106997 ) ) ;
#68439 = CARTESIAN_POINT ( 'NONE',  ( 0.6443221131828161807, 46.14907239561987495, -16.41599980877370868 ) ) ;
#68440 = CARTESIAN_POINT ( 'NONE',  ( 12.33349330513380693, -4.000000000000000888, 4.898587196589416773E-16 ) ) ;
#68441 = ORIENTED_EDGE ( 'NONE', *, *, #36235, .F. ) ;
#68442 = EDGE_LOOP ( 'NONE', ( #32368, #63619, #105948, #61233 ) ) ;
#68443 = CARTESIAN_POINT ( 'NONE',  ( 52.16619185189158259, -46.43791850696331380, 57.11334052445853615 ) ) ;
#68444 = PRESENTATION_LAYER_ASSIGNMENT (  '', '', ( #8127 ) ) ;
#68445 = CARTESIAN_POINT ( 'NONE',  ( 7.006861261201393631, 41.19339584001859578, -58.48462847601448544 ) ) ;
#68446 = CARTESIAN_POINT ( 'NONE',  ( -7.500000000000007994, 40.00000000000000000, -71.41947339646975479 ) ) ;
#68447 = VERTEX_POINT ( 'NONE', #18783 ) ;
#68448 = CARTESIAN_POINT ( 'NONE',  ( -85.63190312002936366, -38.36025793955835184, -22.26003858040750316 ) ) ;
#68449 = VERTEX_POINT ( 'NONE', #26876 ) ;
#68450 = CARTESIAN_POINT ( 'NONE',  ( 110.2505909221214893, -38.35601218213372476, 184.3274032030269325 ) ) ;
#68451 = CARTESIAN_POINT ( 'NONE',  ( 10.04228541497385763, 14.34591999596507605, 10.47348714142258963 ) ) ;
#68453 = CARTESIAN_POINT ( 'NONE',  ( 83.72361235177345407, -37.85036601058070005, 34.46266949494848575 ) ) ;
#68452 = CIRCLE ( 'NONE', #94327, 8.000000000000005329 ) ;
#68454 = AXIS2_PLACEMENT_3D ( 'NONE', #2427, #101133, #27293 ) ;
#68455 = CARTESIAN_POINT ( 'NONE',  ( -0.7826757305971107082, 46.11193258928162209, -16.51179486519325579 ) ) ;
#68457 =( GEOMETRIC_REPRESENTATION_CONTEXT ( 3 ) GLOBAL_UNCERTAINTY_ASSIGNED_CONTEXT ( ( #47182 ) ) GLOBAL_UNIT_ASSIGNED_CONTEXT ( ( #105026, #36884, #27197 ) ) REPRESENTATION_CONTEXT ( 'NONE', 'WORKASPACE' ) );
#68456 = CARTESIAN_POINT ( 'NONE',  ( -27.52310014629760815, 306.6583113186411538, -9.375678193793236304 ) ) ;
#68458 = DIRECTION ( 'NONE',  ( 0.000000000000000000, 1.000000000000000000, 0.000000000000000000 ) ) ;
#68459 = AXIS2_PLACEMENT_3D ( 'NONE', #21586, #60970, #93856 ) ;
#68460 = FILL_AREA_STYLE ('',( #35584 ) ) ;
#68461 = CARTESIAN_POINT ( 'NONE',  ( 8.588478090880302673, 128.2033481600901723, 5.000000000001228351 ) ) ;
#68462 = AXIS2_PLACEMENT_3D ( 'NONE', #96263, #105906, #22912 ) ;
#68463 = ORIENTED_EDGE ( 'NONE', *, *, #101515, .F. ) ;
#68464 = DIRECTION ( 'NONE',  ( 0.000000000000000000, 0.000000000000000000, 1.000000000000000000 ) ) ;
#68465 = ADVANCED_FACE ( 'NONE', ( #51630 ), #68666, .T. ) ;
#68466 = CARTESIAN_POINT ( 'NONE',  ( 7.432466292033693023, 40.29241581942148542, -70.20618918290337263 ) ) ;
#68467 = B_SPLINE_CURVE_WITH_KNOTS ( 'NONE', 3,
 ( #9752, #11890, #93359, #42667, #35140 ),
 .UNSPECIFIED., .F., .F.,
 ( 4, 1, 4 ),
 ( 0.000000000000000000, 0.003752776749732569632, 0.007505553499465139264 ),
 .UNSPECIFIED. ) ;
#68468 = CARTESIAN_POINT ( 'NONE',  ( -32.64042345616925900, 439.6777095554002699, 24.07006591916626448 ) ) ;
#68469 = ORIENTED_EDGE ( 'NONE', *, *, #96960, .F. ) ;
#68470 = CARTESIAN_POINT ( 'NONE',  ( -27.01428231532773339, 307.6193483853298289, -8.382184669494519014 ) ) ;
#68471 = CARTESIAN_POINT ( 'NONE',  ( -27.27224646721448664, 307.4876125405418748, 11.01357167080802313 ) ) ;
#68472 = DIRECTION ( 'NONE',  ( 0.000000000000000000, -1.000000000000000000, 0.000000000000000000 ) ) ;
#68473 = CARTESIAN_POINT ( 'NONE',  ( -37.50059943756144776, 490.7879993827797307, 12.38039871356719246 ) ) ;
#68474 = CARTESIAN_POINT ( 'NONE',  ( -5.656854249492379694, -22.43749999999999289, -5.656854249492380582 ) ) ;
#68475 = FILL_AREA_STYLE ('',( #43651 ) ) ;
#68476 = EDGE_CURVE ( 'NONE', #44795, #89572, #104835, .T. ) ;
#68477 = VECTOR ( 'NONE', #47600, 1000.000000000000114 ) ;
#68478 = CARTESIAN_POINT ( 'NONE',  ( 16.48332215917152155, 43.52969185147832576, -6.657797401561809991 ) ) ;
#68479 = ORIENTED_EDGE ( 'NONE', *, *, #98646, .F. ) ;
#68480 = CARTESIAN_POINT ( 'NONE',  ( 82.96302377660713034, -50.06046201639240678, 183.0585499319920757 ) ) ;
#68482 =( GEOMETRIC_REPRESENTATION_CONTEXT ( 3 ) GLOBAL_UNCERTAINTY_ASSIGNED_CONTEXT ( ( #75304 ) ) GLOBAL_UNIT_ASSIGNED_CONTEXT ( ( #42, #8171, #66408 ) ) REPRESENTATION_CONTEXT ( 'NONE', 'WORKASPACE' ) );
#68481 = SURFACE_STYLE_USAGE ( .BOTH. , #77627 ) ;
#68483 = DIRECTION ( 'NONE',  ( -1.000000000000000000, -0.000000000000000000, -0.000000000000000000 ) ) ;
#68484 = ORIENTED_EDGE ( 'NONE', *, *, #71879, .F. ) ;
#68485 = CARTESIAN_POINT ( 'NONE',  ( -93.38272968296267607, -60.15495384420781733, 76.37983926362966258 ) ) ;
#68486 = ADVANCED_FACE ( 'NONE', ( #63342 ), #22175, .F. ) ;
#68487 = CARTESIAN_POINT ( 'NONE',  ( 0.3167204509598380846, 8.479269695850865318, -1.313474075707212974 ) ) ;
#68488 = CARTESIAN_POINT ( 'NONE',  ( -2.352990130084491319E-16, 7.505553499465148271, -8.000000000000000000 ) ) ;
#68489 = DIRECTION ( 'NONE',  ( -1.224646799147353454E-16, 0.000000000000000000, -1.000000000000000000 ) ) ;
#68490 = COLOUR_RGB ( '', 0.72549020, 0.75294118, 0.79215686) ;
#68491 = CARTESIAN_POINT ( 'NONE',  ( -27.77082267131420323, -28.74908582187916650, -38.27462747494718087 ) ) ;
#68492 = EDGE_CURVE ( 'NONE', #35999, #69803, #63499, .T. ) ;
#68493 = CARTESIAN_POINT ( 'NONE',  ( 48.33459193932809228, -60.00000000000000711, 67.79618997339092346 ) ) ;
#68494 = CARTESIAN_POINT ( 'NONE',  ( 31.89015935598033025, -33.67774583439580027, 41.76421769273258633 ) ) ;
#68495 = CARTESIAN_POINT ( 'NONE',  ( 7.619135598915497631, 108.1730536778467808, 2.449260492474795825 ) ) ;
#68496 = CARTESIAN_POINT ( 'NONE',  ( 3.561767179485014090, -12.72028797016299961, 32.14637440348908370 ) ) ;
#68497 = CIRCLE ( 'NONE', #23696, 2.000000000000001776 ) ;
#68499 = CARTESIAN_POINT ( 'NONE',  ( -11.41761984211839831, 20.35610067118025768, 8.182845679249426851 ) ) ;
#68498 = CARTESIAN_POINT ( 'NONE',  ( -27.49170040733129738, -30.74798487600258312, 39.28685883056335371 ) ) ;
#68500 = CARTESIAN_POINT ( 'NONE',  ( 5.433201317513493223, 294.7714280552164041, -8.410911388643073749 ) ) ;
#68501 = CARTESIAN_POINT ( 'NONE',  ( 2.977408999572651815, -10.43750000204838457, 7.188101187500000933 ) ) ;
#68502 = CARTESIAN_POINT ( 'NONE',  ( 0.000000000000000000, 4.898587196589412829E-16, -4.000000000000000000 ) ) ;
#68503 = ORIENTED_EDGE ( 'NONE', *, *, #64871, .F. ) ;
#68504 = FACE_OUTER_BOUND ( 'NONE', #3265, .T. ) ;
#68505 = AXIS2_PLACEMENT_3D ( 'NONE', #60281, #60798, #10620 ) ;
#68506 = CARTESIAN_POINT ( 'NONE',  ( 2.377971153322278042E-07, -60.00000000000000000, 39.63907915656436387 ) ) ;
#68507 = VERTEX_POINT ( 'NONE', #54673 ) ;
#68508 = CARTESIAN_POINT ( 'NONE',  ( 17.81438722625302518, 1.482358050883964840E-15, 0.000000000000000000 ) ) ;
#68509 = PLANE ( 'NONE',  #50492 ) ;
#68510 = CARTESIAN_POINT ( 'NONE',  ( 40.02592568779148507, 1.482358050883964840E-15, 0.000000000000000000 ) ) ;
#68511 = CARTESIAN_POINT ( 'NONE',  ( 47.11570157807129533, -34.58947700826256977, -28.29334103084299556 ) ) ;
#68512 = ADVANCED_FACE ( 'NONE', ( #39062 ), #94534, .T. ) ;
#68513 = ORIENTED_EDGE ( 'NONE', *, *, #43518, .T. ) ;
#68514 = CARTESIAN_POINT ( 'NONE',  ( 43.58349330513380693, 1.593028355512270567E-15, 0.000000000000000000 ) ) ;
#68515 = CARTESIAN_POINT ( 'NONE',  ( -1.000000000001115108, -52.55160771104127093, 2.953793101315682623 ) ) ;
#68516 = COLOUR_RGB ( '', 0.40784314, 0.44705882, 0.49803922) ;
#68517 = CIRCLE ( 'NONE', #28911, 4.000000000000000888 ) ;
#68518 = ORIENTED_EDGE ( 'NONE', *, *, #11330, .F. ) ;
#68519 = EDGE_CURVE ( 'NONE', #65192, #26769, #35978, .T. ) ;
#68520 = DIRECTION ( 'NONE',  ( 0.000000000000000000, -1.000000000000000000, -2.311253228826400140E-16 ) ) ;
#68521 = EDGE_CURVE ( 'NONE', #53206, #6761, #6657, .T. ) ;
#68522 = CARTESIAN_POINT ( 'NONE',  ( 0.000000000000000000, 0.000000000000000000, 0.000000000000000000 ) ) ;
#68523 = CARTESIAN_POINT ( 'NONE',  ( 0.000000000000000000, 0.000000000000000000, 0.000000000000000000 ) ) ;
#68524 = CARTESIAN_POINT ( 'NONE',  ( -93.39231211507048158, -60.00000000000000711, 36.05560009178016401 ) ) ;
#68525 = STYLED_ITEM ( 'NONE', ( #30865 ), #59131 ) ;
#68526 = SURFACE_STYLE_FILL_AREA ( #2158 ) ;
#68527 = DIRECTION ( 'NONE',  ( 0.000000000000000000, -1.000000000000000000, 0.000000000000000000 ) ) ;
#68528 = CIRCLE ( 'NONE', #56493, 6.500000000000000888 ) ;
#68529 = CARTESIAN_POINT ( 'NONE',  ( 35.56416567323501710, 480.2820146177156175, -4.363888856302766683 ) ) ;
#68530 = CARTESIAN_POINT ( 'NONE',  ( 40.86877072095135333, 461.0519673121681876, 2.323807444222599106 ) ) ;
#68531 = B_SPLINE_CURVE_WITH_KNOTS ( 'NONE', 3,
 ( #90527, #15033, #16639, #6942, #33376, #15569, #66249, #48984, #32849, #31264, #56001, #65189, #88938, #99130, #48460, #80830, #25295, #81350, #58153, #39862, #40378, #49528 ),
 .UNSPECIFIED., .F., .F.,
 ( 4, 2, 2, 2, 2, 2, 2, 2, 2, 2, 4 ),
 ( 0.003086826075679745870, 0.003590365117157389135, 0.004093904158635032833, 0.004597443200112676098, 0.005100982241590319363, 0.005604521283067962628, 0.005856290803806785995, 0.006108060324545609363, 0.006611599366023262168, 0.006863368886762087270, 0.007115138407500913240 ),
 .UNSPECIFIED. ) ;
#68533 = DIRECTION ( 'NONE',  ( 0.000000000000000000, -1.000000000000000000, 0.000000000000000000 ) ) ;
#68532 = CARTESIAN_POINT ( 'NONE',  ( -1.308996937483428269, -3.000000000000002665, -75.00000000000001421 ) ) ;
#68534 = CARTESIAN_POINT ( 'NONE',  ( -84.64411001500138809, -28.97345275897948724, 168.9245721654432657 ) ) ;
#68535 = ORIENTED_EDGE ( 'NONE', *, *, #45450, .T. ) ;
#68536 = ORIENTED_EDGE ( 'NONE', *, *, #87301, .F. ) ;
#68537 = EDGE_LOOP ( 'NONE', ( #34345, #6619, #18179, #89559, #83458, #46537 ) ) ;
#68538 = AXIS2_PLACEMENT_3D ( 'NONE', #97994, #74244, #99037 ) ;
#68539 = DIRECTION ( 'NONE',  ( -0.000000000000000000, -1.000000000000000000, -0.000000000000000000 ) ) ;
#68540 = CARTESIAN_POINT ( 'NONE',  ( 18.00094660900708377, -4.332661967061082642, 2.683237397146490011 ) ) ;
#68541 = EDGE_LOOP ( 'NONE', ( #65640, #70988, #21053, #66801 ) ) ;
#68542 = EDGE_CURVE ( 'NONE', #73679, #87052, #106518, .T. ) ;
#68543 = AXIS2_PLACEMENT_3D ( 'NONE', #15681, #48571, #76571 ) ;
#68544 = DIRECTION ( 'NONE',  ( 0.000000000000000000, -1.000000000000000000, 0.000000000000000000 ) ) ;
#68545 = CARTESIAN_POINT ( 'NONE',  ( -85.55066431120862092, -57.67066120584623690, -26.59325976709777706 ) ) ;
#68546 = CARTESIAN_POINT ( 'NONE',  ( 7.986468734911285949, -13.97313679723080782, 0.5341897780976077037 ) ) ;
#68547 = CARTESIAN_POINT ( 'NONE',  ( 62.33904886068935980, 6.975173280561618775E-15, 0.000000000000000000 ) ) ;
#68548 = CARTESIAN_POINT ( 'NONE',  ( 23.21751746555303342, 28.11705169068991594, 30.70617127781016720 ) ) ;
#68549 = CARTESIAN_POINT ( 'NONE',  ( 13.86650669486618881, 0.000000000000000000, 4.000000000000000888 ) ) ;
#68550 = CARTESIAN_POINT ( 'NONE',  ( -5.000000000000000000, -14.29967096554028849, 12.05652987285084343 ) ) ;
#68551 = CARTESIAN_POINT ( 'NONE',  ( 91.50784380495012726, -29.99999999999993960, 42.72614900145088512 ) ) ;
#68552 = ADVANCED_FACE ( 'NONE', ( #45563 ), #10483, .T. ) ;
#68553 = CARTESIAN_POINT ( 'NONE',  ( -84.52733067048065152, -59.99999999999991473, 202.7036346196431111 ) ) ;
#68554 = CARTESIAN_POINT ( 'NONE',  ( -60.96421378324996709, -18.64597550156105754, 64.94627126466191669 ) ) ;
#68555 = AXIS2_PLACEMENT_3D ( 'NONE', #84337, #49832, #18020 ) ;
#68556 = ORIENTED_EDGE ( 'NONE', *, *, #96164, .T. ) ;
#68557 = EDGE_LOOP ( 'NONE', ( #15455, #61519, #14780, #25635, #74884, #75989, #11807, #28312, #36711, #78911, #66807, #90964 ) ) ;
#68558 = CARTESIAN_POINT ( 'NONE',  ( -105.2860375889557076, -52.71044453558685206, 172.7917639000798715 ) ) ;
#68559 = FILL_AREA_STYLE_COLOUR ( '', #14443 ) ;
#68560 = ADVANCED_FACE ( 'NONE', ( #94654 ), #20799, .T. ) ;
#68561 = CARTESIAN_POINT ( 'NONE',  ( -6.133363361299304373, 51.27081518319509712, 8.207696194639346743 ) ) ;
#68562 = CIRCLE ( 'NONE', #80538, 4.000000000000002665 ) ;
#68563 = CARTESIAN_POINT ( 'NONE',  ( 16.52731600354976749, 43.98685737190850631, -87.77869701378344303 ) ) ;
#68564 = ORIENTED_EDGE ( 'NONE', *, *, #94287, .T. ) ;
#68565 = CARTESIAN_POINT ( 'NONE',  ( 6.827804075408431927, -2.999999999999529265, -71.19745151638494463 ) ) ;
#68566 = CARTESIAN_POINT ( 'NONE',  ( -46.69195340547801010, -59.99999999999998579, 64.09799256419935887 ) ) ;
#68567 = CARTESIAN_POINT ( 'NONE',  ( -3.753470829068492165, -1.089309597783810757, 104.5911851069063374 ) ) ;
#68568 = CARTESIAN_POINT ( 'NONE',  ( 7.188101187500000044, -12.03125000204838635, 0.000000000000000000 ) ) ;
#68569 = DIRECTION ( 'NONE',  ( 0.000000000000000000, 0.000000000000000000, -1.000000000000000000 ) ) ;
#68570 = DIRECTION ( 'NONE',  ( 1.000000000000000000, 0.000000000000000000, 0.000000000000000000 ) ) ;
#68571 = CARTESIAN_POINT ( 'NONE',  ( 7.540142361526415371, 0.000000000000000000, -15.29459302239930274 ) ) ;
#68572 = CARTESIAN_POINT ( 'NONE',  ( -25.95507789760542039, 309.1386286255022924, 10.94030088463808070 ) ) ;
#68573 = CARTESIAN_POINT ( 'NONE',  ( 43.71297783477844234, 485.1278128289774827, -1.116606130290200172 ) ) ;
#68574 = DIRECTION ( 'NONE',  ( 1.000000000000000000, 1.224606353822377258E-16, 0.000000000000000000 ) ) ;
#68575 = CARTESIAN_POINT ( 'NONE',  ( -7.500000000000003553, 7.934965735923709573, -31.00258070019285839 ) ) ;
#68576 = UNCERTAINTY_MEASURE_WITH_UNIT (LENGTH_MEASURE( 1.000000000000000082E-05 ), #97149, 'distance_accuracy_value', 'NONE');
#68577 = CARTESIAN_POINT ( 'NONE',  ( -31.94552423878153746, -39.49308952852756960, 33.87865584480293535 ) ) ;
#68578 = DIRECTION ( 'NONE',  ( -1.000000000000000000, 0.000000000000000000, 0.000000000000000000 ) ) ;
#68579 = MECHANICAL_DESIGN_GEOMETRIC_PRESENTATION_REPRESENTATION (  '', ( #97799 ), #59966 ) ;
#68580 = UNCERTAINTY_MEASURE_WITH_UNIT (LENGTH_MEASURE( 1.000000000000000082E-05 ), #104340, 'distance_accuracy_value', 'NONE');
#68581 = CARTESIAN_POINT ( 'NONE',  ( 43.99760445235895645, -42.98121213538102836, 43.39625074881774935 ) ) ;
#68582 = CARTESIAN_POINT ( 'NONE',  ( -4.250000000000000000, 5.204748896376250699E-16, -3.764187203485586330 ) ) ;
#68584 = CIRCLE ( 'NONE', #82337, 4.000000000000000888 ) ;
#68583 = DIRECTION ( 'NONE',  ( 0.000000000000000000, 1.000000000000000000, 0.000000000000000000 ) ) ;
#68585 = CARTESIAN_POINT ( 'NONE',  ( -97.92846326097485132, -38.48021779882554938, 200.9938350945185448 ) ) ;
#68586 = VERTEX_POINT ( 'NONE', #70358 ) ;
#68588 = CYLINDRICAL_SURFACE ( 'NONE', #54248, 4.000000000000000000 ) ;
#68587 = CARTESIAN_POINT ( 'NONE',  ( -16.10373777989384791, 21.82388053253103877, 0.8730104594837211351 ) ) ;
#68589 = CARTESIAN_POINT ( 'NONE',  ( 32.75304820937488159, -59.99999999999998579, 37.97536356120721024 ) ) ;
#68590 = CARTESIAN_POINT ( 'NONE',  ( -19.08521797759478744, 49.65371826308247449, 61.76473638255668419 ) ) ;
#68591 = CARTESIAN_POINT ( 'NONE',  ( 4.966176485634620441, 41.64999999999997726, -70.47555195150160046 ) ) ;
#68592 = CYLINDRICAL_SURFACE ( 'NONE', #34304, 1.000000000000000000 ) ;
#68593 = CARTESIAN_POINT ( 'NONE',  ( -21.52055329178771359, 305.1194042196812575, 8.994324108963519748 ) ) ;
#68594 = CARTESIAN_POINT ( 'NONE',  ( -7.500000000000006217, 39.99999999999122480, -59.88032989330939415 ) ) ;
#68595 = CIRCLE ( 'NONE', #18630, 4.000000000000001776 ) ;
#68596 = CARTESIAN_POINT ( 'NONE',  ( 112.1219226975825052, -60.00000000000001421, 177.4905933672216349 ) ) ;
#68597 = PRESENTATION_LAYER_ASSIGNMENT (  '', '', ( #99502 ) ) ;
#68598 = DIRECTION ( 'NONE',  ( 0.000000000000000000, 0.000000000000000000, -1.000000000000000000 ) ) ;
#68599 = VERTEX_POINT ( 'NONE', #21305 ) ;
#68600 =( NAMED_UNIT ( * ) PLANE_ANGLE_UNIT ( ) SI_UNIT ( $, .RADIAN. ) );
#68601 = EDGE_CURVE ( 'NONE', #9794, #13534, #46322, .T. ) ;
#68602 = CARTESIAN_POINT ( 'NONE',  ( -3.400000000000000355, 4.163799117101001052E-16, -4.147675477074182382 ) ) ;
#68603 = EDGE_LOOP ( 'NONE', ( #25960, #103777, #43351, #46760, #20234 ) ) ;
#68604 = CARTESIAN_POINT ( 'NONE',  ( 5.233596130300162130, 8.457361458019045486, -28.79146962302072055 ) ) ;
#68605 = CARTESIAN_POINT ( 'NONE',  ( 8.000000000000000000, -21.40624999999999645, -3.313708498984761164 ) ) ;
#68606 = CARTESIAN_POINT ( 'NONE',  ( 8.559508646656350805, -1.200000000000000030E-05, -2.781152949374623873 ) ) ;
#68607 = CARTESIAN_POINT ( 'NONE',  ( 3.140345045834405546, -5.000000000000000000, -16.11513581654612537 ) ) ;
#68608 = AXIS2_PLACEMENT_3D ( 'NONE', #21878, #100754, #84594 ) ;
#68609 = CARTESIAN_POINT ( 'NONE',  ( -2.977408999572650039, -20.56250000204838457, -7.188101187500001821 ) ) ;
#68610 = CIRCLE ( 'NONE', #16930, 12.50000000000000533 ) ;
#68611 = CARTESIAN_POINT ( 'NONE',  ( -43.59756234217317683, 434.3244621007142996, 14.55946156040369921 ) ) ;
#68612 = EDGE_CURVE ( 'NONE', #95088, #45889, #89362, .T. ) ;
#68613 = EDGE_CURVE ( 'NONE', #102378, #20513, #47994, .T. ) ;
#68614 = UNCERTAINTY_MEASURE_WITH_UNIT (LENGTH_MEASURE( 1.000000000000000082E-05 ), #56210, 'distance_accuracy_value', 'NONE');
#68615 = CIRCLE ( 'NONE', #58267, 4.000000000000000888 ) ;
#68616 = EDGE_CURVE ( 'NONE', #82136, #214, #41079, .T. ) ;
#68617 = CARTESIAN_POINT ( 'NONE',  ( -17.49999999999999645, -2.499999999999999556, 0.000000000000000000 ) ) ;
#68618 = ORIENTED_EDGE ( 'NONE', *, *, #104465, .F. ) ;
#68619 = CARTESIAN_POINT ( 'NONE',  ( 82.18267182277710958, -42.97061699490445363, 167.7090913738393567 ) ) ;
#68620 = EDGE_CURVE ( 'NONE', #23946, #74912, #64915, .T. ) ;
#68621 = FACE_OUTER_BOUND ( 'NONE', #30009, .T. ) ;
#68623 = ADVANCED_FACE ( 'NONE', ( #65967 ), #39595, .T. ) ;
#68622 = CARTESIAN_POINT ( 'NONE',  ( 6.831985876597696183, -3.295913427296359277, -6.443925148804115821 ) ) ;
#68624 = ORIENTED_EDGE ( 'NONE', *, *, #23335, .T. ) ;
#68625 = CARTESIAN_POINT ( 'NONE',  ( -16.99886460162771584, 302.5644684816759309, -10.06107950202810031 ) ) ;
#68626 = ADVANCED_FACE ( 'NONE', ( #8788 ), #69102, .T. ) ;
#68627 = CARTESIAN_POINT ( 'NONE',  ( -4.966176470918042263, 41.64999999999998437, -70.47555194646970733 ) ) ;
#68628 = SURFACE_STYLE_FILL_AREA ( #21163 ) ;
#68629 = DIRECTION ( 'NONE',  ( -1.000000000000000000, -1.224606353822377258E-16, -0.000000000000000000 ) ) ;
#68630 = CARTESIAN_POINT ( 'NONE',  ( -5.649205854336965871, 253.4535453281150410, -2.034449005107577868 ) ) ;
#68631 = CARTESIAN_POINT ( 'NONE',  ( 17.72964667321921084, 43.18374047180136444, 6.032092183256372309 ) ) ;
#68632 = CARTESIAN_POINT ( 'NONE',  ( 9.241465400471236435, -0.3878019662490226893, 19.78591767756827124 ) ) ;
#68633 = VERTEX_POINT ( 'NONE', #82142 ) ;
#68634 =( NAMED_UNIT ( * ) PLANE_ANGLE_UNIT ( ) SI_UNIT ( $, .RADIAN. ) );
#68635 = CARTESIAN_POINT ( 'NONE',  ( 65.52222222222222570, -3.309500000000000774, 0.000000000000000000 ) ) ;
#68636 = CARTESIAN_POINT ( 'NONE',  ( -5.000000000000000888, -70.02685735654881682, 13.01550610203317682 ) ) ;
#68637 = CARTESIAN_POINT ( 'NONE',  ( 87.01843083760033437, -46.44379687455451489, 190.9307336648631406 ) ) ;
#68639 = DIRECTION ( 'NONE',  ( 0.000000000000000000, 0.000000000000000000, 1.000000000000000000 ) ) ;
#68638 = CARTESIAN_POINT ( 'NONE',  ( 42.73089261237365832, 435.7309723475635792, 18.11242468272457984 ) ) ;
#68640 = CIRCLE ( 'NONE', #1456, 55.00000000000000000 ) ;
#68641 = CARTESIAN_POINT ( 'NONE',  ( -7.188101187500001821, -23.00000000204839523, -2.977408999572651371 ) ) ;
#68642 = DIRECTION ( 'NONE',  ( 0.8660254037844380415, -0.5000000000000011102, 0.000000000000000000 ) ) ;
#68643 = CARTESIAN_POINT ( 'NONE',  ( 7.996316163938711696, -5.000000000000000000, 6.145999768513703110 ) ) ;
#68644 = AXIS2_PLACEMENT_3D ( 'NONE', #54888, #6331, #22578 ) ;
#68645 = DIRECTION ( 'NONE',  ( 0.000000000000000000, 1.000000000000000000, 0.000000000000000000 ) ) ;
#68646 = EDGE_LOOP ( 'NONE', ( #70837, #59256, #1732, #63510, #60370, #32394 ) ) ;
#68647 = CARTESIAN_POINT ( 'NONE',  ( 1.494050070974696619E-08, -60.00000000000001421, -44.99999999996100541 ) ) ;
#68648 = CARTESIAN_POINT ( 'NONE',  ( -5.898801552711128160, 4.639897325518991700, -5.000000000000000000 ) ) ;
#68649 = DIRECTION ( 'NONE',  ( 0.000000000000000000, -1.000000000000000000, 0.000000000000000000 ) ) ;
#68650 = ORIENTED_EDGE ( 'NONE', *, *, #93351, .F. ) ;
#68651 = AXIS2_PLACEMENT_3D ( 'NONE', #42090, #74449, #17842 ) ;
#68652 = CARTESIAN_POINT ( 'NONE',  ( -8.400245266945324474, 51.89220219220736396, -1.531152949373711269 ) ) ;
#68653 = CARTESIAN_POINT ( 'NONE',  ( -33.85195725564122426, 465.2464970902066739, 17.18122764674262370 ) ) ;
#68654 = ORIENTED_EDGE ( 'NONE', *, *, #58934, .T. ) ;
#68655 = STYLED_ITEM ( 'NONE', ( #91398 ), #2790 ) ;
#68656 = EDGE_CURVE ( 'NONE', #39378, #70947, #41170, .T. ) ;
#68657 = CARTESIAN_POINT ( 'NONE',  ( 32.15507750052547919, 435.6575521615077378, 19.42892730969162685 ) ) ;
#68658 = CARTESIAN_POINT ( 'NONE',  ( -8.875831270970040876, 51.71986688677656474, -1.561544505752369139 ) ) ;
#68659 = CARTESIAN_POINT ( 'NONE',  ( 10.00005432054556742, 100.9998641986208838, 0.2621623937322780651 ) ) ;
#68660 = CARTESIAN_POINT ( 'NONE',  ( -16.75187969033459012, 36.38380281757147827, 24.30698433969199357 ) ) ;
#68661 = CARTESIAN_POINT ( 'NONE',  ( -94.42299775263619210, -60.00000000000000000, 202.5617398974961247 ) ) ;
#68662 = DIRECTION ( 'NONE',  ( -1.000000000000000000, -1.224606353822377258E-16, -0.000000000000000000 ) ) ;
#68663 = CARTESIAN_POINT ( 'NONE',  ( 9.067167209133366157, 43.96885688137683701, -13.86970262315736413 ) ) ;
#68665 = AXIS2_PLACEMENT_3D ( 'NONE', #7899, #8962, #73699 ) ;
#68664 = DIRECTION ( 'NONE',  ( -1.000000000000000000, -1.224606353822377258E-16, -0.000000000000000000 ) ) ;
#68666 = CONICAL_SURFACE ( 'NONE', #53188, 4.000000000000001776, 0.9599310885968808105 ) ;
#68667 = CARTESIAN_POINT ( 'NONE',  ( -85.89786254057293036, -25.01153798521900384, 177.6387691999012475 ) ) ;
#68668 = ORIENTED_EDGE ( 'NONE', *, *, #88801, .F. ) ;
#68669 = LINE ( 'NONE', #67596, #6143 ) ;
#68670 = CARTESIAN_POINT ( 'NONE',  ( 1.000000000000000222, -5.000000000000000000, -14.14213562373095101 ) ) ;
#68671 = CARTESIAN_POINT ( 'NONE',  ( -83.76838281802336894, -45.26691656702287503, 6.940423426407160257 ) ) ;
#68672 = DIRECTION ( 'NONE',  ( 0.5735764363510491570, -0.8191520442889895781, 1.003171929053522035E-16 ) ) ;
#68673 = CARTESIAN_POINT ( 'NONE',  ( -15.55686096457869461, 44.07612650370892737, 4.784268412334826692 ) ) ;
#68674 = CARTESIAN_POINT ( 'NONE',  ( -15.69541548456635915, -4.397703964512687413, 14.35461870892897629 ) ) ;
#68676 = CARTESIAN_POINT ( 'NONE',  ( 28.31925951855187051, 36.30018004457540570, -9.115863556877831897 ) ) ;
#68675 = PRESENTATION_LAYER_ASSIGNMENT (  '', '', ( #106527 ) ) ;
#68677 = CARTESIAN_POINT ( 'NONE',  ( 55.65414010178471926, 42.00000000000000000, 72.41885610124163009 ) ) ;
#68678 = CARTESIAN_POINT ( 'NONE',  ( 55.31236231582965956, -60.00000000000003553, 93.46951393418744658 ) ) ;
#68679 = CARTESIAN_POINT ( 'NONE',  ( -23.61990465140407380, 60.76237703744687479, 11.80995232570203690 ) ) ;
#68680 = CARTESIAN_POINT ( 'NONE',  ( -89.66254536497091010, -30.00000000000007461, 1.293233577394788725 ) ) ;
#68681 = CARTESIAN_POINT ( 'NONE',  ( -71.58537349543678374, -60.33171839608677800, 120.7708638787018742 ) ) ;
#68682 = ORIENTED_EDGE ( 'NONE', *, *, #10578, .F. ) ;
#68683 = CARTESIAN_POINT ( 'NONE',  ( 81.96363334812492951, -30.00000000000004263, 194.6668941393791386 ) ) ;
#68684 = CARTESIAN_POINT ( 'NONE',  ( 61.99203922365963138, 40.83832228034810186, -19.76974671391372596 ) ) ;
#68685 = ORIENTED_EDGE ( 'NONE', *, *, #91617, .F. ) ;
#68686 = CARTESIAN_POINT ( 'NONE',  ( 79.64422146358542420, -57.67118961797744703, -30.40228359957061599 ) ) ;
#68687 = COLOUR_RGB ( '', 0.08235294, 0.09019608, 0.10196078) ;
#68688 = ORIENTED_EDGE ( 'NONE', *, *, #104253, .T. ) ;
#68689 = CARTESIAN_POINT ( 'NONE',  ( 14.46849319673338918, -7.726810110884599681, 12.86012526411075463 ) ) ;
#68690 = CARTESIAN_POINT ( 'NONE',  ( -7.188101187500000044, -27.78125000204838813, -8.802885111219163269E-16 ) ) ;
#68691 = EDGE_CURVE ( 'NONE', #43850, #46319, #16352, .T. ) ;
#68692 = CARTESIAN_POINT ( 'NONE',  ( -1.250365908232453638, 27.68769234945010638, -39.65568885478079153 ) ) ;
#68693 = VERTEX_POINT ( 'NONE', #7719 ) ;
#68694 = CARTESIAN_POINT ( 'NONE',  ( 43.51084452654469459, 465.2903130129626561, 9.421687747985401984 ) ) ;
#68695 = ORIENTED_EDGE ( 'NONE', *, *, #102647, .F. ) ;
#68696 = CARTESIAN_POINT ( 'NONE',  ( 8.169585525225409484, 39.99999999999999289, -72.41994148081866456 ) ) ;
#68697 = DIRECTION ( 'NONE',  ( -1.000000000000000000, -1.224606353822377258E-16, -0.000000000000000000 ) ) ;
#68698 = CARTESIAN_POINT ( 'NONE',  ( -42.76485599677753413, -59.99999999998050271, 61.36626925380817710 ) ) ;
#68699 = CARTESIAN_POINT ( 'NONE',  ( 33.71177684279670927, 320.6764605112623485, -5.903303350106816616 ) ) ;
#68700 = CARTESIAN_POINT ( 'NONE',  ( -1.320432766682874540E-15, -12.03125000204838635, 7.188101187500000044 ) ) ;
#68701 = CARTESIAN_POINT ( 'NONE',  ( -49.09761780907699347, 12.98984206366086980, 16.25597134831825130 ) ) ;
#68702 = DIRECTION ( 'NONE',  ( -1.000000000000000000, 0.000000000000000000, 0.000000000000000000 ) ) ;
#68703 = CARTESIAN_POINT ( 'NONE',  ( 3.454253436624921569, -49.15858197120396511, 103.7259032015043090 ) ) ;
#68704 = CARTESIAN_POINT ( 'NONE',  ( -8.000000000000000000, -14.74999999999999289, -9.797174393178825657E-16 ) ) ;
#68705 = CARTESIAN_POINT ( 'NONE',  ( 40.79885302903696243, 436.7553892629202323, 6.138960499418544714 ) ) ;
#68706 = PRESENTATION_LAYER_ASSIGNMENT (  '', '', ( #80673 ) ) ;
#68707 = ORIENTED_EDGE ( 'NONE', *, *, #67464, .F. ) ;
#68708 = CARTESIAN_POINT ( 'NONE',  ( 0.000000000000000000, -48.79941684889506348, 120.8571428571428612 ) ) ;
#68709 = CIRCLE ( 'NONE', #36018, 4.000000000000000888 ) ;
#68711 = CARTESIAN_POINT ( 'NONE',  ( 33.47252721207472348, -56.83589283137767012, 37.78155003957702007 ) ) ;
#68710 = CARTESIAN_POINT ( 'NONE',  ( 43.38825400968193691, 436.1092026048715411, 18.83721859163726009 ) ) ;
#68712 = CARTESIAN_POINT ( 'NONE',  ( -3.301606509414339641, -4.285714285714286476, -25.22241582816893413 ) ) ;
#68713 = ORIENTED_EDGE ( 'NONE', *, *, #23177, .T. ) ;
#68714 = CARTESIAN_POINT ( 'NONE',  ( -22.19943786829402299, 26.05963078907934971, -31.21165477453312320 ) ) ;
#68715 = CONICAL_SURFACE ( 'NONE', #22215, 4.000000000000001776, 0.9599310885968808105 ) ;
#68717 = CARTESIAN_POINT ( 'NONE',  ( 6.924711585765388477, 40.92328497145224020, -70.90711766198887744 ) ) ;
#68716 = DIRECTION ( 'NONE',  ( 0.000000000000000000, 0.000000000000000000, -1.000000000000000000 ) ) ;
#68718 = CARTESIAN_POINT ( 'NONE',  ( 82.42421628608209971, 5.000000000000020428, 0.000000000000000000 ) ) ;
#68719 = CARTESIAN_POINT ( 'NONE',  ( -43.03265099499976998, 484.2747968070553952, -0.8099405866661972819 ) ) ;
#68720 = LINE ( 'NONE', #75174, #54920 ) ;
#68721 = CARTESIAN_POINT ( 'NONE',  ( 32.77384846114002670, 465.0024891621475831, 11.55799621383277476 ) ) ;
#68722 = CARTESIAN_POINT ( 'NONE',  ( -7.500000000000000000, 3.608439182435155601, -7.298562697733106397 ) ) ;
#68724 = ORIENTED_EDGE ( 'NONE', *, *, #4236, .T. ) ;
#68723 = CIRCLE ( 'NONE', #106558, 4.000000000000000888 ) ;
#68725 = CARTESIAN_POINT ( 'NONE',  ( 92.46921543868899107, -60.00000000000001421, -0.8085169714401274632 ) ) ;
#68726 = LINE ( 'NONE', #101608, #8522 ) ;
#68727 = FACE_OUTER_BOUND ( 'NONE', #62022, .T. ) ;
#68728 = CARTESIAN_POINT ( 'NONE',  ( -6.890281280090280625, 41.03680257558234246, -70.85895802555796763 ) ) ;
#68729 = CARTESIAN_POINT ( 'NONE',  ( 100.6222222222222200, 1.023464760207051730E-14, 0.000000000000000000 ) ) ;
#68730 = ORIENTED_EDGE ( 'NONE', *, *, #47468, .F. ) ;
#68731 = CARTESIAN_POINT ( 'NONE',  ( -105.5920425955938384, -29.99999999999728928, 194.5055816160023028 ) ) ;
#68732 = ORIENTED_EDGE ( 'NONE', *, *, #58862, .F. ) ;
#68733 = CIRCLE ( 'NONE', #32553, 2.000000000000001776 ) ;
#68734 = CARTESIAN_POINT ( 'NONE',  ( 7.801339272325196639, 81.41268528040301078, -1.788609912539675495 ) ) ;
#68735 = DIRECTION ( 'NONE',  ( 0.5735764363510468256, 0.8191520442889913545, 0.000000000000000000 ) ) ;
#68736 = CARTESIAN_POINT ( 'NONE',  ( 0.000000000000000000, -6.938893903907228378E-15, 0.000000000000000000 ) ) ;
#68737 = CARTESIAN_POINT ( 'NONE',  ( 86.47354485262529522, -60.23000014668301105, -12.63761204200946153 ) ) ;
#68738 = CARTESIAN_POINT ( 'NONE',  ( -30.91631631796286328, 309.2558939697229334, -8.523808448843370300 ) ) ;
#68739 = CARTESIAN_POINT ( 'NONE',  ( -13.58421898291219598, 304.5480222432819346, -10.06457054468338619 ) ) ;
#68740 = CARTESIAN_POINT ( 'NONE',  ( -18.19227789368855852, 45.00000000000000711, 62.45676960188954752 ) ) ;
#68741 = PRESENTATION_STYLE_ASSIGNMENT (( #27243 ) ) ;
#68742 = ORIENTED_EDGE ( 'NONE', *, *, #105601, .F. ) ;
#68743 = CARTESIAN_POINT ( 'NONE',  ( -42.83167223030816473, 435.5834305853701949, 17.69761675601652584 ) ) ;
#68744 = EDGE_CURVE ( 'NONE', #9776, #103460, #49237, .T. ) ;
#68745 = ORIENTED_EDGE ( 'NONE', *, *, #93701, .F. ) ;
#68746 = SURFACE_STYLE_FILL_AREA ( #101090 ) ;
#68747 =( NAMED_UNIT ( * ) SI_UNIT ( $, .STERADIAN. ) SOLID_ANGLE_UNIT ( ) );
#68748 = MECHANICAL_DESIGN_GEOMETRIC_PRESENTATION_REPRESENTATION (  '', ( #94619 ), #80793 ) ;
#68749 = B_SPLINE_CURVE_WITH_KNOTS ( 'NONE', 3,
 ( #2670, #51213, #50672, #68496, #91704, #9695, #42604, #76033, #51755, #67953, #59879, #50167, #59340, #83585, #74958, #19452, #83069, #75501, #18361, #101386, #52287, #42073, #509, #33476, #1597, #34559, #1050, #27539, #34023, #11282, #66897, #26470, #99233, #99782, #84670, #67433, #84138, #10235, #43150, #74432, #2129, #43671, #58261, #66349, #25401, #100835, #76559, #60418, #91186, #17293, #44215, #45282, #5351, #20528, #4280, #79223, #53365, #45804, #36692, #103503, #77103, #93827, #104023, #22078, #21044, #37750, #62010, #94365, #78681, #52825, #38272, #4814, #12357, #70612, #60937, #28590, #30165, #78162, #19980, #3221, #28064, #86286, #29655, #21553, #62527, #95412, #85752, #29140, #61473, #44755, #95954, #11824, #37209, #94903, #71131, #54933, #63051, #54389, #86811, #70078, #102979, #77643, #87861, #3760, #36162, #69555, #53878, #69032, #102445, #87335, #12884, #13411, #46335, #101906, #98586, #97509, #81328 ),
 .UNSPECIFIED., .F., .F.,
 ( 4, 2, 2, 2, 1, 1, 1, 1, 2, 2, 2, 1, 1, 1, 1, 1, 2, 2, 2, 2, 1, 1, 1, 1, 1, 2, 2, 2, 2, 1, 1, 1, 1, 2, 2, 2, 2, 1, 1, 1, 1, 2, 2, 2, 2, 1, 1, 1, 1, 1, 2, 2, 2, 2, 1, 1, 1, 1, 1, 2, 2, 2, 2, 1, 1, 1, 1, 1, 1, 2, 2, 2, 1, 1, 1, 1, 1, 2, 2, 4 ),
 ( 0.5037612912634689133, 0.5192687509114792821, 0.5347762105594896509, 0.5352608186734899576, 0.5357454267874903753, 0.5367146430154909886, 0.5386530754714922153, 0.5425299403834946688, 0.5502836702074995756, 0.5657911298555096113, 0.5660334339125097092, 0.5662757379695099180, 0.5667603460835102247, 0.5677295623115108381, 0.5696679947675119537, 0.5735448596795142961, 0.5812985895035190920, 0.5968060491515284616, 0.6278209684475473118, 0.6280632725045475206, 0.6283055765615477295, 0.6287901846755481472, 0.6297594009035489826, 0.6316978333595504314, 0.6355746982715534399, 0.6433284280955595680, 0.6588358877435718242, 0.6898508070395963365, 0.6903354151535967542, 0.6908200232675971719, 0.6917892394955980073, 0.6937276719515996781, 0.6976045368636032418, 0.7053582666876103691, 0.7208657263356246236, 0.7518806456316531328, 0.7523652537456535505, 0.7528498618596540792, 0.7538190780876552477, 0.7557575105436572516, 0.7596343754556612593, 0.7673881052796691637, 0.7828955649276855278, 0.8139104842237181447, 0.8141527882807184646, 0.8143950923377187845, 0.8148797004517192022, 0.8158489166797204817, 0.8177873491357228186, 0.8216642140477272704, 0.8294179438717363961, 0.8449254035197544255, 0.8759403228157905952, 0.8761826268727910261, 0.8764249309297913459, 0.8769095390437922077, 0.8778787552717941534, 0.8798171877277980446, 0.8836940526398056051, 0.8914477824638205039, 0.9069552421118506347, 0.9379701614079103411, 0.9380913134364107231, 0.9382124654649108830, 0.9384547695219115360, 0.9389393776359126198, 0.9399085938639146764, 0.9418470263199185677, 0.9457238912319263502, 0.9534776210559416931, 0.9689850807039722680, 0.9691062327324724279, 0.9692273847609724768, 0.9694696888179727967, 0.9699542969319729924, 0.9709235131599739388, 0.9728619456159757206, 0.9767388105279791732, 0.9844925403519861895, 1.000000000000000000 ),
 .UNSPECIFIED. ) ;
#68751 = EDGE_LOOP ( 'NONE', ( #50321, #105902, #98902, #43833 ) ) ;
#68750 = CARTESIAN_POINT ( 'NONE',  ( 5.411617511166468830, 41.81753644224158251, -58.91471485095114247 ) ) ;
#68752 = CARTESIAN_POINT ( 'NONE',  ( 78.83263402278350895, -18.67162436856858676, 121.1150609631452539 ) ) ;
#68753 = CIRCLE ( 'NONE', #22243, 4.000000000000001776 ) ;
#68754 = ORIENTED_EDGE ( 'NONE', *, *, #73796, .F. ) ;
#68755 = CARTESIAN_POINT ( 'NONE',  ( 6.794369677605540225, -48.10722477442604372, 39.24113341299863578 ) ) ;
#68756 = CARTESIAN_POINT ( 'NONE',  ( -7.000000000000000000, 8.572527594031471218E-16, -13.00000000000000000 ) ) ;
#68757 = EDGE_CURVE ( 'NONE', #35102, #105955, #97970, .T. ) ;
#68758 = CARTESIAN_POINT ( 'NONE',  ( 5.082755093536324154, -23.84375000204838457, 5.082755093536326818 ) ) ;
#68759 = EDGE_CURVE ( 'NONE', #98535, #26380, #11810, .T. ) ;
#68760 = CARTESIAN_POINT ( 'NONE',  ( -76.77372030740811226, -57.52889592737719227, 194.6762175334667972 ) ) ;
#68761 = ORIENTED_EDGE ( 'NONE', *, *, #56506, .T. ) ;
#68762 = CARTESIAN_POINT ( 'NONE',  ( 0.000000000000000000, 79.50000000000000000, -65.50000000000000000 ) ) ;
#68763 = CARTESIAN_POINT ( 'NONE',  ( 106.5029100764443513, -60.15152792750651400, 170.5906469400855201 ) ) ;
#68764 = VECTOR ( 'NONE', #80125, 1000.000000000000114 ) ;
#68765 = CARTESIAN_POINT ( 'NONE',  ( -37.56673239365863282, 27.60449318992554879, -13.45617127781024891 ) ) ;
#68766 = DIRECTION ( 'NONE',  ( -0.000000000000000000, -0.000000000000000000, -1.000000000000000000 ) ) ;
#68767 = CARTESIAN_POINT ( 'NONE',  ( 3.313708498984762496, -18.96875000409676915, 7.999999999999998224 ) ) ;
#68768 = CARTESIAN_POINT ( 'NONE',  ( -49.89404489861477288, -29.66878297426404387, 46.44302417657395665 ) ) ;
#68769 = CIRCLE ( 'NONE', #22265, 8.000000000000000000 ) ;
#68770 = CARTESIAN_POINT ( 'NONE',  ( 31.84999999999999787, -3.309499999999999886, 4.475777889183790779E-16 ) ) ;
#68771 = CARTESIAN_POINT ( 'NONE',  ( 0.000000000000000000, 4.898587196589412829E-16, -4.000000000000000000 ) ) ;
#68772 = CARTESIAN_POINT ( 'NONE',  ( 61.85555555555556140, 3.309500000000014541, 4.052968581778174646E-16 ) ) ;
#68773 = DIRECTION ( 'NONE',  ( 2.775557561562891351E-17, -0.1585527532634883607, 0.9873505073845698643 ) ) ;
#68774 = CARTESIAN_POINT ( 'NONE',  ( 7.122964895856751077, -30.00000000000000355, -0.9654893961775683486 ) ) ;
#68775 = ORIENTED_EDGE ( 'NONE', *, *, #29019, .F. ) ;
#68776 = CARTESIAN_POINT ( 'NONE',  ( -3.443402964575895009, -49.16961384600919871, 44.01147765779307264 ) ) ;
#68777 = CARTESIAN_POINT ( 'NONE',  ( 11.87025963472306422, -4.834378162015144476, -12.56279239310862472 ) ) ;
#68778 = CARTESIAN_POINT ( 'NONE',  ( 0.000000000000000000, 0.000000000000000000, -3.852324522925831385 ) ) ;
#68779 = CARTESIAN_POINT ( 'NONE',  ( -85.97022708240267264, -30.00000000000000711, 178.4417459103200088 ) ) ;
#68780 = EDGE_LOOP ( 'NONE', ( #71230, #39304, #95149, #3981 ) ) ;
#68781 = DIRECTION ( 'NONE',  ( 0.000000000000000000, 1.000000000000000000, 0.000000000000000000 ) ) ;
#68782 = CARTESIAN_POINT ( 'NONE',  ( 86.24777464318049169, -57.57757783600133195, 202.8079723600879163 ) ) ;
#68783 = CARTESIAN_POINT ( 'NONE',  ( 7.996668423981797780, 47.99999999999999289, -78.85453280025083700 ) ) ;
#68784 = EDGE_CURVE ( 'NONE', #23042, #39006, #66960, .T. ) ;
#68785 = CARTESIAN_POINT ( 'NONE',  ( 36.00270731313416661, -31.67306530563417155, -37.80042584635362601 ) ) ;
#68786 = CARTESIAN_POINT ( 'NONE',  ( -16.12882272094105218, 21.28108484451415094, -2.990375924008328745 ) ) ;
#68787 = CARTESIAN_POINT ( 'NONE',  ( 0.000000000000000000, 69.00000000000000000, 0.000000000000000000 ) ) ;
#68788 = CARTESIAN_POINT ( 'NONE',  ( -59.99645216862890607, -59.99999999999999289, 100.5209178649575961 ) ) ;
#68789 = DIRECTION ( 'NONE',  ( 0.000000000000000000, 1.000000000000000000, 0.000000000000000000 ) ) ;
#68790 = CIRCLE ( 'NONE', #65302, 5.000000000000001776 ) ;
#68791 = CARTESIAN_POINT ( 'NONE',  ( -85.42895892553163151, -50.19694353309194668, 189.9724354759997311 ) ) ;
#68792 = ORIENTED_EDGE ( 'NONE', *, *, #91136, .F. ) ;
#68793 = CARTESIAN_POINT ( 'NONE',  ( -43.00000000000002842, 461.4080316921935605, 3.462976341553847259 ) ) ;
#68794 = CARTESIAN_POINT ( 'NONE',  ( -2.007454225884796717, -35.99435325406362551, 29.88636456374760186 ) ) ;
#68795 = CARTESIAN_POINT ( 'NONE',  ( -6.492510984469592294, 41.78432685485347520, -59.03546988472429291 ) ) ;
#68796 = CARTESIAN_POINT ( 'NONE',  ( 32.82691535583474973, 485.1045372766795367, 1.724905475515037701 ) ) ;
#68797 =( BOUNDED_SURFACE ( )  B_SPLINE_SURFACE ( 3, 2, ( 
 ( #18836, #36089, #17745 ),
 ( #51144, #101316, #27465 ),
 ( #51681, #26929, #2062 ),
 ( #76489, #18289, #59802 ) ),
 .UNSPECIFIED., .F., .F., .F. ) 
 B_SPLINE_SURFACE_WITH_KNOTS ( ( 4, 4 ),
 ( 3, 3 ),
 ( -1.347446459964984911E-15, 0.0002182297367799811963 ),
 ( 0.000000000000000000, 1.000000000000000000 ),
 .UNSPECIFIED. ) 
 GEOMETRIC_REPRESENTATION_ITEM ( )  RATIONAL_B_SPLINE_SURFACE ( (
 ( 1.000000000000000000, 0.8274831119534725721, 1.000000000000000000),
 ( 1.000000000000000000, 0.8286506196641503230, 1.000000000000000000),
 ( 1.000000000000000000, 0.8297675374346515920, 1.000000000000000000),
 ( 1.000000000000000000, 0.8308329163124033023, 1.000000000000000000) ) ) 
 REPRESENTATION_ITEM ( '' )  SURFACE ( )  );
#68800 = EDGE_CURVE ( 'NONE', #53725, #6335, #84279, .T. ) ;
#68799 = DIRECTION ( 'NONE',  ( -1.000000000000000000, -0.000000000000000000, -0.000000000000000000 ) ) ;
#68798 = CARTESIAN_POINT ( 'NONE',  ( -25.05812948974611132, 295.6566298158938366, 2.109544210833623090 ) ) ;
#68801 = EDGE_LOOP ( 'NONE', ( #10786, #68713, #85542, #56152 ) ) ;
#68802 = B_SPLINE_CURVE_WITH_KNOTS ( 'NONE', 3,
 ( #101259, #42469, #59208, #76966, #50547, #9032 ),
 .UNSPECIFIED., .F., .F.,
 ( 4, 2, 4 ),
 ( 0.003841072314098338547, 0.005765657563962176858, 0.007690242813826015170 ),
 .UNSPECIFIED. ) ;
#68803 = CARTESIAN_POINT ( 'NONE',  ( 20.77592568779148863, 1.482358050883964840E-15, 0.000000000000000000 ) ) ;
#68804 = AXIS2_PLACEMENT_3D ( 'NONE', #59865, #35606, #43133 ) ;
#68805 = CARTESIAN_POINT ( 'NONE',  ( 0.3334354129020682400, 27.31151862705754141, 40.70764297020699019 ) ) ;
#68806 = DIRECTION ( 'NONE',  ( 0.000000000000000000, -1.000000000000000000, 0.000000000000000000 ) ) ;
#68807 = CARTESIAN_POINT ( 'NONE',  ( 26.38526321989008139, 295.9613804530332004, -9.761259522514095011 ) ) ;
#68808 = CARTESIAN_POINT ( 'NONE',  ( 35.74483125092430669, 413.6409941285803598, 6.029078300230034770 ) ) ;
#68809 = AXIS2_PLACEMENT_3D ( 'NONE', #47697, #95741, #61807 ) ;
#68810 = CARTESIAN_POINT ( 'NONE',  ( 103.2975989548790494, -14.21045842199431064, 133.3107955441116985 ) ) ;
#68811 = CARTESIAN_POINT ( 'NONE',  ( -79.16567614127620800, -49.90816960768657395, 152.0318120169229985 ) ) ;
#68812 = ORIENTED_EDGE ( 'NONE', *, *, #29407, .T. ) ;
#68813 = CARTESIAN_POINT ( 'NONE',  ( 5.980543423763066357, 253.9709640750106985, -0.5500789318242854664 ) ) ;
#68814 = CARTESIAN_POINT ( 'NONE',  ( 52.71793837654925596, -57.67618728593465960, 84.69386162797044904 ) ) ;
#68815 = CARTESIAN_POINT ( 'NONE',  ( -4.406842699996125212, 6.115962218725286448, 2.334422802632851734E-15 ) ) ;
#68816 = CARTESIAN_POINT ( 'NONE',  ( 44.28689199344569971, 335.5423528813348639, -0.1654540242942443840 ) ) ;
#68817 = ADVANCED_FACE ( 'NONE', ( #26617 ), #106587, .T. ) ;
#68818 = AXIS2_PLACEMENT_3D ( 'NONE', #39215, #71030, #13843 ) ;
#68819 = DIRECTION ( 'NONE',  ( 0.000000000000000000, -1.000000000000000000, 0.000000000000000000 ) ) ;
#68820 = EDGE_LOOP ( 'NONE', ( #90013, #8154, #26089, #91498, #96585, #104931 ) ) ;
#68821 = UNCERTAINTY_MEASURE_WITH_UNIT (LENGTH_MEASURE( 1.000000000000000082E-05 ), #16828, 'distance_accuracy_value', 'NONE');
#68822 = CARTESIAN_POINT ( 'NONE',  ( 4.079861200793539311, 53.97863311128789121, -7.631710309917290935 ) ) ;
#68823 = CARTESIAN_POINT ( 'NONE',  ( 31.43208348565381627, 438.4707862388070794, 22.17802677910626841 ) ) ;
#68824 = CARTESIAN_POINT ( 'NONE',  ( 7.188101187499999156, -29.75000000204838813, 2.977408999572654924 ) ) ;
#68825 = ORIENTED_EDGE ( 'NONE', *, *, #72528, .T. ) ;
#68826 =( LENGTH_UNIT ( ) NAMED_UNIT ( * ) SI_UNIT ( .MILLI., .METRE. ) );
#68828 = ADVANCED_FACE ( 'NONE', ( #99921 ), #39475, .T. ) ;
#68827 = CARTESIAN_POINT ( 'NONE',  ( -3.826949319562310325, 15.99999999999999645, 9.246271506234595705 ) ) ;
#68829 = CARTESIAN_POINT ( 'NONE',  ( 6.335691922401378129, 41.93068719163046154, -69.89754162678619309 ) ) ;
#68830 = CARTESIAN_POINT ( 'NONE',  ( 54.34415824577756382, 50.00000000000000000, -32.38913437803500983 ) ) ;
#68831 = DIRECTION ( 'NONE',  ( 0.000000000000000000, 0.000000000000000000, -1.000000000000000000 ) ) ;
#68832 = VERTEX_POINT ( 'NONE', #102046 ) ;
#68833 = CARTESIAN_POINT ( 'NONE',  ( 76.22636411394974232, -60.00000000000002132, -29.93832294592251131 ) ) ;
#68835 = CARTESIAN_POINT ( 'NONE',  ( 19.02302005367418758, -39.47349632058700308, 30.89158363994719281 ) ) ;
#68834 = CARTESIAN_POINT ( 'NONE',  ( -69.92584042677506773, -30.00000000000002842, 127.5397447585766599 ) ) ;
#68836 = AXIS2_PLACEMENT_3D ( 'NONE', #36024, #68898, #27937 ) ;
#68837 = CARTESIAN_POINT ( 'NONE',  ( 55.68167212273443312, 51.11204936430952017, 27.84083606136722722 ) ) ;
#68838 = CARTESIAN_POINT ( 'NONE',  ( -35.05923457201825499, -25.64776234952272560, 32.62731220559753353 ) ) ;
#68839 = UNCERTAINTY_MEASURE_WITH_UNIT (LENGTH_MEASURE( 1.000000000000000082E-05 ), #61167, 'distance_accuracy_value', 'NONE');
#68840 = ORIENTED_EDGE ( 'NONE', *, *, #12344, .F. ) ;
#68841 = DIRECTION ( 'NONE',  ( 0.000000000000000000, 0.000000000000000000, 1.000000000000000000 ) ) ;
#68842 =( LENGTH_UNIT ( ) NAMED_UNIT ( * ) SI_UNIT ( .MILLI., .METRE. ) );
#68843 = CARTESIAN_POINT ( 'NONE',  ( -13.44288011066907096, -55.29289060621445628, 30.91149535780206747 ) ) ;
#68844 = AXIS2_PLACEMENT_3D ( 'NONE', #101066, #10453, #60637 ) ;
#68845 =( LENGTH_UNIT ( ) NAMED_UNIT ( * ) SI_UNIT ( .MILLI., .METRE. ) );
#68846 = CARTESIAN_POINT ( 'NONE',  ( 7.045965687440312486, -63.69607536213965915, 3.790395326974321133 ) ) ;
#68847 = CARTESIAN_POINT ( 'NONE',  ( 12.23997345424373506, -2.653384265557077626, 20.68770798023725987 ) ) ;
#68848 = ORIENTED_EDGE ( 'NONE', *, *, #5247, .T. ) ;
#68849 = CARTESIAN_POINT ( 'NONE',  ( -16.34245632501147583, 37.19060558336133937, -21.87293403489680088 ) ) ;
#68850 = ORIENTED_EDGE ( 'NONE', *, *, #81930, .T. ) ;
#68851 = CARTESIAN_POINT ( 'NONE',  ( 92.90552581771817131, -29.99999999999993960, 191.0990075023869394 ) ) ;
#68852 = CARTESIAN_POINT ( 'NONE',  ( -12.26692696938333782, 5.750203097402547314, -8.488608934173381471 ) ) ;
#68853 = UNCERTAINTY_MEASURE_WITH_UNIT (LENGTH_MEASURE( 1.000000000000000082E-05 ), #72048, 'distance_accuracy_value', 'NONE');
#68854 = ADVANCED_FACE ( 'NONE', ( #75100 ), #10895, .T. ) ;
#68855 = CARTESIAN_POINT ( 'NONE',  ( 35.58361799548379167, 3.851859888774471706E-31, 5.000000000000001776 ) ) ;
#68856 = CARTESIAN_POINT ( 'NONE',  ( 80.78006440248529429, -30.00000000000000000, 9.594317255054795268 ) ) ;
#68857 = CARTESIAN_POINT ( 'NONE',  ( -22.70225368124910759, 304.4484656627207073, 10.06577508047792691 ) ) ;
#68858 = VERTEX_POINT ( 'NONE', #58950 ) ;
#68859 = AXIS2_PLACEMENT_3D ( 'NONE', #27855, #29441, #69864 ) ;
#68860 = ORIENTED_EDGE ( 'NONE', *, *, #103803, .T. ) ;
#68861 = ORIENTED_EDGE ( 'NONE', *, *, #77459, .F. ) ;
#68863 = MECHANICAL_DESIGN_GEOMETRIC_PRESENTATION_REPRESENTATION (  '', ( #8532 ), #10232 ) ;
#68862 = CARTESIAN_POINT ( 'NONE',  ( -46.92822048327052897, 13.65838325462196323, -15.00718171297879344 ) ) ;
#68864 = SURFACE_SIDE_STYLE ('',( #35990 ) ) ;
#68865 = DIRECTION ( 'NONE',  ( -1.000000000000000000, -1.224606353822377258E-16, -0.000000000000000000 ) ) ;
#68866 = CARTESIAN_POINT ( 'NONE',  ( 4.814352310392309597, -11.79678594103575762, -3.583053941560742306 ) ) ;
#68867 = CARTESIAN_POINT ( 'NONE',  ( -17.73049404743309410, 43.18361977675543528, -6.030632858976519906 ) ) ;
#68868 = DIRECTION ( 'NONE',  ( 0.000000000000000000, 1.000000000000000000, 0.000000000000000000 ) ) ;
#68869 = FACE_OUTER_BOUND ( 'NONE', #6234, .T. ) ;
#68871 = ORIENTED_EDGE ( 'NONE', *, *, #77719, .F. ) ;
#68870 = CONICAL_SURFACE ( 'NONE', #58534, 5.999999999999998224, 0.7853981633974509435 ) ;
#68872 = CARTESIAN_POINT ( 'NONE',  ( 1.570796324980112679, 50.00000000000000000, -97.00000000000000000 ) ) ;
#68873 = ORIENTED_EDGE ( 'NONE', *, *, #17076, .F. ) ;
#68874 = CARTESIAN_POINT ( 'NONE',  ( -4.656390720430120922, -63.68353814039456751, 3.786082374785837867 ) ) ;
#68875 = CARTESIAN_POINT ( 'NONE',  ( 70.17483447761377136, -38.33017349177596600, 135.4944106953618075 ) ) ;
#68876 = CARTESIAN_POINT ( 'NONE',  ( -32.93292175078001804, 485.0466323666404378, 1.209345195306022802 ) ) ;
#68877 = CARTESIAN_POINT ( 'NONE',  ( 27.42231666649601962, 296.7076166580016547, 10.34122299797418698 ) ) ;
#68878 = CIRCLE ( 'NONE', #60265, 4.000000000000000888 ) ;
#68879 = CARTESIAN_POINT ( 'NONE',  ( -4.503026011213022706, 249.4565813771667990, 3.965236350746923488 ) ) ;
#68880 = VERTEX_POINT ( 'NONE', #100989 ) ;
#68881 = CARTESIAN_POINT ( 'NONE',  ( -6.145467199749145237, -3.000000000000002665, -92.99666842398180222 ) ) ;
#68882 = DIRECTION ( 'NONE',  ( 0.000000000000000000, 0.000000000000000000, 1.000000000000000000 ) ) ;
#68883 = FACE_OUTER_BOUND ( 'NONE', #12657, .T. ) ;
#68884 = AXIS2_PLACEMENT_3D ( 'NONE', #88854, #40295, #46274 ) ;
#68885 = EDGE_CURVE ( 'NONE', #36374, #54423, #42216, .T. ) ;
#68886 = LINE ( 'NONE', #21934, #87697 ) ;
#68887 = ORIENTED_EDGE ( 'NONE', *, *, #18813, .T. ) ;
#68888 = AXIS2_PLACEMENT_3D ( 'NONE', #46585, #6650, #78951 ) ;
#68889 = CARTESIAN_POINT ( 'NONE',  ( 7.999885325681428405, -88.99977065129938580, 0.2682325777720067084 ) ) ;
#68890 =( NAMED_UNIT ( * ) SI_UNIT ( $, .STERADIAN. ) SOLID_ANGLE_UNIT ( ) );
#68891 = CARTESIAN_POINT ( 'NONE',  ( -43.47770857297121694, 484.8227827122652229, 4.253339224812703101 ) ) ;
#68892 = DIRECTION ( 'NONE',  ( 1.000000000000000000, -0.000000000000000000, -0.000000000000000000 ) ) ;
#68893 = EDGE_CURVE ( 'NONE', #94793, #7449, #60557, .T. ) ;
#68894 =( NAMED_UNIT ( * ) SI_UNIT ( $, .STERADIAN. ) SOLID_ANGLE_UNIT ( ) );
#68895 = AXIS2_PLACEMENT_3D ( 'NONE', #98255, #24408, #57247 ) ;
#68896 = CARTESIAN_POINT ( 'NONE',  ( 4.424031367839869944, 4.951337798340052387, -6.056431503346638046 ) ) ;
#68897 = CARTESIAN_POINT ( 'NONE',  ( 86.44384447875494004, -17.06518992601345275, 183.2574884712147139 ) ) ;
#68898 = DIRECTION ( 'NONE',  ( -1.000000000000000000, -1.224606353822377258E-16, -0.000000000000000000 ) ) ;
#68899 = CARTESIAN_POINT ( 'NONE',  ( -3.626860598991949125, 129.3176399044602931, 5.000000000000000888 ) ) ;
#68900 = EDGE_LOOP ( 'NONE', ( #101374, #95328, #45880, #3594 ) ) ;
#68901 = CARTESIAN_POINT ( 'NONE',  ( 2.807699812566442521, -57.67114347947145347, -44.61185890016353284 ) ) ;
#68902 = CARTESIAN_POINT ( 'NONE',  ( 8.125792988224667113, -15.92269399258319851, -34.96259303599431689 ) ) ;
#68903 = LINE ( 'NONE', #11153, #45293 ) ;
#68904 = CARTESIAN_POINT ( 'NONE',  ( 29.08076923076923137, 4.172000000000003261, 0.000000000000000000 ) ) ;
#68905 = CARTESIAN_POINT ( 'NONE',  ( 5.000000000000000000, -13.82968113844978220, 11.07308787588975285 ) ) ;
#68906 = CARTESIAN_POINT ( 'NONE',  ( -82.07453358999418924, -30.00000000000000000, 34.72976722373532255 ) ) ;
#68907 = CARTESIAN_POINT ( 'NONE',  ( 23.58349330513380337, 1.593028355512270962E-15, 0.000000000000000000 ) ) ;
#68908 = CARTESIAN_POINT ( 'NONE',  ( 4.154708322984369194E-08, -57.67120202538961138, 41.61186700422869933 ) ) ;
#68909 = CIRCLE ( 'NONE', #46482, 15.00000000000001421 ) ;
#68910 = CARTESIAN_POINT ( 'NONE',  ( -9.253817200599856463, 248.7000727008313277, -3.791916801615155208 ) ) ;
#68911 = EDGE_CURVE ( 'NONE', #68447, #81401, #34702, .T. ) ;
#68912 = CARTESIAN_POINT ( 'NONE',  ( 6.966966640339024686, -46.95039021837323645, 39.14360059807137304 ) ) ;
#68913 = CARTESIAN_POINT ( 'NONE',  ( -15.00532868743633230, -22.79648478323108662, 27.82648325657085664 ) ) ;
#68914 = CARTESIAN_POINT ( 'NONE',  ( 14.62196750106410015, 42.00000000000002132, -88.48477917736602194 ) ) ;
#68915 = CARTESIAN_POINT ( 'NONE',  ( 6.106896958092508321, -4.373166921188613721, -16.80698729315718865 ) ) ;
#68916 = CARTESIAN_POINT ( 'NONE',  ( 41.43589798968741889, 484.8608061051571667, -3.494608281236457614 ) ) ;
#68917 = CARTESIAN_POINT ( 'NONE',  ( 42.59497354870452313, -25.61862108974249708, -29.74171580790378044 ) ) ;
#68918 = ADVANCED_FACE ( 'NONE', ( #83730 ), #27148, .T. ) ;
#68919 = CARTESIAN_POINT ( 'NONE',  ( -21.99509306790069729, -22.07688988618103920, 28.30121125513787561 ) ) ;
#68920 = ORIENTED_EDGE ( 'NONE', *, *, #5855, .T. ) ;
#68921 = CARTESIAN_POINT ( 'NONE',  ( 40.02990647470488028, 485.1981161833907095, -4.348266463183992236 ) ) ;
#68922 = CARTESIAN_POINT ( 'NONE',  ( -16.01663249378604803, -60.36515267375860816, 34.15509718080474499 ) ) ;
#68925 = EDGE_CURVE ( 'NONE', #82896, #19223, #10374, .T. ) ;
#68924 = CARTESIAN_POINT ( 'NONE',  ( -3.311033882356798252E-14, 37.21016666119783167, -27.24999999999961986 ) ) ;
#68923 = FILL_AREA_STYLE ('',( #86178 ) ) ;
#68926 = VERTEX_POINT ( 'NONE', #60034 ) ;
#68927 = CIRCLE ( 'NONE', #36239, 4.000000000000007105 ) ;
#68928 = B_SPLINE_CURVE_WITH_KNOTS ( 'NONE', 3,
 ( #59284, #92161, #77048, #52233, #43095, #85142, #11235, #3164, #60883, #36109, #101854, #53829, #96435, #78110, #63539, #31192, #53313, #61956, #37162, #54880, #71079, #94848 ),
 .UNSPECIFIED., .F., .F.,
 ( 4, 2, 2, 2, 2, 2, 2, 2, 2, 2, 4 ),
 ( 0.007230059716208242504, 0.007733998775341412342, 0.008237937834474582180, 0.008741876893607751151, 0.009245815952740921856, 0.009749755011874090826, 0.01000172454144068052, 0.01025369407100727021, 0.01050566360057385989, 0.01075763313014044958, 0.01126157218927362549 ),
 .UNSPECIFIED. ) ;
#68929 = FACE_OUTER_BOUND ( 'NONE', #15224, .T. ) ;
#68930 = VERTEX_POINT ( 'NONE', #52428 ) ;
#68931 = LINE ( 'NONE', #14364, #92974 ) ;
#68932 = CIRCLE ( 'NONE', #86187, 15.00000000000000711 ) ;
#68933 = CARTESIAN_POINT ( 'NONE',  ( 15.13200660511079754, 3.596720279097880724, 4.250825932782807293 ) ) ;
#68934 = CARTESIAN_POINT ( 'NONE',  ( -43.52560603733947886, 486.7876375777498197, 7.034422870327485811 ) ) ;
#68935 = VERTEX_POINT ( 'NONE', #92895 ) ;
#68936 = DIRECTION ( 'NONE',  ( -0.5735764363510497121, 0.8191520442889892450, 1.003171929053521665E-16 ) ) ;
#68937 = CARTESIAN_POINT ( 'NONE',  ( 102.5259657431785456, -45.28272343595455141, 187.4750528580337345 ) ) ;
#68938 = CARTESIAN_POINT ( 'NONE',  ( -7.897196874019792645, -6.208727958321951235, -1.302055520192089366 ) ) ;
#68939 = B_SPLINE_CURVE_WITH_KNOTS ( 'NONE', 3,
 ( #73137, #41854, #98489, #82313, #88818, #14913, #40792, #55883, #49943, #81236 ),
 .UNSPECIFIED., .F., .F.,
 ( 4, 2, 2, 2, 4 ),
 ( 0.000000000000000000, 0.0008124082233778996513, 0.001624816446755799303, 0.002437224670133698954, 0.003249632893511598605 ),
 .UNSPECIFIED. ) ;
#68940 = ADVANCED_FACE ( 'NONE', ( #19057 ), #53254, .T. ) ;
#68941 = ORIENTED_EDGE ( 'NONE', *, *, #1640, .F. ) ;
#68942 =( GEOMETRIC_REPRESENTATION_CONTEXT ( 3 ) GLOBAL_UNCERTAINTY_ASSIGNED_CONTEXT ( ( #2477 ) ) GLOBAL_UNIT_ASSIGNED_CONTEXT ( ( #87426, #7004, #22704 ) ) REPRESENTATION_CONTEXT ( 'NONE', 'WORKASPACE' ) );
#68943 = ORIENTED_EDGE ( 'NONE', *, *, #342, .T. ) ;
#68944 = VERTEX_POINT ( 'NONE', #77789 ) ;
#68945 = CARTESIAN_POINT ( 'NONE',  ( 23.32412973071527773, 304.7201357075585406, 10.12579726553843962 ) ) ;
#68946 = AXIS2_PLACEMENT_3D ( 'NONE', #99453, #57933, #75175 ) ;
#68947 = EDGE_CURVE ( 'NONE', #68926, #40910, #92888, .T. ) ;
#68948 = CARTESIAN_POINT ( 'NONE',  ( 0.000000000000000000, -54.00000000000000711, 27.00000000000000000 ) ) ;
#68949 =( NAMED_UNIT ( * ) SI_UNIT ( $, .STERADIAN. ) SOLID_ANGLE_UNIT ( ) );
#68950 = ORIENTED_EDGE ( 'NONE', *, *, #49364, .T. ) ;
#68951 = CARTESIAN_POINT ( 'NONE',  ( 0.5805565836007602343, 3.752776749732561257, -6.499999999999999112 ) ) ;
#68952 = CARTESIAN_POINT ( 'NONE',  ( -6.335691858987115843, 41.93068706802236534, -69.89754241407730717 ) ) ;
#68953 = FACE_OUTER_BOUND ( 'NONE', #93757, .T. ) ;
#68954 = CARTESIAN_POINT ( 'NONE',  ( -69.57556824456027300, -60.00000000001938361, -35.22474675930589427 ) ) ;
#68955 = AXIS2_PLACEMENT_3D ( 'NONE', #29784, #6514, #80938 ) ;
#68956 = CARTESIAN_POINT ( 'NONE',  ( 29.98176661990081371, 1.340359594676612611E-15, 0.000000000000000000 ) ) ;
#68957 = CARTESIAN_POINT ( 'NONE',  ( 6.683837171061802529, 3.955946848495958346, -6.851900933636989599 ) ) ;
#68958 = CARTESIAN_POINT ( 'NONE',  ( -6.810576809588133607, 41.35122479108419213, -58.50275420946741889 ) ) ;
#68959 = CARTESIAN_POINT ( 'NONE',  ( -86.49433777984398830, -14.21045842199439946, 11.85125679505764928 ) ) ;
#68960 = EDGE_CURVE ( 'NONE', #102006, #6367, #103645, .T. ) ;
#68961 = FACE_OUTER_BOUND ( 'NONE', #9587, .T. ) ;
#68962 = CARTESIAN_POINT ( 'NONE',  ( -48.44050217894999832, -32.60199816967398334, 46.13225639932870337 ) ) ;
#68963 = AXIS2_PLACEMENT_3D ( 'NONE', #47589, #71872, #104778 ) ;
#68964 = ORIENTED_EDGE ( 'NONE', *, *, #5996, .F. ) ;
#68965 = CARTESIAN_POINT ( 'NONE',  ( -12.13034742782427955, 48.00000000000000000, -93.82352941176471006 ) ) ;
#68966 = ORIENTED_EDGE ( 'NONE', *, *, #25370, .F. ) ;
#68967 = CARTESIAN_POINT ( 'NONE',  ( -7.697757149361867945, 296.0912719809052760, -10.02629731371196264 ) ) ;
#68968 = CARTESIAN_POINT ( 'NONE',  ( 6.466227039643102081, 2.668354129823723664, 6.840182550749403845 ) ) ;
#68969 = ORIENTED_EDGE ( 'NONE', *, *, #6746, .F. ) ;
#68970 = SURFACE_STYLE_FILL_AREA ( #3156 ) ;
#68971 = VERTEX_POINT ( 'NONE', #94519 ) ;
#68972 = CARTESIAN_POINT ( 'NONE',  ( 89.93155271925053285, -30.00000000000346745, -2.506699656231715867 ) ) ;
#68973 = CARTESIAN_POINT ( 'NONE',  ( -2.352990130084491319E-16, 8.660254037844390851, -7.422398894150036064 ) ) ;
#68974 = FACE_OUTER_BOUND ( 'NONE', #69467, .T. ) ;
#68975 = CARTESIAN_POINT ( 'NONE',  ( 7.040971602393473638, 41.74416448739698637, -59.82830749617803434 ) ) ;
#68976 = CARTESIAN_POINT ( 'NONE',  ( -19.32152200348980742, 18.64316884709133504, -33.52312678235660570 ) ) ;
#68977 = CARTESIAN_POINT ( 'NONE',  ( 87.06181006619939922, -30.00000000000000000, 183.9460334166788016 ) ) ;
#68978 = CARTESIAN_POINT ( 'NONE',  ( -11.29926588360462603, 43.19537255330742198, -14.89485451155379359 ) ) ;
#68979 = LINE ( 'NONE', #59821, #7061 ) ;
#68980 = B_SPLINE_CURVE_WITH_KNOTS ( 'NONE', 3,
 ( #99754, #2641, #9135, #60386, #43118, #18882, #27510, #28037, #36134, #44184, #76004, #35587, #101877, #1569, #100282, #26443, #93797, #93263, #51725, #59310, #83043, #35054 ),
 .UNSPECIFIED., .F., .F.,
 ( 4, 2, 2, 2, 2, 2, 2, 2, 2, 2, 4 ),
 ( 0.003198323314689233317, 0.003450306839784169494, 0.003702290364879106104, 0.004206257415068978892, 0.004710224465258851245, 0.005214191515448723599, 0.006222125615828478715, 0.006474109140923419228, 0.006726092666018360609, 0.006978076191113301990, 0.007230059716208242504 ),
 .UNSPECIFIED. ) ;
#68981 = ORIENTED_EDGE ( 'NONE', *, *, #72650, .T. ) ;
#68982 = VERTEX_POINT ( 'NONE', #20669 ) ;
#68983 = CARTESIAN_POINT ( 'NONE',  ( 53.79279109633859690, -29.09796998240493693, 53.78371313197352777 ) ) ;
#68984 = CARTESIAN_POINT ( 'NONE',  ( 6.670526534797884821, 41.45458331230783244, -58.55661123927227862 ) ) ;
#68985 = DIRECTION ( 'NONE',  ( -1.000000000000000000, -0.000000000000000000, -0.000000000000000000 ) ) ;
#68986 = ORIENTED_EDGE ( 'NONE', *, *, #18862, .T. ) ;
#68987 = CARTESIAN_POINT ( 'NONE',  ( -91.45622412403105272, -38.38807348690984611, -7.605349006447526428 ) ) ;
#68988 = AXIS2_PLACEMENT_3D ( 'NONE', #59297, #58215, #9648 ) ;
#68989 = ORIENTED_EDGE ( 'NONE', *, *, #54768, .F. ) ;
#68990 = FILL_AREA_STYLE ('',( #102399 ) ) ;
#68991 = CARTESIAN_POINT ( 'NONE',  ( 108.2517700566951646, -38.35773586447793804, 192.2691011081020349 ) ) ;
#68992 = CARTESIAN_POINT ( 'NONE',  ( 11.80622600566693770, 16.45187812399441896, 9.389573745708821306 ) ) ;
#68993 = CARTESIAN_POINT ( 'NONE',  ( 82.59045073928865577, -37.86127578031408802, 5.516604945292076678 ) ) ;
#68994 = CARTESIAN_POINT ( 'NONE',  ( 40.24508711046470921, 341.7448991600085151, 21.01852089427141124 ) ) ;
#68995 = DIRECTION ( 'NONE',  ( 0.000000000000000000, -1.000000000000000000, 0.000000000000000000 ) ) ;
#68996 = CARTESIAN_POINT ( 'NONE',  ( 6.934100574218750701, -13.60622170955989141, -6.341742298311421777 ) ) ;
#68997 = CARTESIAN_POINT ( 'NONE',  ( 6.338278980374460581, -2.729992536301357742, 6.499999999999423572 ) ) ;
#68998 = CARTESIAN_POINT ( 'NONE',  ( -44.33427973454566029, 435.2106362794498295, 13.55537084937450665 ) ) ;
#68999 = CARTESIAN_POINT ( 'NONE',  ( 7.869427812660434896, 64.69537499111491741, 4.999999999992629895 ) ) ;
#69000 = ORIENTED_EDGE ( 'NONE', *, *, #91279, .T. ) ;
#69001 = EDGE_CURVE ( 'NONE', #23867, #17408, #71791, .T. ) ;
#69002 = CARTESIAN_POINT ( 'NONE',  ( 17.50000000000002842, 45.00000000000000711, 64.09953197936602010 ) ) ;
#69003 = CARTESIAN_POINT ( 'NONE',  ( 7.274972994441586849, 40.00000000291657187, -70.77553163430461325 ) ) ;
#69004 = CIRCLE ( 'NONE', #103476, 2.999999999999999112 ) ;
#69005 = CARTESIAN_POINT ( 'NONE',  ( -32.73339311437064936, 439.3386803523824824, 23.76693748282156804 ) ) ;
#69006 = ORIENTED_EDGE ( 'NONE', *, *, #63103, .F. ) ;
#69007 = DIRECTION ( 'NONE',  ( 0.000000000000000000, -1.000000000000000000, 0.000000000000000000 ) ) ;
#69008 = CARTESIAN_POINT ( 'NONE',  ( -37.78559634195402595, 315.0293482688398399, 14.83292048122523354 ) ) ;
#69009 = LINE ( 'NONE', #60393, #2003 ) ;
#69010 = CARTESIAN_POINT ( 'NONE',  ( 43.86650669486618881, 1.474610560812782335E-15, 0.000000000000000000 ) ) ;
#69011 = CARTESIAN_POINT ( 'NONE',  ( 5.656854249492378806, -23.18749999999999289, 5.656854249492381470 ) ) ;
#69012 =( NAMED_UNIT ( * ) PLANE_ANGLE_UNIT ( ) SI_UNIT ( $, .RADIAN. ) );
#69013 = EDGE_CURVE ( 'NONE', #62090, #21078, #106664, .T. ) ;
#69014 = VECTOR ( 'NONE', #42629, 1000.000000000000000 ) ;
#69015 = CYLINDRICAL_SURFACE ( 'NONE', #51907, 4.000000000000000000 ) ;
#69016 = ORIENTED_EDGE ( 'NONE', *, *, #77017, .F. ) ;
#69017 = CARTESIAN_POINT ( 'NONE',  ( 84.33010434533966304, -46.56536763441548743, 185.7282459068632932 ) ) ;
#69018 = DIRECTION ( 'NONE',  ( 1.000000000000000000, 1.224606353822377258E-16, 0.000000000000000000 ) ) ;
#69019 = CARTESIAN_POINT ( 'NONE',  ( -15.39894322001510574, 46.20524723896237163, 5.264004132386240542 ) ) ;
#69020 = ORIENTED_EDGE ( 'NONE', *, *, #88394, .T. ) ;
#69021 = CARTESIAN_POINT ( 'NONE',  ( -99.21263190360249951, -60.15509383132980048, 110.4768515106927396 ) ) ;
#69022 = CONICAL_SURFACE ( 'NONE', #67318, 4.000000000000007105, 0.9599310885968835860 ) ;
#69023 =( LENGTH_UNIT ( ) NAMED_UNIT ( * ) SI_UNIT ( .MILLI., .METRE. ) );
#69024 = CARTESIAN_POINT ( 'NONE',  ( 5.499265899522581158, -4.999999999985523580, -99.22427370007513048 ) ) ;
#69025 = CARTESIAN_POINT ( 'NONE',  ( 32.17646412119353272, 464.6980787822281513, 10.84896803613063021 ) ) ;
#69026 = CARTESIAN_POINT ( 'NONE',  ( -23.19062926906127231, -27.02661850035177693, -38.42076749808039438 ) ) ;
#69027 = AXIS2_PLACEMENT_3D ( 'NONE', #15104, #80899, #7008 ) ;
#69028 = EDGE_CURVE ( 'NONE', #79700, #33682, #104702, .T. ) ;
#69029 = AXIS2_PLACEMENT_3D ( 'NONE', #104978, #29023, #103385 ) ;
#69030 = CARTESIAN_POINT ( 'NONE',  ( 39.17414499517634852, -60.00000000000001421, 50.97255646505768567 ) ) ;
#69031 = CARTESIAN_POINT ( 'NONE',  ( 27.19894980877528567, -30.54737125749132787, 39.15565882474543713 ) ) ;
#69032 = CARTESIAN_POINT ( 'NONE',  ( 51.39917057842919945, -29.90070880694079136, 48.99695014035973628 ) ) ;
#69034 = CARTESIAN_POINT ( 'NONE',  ( -12.14245043011195335, 17.44669189061015047, 8.974181497934978324 ) ) ;
#69033 = CARTESIAN_POINT ( 'NONE',  ( 33.52734911656129668, 435.4192553323662764, 9.514907176917411391 ) ) ;
#69035 = VECTOR ( 'NONE', #21668, 1000.000000000000000 ) ;
#69036 = CARTESIAN_POINT ( 'NONE',  ( 8.269522720448799546, 294.6925646269233994, -5.661848168216897292 ) ) ;
#69037 = CARTESIAN_POINT ( 'NONE',  ( 44.43774958859658142, 337.2802145563449017, 0.2445019049555710311 ) ) ;
#69038 = CARTESIAN_POINT ( 'NONE',  ( 36.02979557281435063, 304.0160159841871064, 0.1093096093688138148 ) ) ;
#69039 = EDGE_LOOP ( 'NONE', ( #22967, #32860, #79173, #85145, #7186, #82103, #25888, #87233, #51384, #54296, #20473 ) ) ;
#69040 = CIRCLE ( 'NONE', #103291, 8.000000000000000000 ) ;
#69041 = CARTESIAN_POINT ( 'NONE',  ( 3.528928113779659093, -5.468125903023639545, -1.782684363745784063E-14 ) ) ;
#69042 =( LENGTH_UNIT ( ) NAMED_UNIT ( * ) SI_UNIT ( .MILLI., .METRE. ) );
#69043 = ORIENTED_EDGE ( 'NONE', *, *, #59820, .F. ) ;
#69044 = SURFACE_STYLE_FILL_AREA ( #58415 ) ;
#69045 = CARTESIAN_POINT ( 'NONE',  ( 5.982126593009819970, -61.02665772107069131, 0.5333292889181870944 ) ) ;
#69048 = EDGE_CURVE ( 'NONE', #96921, #66630, #45949, .T. ) ;
#69047 = CARTESIAN_POINT ( 'NONE',  ( -0.001384332131796172554, -60.22811001523060526, -36.92766828953757141 ) ) ;
#69046 = CARTESIAN_POINT ( 'NONE',  ( 9.253583916535195186, 251.2980390800503869, 3.792462592445548619 ) ) ;
#69049 = ORIENTED_EDGE ( 'NONE', *, *, #30809, .F. ) ;
#69050 = DIRECTION ( 'NONE',  ( -0.000000000000000000, -0.000000000000000000, 1.000000000000000000 ) ) ;
#69051 = CARTESIAN_POINT ( 'NONE',  ( -3.999995229665001428, -8.688226215992830959, 6.928205984420947594 ) ) ;
#69052 = ORIENTED_EDGE ( 'NONE', *, *, #15917, .T. ) ;
#69053 = AXIS2_PLACEMENT_3D ( 'NONE', #85950, #102641, #12021 ) ;
#69054 = DIRECTION ( 'NONE',  ( -1.000000000000000000, -1.224606353822377258E-16, -0.000000000000000000 ) ) ;
#69055 = CARTESIAN_POINT ( 'NONE',  ( 0.000000000000000000, 300.0000000000000000, 0.000000000000000000 ) ) ;
#69056 = CIRCLE ( 'NONE', #22581, 4.000000000000001776 ) ;
#69057 =( NAMED_UNIT ( * ) PLANE_ANGLE_UNIT ( ) SI_UNIT ( $, .RADIAN. ) );
#69058 = CARTESIAN_POINT ( 'NONE',  ( -92.21137906100017290, -60.00000000000002132, 2.742975087226245723 ) ) ;
#69059 = CARTESIAN_POINT ( 'NONE',  ( 27.02022815836235026, 1.340359594676612611E-15, 0.000000000000000000 ) ) ;
#69060 = DIRECTION ( 'NONE',  ( 0.000000000000000000, -1.000000000000000000, 0.000000000000000000 ) ) ;
#69061 = CARTESIAN_POINT ( 'NONE',  ( -9.819056950928635175, 294.6481068335448299, 1.893705519456528652 ) ) ;
#69062 = FACE_OUTER_BOUND ( 'NONE', #47293, .T. ) ;
#69064 = CARTESIAN_POINT ( 'NONE',  ( 15.90614609307868399, -3.157894736842107530, 14.66382285868950675 ) ) ;
#69063 = CARTESIAN_POINT ( 'NONE',  ( -7.996668422906619611, -3.000000000000002665, -78.85453279917568636 ) ) ;
#69065 = CARTESIAN_POINT ( 'NONE',  ( -85.11760744219132846, -22.05730720455698801, 161.9244985632302871 ) ) ;
#69066 = ORIENTED_EDGE ( 'NONE', *, *, #103844, .F. ) ;
#69067 = CARTESIAN_POINT ( 'NONE',  ( -39.71213755904588538, 490.7526980994967403, 11.81179577511689516 ) ) ;
#69068 = ORIENTED_EDGE ( 'NONE', *, *, #7083, .T. ) ;
#69069 = EDGE_LOOP ( 'NONE', ( #52642, #6019, #105157, #30204, #58925, #15519, #72145, #50355, #3040, #69523, #70102 ) ) ;
#69070 = CARTESIAN_POINT ( 'NONE',  ( 7.549954993183454199, -4.999999999999999112, -15.49602501671512833 ) ) ;
#69071 = EDGE_CURVE ( 'NONE', #46447, #98765, #60140, .T. ) ;
#69072 = CARTESIAN_POINT ( 'NONE',  ( 33.80022934467060480, 484.1533297400391120, 1.810399503708082003 ) ) ;
#69073 = EDGE_LOOP ( 'NONE', ( #98332, #61929, #35778, #93617, #7929 ) ) ;
#69074 = DIRECTION ( 'NONE',  ( 0.000000000000000000, 1.000000000000000000, 0.000000000000000000 ) ) ;
#69075 = CARTESIAN_POINT ( 'NONE',  ( -93.33808876947477984, -57.65441397348698160, -16.37300446327261128 ) ) ;
#69076 = CARTESIAN_POINT ( 'NONE',  ( -5.855777637195782148, -68.78106496758447008, -1.331220292256681592 ) ) ;
#69077 = CIRCLE ( 'NONE', #43192, 0.5000000000000000000 ) ;
#69078 = CARTESIAN_POINT ( 'NONE',  ( 0.7145311798163270778, 9.237604307034018802, 3.185620757954082679E-16 ) ) ;
#69079 = DIRECTION ( 'NONE',  ( -1.000000000000000000, -1.224606353822377258E-16, -0.000000000000000000 ) ) ;
#69080 = CARTESIAN_POINT ( 'NONE',  ( -13.38886880393120116, -53.47610516573492845, 31.09159242423791270 ) ) ;
#69081 = CARTESIAN_POINT ( 'NONE',  ( 33.00000000000000000, 488.8442721620235716, 4.433647275927634190 ) ) ;
#69082 = CARTESIAN_POINT ( 'NONE',  ( 89.06755727843562909, -14.21045842199420939, 44.45805076957166335 ) ) ;
#69083 = EDGE_CURVE ( 'NONE', #53314, #63428, #104925, .T. ) ;
#69084 = CARTESIAN_POINT ( 'NONE',  ( -83.30586888084981467, -14.21045842199414011, 194.5088339777059332 ) ) ;
#69085 = CARTESIAN_POINT ( 'NONE',  ( -53.47679039029645054, -60.31905840357084259, 65.32239846319221499 ) ) ;
#69086 = ORIENTED_EDGE ( 'NONE', *, *, #2942, .F. ) ;
#69087 = DIRECTION ( 'NONE',  ( 0.000000000000000000, -1.000000000000000000, 0.000000000000000000 ) ) ;
#69088 = EDGE_CURVE ( 'NONE', #70018, #23629, #5486, .T. ) ;
#69089 = ORIENTED_EDGE ( 'NONE', *, *, #90940, .T. ) ;
#69090 = CARTESIAN_POINT ( 'NONE',  ( -101.6861282671374624, -45.26497370855512514, 189.9345094133276746 ) ) ;
#69091 = CARTESIAN_POINT ( 'NONE',  ( 2.787519624836773513, -30.00000000000000711, 6.642210194323184602 ) ) ;
#69092 = ORIENTED_EDGE ( 'NONE', *, *, #96316, .T. ) ;
#69093 = CARTESIAN_POINT ( 'NONE',  ( 6.931554132376503752, -2.999999999999883649, -71.13906995425703883 ) ) ;
#69095 = AXIS2_PLACEMENT_3D ( 'NONE', #96768, #5100, #6675 ) ;
#69094 = CARTESIAN_POINT ( 'NONE',  ( -2.822539341787094980, -59.99999999999998579, 39.63907887523128437 ) ) ;
#69096 = CARTESIAN_POINT ( 'NONE',  ( -3.534854069000198162, -1.070477528868992723, 104.4405781011824956 ) ) ;
#69097 = CARTESIAN_POINT ( 'NONE',  ( -5.082755093536326818, -17.09375000204838813, 5.082755093536325042 ) ) ;
#69099 = ADVANCED_FACE ( 'NONE', ( #13558 ), #83557, .F. ) ;
#69098 = AXIS2_PLACEMENT_3D ( 'NONE', #8217, #72939, #71892 ) ;
#69100 = DIRECTION ( 'NONE',  ( -1.000000000000000000, -1.224606353822377258E-16, -0.000000000000000000 ) ) ;
#69101 = DIRECTION ( 'NONE',  ( -1.000000000000000000, -0.000000000000000000, -0.000000000000000000 ) ) ;
#69102 =( BOUNDED_SURFACE ( )  B_SPLINE_SURFACE ( 2, 3, ( 
 ( #89728, #64396, #25552, #65445 ),
 ( #23963, #90248, #72467, #57328 ),
 ( #74049, #48706, #25005, #57859 ) ),
 .UNSPECIFIED., .F., .F., .F. ) 
 B_SPLINE_SURFACE_WITH_KNOTS ( ( 3, 3 ),
 ( 4, 4 ),
 ( 0.000000000000000000, 1.000000000000000000 ),
 ( 0.01818793032717390401, 0.02264331519860534464 ),
 .UNSPECIFIED. ) 
 GEOMETRIC_REPRESENTATION_ITEM ( )  RATIONAL_B_SPLINE_SURFACE ( (
 ( 1.000000000000000000, 1.000000000000000000, 1.000000000000000000, 1.000000000000000000),
 ( 1.857142857142858317, 1.857142857142858317, 1.857142857142858317, 1.857142857142858317),
 ( 1.000000000000000000, 1.000000000000000000, 1.000000000000000000, 1.000000000000000000) ) ) 
 REPRESENTATION_ITEM ( '' )  SURFACE ( )  );
#69103 = CARTESIAN_POINT ( 'NONE',  ( -29.45362385905110969, 325.9253963054578662, 15.14270878922920716 ) ) ;
#69104 = CIRCLE ( 'NONE', #19251, 4.000000000000007105 ) ;
#69105 = CARTESIAN_POINT ( 'NONE',  ( -9.341113524656639910, 10.95974597718367249, 1.301042606982605124E-15 ) ) ;
#69106 = CARTESIAN_POINT ( 'NONE',  ( -15.66121600890969390, 45.99808261488237804, -6.197534896530083159 ) ) ;
#69107 = CARTESIAN_POINT ( 'NONE',  ( -30.60580106567836722, -56.85883406477462643, 36.44144671480716369 ) ) ;
#69108 = STYLED_ITEM ( 'NONE', ( #78179 ), #79642 ) ;
#69109 = CARTESIAN_POINT ( 'NONE',  ( 0.000000000000000000, -1.023477375540016387, 16.09658290236430389 ) ) ;
#69110 = CARTESIAN_POINT ( 'NONE',  ( 47.00049515621073937, -53.35381624944555057, 50.28993904774486623 ) ) ;
#69111 = FACE_OUTER_BOUND ( 'NONE', #21859, .T. ) ;
#69112 = COLOUR_RGB ( '', 0.09019608, 0.27058824, 0.51372549) ;
#69113 = CARTESIAN_POINT ( 'NONE',  ( -6.999999999999993783, -4.000000000000003553, 102.2532056551910387 ) ) ;
#69114 = CIRCLE ( 'NONE', #65706, 9.000000000000000000 ) ;
#69115 = CARTESIAN_POINT ( 'NONE',  ( -88.28417624129785679, -38.54991672500991484, 200.0595944994497870 ) ) ;
#69116 = ORIENTED_EDGE ( 'NONE', *, *, #77026, .T. ) ;
#69118 = CARTESIAN_POINT ( 'NONE',  ( 43.00000000000000000, 461.6622277975420729, 10.18145404766792161 ) ) ;
#69117 = DIRECTION ( 'NONE',  ( 0.000000000000000000, 0.000000000000000000, 1.000000000000000000 ) ) ;
#69119 = CARTESIAN_POINT ( 'NONE',  ( 13.26742752227355737, 3.866425058570867712, -6.913453055525036639 ) ) ;
#69120 = CARTESIAN_POINT ( 'NONE',  ( -18.96017730465335305, 49.36529653577810706, 62.00134825986546616 ) ) ;
#69121 = CARTESIAN_POINT ( 'NONE',  ( -7.173661105156260653, 41.42016048193522693, -58.97621011332057606 ) ) ;
#69122 = FACE_OUTER_BOUND ( 'NONE', #100138, .T. ) ;
#69123 = DIRECTION ( 'NONE',  ( 0.000000000000000000, -1.000000000000000000, 0.000000000000000000 ) ) ;
#69124 = CARTESIAN_POINT ( 'NONE',  ( -20.09607536593551558, 304.8434239371439389, 8.935218438115660078 ) ) ;
#69125 = CARTESIAN_POINT ( 'NONE',  ( 31.73457237641028073, 436.7287042522650609, 21.10271224642818666 ) ) ;
#69126 = CARTESIAN_POINT ( 'NONE',  ( 106.0955882055216080, -60.00000000000000711, 198.2014181196565801 ) ) ;
#69127 = CARTESIAN_POINT ( 'NONE',  ( 36.36650669486618881, 1.474610560812782335E-15, 0.000000000000000000 ) ) ;
#69128 = ORIENTED_EDGE ( 'NONE', *, *, #80508, .T. ) ;
#69129 = ADVANCED_FACE ( 'NONE', ( #32964 ), #6524, .F. ) ;
#69130 = CARTESIAN_POINT ( 'NONE',  ( 34.53191791165118474, 437.2926915873509301, 5.227229271292882729 ) ) ;
#69131 = MECHANICAL_DESIGN_GEOMETRIC_PRESENTATION_REPRESENTATION (  '', ( #7120 ), #84595 ) ;
#69132 = CARTESIAN_POINT ( 'NONE',  ( -80.03095223124314828, -29.99999999999999289, -13.76337047395467117 ) ) ;
#69133 = ORIENTED_EDGE ( 'NONE', *, *, #105991, .F. ) ;
#69135 = CARTESIAN_POINT ( 'NONE',  ( 5.299529629523134666, 19.77438493592522306, -39.01802436143358221 ) ) ;
#69134 = CARTESIAN_POINT ( 'NONE',  ( -88.40077111556168177, -38.54200826082194453, 200.1329272985095429 ) ) ;
#69136 = LINE ( 'NONE', #20088, #37374 ) ;
#69137 = CARTESIAN_POINT ( 'NONE',  ( 43.34934355818124629, 465.4850867214036612, 10.08239944467128346 ) ) ;
#69138 = DIRECTION ( 'NONE',  ( 0.000000000000000000, -1.000000000000000000, 0.000000000000000000 ) ) ;
#69139 = CARTESIAN_POINT ( 'NONE',  ( 7.188101187499999156, -10.62500000204838813, 2.977408999572654924 ) ) ;
#69140 = CIRCLE ( 'NONE', #60585, 5.000000000000001776 ) ;
#69141 = FILL_AREA_STYLE ('',( #60524 ) ) ;
#69142 = EDGE_CURVE ( 'NONE', #96238, #58987, #27426, .T. ) ;
#69143 = EDGE_CURVE ( 'NONE', #45319, #43284, #97135, .T. ) ;
#69144 = CONICAL_SURFACE ( 'NONE', #27971, 4.000000000000000000, 0.9599310885968912466 ) ;
#69145 = PRODUCT ( '9. Reciprocating Link', '9. Reciprocating Link', '', ( #39052 ) ) ;
#69146 = DIRECTION ( 'NONE',  ( 0.000000000000000000, -0.000000000000000000, 1.000000000000000000 ) ) ;
#69148 = VERTEX_POINT ( 'NONE', #48574 ) ;
#69147 = CARTESIAN_POINT ( 'NONE',  ( -32.22120753352774614, 464.6691781026585204, 10.60621122532632832 ) ) ;
#69149 = CARTESIAN_POINT ( 'NONE',  ( 85.95997101110781102, -18.45075829103920384, 165.1113332624142345 ) ) ;
#69150 = CARTESIAN_POINT ( 'NONE',  ( 5.000000000000000000, 6.123233995736766282E-16, -2.868028571428571372 ) ) ;
#69151 = CARTESIAN_POINT ( 'NONE',  ( 9.989113211954167681, 88.97299273548998144, 0.5334031035449028346 ) ) ;
#69152 = EDGE_LOOP ( 'NONE', ( #52764, #68393, #91652, #28392, #33687 ) ) ;
#69153 = CARTESIAN_POINT ( 'NONE',  ( 1.530808498934196254E-15, 0.000000000000000000, 12.00000000000003908 ) ) ;
#69154 = DIRECTION ( 'NONE',  ( -0.5735764363510510444, -0.8191520442889883569, 0.000000000000000000 ) ) ;
#69155 = CARTESIAN_POINT ( 'NONE',  ( 8.000000000000000000, -28.90624999999999645, -3.313708498984761164 ) ) ;
#69156 = CARTESIAN_POINT ( 'NONE',  ( 0.6249480602962063092, 13.29596660449504952, 51.58658030989757037 ) ) ;
#69157 = CARTESIAN_POINT ( 'NONE',  ( 7.477168027001042994, -0.5783290275783404821, 15.45228033502481146 ) ) ;
#69158 = ADVANCED_FACE ( 'NONE', ( #24867 ), #64265, .F. ) ;
#69159 = ORIENTED_EDGE ( 'NONE', *, *, #75805, .T. ) ;
#69160 = CIRCLE ( 'NONE', #22660, 7.500000000000003553 ) ;
#69161 = SHAPE_REPRESENTATION_RELATIONSHIP ( 'NONE' , 'NONE' ,  #62661, #7337 ) ;
#69162 = CARTESIAN_POINT ( 'NONE',  ( -6.548324412163373687, 297.0730707799401102, 7.562729261318960283 ) ) ;
#69163 = CARTESIAN_POINT ( 'NONE',  ( 1.196618058419959393E-20, 36.30024107553216339, -29.75000000000000355 ) ) ;
#69165 = EDGE_CURVE ( 'NONE', #3656, #86116, #40500, .T. ) ;
#69164 = CARTESIAN_POINT ( 'NONE',  ( 14.47547278523829739, 21.82816532775421337, 4.801868590621356070 ) ) ;
#69167 = FILL_AREA_STYLE_COLOUR ( '', #36090 ) ;
#69166 = CARTESIAN_POINT ( 'NONE',  ( 43.66727438528342020, 435.6676895479272389, 17.39383282232698136 ) ) ;
#69168 = CARTESIAN_POINT ( 'NONE',  ( -1.320432766682874540E-15, -24.03125000204838457, 7.188101187500000044 ) ) ;
#69169 = CARTESIAN_POINT ( 'NONE',  ( 16.15440707770680007, 294.5642616619309138, -10.06111921690162880 ) ) ;
#69170 = FACE_BOUND ( 'NONE', #25023, .T. ) ;
#69171 = DIRECTION ( 'NONE',  ( 1.000000000000000000, 1.224606353822377258E-16, 0.000000000000000000 ) ) ;
#69172 = EDGE_LOOP ( 'NONE', ( #66246, #62775, #11243, #24488 ) ) ;
#69174 = B_SPLINE_CURVE_WITH_KNOTS ( 'NONE', 3,
 ( #32494, #89643, #23877, #16818, #6050, #53, #15210, #57249, #90169, #24927, #57780, #6579, #97188, #7113, #14662, #41089, #106329, #40029, #80468, #64834, #64315, #89114 ),
 .UNSPECIFIED., .F., .F.,
 ( 4, 2, 2, 2, 2, 2, 2, 2, 2, 2, 4 ),
 ( 0.06722862433541047789, 0.06787642855568201683, 0.06852423277595354190, 0.06981984121649660591, 0.07046764543676813097, 0.07111544965703966992, 0.07241105809758273393, 0.07370666653812581182, 0.07500227497866887583, 0.07629788341921195371, 0.07759349185975501773 ),
 .UNSPECIFIED. ) ;
#69173 = AXIS2_PLACEMENT_3D ( 'NONE', #1991, #33333, #66201 ) ;
#69175 = CARTESIAN_POINT ( 'NONE',  ( -36.24853743861725519, 490.9518012583203586, 12.45319371584819379 ) ) ;
#69176 = CIRCLE ( 'NONE', #100182, 1.000000000000002442 ) ;
#69177 = CARTESIAN_POINT ( 'NONE',  ( -4.498984042742175227, 9.307284623892885023, -5.000000000000000000 ) ) ;
#69178 = SURFACE_SIDE_STYLE ('',( #20125 ) ) ;
#69179 = VERTEX_POINT ( 'NONE', #8121 ) ;
#69180 = AXIS2_PLACEMENT_3D ( 'NONE', #2562, #75931, #59768 ) ;
#69181 = CARTESIAN_POINT ( 'NONE',  ( 34.84533103728120551, 490.9263297235970072, 11.68229585404477611 ) ) ;
#69182 = CARTESIAN_POINT ( 'NONE',  ( 3.313708498984781592, -21.96875000409677270, 7.999999999999979572 ) ) ;
#69183 = CIRCLE ( 'NONE', #65700, 4.000000000000000888 ) ;
#69185 = CARTESIAN_POINT ( 'NONE',  ( 30.00000000000000000, 0.000000000000000000, 0.000000000000000000 ) ) ;
#69184 = STYLED_ITEM ( 'NONE', ( #32688 ), #74164 ) ;
#69186 =( NAMED_UNIT ( * ) PLANE_ANGLE_UNIT ( ) SI_UNIT ( $, .RADIAN. ) );
#69187 = CARTESIAN_POINT ( 'NONE',  ( 9.333079356992097786, 103.2216691992513091, 3.592383266237785477 ) ) ;
#69188 = SURFACE_STYLE_FILL_AREA ( #20134 ) ;
#69189 = CARTESIAN_POINT ( 'NONE',  ( -111.1411582638900200, -60.00000000000000000, 186.5650987214990266 ) ) ;
#69190 = PRESENTATION_STYLE_ASSIGNMENT (( #43303 ) ) ;
#69191 = DIRECTION ( 'NONE',  ( 1.000000000000000000, 0.000000000000000000, -0.000000000000000000 ) ) ;
#69192 = SURFACE_STYLE_FILL_AREA ( #52441 ) ;
#69193 = CARTESIAN_POINT ( 'NONE',  ( -45.29905483860081716, 480.9466865490944656, -2.171671249451534003 ) ) ;
#69194 = CARTESIAN_POINT ( 'NONE',  ( -82.39105173393342341, -53.57895264400556812, 183.5905530224347331 ) ) ;
#69195 = SURFACE_SIDE_STYLE ('',( #51383 ) ) ;
#69196 = ORIENTED_EDGE ( 'NONE', *, *, #68390, .F. ) ;
#69197 = CARTESIAN_POINT ( 'NONE',  ( 0.000000000000000000, 0.000000000000000000, -8.000000000000000000 ) ) ;
#69198 = EDGE_CURVE ( 'NONE', #34395, #8292, #41161, .T. ) ;
#69199 = CARTESIAN_POINT ( 'NONE',  ( 46.85000000000000142, 0.000000000000000000, 4.171999999999999709 ) ) ;
#69200 = CARTESIAN_POINT ( 'NONE',  ( -84.05233785748785635, -45.26991514358498847, 1.856990868721440480 ) ) ;
#69201 = AXIS2_PLACEMENT_3D ( 'NONE', #43196, #76611, #2182 ) ;
#69202 = DIRECTION ( 'NONE',  ( 0.000000000000000000, 0.000000000000000000, 1.000000000000000000 ) ) ;
#69203 = DIRECTION ( 'NONE',  ( -1.000000000000000000, -1.224606353822377258E-16, -0.000000000000000000 ) ) ;
#69204 = CARTESIAN_POINT ( 'NONE',  ( 2.849086893379675356, 81.66418373412562914, -5.000000000000000000 ) ) ;
#69205 = CARTESIAN_POINT ( 'NONE',  ( -6.022743854525172580, -12.63762613047084571, 12.76172509297431468 ) ) ;
#69206 = CARTESIAN_POINT ( 'NONE',  ( 55.65414010180120385, 42.00000000000000000, -72.41885610122511707 ) ) ;
#69207 = EDGE_CURVE ( 'NONE', #44531, #76218, #101447, .T. ) ;
#69208 = CARTESIAN_POINT ( 'NONE',  ( 55.43986775084101737, -14.21045842199435860, 70.80752230913886081 ) ) ;
#69209 = CARTESIAN_POINT ( 'NONE',  ( -0.000000000000000000, 60.76237703744687479, -11.80995232570204045 ) ) ;
#69210 = EDGE_CURVE ( 'NONE', #9645, #15128, #80330, .T. ) ;
#69211 = CARTESIAN_POINT ( 'NONE',  ( -76.02716361407355805, -14.21045842199433018, -24.18402117868763312 ) ) ;
#69212 = PRESENTATION_LAYER_ASSIGNMENT (  '', '', ( #95079 ) ) ;
#69213 = CARTESIAN_POINT ( 'NONE',  ( -65.92007518974624247, -60.34191306316107983, 100.3556483961110501 ) ) ;
#69214 = ORIENTED_EDGE ( 'NONE', *, *, #9585, .T. ) ;
#69215 = CARTESIAN_POINT ( 'NONE',  ( 78.81966326594580607, -14.21045842199438347, 187.8133603351751333 ) ) ;
#69216 = CARTESIAN_POINT ( 'NONE',  ( -28.75499683032297327, 40.83805150464743861, 58.36934873979967620 ) ) ;
#69217 = CARTESIAN_POINT ( 'NONE',  ( 5.615082869220882955, -57.67118258056662938, -44.55225991330173230 ) ) ;
#69218 = VERTEX_POINT ( 'NONE', #23826 ) ;
#69219 = CARTESIAN_POINT ( 'NONE',  ( 13.95281146043403098, -57.79492310796621979, 25.82616780902253950 ) ) ;
#69220 = CARTESIAN_POINT ( 'NONE',  ( -2.977408999572654480, -23.00000000204839523, 7.188101187499999156 ) ) ;
#69221 = CARTESIAN_POINT ( 'NONE',  ( -4.589925132946517827, -8.934739837074847202, 3.864926970398263162 ) ) ;
#69222 = ORIENTED_EDGE ( 'NONE', *, *, #28720, .F. ) ;
#69223 = CARTESIAN_POINT ( 'NONE',  ( 45.94900261086841198, 5.000000000000002665, 0.000000000000000000 ) ) ;
#69224 = ORIENTED_EDGE ( 'NONE', *, *, #39683, .F. ) ;
#69225 = CARTESIAN_POINT ( 'NONE',  ( -8.169585525225413036, 39.99999999999999289, -72.41994148081866456 ) ) ;
#69226 = CARTESIAN_POINT ( 'NONE',  ( 48.02835407290504577, 16.78162100668611956, -14.35535821593549954 ) ) ;
#69227 = CARTESIAN_POINT ( 'NONE',  ( -84.33588122351162042, -60.00000000000000000, -25.03827388917266106 ) ) ;
#69228 = FACE_BOUND ( 'NONE', #83547, .T. ) ;
#69229 = CARTESIAN_POINT ( 'NONE',  ( -3.594029361870008099, -9.156975552773349847, 6.225090491531445558 ) ) ;
#69230 = ADVANCED_FACE ( 'NONE', ( #81463 ), #96310, .T. ) ;
#69231 = DIRECTION ( 'NONE',  ( 0.5735764363510440500, 0.8191520442889932418, 0.000000000000000000 ) ) ;
#69233 = B_SPLINE_CURVE_WITH_KNOTS ( 'NONE', 3,
 ( #82062, #30498, #12684, #95226, #7632, #54198, #98256, #96295, #24409, #29974, #57248, #62862, #90167, #73970, #8182, #81511, #95747, #22419, #54730, #58879, #579, #2740 ),
 .UNSPECIFIED., .F., .F.,
 ( 4, 2, 2, 2, 2, 2, 2, 2, 2, 2, 4 ),
 ( 0.003159815893393695240, 0.003663154312159962872, 0.004166492730926230938, 0.004669831149692498136, 0.004921500359075634337, 0.005173169568458770538, 0.005676507987225038604, 0.005928177196608170468, 0.006179846405991303200, 0.006683184824757560857, 0.007186523243523819382 ),
 .UNSPECIFIED. ) ;
#69232 = FACE_OUTER_BOUND ( 'NONE', #52397, .T. ) ;
#69234 = CARTESIAN_POINT ( 'NONE',  ( -7.374560640988130800, 50.00000000000000000, -94.59600210748763516 ) ) ;
#69235 = CARTESIAN_POINT ( 'NONE',  ( -7.551437640244095029, 108.0087246252290498, -2.648272645923386737 ) ) ;
#69236 = CARTESIAN_POINT ( 'NONE',  ( 37.85084083633365282, 438.0234350436313093, 4.171260309356221718 ) ) ;
#69237 = EDGE_LOOP ( 'NONE', ( #3674, #78122, #89596, #103081, #16479 ) ) ;
#69239 = CARTESIAN_POINT ( 'NONE',  ( 31.20659673062720785, -25.60560110436567172, 31.04007313146203728 ) ) ;
#69238 = FACE_OUTER_BOUND ( 'NONE', #91263, .T. ) ;
#69240 = CARTESIAN_POINT ( 'NONE',  ( -20.16952962162108065, -4.285714285713656757, 15.50035291838862683 ) ) ;
#69241 = VERTEX_POINT ( 'NONE', #73376 ) ;
#69242 = CARTESIAN_POINT ( 'NONE',  ( 34.04714008975750517, 484.1152113529149688, 1.016147467615621247 ) ) ;
#69244 = CARTESIAN_POINT ( 'NONE',  ( -20.52350613252515643, 304.8999024697870937, 9.947223320822450532 ) ) ;
#69243 = CARTESIAN_POINT ( 'NONE',  ( -26.28481937415909542, 35.01454853161727954, -7.860150299234582860 ) ) ;
#69245 = CARTESIAN_POINT ( 'NONE',  ( 64.29999999999999716, 3.309500000000014541, 0.000000000000000000 ) ) ;
#69246 = CARTESIAN_POINT ( 'NONE',  ( -44.12472801210822837, 485.7238370326490440, 3.975897585127424527 ) ) ;
#69247 = DIRECTION ( 'NONE',  ( 1.000000000000000000, 1.224606353822377258E-16, 0.000000000000000000 ) ) ;
#69248 = CARTESIAN_POINT ( 'NONE',  ( 7.036764705882354143, 40.00000000373363207, -71.06385277390853616 ) ) ;
#69249 = CARTESIAN_POINT ( 'NONE',  ( 32.81992448453848965, 465.7192846569214453, 11.17271167765358442 ) ) ;
#69250 = DIRECTION ( 'NONE',  ( 0.000000000000000000, 0.000000000000000000, -1.000000000000000000 ) ) ;
#69251 = ORIENTED_EDGE ( 'NONE', *, *, #42893, .F. ) ;
#69252 = CARTESIAN_POINT ( 'NONE',  ( 92.26840822479495330, -60.00000000000002842, 1.944625616427832826 ) ) ;
#69253 = B_SPLINE_CURVE_WITH_KNOTS ( 'NONE', 3,
 ( #688, #29182, #10408, #76204 ),
 .UNSPECIFIED., .F., .F.,
 ( 4, 4 ),
 ( 0.000000000000000000, 0.002502641776602361305 ),
 .UNSPECIFIED. ) ;
#69254 = CARTESIAN_POINT ( 'NONE',  ( -20.00000000000000000, 12.99999999999999289, 0.000000000000000000 ) ) ;
#69256 = PRESENTATION_STYLE_ASSIGNMENT (( #28283 ) ) ;
#69255 = VECTOR ( 'NONE', #35201, 1000.000000000000000 ) ;
#69257 = CARTESIAN_POINT ( 'NONE',  ( -35.68159617069628098, 373.6642197484802068, 4.177052563641423077 ) ) ;
#69258 = CIRCLE ( 'NONE', #33148, 5.000000000000011546 ) ;
#69259 = CARTESIAN_POINT ( 'NONE',  ( -6.960057398333500345, 40.00000000008189716, -71.11869238929787684 ) ) ;
#69260 = CARTESIAN_POINT ( 'NONE',  ( 29.08076923076923137, -4.171999999999999709, 5.616230220889763424E-16 ) ) ;
#69261 = ORIENTED_EDGE ( 'NONE', *, *, #88867, .T. ) ;
#69262 = EDGE_CURVE ( 'NONE', #66178, #444, #68753, .T. ) ;
#69263 = CARTESIAN_POINT ( 'NONE',  ( -84.45944469708555857, -29.99999999999518252, 196.7683117583226533 ) ) ;
#69264 = ORIENTED_EDGE ( 'NONE', *, *, #79096, .T. ) ;
#69265 =( LENGTH_UNIT ( ) NAMED_UNIT ( * ) SI_UNIT ( .MILLI., .METRE. ) );
#69266 = CARTESIAN_POINT ( 'NONE',  ( 6.683837171061806082, 7.911893696991936231, -4.595687358162529387E-16 ) ) ;
#69267 = CARTESIAN_POINT ( 'NONE',  ( 16.14595037817326428, 20.48388002517883066, -4.555408037434820478 ) ) ;
#69268 = CARTESIAN_POINT ( 'NONE',  ( 85.28627536060220393, -60.19927222349419793, -15.58279874029676471 ) ) ;
#69269 = AXIS2_PLACEMENT_3D ( 'NONE', #184, #58466, #33150 ) ;
#69270 = CARTESIAN_POINT ( 'NONE',  ( -2.977408999572654480, -29.00000000204838813, 7.188101187499999156 ) ) ;
#69271 = CARTESIAN_POINT ( 'NONE',  ( -17.94988149306818315, 34.25920654870290605, 23.42332176153287193 ) ) ;
#69272 = CARTESIAN_POINT ( 'NONE',  ( 9.295423129715947752, 45.72519545954834541, -14.93632663516908821 ) ) ;
#69273 = EDGE_LOOP ( 'NONE', ( #4999, #1642, #28498, #85600, #6292 ) ) ;
#69275 = ADVANCED_FACE ( 'NONE', ( #38236 ), #77357, .T. ) ;
#69274 = CARTESIAN_POINT ( 'NONE',  ( -6.499999999999999112, -4.077972562205410156, -6.122137109124706988 ) ) ;
#69276 =( GEOMETRIC_REPRESENTATION_CONTEXT ( 3 ) GLOBAL_UNCERTAINTY_ASSIGNED_CONTEXT ( ( #66674 ) ) GLOBAL_UNIT_ASSIGNED_CONTEXT ( ( #91054, #33890, #100711 ) ) REPRESENTATION_CONTEXT ( 'NONE', 'WORKASPACE' ) );
#69277 = ORIENTED_EDGE ( 'NONE', *, *, #14417, .F. ) ;
#69278 = DIRECTION ( 'NONE',  ( 0.000000000000000000, 1.000000000000000000, 0.000000000000000000 ) ) ;
#69279 = ADVANCED_FACE ( 'NONE', ( #47349 ), #44641, .F. ) ;
#69280 = ORIENTED_EDGE ( 'NONE', *, *, #71142, .F. ) ;
#69281 = CARTESIAN_POINT ( 'NONE',  ( 81.43616672422064084, -29.09222109329241945, 143.4168869114997165 ) ) ;
#69282 = ORIENTED_EDGE ( 'NONE', *, *, #73235, .T. ) ;
#69283 = CARTESIAN_POINT ( 'NONE',  ( 4.461741436590552112, -48.02090051515271796, 43.16544567096210017 ) ) ;
#69284 = CARTESIAN_POINT ( 'NONE',  ( 2.977408999572652260, -19.43750000204838457, 7.188101187500000044 ) ) ;
#69285 = CARTESIAN_POINT ( 'NONE',  ( -109.5878728966581832, -57.66746364524283308, 196.8330158634452118 ) ) ;
#69286 = B_SPLINE_CURVE_WITH_KNOTS ( 'NONE', 3,
 ( #33250, #41844, #98481, #57480, #24109, #33784, #89873, #90406, #15980, #48333, #99000, #7873 ),
 .UNSPECIFIED., .F., .F.,
 ( 4, 2, 2, 2, 2, 4 ),
 ( 0.000000000000000000, 0.0008247946606697752940, 0.001649589321339550588, 0.002061986651674447071, 0.002474383982009343771, 0.003299178642679118957 ),
 .UNSPECIFIED. ) ;
#69287 = ORIENTED_EDGE ( 'NONE', *, *, #89266, .T. ) ;
#69288 = PRESENTATION_LAYER_ASSIGNMENT (  '', '', ( #2104 ) ) ;
#69289 =( NAMED_UNIT ( * ) PLANE_ANGLE_UNIT ( ) SI_UNIT ( $, .RADIAN. ) );
#69290 = DIRECTION ( 'NONE',  ( 0.000000000000000000, 0.000000000000000000, 1.000000000000000000 ) ) ;
#69291 = CARTESIAN_POINT ( 'NONE',  ( -5.093234209761996034, -12.44467773464909754, 3.176141468578047800 ) ) ;
#69292 = CARTESIAN_POINT ( 'NONE',  ( -36.80513907854941635, 28.12583545932849916, -11.20123465776408445 ) ) ;
#69293 = CARTESIAN_POINT ( 'NONE',  ( 8.929771841637641927, -5.000000000000000888, 6.123233995736769241E-16 ) ) ;
#69294 = CARTESIAN_POINT ( 'NONE',  ( 8.000000000000000000, -18.68750000409676915, 0.000000000000000000 ) ) ;
#69295 = CARTESIAN_POINT ( 'NONE',  ( -45.76875562652180207, -28.55789701437204542, 40.90047540029672035 ) ) ;
#69296 = CARTESIAN_POINT ( 'NONE',  ( 9.537927238823520781, 247.3537314288182358, -3.010735687602435373 ) ) ;
#69297 = CARTESIAN_POINT ( 'NONE',  ( -43.84752573847097068, 486.0721194390189339, 5.282948175116183975 ) ) ;
#69298 = ADVANCED_FACE ( 'NONE', ( #105072 ), #62491, .F. ) ;
#69299 = CARTESIAN_POINT ( 'NONE',  ( 9.482993638194542996, 32.44348720253677243, -3.177441187500463560 ) ) ;
#69300 = CARTESIAN_POINT ( 'NONE',  ( 25.59999999999999787, 1.533819458162526451E-15, 0.000000000000000000 ) ) ;
#69301 = SHAPE_DEFINITION_REPRESENTATION ( #2784, #77771 ) ;
#69302 = CARTESIAN_POINT ( 'NONE',  ( 32.94352307844687289, 463.6326549538520112, 6.941370215393830811 ) ) ;
#69303 = ORIENTED_EDGE ( 'NONE', *, *, #97094, .F. ) ;
#69304 = CARTESIAN_POINT ( 'NONE',  ( -3.913636579744179667, -52.92916190526523934, 40.44644374621901051 ) ) ;
#69305 = CARTESIAN_POINT ( 'NONE',  ( 7.150000000000005684, 41.64999999999999147, -68.91429206202190016 ) ) ;
#69306 = FACE_OUTER_BOUND ( 'NONE', #97019, .T. ) ;
#69307 = CARTESIAN_POINT ( 'NONE',  ( 74.41155834966481564, -38.35600210799680809, -29.41977220444294261 ) ) ;
#69308 = CARTESIAN_POINT ( 'NONE',  ( -86.31537193578998313, -29.99999999999998934, 180.5207776403601372 ) ) ;
#69309 = VERTEX_POINT ( 'NONE', #31212 ) ;
#69310 = CARTESIAN_POINT ( 'NONE',  ( -12.99999999999996625, -1.778091562876227272E-14, -8.000000000000000000 ) ) ;
#69311 = CARTESIAN_POINT ( 'NONE',  ( 73.89615930086935691, -57.61735591279438751, 186.5259515469176108 ) ) ;
#69312 = CARTESIAN_POINT ( 'NONE',  ( 1.308996938995747872, 48.00000000000001421, -95.00000000000000000 ) ) ;
#69313 = CARTESIAN_POINT ( 'NONE',  ( 28.39691108350841375, -28.98146926308949389, -38.24856420472010399 ) ) ;
#69314 = CARTESIAN_POINT ( 'NONE',  ( 43.00000000000000000, 438.3878896346935790, 16.22878885428537998 ) ) ;
#69315 = CARTESIAN_POINT ( 'NONE',  ( 6.145467199749145237, -3.000000000000003109, -92.99666842398180222 ) ) ;
#69316 = CARTESIAN_POINT ( 'NONE',  ( -56.17991941645016141, -60.00000000000000000, 88.71135144568317799 ) ) ;
#69317 = CARTESIAN_POINT ( 'NONE',  ( 18.58349330513380337, -4.000000000000000000, 4.898587196589415787E-16 ) ) ;
#69318 = CARTESIAN_POINT ( 'NONE',  ( -86.75643894772611020, -28.06581177804503824, 186.0048141377419881 ) ) ;
#69319 = B_SPLINE_CURVE_WITH_KNOTS ( 'NONE', 3,
 ( #68506, #71534, #36702, #104435, #27549, #51767, #60429, #52837, #93307, #19461, #65578, #40762, #106556, #32708, #89332, #14352, #49374, #98462, #81207, #16493, #32162, #7323, #39723, #96890, #47779, #57463, #23025, #90384, #56933, #82282, #55855, #8395, #41297, #65042, #105505, #23554, #73650, #22506, #24614, #40234, #74184, #30584, #63477, #96376, #55345, #73107, #88274, #80684, #106016, #48313, #47258, #80158, #6261, #56396, #39197, #72075, #104984, #97940, #24090, #31128, #89853, #81730, #88796, #64013, #15425, #14886, #6804, #72600, #31645, #97394, #64526, #15962, #48840, #7856, #92502, #82822, #58562, #74714, #84955, #10520, #59630, #27294, #18654, #98981, #75246, #18109, #26230, #51513, #43436, #59091, #93045, #41827, #25701, #19210, #84428, #100065, #100595, #83349, #25146, #76316, #1346, #42359, #49914, #8921, #91461, #101134, #26755, #2428, #9440, #66104, #792, #34841, #91975, #35372, #68241, #60177, #52042, #11043, #50968, #90925, #43961, #33765, #1888, #263, #83879, #9993, #34309, #66639, #17575, #33231, #99522, #58002, #17039, #50437, #67186, #42899, #75793, #67712, #45046, #69835, #87091, #21314, #21844, #62813, #4569, #76853, #13168, #2958, #78979, #12637, #101669, #94106, #45571, #94663, #95703, #70894, #46094, #102735, #38033, #87619, #103784, #70369, #3509, #69316, #20273, #53123, #28894, #68788, #29926, #61768, #36450, #85496, #20809, #13703, #53643, #103264, #37506, #102195, #62292, #29413, #35916, #12115, #95182, #86040, #77928, #93584, #27829, #54151, #54685, #78446, #44504, #4037, #86574, #36969, #5102, #60698, #19735, #52572, #77395, #11576, #28342, #61220, #14228, #96251, #14759, #88670, #89204, #104856, #6677, #47134, #48190, #7731, #23427, #56267, #55737, #6142, #63881, #73522, #39071, #106423, #72990, #15303, #65456, #5621, #96770, #63351, #22377, #71952, #22899, #97808, #98349, #32582, #81093, #46614, #89739, #79511, #48716, #7206, #71409, #47661, #40114, #23972, #24503, #80557, #39605, #105896, #32043, #57336, #81604, #64923, #80029, #30999, #72478, #105384, #31523, #38544, #40638, #64405, #97278, #55222, #56814, #15834, #90259, #104308, #30458, #88148, #41179, #17451, #16912, #58425, #42764, #33632, #91336, #33113, #8266, #9852, #35234, #91850, #90798, #99385, #26108, #2285, #50317, #16361, #74058, #17976, #43302, #146, #58965, #65977, #101000, #49248, #25017, #98856, #76186, #34714, #57871, #83221, #34178, #42226, #67588, #59498, #82153, #49790, #82695, #9316, #50837, #8800, #27158, #41708, #83742, #74590, #18517, #666, #75113, #66510, #25567, #1209, #10385, #75655, #68100, #92368, #67056, #84291, #60046, #99933, #1757, #100466, #26626, #51376, #44914, #37372, #52438, #2827, #11983, #68661, #103137, #29285, #85355, #52990, #94529, #20680, #19607, #78314, #45438, #29807, #11441, #4972, #35783, #60570, #93460, #101540, #4430, #37901, #93980, #70762, #70236, #86967, #44368, #78843, #20136, #84825, #61637, #13034, #10905, #28755, #43824, #103657, #92904, #27693, #76716, #45962, #62168, #77265, #61091, #3910, #77798, #95058, #21192, #36842, #19071, #51911, #85910, #53519, #3377, #36319, #69189, #86447, #102061, #54023, #28220, #69709, #102602, #12508, #14095, #56680, #89070, #105769, #38934, #21710, #63212, #23291, #89602, #15696, #30320, #5498, #30867, #104712, #105252, #47002, #22769, #96104, #64276, #23835, #39470, #72349, #71805, #22238, #79900, #48585, #55087, #54547, #38420, #31398, #81473, #87490, #6010, #79376, #71283, #88016, #63746, #7072, #7591, #40509, #97144, #62682, #31909, #95574, #64788, #56128, #13571, #73386, #39988, #72860, #46487, #97667, #96633, #47533, #55605, #104178, #48055, #88542, #14622, #80426, #106283, #6537, #15168, #80957, #99805, #26499, #92232, #42631, #1624, #34586, #91210, #16225, #51237, #67457, #83094, #18386, #34048, #73927, #65847, #9, #9717, #84166, #100335, #74982, #24362, #82012, #1073, #59370, #10261, #66925, #537, #25426, #75530, #57206, #43175, #42097, #76056, #91730, #74457, #32449, #65321, #8668, #98209, #33498, #90125, #83613, #49112, #8133, #41044, #58284, #32977, #98726, #24880, #50192, #25975, #57734, #58836, #17317, #90658, #16765, #49656, #9187, #82564, #41571, #66374, #99254, #17848, #50699, #36719, #35648, #94393, #61501, #45833, #101416, #21067, #51781, #76586, #2700, #10778, #20559, #53905, #3249, #86836, #53395, #103007, #68524, #94931, #36189, #11853, #93320, #12907, #86316, #84694, #60447, #27567, #2157, #12381, #45309, #78190, #4304, #19477, #52314, #37241, #44783, #93851, #20010, #70101, #35111, #43697, #85222, #67978, #29165, #101930, #102473, #11311, #44243, #100865, #62040, #28090, #28620, #77131, #27027, #59908, #69058, #52853, #60965, #85780, #77673, #92778, #18939, #3783, #69584, #37774, #79249, #6407, #71674, #47925, #6945, #88940, #80832, #39864, #30737, #62551, #97537, #72736, #22645, #64662, #55480, #88417, #87887, #38294, #95977, #105640, #71155, #31780, #105126, #23698, #104050, #56550, #89477, #80296, #46875, #104581, #15035, #70636, #15572, #14490, #39345, #78705, #4840, #103530, #29679, #47401, #95437, #22103, #72224, #96512, #21580, #54416, #87359, #63623, #13439, #46360, #5375, #31267, #64151, #30188, #54958, #13967, #97022, #63077, #79777, #23164, #5879, #38806, #56004, #59241, #410, #41972, #82972, #81885, #33922, #941, #92117, #40915, #67333, #98085, #48986, #57084, #66794, #100213, #49530, #26379, #99681, #42505, #16104, #34463, #82439, #48463, #40380, #17190, #75402, #73259, #91082, #106159, #81352, #7463, #25852, #91609, #58709, #73806, #106701, #17715, #50064, #33377, #66251, #50576, #32320, #65191, #83494, #24235, #89997, #99134, #9592, #8005, #1499, #65729, #41444, #32852, #98608, #24758, #57606, #90530, #25297, #16641, #8539, #74336, #58155, #9066, #74856, #59777, #51655, #92653, #102343, #37117, #20425, #60838, #44658, #45192, #43574, #78065, #102880, #19882, #93194 ),
 .UNSPECIFIED., .F., .F.,
 ( 4, 1, 1, 1, 1, 1, 2, 2, 1, 1, 1, 1, 1, 2, 2, 1, 1, 1, 1, 1, 1, 1, 2, 2, 1, 1, 1, 1, 1, 1, 1, 2, 2, 1, 1, 1, 1, 1, 1, 2, 2, 1, 1, 1, 1, 1, 1, 2, 2, 1, 1, 1, 1, 1, 2, 2, 1, 1, 1, 1, 2, 2, 1, 1, 1, 1, 2, 2, 1, 1, 1, 1, 1, 2, 2, 1, 1, 1, 1, 1, 1, 2, 2, 1, 1, 1, 1, 1, 1, 2, 2, 1, 1, 1, 1, 1, 1, 2, 2, 1, 1, 1, 1, 1, 1, 1, 2, 2, 1, 1, 1, 1, 1, 1, 1, 2, 2, 1, 1, 1, 1, 1, 1, 1, 2, 2, 1, 1, 1, 2, 2, 1, 1, 1, 1, 1, 1, 2, 2, 1, 1, 1, 1, 1, 1, 2, 2, 1, 1, 1, 1, 2, 2, 1, 1, 1, 1, 1, 1, 1, 2, 2, 1, 1, 1, 1, 1, 1, 1, 2, 2, 1, 1, 1, 1, 1, 1, 1, 2, 2, 1, 1, 1, 1, 2, 2, 1, 1, 1, 1, 1, 1, 1, 1, 2, 2, 1, 1, 1, 1, 1, 1, 1, 2, 2, 1, 1, 1, 1, 1, 1, 1, 2, 2, 1, 1, 1, 1, 1, 1, 2, 2, 1, 1, 1, 1, 2, 2, 1, 1, 1, 1, 2, 2, 1, 1, 1, 1, 2, 2, 1, 1, 1, 1, 2, 2, 1, 1, 1, 1, 1, 2, 2, 1, 1, 1, 2, 2, 1, 1, 2, 2, 1, 1, 1, 2, 2, 1, 1, 1, 1, 1, 2, 2, 1, 1, 1, 1, 2, 2, 1, 1, 1, 1, 1, 2, 2, 1, 1, 1, 1, 1, 1, 1, 2, 2, 1, 1, 1, 1, 1, 1, 1, 1, 2, 2, 1, 1, 1, 1, 1, 1, 1, 2, 2, 1, 1, 1, 1, 1, 1, 1, 1, 2, 2, 1, 1, 1, 1, 1, 1, 1, 1, 2, 2, 1, 1, 1, 1, 1, 1, 1, 2, 2, 1, 1, 1, 1, 1, 1, 1, 2, 2, 1, 1, 1, 1, 1, 1, 1, 1, 1, 2, 2, 1, 1, 1, 1, 1, 1, 1, 1, 1, 1, 2, 2, 1, 1, 1, 1, 1, 1, 2, 2, 1, 1, 1, 1, 1, 1, 1, 1, 1, 2, 2, 1, 1, 1, 1, 1, 1, 1, 1, 1, 2, 2, 1, 1, 1, 1, 1, 1, 1, 1, 2, 2, 1, 1, 1, 1, 1, 1, 2, 2, 1, 1, 1, 1, 1, 1, 1, 2, 2, 1, 1, 1, 1, 1, 1, 1, 1, 2, 2, 1, 1, 1, 1, 1, 1, 2, 2, 1, 1, 1, 1, 1, 1, 2, 2, 1, 1, 1, 1, 1, 1, 1, 1, 1, 2, 2, 1, 1, 1, 1, 1, 1, 1, 2, 2, 1, 1, 1, 1, 1, 1, 2, 2, 1, 1, 1, 1, 1, 2, 2, 1, 1, 1, 1, 1, 2, 2, 1, 1, 1, 1, 1, 1, 2, 2, 1, 1, 1, 1, 1, 2, 2, 1, 1, 1, 2, 2, 1, 1, 1, 1, 1, 1, 2, 2, 1, 1, 1, 1, 1, 1, 1, 1, 2, 2, 1, 1, 1, 1, 1, 1, 1, 1, 1, 2, 2, 1, 1, 1, 1, 1, 1, 1, 1, 2, 2, 1, 1, 1, 1, 1, 1, 1, 2, 2, 1, 1, 2, 2, 1, 1, 1, 1, 1, 1, 2, 2, 4 ),
 ( 0.000000000000000000, 0.001953124999994617153, 0.002929687499991924862, 0.003417968749990578717, 0.003662109374989905210, 0.003784179687489569541, 0.003845214843739401707, 0.003906249999989233872, 0.005859374999983863602, 0.006835937499981179118, 0.007324218749979836442, 0.007568359374979166838, 0.007690429687478832037, 0.007751464843728667238, 0.007812499999978501572, 0.01171874999996791455, 0.01367187499996262018, 0.01464843749995997299, 0.01513671874995865113, 0.01538085937495798847, 0.01550292968745766234, 0.01556396484370749927, 0.01559448242183242295, 0.01562499999995734662, 0.01953124999994798605, 0.02148437499994329883, 0.02246093749994096389, 0.02294921874993979469, 0.02319335937493920835, 0.02331542968743891692, 0.02337646484368876773, 0.02340698242181369487, 0.02343749999993862201, 0.02734374999992915389, 0.02929687499992441463, 0.03027343749992204847, 0.03076171874992086192, 0.03100585937492025823, 0.03112792968741995639, 0.03118896484366980026, 0.03124999999991964761, 0.03515624999990984989, 0.03710937499990496491, 0.03808593749990252242, 0.03857421874990130117, 0.03881835937490069055, 0.03894042968740039218, 0.03900146484365024646, 0.03906249999990010074, 0.04296874999989073324, 0.04492187499988607030, 0.04589843749988371802, 0.04638671874988255922, 0.04663085937488198329, 0.04675292968738167798, 0.04687499999988137961, 0.05078124999987168597, 0.05273437499986684263, 0.05371093749986441401, 0.05419921874986322052, 0.05444335937486263766, 0.05468749999986205479, 0.05859374999985263177, 0.06054687499984789251, 0.06152343749984554716, 0.06201171874984434673, 0.06225585937484374999, 0.06249999999984315324, 0.06640624999983363308, 0.06835937499982885912, 0.06933593749982645826, 0.06982421874982525090, 0.07006835937482468191, 0.07019042968732440435, 0.07031249999982411292, 0.07421874999981531440, 0.07617187499981092902, 0.07714843749980873633, 0.07763671874980763998, 0.07788085937480709875, 0.07800292968730684895, 0.07806396484355672405, 0.07812499999980659915, 0.08203124999979773124, 0.08398437499979329035, 0.08496093749979106990, 0.08544921874978994580, 0.08569335937478939069, 0.08581542968728912701, 0.08587646484353898824, 0.08593749999978883558, 0.08984374999977955134, 0.09179687499977487453, 0.09277343749977254306, 0.09326171874977139120, 0.09350585937477079446, 0.09362792968727050302, 0.09368896484352036425, 0.09374999999977022547, 0.1015624999997554456, 0.1054687499997480626, 0.1074218749997443711, 0.1083984374997425532, 0.1088867187497416511, 0.1091308593747411515, 0.1092529296872409572, 0.1093139648434908601, 0.1093749999997407629, 0.1171874999997305072, 0.1210937499997254280, 0.1230468749997228883, 0.1240234374997216116, 0.1245117187497209732, 0.1247558593747206124, 0.1248779296872204042, 0.1249389648434702932, 0.1249999999997201960, 0.1328124999997058742, 0.1367187499996986855, 0.1386718749996950495, 0.1396484374996932731, 0.1401367187496924127, 0.1403808593746919409, 0.1405029296871916911, 0.1405639648434415523, 0.1406249999996913858, 0.1484374999996694588, 0.1523437499996584676, 0.1542968749996529720, 0.1552734374996502242, 0.1562499999996474764, 0.1718749999996030120, 0.1796874999995808353, 0.1835937499995697331, 0.1855468749995641820, 0.1865234374995614064, 0.1870117187495600464, 0.1872558593745593802, 0.1874999999995587141, 0.2031249999995167199, 0.2109374999994957089, 0.2148437499994851896, 0.2167968749994799160, 0.2177734374994772515, 0.2182617187494758915, 0.2185058593744751976, 0.2187499999994745037, 0.2343749999994305389, 0.2421874999994086675, 0.2460937499993977040, 0.2480468749993922917, 0.2490234374993895161, 0.2499999999993867683, 0.2656249999993429700, 0.2734374999993210986, 0.2773437499993101074, 0.2792968749993046118, 0.2802734374993018363, 0.2807617187493005040, 0.2810058593742998378, 0.2811279296867994493, 0.2812499999992990052, 0.2890624999992653654, 0.2929687499992484900, 0.2949218749992400523, 0.2958984374992357780, 0.2963867187492336130, 0.2966308593742324473, 0.2967529296867319477, 0.2968139648429816146, 0.2968749999992312816, 0.3007812499992075228, 0.3027343749991956989, 0.3037109374991898147, 0.3041992187491868171, 0.3044433593741853183, 0.3045654296866845967, 0.3046264648429341526, 0.3046569824210589306, 0.3046874999991837640, 0.3085937499991546207, 0.3105468749991400768, 0.3115234374991328603, 0.3120117187491293076, 0.3122558593741275312, 0.3124999999991257549, 0.3164062499990981658, 0.3183593749990843991, 0.3193359374990775157, 0.3198242187490740185, 0.3200683593740721866, 0.3201904296865712984, 0.3202514648428208544, 0.3202819824209456323, 0.3202972412100081323, 0.3203124999990706323, 0.3242187499990919486, 0.3261718749991026067, 0.3271484374991079358, 0.3276367187491106558, 0.3278808593741120991, 0.3280029296866128208, 0.3280639648428630983, 0.3280944824209881538, 0.3281249999991131538, 0.3320312499991172617, 0.3339843749991192046, 0.3349609374991203148, 0.3354492187491209254, 0.3356933593741212585, 0.3358154296866214250, 0.3358764648428715915, 0.3359069824209966471, 0.3359374999991216471, 0.3398437499991351363, 0.3417968749991417976, 0.3427734374991450728, 0.3432617187491466271, 0.3435058593741474597, 0.3436279296866479593, 0.3436889648428982369, 0.3437499999991484589, 0.3457031249991600608, 0.3466796874991657784, 0.3471679687491686650, 0.3474121093741702193, 0.3475341796866709965, 0.3476562499991717736, 0.3496093749991845412, 0.3505859374991909250, 0.3510742187491941446, 0.3513183593741958655, 0.3514404296866966981, 0.3515624999991975308, 0.3554687499992247313, 0.3574218749992383315, 0.3583984374992451039, 0.3588867187492485455, 0.3591308593742503219, 0.3593749999992520983, 0.3632812499992802424, 0.3652343749992943978, 0.3662109374993013922, 0.3666992187493048894, 0.3669433593743067212, 0.3671874999993085531, 0.3710937499993385846, 0.3730468749993535726, 0.3740234374993610666, 0.3745117187493647859, 0.3747558593743665623, 0.3748779296868675059, 0.3749999999993684496, 0.3789062499993985922, 0.3808593749994136357, 0.3818359374994211852, 0.3823242187494248490, 0.3828124999994285682, 0.3847656249994435562, 0.3857421874994511057, 0.3862304687494548250, 0.3867187499994585997, 0.3886718749994738098, 0.3896484374994814703, 0.3901367187494852451, 0.3903808593744871325, 0.3906249999994890199, 0.3945312499995182742, 0.3964843749995329292, 0.3974609374995403122, 0.3979492187495439759, 0.3981933593745456967, 0.3983154296870465849, 0.3984374999995474731, 0.4023437499995760613, 0.4042968749995903277, 0.4052734374995974886, 0.4057617187496010414, 0.4060058593746028732, 0.4062499999996046496, 0.4101562499996342925, 0.4121093749996490030, 0.4130859374996563860, 0.4135742187496600497, 0.4138183593746619371, 0.4139404296871629363, 0.4140624999996639355, 0.4179687499996955768, 0.4199218749997114530, 0.4208984374997194466, 0.4213867187497234434, 0.4216308593747254974, 0.4217529296872264966, 0.4218139648434769962, 0.4218444824216022182, 0.4218749999997274958, 0.4296874999997709055, 0.4335937499997924993, 0.4355468749998033240, 0.4365234374998085976, 0.4370117187498112621, 0.4372558593748125944, 0.4373779296873132605, 0.4374389648435635936, 0.4374694824216888156, 0.4374999999998139821, 0.4453124999998648303, 0.4492187499998902545, 0.4511718749999029665, 0.4521484374999093503, 0.4526367187499124589, 0.4528808593749141242, 0.4530029296874149014, 0.4530639648436652900, 0.4531249999999156786, 0.4609374999999559797, 0.4648437499999760747, 0.4667968749999861222, 0.4677734374999912292, 0.4682617187499937828, 0.4685058593749951150, 0.4686279296874957256, 0.4686889648437460032, 0.4687194824218710587, 0.4687499999999961142, 0.4843750000000557332, 0.4921875000000855982, 0.4960937500001005307, 0.4980468750001079137, 0.4990234375001115774, 0.4995117187501134648, 0.4997558593751144085, 0.4998779296876148526, 0.4999389648438650746, 0.5000000000001153522, 0.5078125000001506573, 0.5117187500001684208, 0.5136718750001773026, 0.5146484375001816325, 0.5151367187501839640, 0.5153808593751850742, 0.5155029296876856293, 0.5155639648439359624, 0.5156250000001861844, 0.5234375000002311484, 0.5273437500002536860, 0.5292968750002650102, 0.5302734375002706724, 0.5307617187502734479, 0.5310058593752747802, 0.5311279296877753353, 0.5311889648440256684, 0.5312500000002758904, 0.5468750000003493872, 0.5546875000003861356, 0.5585937500004045653, 0.5605468750004138911, 0.5615234375004185541, 0.5620117187504208855, 0.5622558593754219958, 0.5623779296879225509, 0.5624389648441727729, 0.5624694824222978840, 0.5625000000004229950, 0.5781250000004987122, 0.5859375000005365708, 0.5898437500005554446, 0.5917968750005648815, 0.5927734375005696554, 0.5932617187505719869, 0.5935058593755730971, 0.5936279296880737633, 0.5936889648443239853, 0.5937194824224492073, 0.5937347412115117073, 0.5937500000005743184, 0.6015625000005714318, 0.6054687500005699885, 0.6074218750005692113, 0.6083984375005688783, 0.6088867187505687673, 0.6091308593755686562, 0.6092529296880686562, 0.6093750000005686562, 0.6171875000005672129, 0.6210937500005664358, 0.6230468750005659917, 0.6240234375005658807, 0.6245117187505657697, 0.6247558593755656586, 0.6248779296880656586, 0.6249389648443157697, 0.6249694824224407697, 0.6249847412115031586, 0.6250000000005656586, 0.6406250000005540013, 0.6484375000005482281, 0.6523437500005453415, 0.6542968750005440093, 0.6552734375005432321, 0.6557617187505427880, 0.6560058593755425660, 0.6561279296880424550, 0.6561889648442924550, 0.6562194824224174550, 0.6562500000005424550, 0.6718750000005199174, 0.6796875000005085932, 0.6835937500005029310, 0.6855468750005001555, 0.6865234375004988232, 0.6870117187504981571, 0.6872558593754978240, 0.6873779296879976020, 0.6874389648442474909, 0.6875000000004973799, 0.6953125000004835021, 0.6992187500004765077, 0.7011718750004729550, 0.7021484375004711787, 0.7026367187504702905, 0.7028808593754698464, 0.7030029296879696243, 0.7031250000004694023, 0.7109375000004556355, 0.7148437500004487521, 0.7167968750004453105, 0.7177734375004436451, 0.7182617187504427569, 0.7185058593754423129, 0.7186279296879420908, 0.7186889648441919798, 0.7187500000004419798, 0.7343750000004218847, 0.7421875000004117817, 0.7460937500004067857, 0.7480468750004042322, 0.7490234375004030110, 0.7495117187504024558, 0.7497558593754021228, 0.7498779296879020118, 0.7499389648441520118, 0.7500000000004019007, 0.7578125000003932410, 0.7617187500003889111, 0.7636718750003868017, 0.7646484375003855805, 0.7651367187503850253, 0.7653808593753848033, 0.7655029296878846923, 0.7656250000003845813, 0.7695312500003802514, 0.7714843750003781420, 0.7724609375003770317, 0.7729492187503764766, 0.7731933593753762546, 0.7733154296878761436, 0.7733764648441261436, 0.7734375000003760325, 0.7773437500003719247, 0.7792968750003699263, 0.7802734375003688161, 0.7807617187503682610, 0.7810058593753680389, 0.7811279296878679279, 0.7811889648441179279, 0.7812194824222428169, 0.7812347412113053169, 0.7812423706058364559, 0.7812500000003677059, 0.7832031250003650413, 0.7841796875003637091, 0.7846679687503629319, 0.7849121093753625988, 0.7850341796878624878, 0.7850952148441124878, 0.7851257324222373768, 0.7851409912112998768, 0.7851562500003622658, 0.7871093750003591571, 0.7880859375003576028, 0.7885742187503567147, 0.7888183593753563816, 0.7889404296878561595, 0.7890014648441061595, 0.7890319824222310485, 0.7890625000003559375, 0.7910156250003529399, 0.7919921875003514966, 0.7924804687503506084, 0.7927246093753502754, 0.7928466796878500533, 0.7929077148441000533, 0.7929687500003499423, 0.7949218750003470557, 0.7958984375003456124, 0.7963867187503447242, 0.7966308593753443912, 0.7967529296878441691, 0.7968139648440941691, 0.7968750000003440581, 0.8007812500003379519, 0.8027343750003349543, 0.8037109375003335110, 0.8041992187503327338, 0.8044433593753322898, 0.8045654296878320677, 0.8046264648440820677, 0.8046875000003319567, 0.8085937500003258505, 0.8105468750003228529, 0.8115234375003212985, 0.8120117187503205214, 0.8122558593753200773, 0.8123779296878198553, 0.8125000000003195222, 0.8164062500003130829, 0.8183593750003097522, 0.8193359375003080869, 0.8198242187503073097, 0.8203125000003065326, 0.8242187500003000933, 0.8261718750002967626, 0.8271484375002952083, 0.8276367187502944311, 0.8278808593752939871, 0.8280029296877937650, 0.8280639648440435430, 0.8281250000002934319, 0.8359375000002851053, 0.8398437500002808864, 0.8417968750002787770, 0.8427734375002777778, 0.8432617187502772227, 0.8435058593752770006, 0.8436279296877768896, 0.8436889648440267786, 0.8437194824221518896, 0.8437500000002768896, 0.8593750000002475797, 0.8671875000002329248, 0.8710937500002255973, 0.8730468750002218226, 0.8740234375002200462, 0.8745117187502191580, 0.8747558593752187139, 0.8748779296877184919, 0.8749389648439683809, 0.8749694824220932698, 0.8750000000002181588, 0.8906250000001916245, 0.8984375000001784128, 0.9023437500001717515, 0.9042968750001685319, 0.9052734375001667555, 0.9057617187501659783, 0.9060058593751655343, 0.9061279296876653122, 0.9061889648439152012, 0.9062500000001649791, 0.9218750000001372236, 0.9296875000001233458, 0.9335937500001163514, 0.9355468750001129097, 0.9365234375001112443, 0.9370117187501103562, 0.9372558593751099121, 0.9373779296876096900, 0.9375000000001093570, 0.9531250000000818234, 0.9609375000000680567, 0.9648437500000611733, 0.9687500000000542899, 0.9765625000000405231, 0.9804687500000336398, 0.9824218750000300870, 0.9833984375000284217, 0.9838867187500275335, 0.9841308593750270894, 0.9842529296875268674, 0.9843750000000266454, 1.000000000000000000 ),
 .UNSPECIFIED. ) ;
#69320 = AXIS2_PLACEMENT_3D ( 'NONE', #20522, #77094, #3214 ) ;
#69321 = ORIENTED_EDGE ( 'NONE', *, *, #52806, .T. ) ;
#69322 = DIRECTION ( 'NONE',  ( 1.000000000000000000, 0.000000000000000000, -1.224646799147353207E-16 ) ) ;
#69323 = CARTESIAN_POINT ( 'NONE',  ( -2.027236533537560614, -46.43928285645216647, 31.62702113814393101 ) ) ;
#69324 = CARTESIAN_POINT ( 'NONE',  ( -6.916167714701083824, 41.81554662627394237, -59.83173445090647391 ) ) ;
#69325 = AXIS2_PLACEMENT_3D ( 'NONE', #59472, #94496, #85327 ) ;
#69326 = CARTESIAN_POINT ( 'NONE',  ( 0.000000000000000000, 0.000000000000000000, -3.012075477074183105 ) ) ;
#69327 = VERTEX_POINT ( 'NONE', #88883 ) ;
#69328 = EDGE_CURVE ( 'NONE', #72766, #27223, #66212, .T. ) ;
#69329 = CARTESIAN_POINT ( 'NONE',  ( -34.01929857393211165, 322.4300229039442911, -5.462111840924722905 ) ) ;
#69330 = DIRECTION ( 'NONE',  ( -1.000000000000000000, -1.224606353822377258E-16, -0.000000000000000000 ) ) ;
#69331 = CARTESIAN_POINT ( 'NONE',  ( 16.84999999999999787, 1.533819458162526451E-15, 0.000000000000000000 ) ) ;
#69332 = CARTESIAN_POINT ( 'NONE',  ( -29.77184624873650520, 12.99572234387823322, -39.60535821593474992 ) ) ;
#69333 = ORIENTED_EDGE ( 'NONE', *, *, #28208, .T. ) ;
#69334 = PRESENTATION_LAYER_ASSIGNMENT (  '', '', ( #22850 ) ) ;
#69335 = CARTESIAN_POINT ( 'NONE',  ( 23.79019632451556276, 303.5314421105786096, -9.853825711238384244 ) ) ;
#69336 = CARTESIAN_POINT ( 'NONE',  ( 45.29905483860081716, 480.9466865490944656, -2.171671249451534003 ) ) ;
#69337 = ADVANCED_FACE ( 'NONE', ( #39285 ), #46471, .F. ) ;
#69338 = DIRECTION ( 'NONE',  ( 0.1270361284032138216, -0.9918980905719710917, 0.000000000000000000 ) ) ;
#69339 = EDGE_CURVE ( 'NONE', #82432, #29715, #13909, .T. ) ;
#69340 = CARTESIAN_POINT ( 'NONE',  ( 102.6948251682922404, -14.21045842199434084, 129.2649694714442035 ) ) ;
#69341 = CARTESIAN_POINT ( 'NONE',  ( -81.85444700155652242, -36.03095774481810309, 154.5099837279508392 ) ) ;
#69342 = ORIENTED_EDGE ( 'NONE', *, *, #47254, .T. ) ;
#69343 = DIRECTION ( 'NONE',  ( 1.000000000000000000, -0.000000000000000000, -0.000000000000000000 ) ) ;
#69344 = CARTESIAN_POINT ( 'NONE',  ( 5.190609988845230838, 252.6392228674358478, -3.016375611400001322 ) ) ;
#69345 = SURFACE_SIDE_STYLE ('',( #20839 ) ) ;
#69346 = APPLICATION_CONTEXT ( 'automotive_design' ) ;
#69347 = CARTESIAN_POINT ( 'NONE',  ( 52.56483885390523625, -79.93083296558610584, -38.23529411764706509 ) ) ;
#69348 = CARTESIAN_POINT ( 'NONE',  ( 33.54469842372052568, 315.6888517999274200, -6.922094226970141762 ) ) ;
#69349 = CARTESIAN_POINT ( 'NONE',  ( 34.78087288526246823, 461.0373983564574019, 3.662433947940674450 ) ) ;
#69350 = ORIENTED_EDGE ( 'NONE', *, *, #92131, .T. ) ;
#69351 = CARTESIAN_POINT ( 'NONE',  ( -13.82057366821712030, 304.5462546222179299, 9.872053150317878334 ) ) ;
#69352 = CARTESIAN_POINT ( 'NONE',  ( 31.41965566404186205, 438.8991828050834556, 23.11713475969801124 ) ) ;
#69353 = CARTESIAN_POINT ( 'NONE',  ( -7.188101187500002709, -27.31250000204838457, 2.977408999572648707 ) ) ;
#69354 = EDGE_CURVE ( 'NONE', #101359, #87625, #30958, .T. ) ;
#69355 = ORIENTED_EDGE ( 'NONE', *, *, #27868, .T. ) ;
#69356 = CARTESIAN_POINT ( 'NONE',  ( -2.352990130084491319E-16, 8.660254037844390851, -10.00000000000000000 ) ) ;
#69357 = LINE ( 'NONE', #18692, #76013 ) ;
#69358 = CARTESIAN_POINT ( 'NONE',  ( -53.52139369739177255, 50.00000000000000000, 33.73130704865319274 ) ) ;
#69359 = CARTESIAN_POINT ( 'NONE',  ( 4.898587196589412829E-16, -18.12499999999999645, -8.000000000000000000 ) ) ;
#69360 = DIRECTION ( 'NONE',  ( 0.000000000000000000, 0.000000000000000000, -1.000000000000000000 ) ) ;
#69361 = ORIENTED_EDGE ( 'NONE', *, *, #49126, .T. ) ;
#69362 = CARTESIAN_POINT ( 'NONE',  ( 19.44199974951657239, -60.00000000000000000, -41.87985567335064019 ) ) ;
#69364 = CARTESIAN_POINT ( 'NONE',  ( 22.80451961301133679, -49.91397639351992410, 33.12551050153431476 ) ) ;
#69363 = CARTESIAN_POINT ( 'NONE',  ( -42.11059216458311028, -14.21045842199439946, 45.52377215771286245 ) ) ;
#69365 = CARTESIAN_POINT ( 'NONE',  ( 113.4944653854903862, 14.17434517210798006, -56.74723269274517179 ) ) ;
#69366 = CARTESIAN_POINT ( 'NONE',  ( -34.67237354032933894, -39.50196040766881822, 35.14490241457752262 ) ) ;
#69367 = ORIENTED_EDGE ( 'NONE', *, *, #44560, .F. ) ;
#69368 = DIRECTION ( 'NONE',  ( -1.000000000000000000, -0.000000000000000000, -0.000000000000000000 ) ) ;
#69369 = CARTESIAN_POINT ( 'NONE',  ( -13.49952125780149714, -55.77501631020759021, 30.71129996282902397 ) ) ;
#69370 = CONICAL_SURFACE ( 'NONE', #62513, 6.499999999999999112, 1.047197551196600296 ) ;
#69371 = CARTESIAN_POINT ( 'NONE',  ( -0.7817778800081601753, 52.07046414514121579, -8.011393227464683520 ) ) ;
#69372 = CARTESIAN_POINT ( 'NONE',  ( 7.412906595240166929, -62.35811727147744676, 3.014362223629234894 ) ) ;
#69373 =( LENGTH_UNIT ( ) NAMED_UNIT ( * ) SI_UNIT ( .MILLI., .METRE. ) );
#69374 = ORIENTED_EDGE ( 'NONE', *, *, #89531, .T. ) ;
#69375 = CARTESIAN_POINT ( 'NONE',  ( -75.89053735638948694, -38.37146565025459211, 177.5147526201425876 ) ) ;
#69376 = DIRECTION ( 'NONE',  ( 0.8191520442889975717, 1.003171929053531773E-16, -0.5735764363510378328 ) ) ;
#69377 = ORIENTED_EDGE ( 'NONE', *, *, #51839, .F. ) ;
#69378 = CARTESIAN_POINT ( 'NONE',  ( 99.84112142693871306, -30.00000000000001066, 152.0655077736769840 ) ) ;
#69379 = CARTESIAN_POINT ( 'NONE',  ( 30.61794937107824310, 40.99878234165733204, -65.44843078843095441 ) ) ;
#69380 = CARTESIAN_POINT ( 'NONE',  ( -5.727189096784633726, -81.42130124751260212, -1.806430436190347377 ) ) ;
#69381 = CARTESIAN_POINT ( 'NONE',  ( 76.78203937826565095, -30.00000000000000000, -16.80719657136269163 ) ) ;
#69382 = DIRECTION ( 'NONE',  ( 0.000000000000000000, -0.1323839925376434634, -0.9911985061125713203 ) ) ;
#69383 = VERTEX_POINT ( 'NONE', #45250 ) ;
#69384 = ORIENTED_EDGE ( 'NONE', *, *, #22910, .T. ) ;
#69385 = VERTEX_POINT ( 'NONE', #22043 ) ;
#69386 = PLANE ( 'NONE',  #28512 ) ;
#69387 =( LENGTH_UNIT ( ) NAMED_UNIT ( * ) SI_UNIT ( .MILLI., .METRE. ) );
#69388 = LINE ( 'NONE', #53718, #51744 ) ;
#69389 = CARTESIAN_POINT ( 'NONE',  ( 33.00000000000000000, 500.0000000000002274, 0.000000000000000000 ) ) ;
#69390 = CARTESIAN_POINT ( 'NONE',  ( -31.33040145750029382, 438.2830743389437771, 22.63980905922802123 ) ) ;
#69391 = CARTESIAN_POINT ( 'NONE',  ( -7.151217271224852290, -86.78749400445713036, -3.587901469523284259 ) ) ;
#69392 = DIRECTION ( 'NONE',  ( -0.000000000000000000, -0.000000000000000000, 1.000000000000000000 ) ) ;
#69393 = ORIENTED_EDGE ( 'NONE', *, *, #45715, .T. ) ;
#69395 = ADVANCED_FACE ( 'NONE', ( #4782 ), #78128, .F. ) ;
#69394 = CARTESIAN_POINT ( 'NONE',  ( 9.596002107491598210, 50.00000000000000000, -77.62543935901993564 ) ) ;
#69396 = ORIENTED_EDGE ( 'NONE', *, *, #56417, .F. ) ;
#69397 = SURFACE_STYLE_USAGE ( .BOTH. , #82908 ) ;
#69398 = CARTESIAN_POINT ( 'NONE',  ( 57.75597479282357227, -38.34392537241339483, 89.45883036084909179 ) ) ;
#69399 = CARTESIAN_POINT ( 'NONE',  ( 21.09715123528542691, 0.000000000000000000, 5.000000000000002665 ) ) ;
#69400 = CARTESIAN_POINT ( 'NONE',  ( 25.23000825560996319, 295.8049451023007350, 10.14223174299324448 ) ) ;
#69401 = CIRCLE ( 'NONE', #74526, 10.00000000000000000 ) ;
#69402 = CARTESIAN_POINT ( 'NONE',  ( -4.589357672516645614, 248.9379396902277790, -3.865585121226774667 ) ) ;
#69403 = CARTESIAN_POINT ( 'NONE',  ( 61.12256913293067839, -29.06402845109642286, 70.22293933626255580 ) ) ;
#69404 = STYLED_ITEM ( 'NONE', ( #41808 ), #83685 ) ;
#69405 = VERTEX_POINT ( 'NONE', #79721 ) ;
#69406 = CARTESIAN_POINT ( 'NONE',  ( -7.996668423981797780, -3.000000000000003109, -91.14546719974914879 ) ) ;
#69407 = DIRECTION ( 'NONE',  ( 1.000000000000000000, 1.224606353822377258E-16, 0.000000000000000000 ) ) ;
#69408 = MECHANICAL_DESIGN_GEOMETRIC_PRESENTATION_REPRESENTATION (  '', ( #76228 ), #36706 ) ;
#69409 = DIRECTION ( 'NONE',  ( -1.000000000000000000, -0.000000000000000000, -0.000000000000000000 ) ) ;
#69410 = EDGE_CURVE ( 'NONE', #65523, #29468, #32710, .T. ) ;
#69411 = CARTESIAN_POINT ( 'NONE',  ( -7.036764705882381676, 40.00000000007575807, -71.06385277390852195 ) ) ;
#69412 = ORIENTED_EDGE ( 'NONE', *, *, #53828, .T. ) ;
#69414 = FACE_OUTER_BOUND ( 'NONE', #85573, .T. ) ;
#69413 = FILL_AREA_STYLE ('',( #4673 ) ) ;
#69415 = DIRECTION ( 'NONE',  ( 0.000000000000000000, -1.000000000000000000, 0.000000000000000000 ) ) ;
#69416 = FILL_AREA_STYLE ('',( #12744 ) ) ;
#69417 = DIRECTION ( 'NONE',  ( -1.000000000000000000, 0.000000000000000000, 0.000000000000000000 ) ) ;
#69418 = CARTESIAN_POINT ( 'NONE',  ( 8.813324044470940422, 294.6780646607570020, 9.900070198401328625 ) ) ;
#69419 = CARTESIAN_POINT ( 'NONE',  ( -7.413471587080149305, 102.3564784083167183, -3.013058070223554541 ) ) ;
#69420 = DIRECTION ( 'NONE',  ( 0.000000000000000000, -1.000000000000000000, 0.000000000000000000 ) ) ;
#69421 = CARTESIAN_POINT ( 'NONE',  ( 84.85594123159673074, -53.83118547258817443, 190.4596540335761006 ) ) ;
#69422 = CARTESIAN_POINT ( 'NONE',  ( -5.171269539170080698, 1.677304854198049089, -22.62158602869747526 ) ) ;
#69423 = EDGE_CURVE ( 'NONE', #65829, #94586, #61979, .T. ) ;
#69424 = CARTESIAN_POINT ( 'NONE',  ( -3.342287015225765767, 120.5339020451717289, 5.000000000000000000 ) ) ;
#69425 = ORIENTED_EDGE ( 'NONE', *, *, #68492, .F. ) ;
#69426 =( NAMED_UNIT ( * ) PLANE_ANGLE_UNIT ( ) SI_UNIT ( $, .RADIAN. ) );
#69427 = CARTESIAN_POINT ( 'NONE',  ( 2.396333687459205386, -15.43569997946047501, -35.20659080967024579 ) ) ;
#69428 = CARTESIAN_POINT ( 'NONE',  ( 0.000000000000000000, -30.00000000000000000, 0.000000000000000000 ) ) ;
#69429 = CARTESIAN_POINT ( 'NONE',  ( 34.47678062874018678, 437.1474145881098821, 5.468662283308735717 ) ) ;
#69430 =( BOUNDED_CURVE ( )  B_SPLINE_CURVE ( 2, ( #104923, #81666, #38092 ),
 .UNSPECIFIED., .F., .F. ) 
 B_SPLINE_CURVE_WITH_KNOTS ( ( 3, 3 ),
 ( 0.000000000000000000, 1.000000000000000000 ),
 .UNSPECIFIED. ) 
 CURVE ( )  GEOMETRIC_REPRESENTATION_ITEM ( )  RATIONAL_B_SPLINE_CURVE ( ( 1.000000000000000000, 1.857142857142858317, 1.000000000000000000 ) ) 
 REPRESENTATION_ITEM ( '' )  );
#69431 = AXIS2_PLACEMENT_3D ( 'NONE', #57942, #34785, #213 ) ;
#69432 = ADVANCED_FACE ( 'NONE', ( #30676 ), #82571, .F. ) ;
#69433 = CARTESIAN_POINT ( 'NONE',  ( -86.41920866340555563, -29.99999999999998934, 66.86452767883984905 ) ) ;
#69434 = COLOUR_RGB ( '', 0.08235294, 0.09019608, 0.10196078) ;
#69435 = CARTESIAN_POINT ( 'NONE',  ( -4.000000000000002665, 0.000000000000000000, -7.974599999999995248 ) ) ;
#69436 = CARTESIAN_POINT ( 'NONE',  ( 18.91792220226865595, -57.67176294956599492, 42.07977622032543508 ) ) ;
#69438 = LINE ( 'NONE', #53246, #6851 ) ;
#69437 = CYLINDRICAL_SURFACE ( 'NONE', #84499, 10.00000000000001954 ) ;
#69439 = CARTESIAN_POINT ( 'NONE',  ( -3.160872658147570124, -18.90246149285938770, 27.03534335979194836 ) ) ;
#69440 = CARTESIAN_POINT ( 'NONE',  ( -17.50570437742704044, 50.00000000000000711, 63.41904368646399348 ) ) ;
#69441 = CARTESIAN_POINT ( 'NONE',  ( -42.61340452791766609, 486.8925439250689351, 7.464118458850250271 ) ) ;
#69442 = DIRECTION ( 'NONE',  ( 1.000000000000000000, 0.000000000000000000, 0.000000000000000000 ) ) ;
#69443 = CARTESIAN_POINT ( 'NONE',  ( 55.93697197481172623, -28.65094093527318364, -26.29639216960241299 ) ) ;
#69444 =( LENGTH_UNIT ( ) NAMED_UNIT ( * ) SI_UNIT ( .MILLI., .METRE. ) );
#69445 = CARTESIAN_POINT ( 'NONE',  ( -21.89279155696590706, -18.59654525183585605, 27.69851634783955419 ) ) ;
#69446 = EDGE_LOOP ( 'NONE', ( #5758, #33313, #63835, #6016, #32216 ) ) ;
#69447 = CARTESIAN_POINT ( 'NONE',  ( 40.50232667759422611, 485.1162572728860596, -4.198421296053016505 ) ) ;
#69448 = CARTESIAN_POINT ( 'NONE',  ( -9.797537890442933772, 108.4655779766619048, 2.014215961808881517 ) ) ;
#69449 = CARTESIAN_POINT ( 'NONE',  ( -18.23433844066610376, -56.88320978890689616, 33.72260518641856208 ) ) ;
#69451 = CARTESIAN_POINT ( 'NONE',  ( -4.000000000000000000, 0.000000000000000000, -0.02540000000000007530 ) ) ;
#69450 = CARTESIAN_POINT ( 'NONE',  ( -1.100699873904698034, 27.52274837490087478, 40.11352787695132349 ) ) ;
#69452 = VERTEX_POINT ( 'NONE', #54354 ) ;
#69453 = EDGE_LOOP ( 'NONE', ( #42758, #74766, #88759, #95430 ) ) ;
#69454 = CARTESIAN_POINT ( 'NONE',  ( 2.078747088351101002, 50.00000000000000711, -97.99984157184401568 ) ) ;
#69455 = CARTESIAN_POINT ( 'NONE',  ( 46.00000000000000000, 450.0000000000002274, 13.20242257375370976 ) ) ;
#69456 = DIRECTION ( 'NONE',  ( 0.000000000000000000, 1.000000000000000000, 0.000000000000000000 ) ) ;
#69457 = ORIENTED_EDGE ( 'NONE', *, *, #81881, .F. ) ;
#69458 = LINE ( 'NONE', #54838, #34297 ) ;
#69459 = CARTESIAN_POINT ( 'NONE',  ( 6.061808134801299985, 49.99999999999999289, -95.47796581436244878 ) ) ;
#69460 = CARTESIAN_POINT ( 'NONE',  ( 102.7253553271523998, -52.71898453613229663, 190.6752664090827523 ) ) ;
#69461 = AXIS2_PLACEMENT_3D ( 'NONE', #11164, #59753, #45168 ) ;
#69462 = CARTESIAN_POINT ( 'NONE',  ( -7.619135598915498520, -6.826946322153224500, 2.449260492474796269 ) ) ;
#69463 = EDGE_LOOP ( 'NONE', ( #92664, #39398, #32655, #7650, #54837, #42520 ) ) ;
#69464 = CIRCLE ( 'NONE', #91856, 10.00000000000000000 ) ;
#69465 = ORIENTED_EDGE ( 'NONE', *, *, #18520, .F. ) ;
#69466 = EDGE_CURVE ( 'NONE', #83030, #85853, #106735, .T. ) ;
#69467 = EDGE_LOOP ( 'NONE', ( #37233, #92526, #15623, #38928, #2050 ) ) ;
#69468 = CARTESIAN_POINT ( 'NONE',  ( 25.25836143086297625, 306.2355318565109883, 10.47456800221746676 ) ) ;
#69469 = EDGE_CURVE ( 'NONE', #18381, #10693, #46912, .T. ) ;
#69470 = CARTESIAN_POINT ( 'NONE',  ( 3.313708498984762496, -14.46875000409676915, 7.999999999999998224 ) ) ;
#69471 = PRESENTATION_STYLE_ASSIGNMENT (( #36606 ) ) ;
#69472 = ORIENTED_EDGE ( 'NONE', *, *, #102673, .T. ) ;
#69473 = FACE_OUTER_BOUND ( 'NONE', #105042, .T. ) ;
#69474 = CARTESIAN_POINT ( 'NONE',  ( -5.406990715186140051, 41.99999999999999289, -69.18631391233250838 ) ) ;
#69475 = CARTESIAN_POINT ( 'NONE',  ( -51.70258171882510112, -60.00000000001934808, -39.97716527442499768 ) ) ;
#69476 = CARTESIAN_POINT ( 'NONE',  ( 7.986468734911287726, -68.97313679723079360, 0.5341897780976170296 ) ) ;
#69477 = CARTESIAN_POINT ( 'NONE',  ( 83.63626497911887725, -60.00000000000972733, -28.47872482695956364 ) ) ;
#69478 = CARTESIAN_POINT ( 'NONE',  ( -16.21528977622788403, -5.000000000000000000, -2.627527450084738536 ) ) ;
#69479 = CARTESIAN_POINT ( 'NONE',  ( 16.08349330513380337, 1.593028355512270567E-15, 0.000000000000000000 ) ) ;
#69481 = CARTESIAN_POINT ( 'NONE',  ( 4.032806863568136890, -35.99137585659471483, 29.88102657759840497 ) ) ;
#69480 = CARTESIAN_POINT ( 'NONE',  ( -98.48977711285814962, -30.00000000000000355, 87.89215492326917456 ) ) ;
#69482 = LINE ( 'NONE', #22550, #89548 ) ;
#69483 = CARTESIAN_POINT ( 'NONE',  ( -48.16068817031700178, -22.22324342221773819, 42.58818931081837889 ) ) ;
#69484 = ORIENTED_EDGE ( 'NONE', *, *, #61183, .F. ) ;
#69485 = CARTESIAN_POINT ( 'NONE',  ( -23.21751746555244722, -1.200000000000000030E-05, 33.20617127781060418 ) ) ;
#69486 = ORIENTED_EDGE ( 'NONE', *, *, #75605, .T. ) ;
#69487 = CARTESIAN_POINT ( 'NONE',  ( 0.1545845557741672149, 7.763550624989376203, -51.74245695911944409 ) ) ;
#69488 = CARTESIAN_POINT ( 'NONE',  ( 17.37733725250692629, 36.93507598878604625, 21.96268678933276775 ) ) ;
#69489 = CARTESIAN_POINT ( 'NONE',  ( 5.476751506168963779, -6.836428771330083975, -2.461144630687907231 ) ) ;
#69490 = EDGE_LOOP ( 'NONE', ( #17122, #97092, #70418, #6147 ) ) ;
#69491 = CARTESIAN_POINT ( 'NONE',  ( 4.813668318631100007, 248.2048677017330931, 3.583991016754775050 ) ) ;
#69492 = EDGE_LOOP ( 'NONE', ( #102155, #46595, #47670, #39996 ) ) ;
#69493 = CARTESIAN_POINT ( 'NONE',  ( 80.65654643016394232, -29.99999999999668887, -24.45529829233118235 ) ) ;
#69494 =( NAMED_UNIT ( * ) PLANE_ANGLE_UNIT ( ) SI_UNIT ( $, .RADIAN. ) );
#69495 = CARTESIAN_POINT ( 'NONE',  ( 3.355892750373768774, -49.00480196350148532, 104.3125661743350179 ) ) ;
#69496 = DIRECTION ( 'NONE',  ( -0.000000000000000000, -0.000000000000000000, -1.000000000000000000 ) ) ;
#69497 = CARTESIAN_POINT ( 'NONE',  ( 37.36680950587120975, 18.64316884708630084, 10.04205104290988437 ) ) ;
#69498 = CARTESIAN_POINT ( 'NONE',  ( 100.4860052063238669, -30.00000000000000000, 182.9306020357272189 ) ) ;
#69499 = STYLED_ITEM ( 'NONE', ( #14173 ), #97466 ) ;
#69500 = FACE_OUTER_BOUND ( 'NONE', #79786, .T. ) ;
#69501 = ORIENTED_EDGE ( 'NONE', *, *, #18813, .F. ) ;
#69502 = STYLED_ITEM ( 'NONE', ( #42739 ), #34531 ) ;
#69503 = CIRCLE ( 'NONE', #40226, 5.000000000000002665 ) ;
#69504 = ORIENTED_EDGE ( 'NONE', *, *, #29619, .F. ) ;
#69505 = EDGE_LOOP ( 'NONE', ( #1943, #75010, #37142, #48507 ) ) ;
#69506 = CARTESIAN_POINT ( 'NONE',  ( 54.66621465509991395, -42.96697404677267684, 60.96662553234383353 ) ) ;
#69507 = COLOUR_RGB ( '', 0.08235294, 0.09019608, 0.10196078) ;
#69508 = CARTESIAN_POINT ( 'NONE',  ( 5.659804915025486771, 41.67004157394842423, -58.69865591471064192 ) ) ;
#69509 = CARTESIAN_POINT ( 'NONE',  ( 21.67692307692307452, 1.411358822780289120E-15, 0.000000000000000000 ) ) ;
#69510 = ORIENTED_EDGE ( 'NONE', *, *, #20921, .T. ) ;
#69512 = ADVANCED_FACE ( 'NONE', ( #63020 ), #22591, .F. ) ;
#69511 = CARTESIAN_POINT ( 'NONE',  ( -90.78511700306292198, -38.40471106913319232, -13.56408848029241199 ) ) ;
#69513 = EDGE_LOOP ( 'NONE', ( #80863, #79074, #49221, #38067 ) ) ;
#69514 = DIRECTION ( 'NONE',  ( -0.2282686145773573927, 0.2753452451907626997, 0.9338513990725574310 ) ) ;
#69515 = CARTESIAN_POINT ( 'NONE',  ( 89.26648953270368736, -38.52947843327230260, 200.3703952722973440 ) ) ;
#69516 = CARTESIAN_POINT ( 'NONE',  ( 11.51161983637667774, 12.49912708945058348, 10.00339853150599367 ) ) ;
#69517 = CARTESIAN_POINT ( 'NONE',  ( 83.79989767149710644, -45.28464700058749060, 6.294244894805590462 ) ) ;
#69518 = CARTESIAN_POINT ( 'NONE',  ( 0.000000000000000000, 0.000000000000000000, 5.000000000000002665 ) ) ;
#69519 = CARTESIAN_POINT ( 'NONE',  ( 5.000000000000000000, -15.93202192939576989, -5.930487099830195952 ) ) ;
#69520 = CARTESIAN_POINT ( 'NONE',  ( 6.288680569791107899, 0.6514782672946227704, 6.828922012435988620 ) ) ;
#69521 = CARTESIAN_POINT ( 'NONE',  ( -43.79821706558210082, 434.9662578767425885, 12.22743114680390342 ) ) ;
#69522 = CARTESIAN_POINT ( 'NONE',  ( 4.323075853814084546, 141.1141821973716617, 5.000000000000000888 ) ) ;
#69523 = ORIENTED_EDGE ( 'NONE', *, *, #41428, .T. ) ;
#69524 = ADVANCED_FACE ( 'NONE', ( #18257 ), #60836, .T. ) ;
#69525 = EDGE_CURVE ( 'NONE', #4466, #38791, #77273, .T. ) ;
#69526 = CARTESIAN_POINT ( 'NONE',  ( 5.947762761376472973, 4.378239541354660425, 5.416666666666664298 ) ) ;
#69527 = CARTESIAN_POINT ( 'NONE',  ( 7.493258622341705255, 40.28998690653781267, -69.65507372783751805 ) ) ;
#69528 = DIRECTION ( 'NONE',  ( -1.000000000000000000, 0.000000000000000000, 0.000000000000000000 ) ) ;
#69529 = ORIENTED_EDGE ( 'NONE', *, *, #83118, .F. ) ;
#69530 = CARTESIAN_POINT ( 'NONE',  ( 0.000000000000000000, -79.93083296558610584, -85.00000000000000000 ) ) ;
#69531 = CARTESIAN_POINT ( 'NONE',  ( -36.56941799720385688, 309.7424336998361696, 13.49796762285306073 ) ) ;
#69532 = DIRECTION ( 'NONE',  ( 0.000000000000000000, 0.000000000000000000, 1.000000000000000000 ) ) ;
#69533 = LINE ( 'NONE', #60917, #30090 ) ;
#69534 = CARTESIAN_POINT ( 'NONE',  ( 8.000000000000000000, -22.99999999999999289, 0.000000000000000000 ) ) ;
#69535 = CARTESIAN_POINT ( 'NONE',  ( -38.00604678449891338, -25.45322539771995807, 34.78474724553195330 ) ) ;
#69536 = CARTESIAN_POINT ( 'NONE',  ( 38.88461863710599431, 437.7975295993173290, 4.475058894670842058 ) ) ;
#69537 = CIRCLE ( 'NONE', #55715, 10.00000000000000178 ) ;
#69538 = ORIENTED_EDGE ( 'NONE', *, *, #52450, .F. ) ;
#69539 = CARTESIAN_POINT ( 'NONE',  ( 85.81934268588042869, -25.08133184341231114, 176.6321996554005977 ) ) ;
#69540 = CARTESIAN_POINT ( 'NONE',  ( -13.00000000000003730, 249.9999999999999432, 4.000000000000002665 ) ) ;
#69541 = EDGE_CURVE ( 'NONE', #9016, #51147, #18808, .T. ) ;
#69542 = DIRECTION ( 'NONE',  ( -1.000000000000000000, -1.224606353822377258E-16, -0.000000000000000000 ) ) ;
#69543 = ORIENTED_EDGE ( 'NONE', *, *, #16832, .T. ) ;
#69544 = AXIS2_PLACEMENT_3D ( 'NONE', #38297, #31270, #15038 ) ;
#69545 = CARTESIAN_POINT ( 'NONE',  ( -97.19992022187756220, -52.71041065253648839, 105.9731406578079032 ) ) ;
#69546 = CARTESIAN_POINT ( 'NONE',  ( 55.26095113931063452, -4.000000000000000000, 0.000000000000000000 ) ) ;
#69547 = CARTESIAN_POINT ( 'NONE',  ( 15.17227823171759837, -5.000000000000002665, -86.54073391195457532 ) ) ;
#69548 = CARTESIAN_POINT ( 'NONE',  ( -30.04470542674692268, 7.904892719711607896, 42.05337092467510729 ) ) ;
#69549 = CARTESIAN_POINT ( 'NONE',  ( -9.569753713556142571, -22.51754484451500815, -38.54307148179644571 ) ) ;
#69550 = STYLED_ITEM ( 'NONE', ( #59921 ), #52620 ) ;
#69551 = EDGE_CURVE ( 'NONE', #8947, #93003, #31484, .T. ) ;
#69552 = CARTESIAN_POINT ( 'NONE',  ( 35.03412771863278152, -60.00000000000000711, 46.43457060836758643 ) ) ;
#69553 = CARTESIAN_POINT ( 'NONE',  ( -3.672464763049774796E-06, -18.02989419364509516, 35.00496915990722613 ) ) ;
#69554 = CARTESIAN_POINT ( 'NONE',  ( 3.052800042147856718, -0.8437115306431165473, 104.0321489743691927 ) ) ;
#69555 = CARTESIAN_POINT ( 'NONE',  ( 51.38078702772865824, -29.89861756130085979, 48.96396542489893733 ) ) ;
#69557 = CARTESIAN_POINT ( 'NONE',  ( -13.15523420476091054, 19.48922470848437172, 7.613334812991558564 ) ) ;
#69556 = CARTESIAN_POINT ( 'NONE',  ( -33.81973378879969516, -34.85196562608981452, 43.20933532560730583 ) ) ;
#69558 = CARTESIAN_POINT ( 'NONE',  ( -1.435124379509183671E-09, 294.8518027762758038, -10.00000000000000178 ) ) ;
#69559 = CARTESIAN_POINT ( 'NONE',  ( 4.401442555609581635E-16, -9.781250002048384573, -7.188101187500000044 ) ) ;
#69560 = EDGE_CURVE ( 'NONE', #170, #38295, #60285, .T. ) ;
#69561 = CARTESIAN_POINT ( 'NONE',  ( 4.898587196589412829E-16, -24.31250000409677270, -8.000000000000000000 ) ) ;
#69562 = DIRECTION ( 'NONE',  ( 0.000000000000000000, -1.000000000000000000, 0.000000000000000000 ) ) ;
#69563 = ORIENTED_EDGE ( 'NONE', *, *, #15608, .T. ) ;
#69564 = CARTESIAN_POINT ( 'NONE',  ( 0.000000000000000000, 294.8518027762758038, -10.00000000000000178 ) ) ;
#69565 = CARTESIAN_POINT ( 'NONE',  ( -17.50000000000003553, 51.60805965402929729, 62.32523305737346675 ) ) ;
#69567 = ADVANCED_FACE ( 'NONE', ( #37115 ), #77000, .F. ) ;
#69566 = AXIS2_PLACEMENT_3D ( 'NONE', #5464, #22738, #55577 ) ;
#69568 = ORIENTED_EDGE ( 'NONE', *, *, #49598, .F. ) ;
#69569 = CARTESIAN_POINT ( 'NONE',  ( -15.88481125434442909, -1.943298766509323316, 14.87559245782164119 ) ) ;
#69570 = CARTESIAN_POINT ( 'NONE',  ( -13.00000000000003730, -65.00000000000000000, 4.000000000000002665 ) ) ;
#69571 = DIRECTION ( 'NONE',  ( 0.000000000000000000, 1.000000000000000000, 0.000000000000000000 ) ) ;
#69572 =( GEOMETRIC_REPRESENTATION_CONTEXT ( 3 ) GLOBAL_UNCERTAINTY_ASSIGNED_CONTEXT ( ( #84747 ) ) GLOBAL_UNIT_ASSIGNED_CONTEXT ( ( #70043, #45770, #4784 ) ) REPRESENTATION_CONTEXT ( 'NONE', 'WORKASPACE' ) );
#69574 = CARTESIAN_POINT ( 'NONE',  ( -12.77240031018320288, -47.40885967665541756, -34.44485374093346763 ) ) ;
#69573 = CARTESIAN_POINT ( 'NONE',  ( 7.000000000000000000, 0.000000000000000000, -6.275264681066861527 ) ) ;
#69575 = ORIENTED_EDGE ( 'NONE', *, *, #94959, .T. ) ;
#69576 = MECHANICAL_DESIGN_GEOMETRIC_PRESENTATION_REPRESENTATION (  '', ( #86830 ), #85118 ) ;
#69577 = DIRECTION ( 'NONE',  ( -1.000000000000000000, -0.000000000000000000, -0.000000000000000000 ) ) ;
#69578 = CARTESIAN_POINT ( 'NONE',  ( -1.000000000001115108, -5.000000000000000000, -14.14213562373095101 ) ) ;
#69579 = VECTOR ( 'NONE', #74947, 999.9999999999998863 ) ;
#69580 = ORIENTED_EDGE ( 'NONE', *, *, #31899, .T. ) ;
#69581 = SHAPE_REPRESENTATION ( 'MAS-677', ( #85193, #92047, #74787, #4199, #36958, #100666, #90352, #64500, #104123, #62804, #57599, #33552, #86908, #69652, #50667, #17988, #67948, #54143, #14568, #11110, #21470, #81700, #23159, #28415, #71400, #78263, #24934, #42070, #35246, #31775, #28333, #40372, #95513, #93821, #83421, #102356 ), #52452 ) ;
#69582 = LINE ( 'NONE', #86313, #46587 ) ;
#69583 = CARTESIAN_POINT ( 'NONE',  ( 28.17977184163764193, -5.000000000000000000, 6.123233995736768255E-16 ) ) ;
#69584 = CARTESIAN_POINT ( 'NONE',  ( -92.23642043756412079, -60.00000000000000000, 2.389009461067983953 ) ) ;
#69585 = ORIENTED_EDGE ( 'NONE', *, *, #79405, .F. ) ;
#69586 = CARTESIAN_POINT ( 'NONE',  ( -10.00000000000000000, 15.00000000000000000, 10.00000000000000000 ) ) ;
#69587 = CARTESIAN_POINT ( 'NONE',  ( -3.313708498984726969, -11.46874999999999289, 8.000000000000039080 ) ) ;
#69588 = CARTESIAN_POINT ( 'NONE',  ( 33.00000000000000000, 500.0000000000002274, 0.000000000000000000 ) ) ;
#69589 = CARTESIAN_POINT ( 'NONE',  ( -3.714954396655790969, -48.94453733868888889, 103.2971887958219952 ) ) ;
#69591 = SURFACE_SIDE_STYLE ('',( #60972 ) ) ;
#69590 = CARTESIAN_POINT ( 'NONE',  ( -5.656854249492379694, -26.93749999999999645, -5.656854249492380582 ) ) ;
#69592 = CARTESIAN_POINT ( 'NONE',  ( -80.54183813965836691, -56.90184267136208973, 174.6177441223669291 ) ) ;
#69593 = ORIENTED_EDGE ( 'NONE', *, *, #52969, .F. ) ;
#69594 = CARTESIAN_POINT ( 'NONE',  ( -7.540142361522498504, 0.000000000000000000, 15.29459302240409002 ) ) ;
#69595 = ORIENTED_EDGE ( 'NONE', *, *, #36116, .T. ) ;
#69596 = ORIENTED_EDGE ( 'NONE', *, *, #28069, .T. ) ;
#69597 = CARTESIAN_POINT ( 'NONE',  ( -3.328192429499065685, -5.000000000000000000, 16.34245136408155830 ) ) ;
#69598 = EDGE_CURVE ( 'NONE', #9392, #5037, #77538, .T. ) ;
#69599 = CARTESIAN_POINT ( 'NONE',  ( 9.970195021754669540, 302.6460196488382053, -10.04373974541433689 ) ) ;
#69600 = VERTEX_POINT ( 'NONE', #86185 ) ;
#69601 = CARTESIAN_POINT ( 'NONE',  ( 0.000000000000000000, 0.000000000000000000, 0.000000000000000000 ) ) ;
#69602 = CARTESIAN_POINT ( 'NONE',  ( -93.98392372475152001, -57.65316015971099972, -14.13389826495936141 ) ) ;
#69603 = CARTESIAN_POINT ( 'NONE',  ( 4.999999999999995559, 0.000000000000000000, 42.58845726811989607 ) ) ;
#69604 = LINE ( 'NONE', #20032, #65100 ) ;
#69605 = CARTESIAN_POINT ( 'NONE',  ( -9.177080501238306098, 104.4665305714573122, -3.972956046786645601 ) ) ;
#69606 = LINE ( 'NONE', #22126, #94246 ) ;
#69607 = EDGE_CURVE ( 'NONE', #80083, #83606, #11965, .T. ) ;
#69608 = CARTESIAN_POINT ( 'NONE',  ( 73.45964196357411424, -30.00000000000000355, -28.33384050355910588 ) ) ;
#69609 = CARTESIAN_POINT ( 'NONE',  ( -85.76719879059909601, -14.21045842199445630, 195.9089143291284074 ) ) ;
#69610 = CARTESIAN_POINT ( 'NONE',  ( -56.50716156543574442, -22.14567382208074164, 56.45488485479982899 ) ) ;
#69611 = VERTEX_POINT ( 'NONE', #78063 ) ;
#69612 = CARTESIAN_POINT ( 'NONE',  ( 6.013035130119651406, 14.79159814833020725, -3.585725784831612195 ) ) ;
#69613 = EDGE_LOOP ( 'NONE', ( #105900, #28562, #102177, #5573 ) ) ;
#69614 = CARTESIAN_POINT ( 'NONE',  ( -105.1976808963021313, -60.15494405590796134, 187.0891470627859405 ) ) ;
#69615 = CARTESIAN_POINT ( 'NONE',  ( 0.000000000000000000, 0.000000000000000000, 0.000000000000000000 ) ) ;
#69616 = TOROIDAL_SURFACE ( 'NONE', #35216, 3.500000000000000000, 0.5000000000000000000 ) ;
#69617 = ADVANCED_FACE ( 'NONE', ( #26375 ), #93190, .T. ) ;
#69618 = SURFACE_SIDE_STYLE ('',( #42668 ) ) ;
#69619 = ORIENTED_EDGE ( 'NONE', *, *, #30046, .T. ) ;
#69620 = CARTESIAN_POINT ( 'NONE',  ( 7.500000017879060010, -5.000000000005163869, -69.80246344212856968 ) ) ;
#69621 = AXIS2_PLACEMENT_3D ( 'NONE', #24014, #54732, #96297 ) ;
#69622 = CARTESIAN_POINT ( 'NONE',  ( 76.12557658274094763, -38.35599704320051728, -28.58424740099940919 ) ) ;
#69623 = CARTESIAN_POINT ( 'NONE',  ( 28.50099738913158376, 1.340359594676612611E-15, 0.000000000000000000 ) ) ;
#69624 = CARTESIAN_POINT ( 'NONE',  ( 4.401442555609581635E-16, -14.65625000204838457, -7.188101187500000044 ) ) ;
#69625 = CARTESIAN_POINT ( 'NONE',  ( -1.000000000000000000, -69.59657292933731298, 12.76848391598547394 ) ) ;
#69626 = CARTESIAN_POINT ( 'NONE',  ( 8.866506694866188809, 1.474610560812782335E-15, 0.000000000000000000 ) ) ;
#69627 = CARTESIAN_POINT ( 'NONE',  ( 7.550180524134850302, -81.99440752786813391, 2.651855549982492732 ) ) ;
#69628 = CARTESIAN_POINT ( 'NONE',  ( -40.77380256327629837, 468.8478597483947965, 21.13608272249925690 ) ) ;
#69629 = CARTESIAN_POINT ( 'NONE',  ( -9.559480721551260274, 9.206076766727413485, -0.000000000000000000 ) ) ;
#69630 = CARTESIAN_POINT ( 'NONE',  ( -16.48350313421780555, 45.65798623861609684, -6.657797401561613704 ) ) ;
#69631 = EDGE_CURVE ( 'NONE', #63106, #14235, #68931, .T. ) ;
#69632 = UNCERTAINTY_MEASURE_WITH_UNIT (LENGTH_MEASURE( 1.000000000000000082E-05 ), #56677, 'distance_accuracy_value', 'NONE');
#69633 = CARTESIAN_POINT ( 'NONE',  ( -27.12260435713527684, -49.91548920431219472, 34.05356483041720139 ) ) ;
#69634 = CARTESIAN_POINT ( 'NONE',  ( 47.58705169032300830, -56.81477742123609431, 52.30342271811583288 ) ) ;
#69635 = CARTESIAN_POINT ( 'NONE',  ( -32.76481181362981943, 487.6128877198520399, 8.618969267356323627 ) ) ;
#69636 = CARTESIAN_POINT ( 'NONE',  ( -0.1682199022586588766, 46.21383923812595640, 16.24999999999999645 ) ) ;
#69638 = EDGE_CURVE ( 'NONE', #56216, #34834, #10268, .T. ) ;
#69637 = CARTESIAN_POINT ( 'NONE',  ( -89.80356045261119391, -38.51850677248155108, 200.5196326713219719 ) ) ;
#69639 = ORIENTED_EDGE ( 'NONE', *, *, #6649, .F. ) ;
#69640 = DIRECTION ( 'NONE',  ( 0.000000000000000000, -1.000000000000000000, 0.000000000000000000 ) ) ;
#69641 = CARTESIAN_POINT ( 'NONE',  ( -18.91882844845346767, 48.67754231730402381, 62.16217783403399721 ) ) ;
#69642 = CARTESIAN_POINT ( 'NONE',  ( 6.661997535587873998, 40.29425722526258369, -71.19925417846640414 ) ) ;
#69643 = CARTESIAN_POINT ( 'NONE',  ( 23.13430097919854944, 28.13531915807118367, 30.70617127781017786 ) ) ;
#69644 = SURFACE_STYLE_USAGE ( .BOTH. , #45898 ) ;
#69645 = FACE_OUTER_BOUND ( 'NONE', #68801, .T. ) ;
#69646 = CARTESIAN_POINT ( 'NONE',  ( 112.1210090530907024, -60.00000000000002132, 177.5107359543562779 ) ) ;
#69647 = CIRCLE ( 'NONE', #100662, 12.00000000000000711 ) ;
#69648 = CARTESIAN_POINT ( 'NONE',  ( 0.000000000000000000, 6.123233995736767268E-16, -5.000000000000000888 ) ) ;
#69649 = ORIENTED_EDGE ( 'NONE', *, *, #55868, .F. ) ;
#69650 = EDGE_CURVE ( 'NONE', #16458, #11369, #89336, .T. ) ;
#69651 = CARTESIAN_POINT ( 'NONE',  ( 89.93133926947346879, 1.016364837396684119E-14, 0.000000000000000000 ) ) ;
#69652 = AXIS2_PLACEMENT_3D ( 'NONE', #101115, #84409, #26214 ) ;
#69653 = AXIS2_PLACEMENT_3D ( 'NONE', #61991, #78655, #12337 ) ;
#69654 = CARTESIAN_POINT ( 'NONE',  ( -81.60154244327691231, -30.00000000000000000, -6.159883939146816090 ) ) ;
#69655 = ORIENTED_EDGE ( 'NONE', *, *, #64694, .T. ) ;
#69657 = CARTESIAN_POINT ( 'NONE',  ( 5.105411401488612277, -2.846505860404147104, -18.47274186656556338 ) ) ;
#69656 = CARTESIAN_POINT ( 'NONE',  ( -64.84495818255328459, -38.33846756661721855, 112.5933220119225666 ) ) ;
#69658 = DIRECTION ( 'NONE',  ( 1.000000000000000000, 1.224606353822377258E-16, 0.000000000000000000 ) ) ;
#69659 = CARTESIAN_POINT ( 'NONE',  ( 6.288404560131952259, 5.029641972278930062, -0.4504974108211907136 ) ) ;
#69660 = CARTESIAN_POINT ( 'NONE',  ( 39.42238789698090784, 436.7568662985880792, 5.264481638451717238 ) ) ;
#69661 = CARTESIAN_POINT ( 'NONE',  ( 2.977408999572651815, -12.31250000204838635, 7.188101187500000933 ) ) ;
#69662 = CARTESIAN_POINT ( 'NONE',  ( -11.99999999999999467, -5.000000000000002665, -83.42920367502566137 ) ) ;
#69663 = CARTESIAN_POINT ( 'NONE',  ( -43.02621584241282449, 434.6128289108255558, 16.97888786059002086 ) ) ;
#69664 = ORIENTED_EDGE ( 'NONE', *, *, #74452, .F. ) ;
#69665 = CARTESIAN_POINT ( 'NONE',  ( 82.28231359831326586, -46.46483616827516272, 174.1978786872764431 ) ) ;
#69666 = CARTESIAN_POINT ( 'NONE',  ( -27.99999999999999645, 0.000000000000000000, 9.000000000000000000 ) ) ;
#69667 = CARTESIAN_POINT ( 'NONE',  ( 9.999952458099484076, 88.99988114523867466, 0.2653554233229086234 ) ) ;
#69668 = ORIENTED_EDGE ( 'NONE', *, *, #2564, .T. ) ;
#69669 = CARTESIAN_POINT ( 'NONE',  ( -32.89392925374600907, 485.8745504891352311, 5.316642333917223517 ) ) ;
#69670 = CARTESIAN_POINT ( 'NONE',  ( -46.77788840983944141, 18.69141115048825696, 15.65052543522504891 ) ) ;
#69671 = DIRECTION ( 'NONE',  ( 1.224646799147352468E-16, 0.000000000000000000, -1.000000000000000000 ) ) ;
#69672 = FILL_AREA_STYLE_COLOUR ( '', #29620 ) ;
#69673 = CARTESIAN_POINT ( 'NONE',  ( 0.5330506804320168657, 13.17793295771842210, 51.63720770525478088 ) ) ;
#69674 = CARTESIAN_POINT ( 'NONE',  ( 9.699093171307941574, 2.767019883226315091, 14.74275178253622265 ) ) ;
#69675 = EDGE_CURVE ( 'NONE', #88866, #34973, #41232, .T. ) ;
#69676 = VERTEX_POINT ( 'NONE', #88810 ) ;
#69677 = COLOUR_RGB ( '', 0.72549020, 0.75294118, 0.79215686) ;
#69678 =( NAMED_UNIT ( * ) SI_UNIT ( $, .STERADIAN. ) SOLID_ANGLE_UNIT ( ) );
#69679 = CARTESIAN_POINT ( 'NONE',  ( -76.11217929027031914, -30.00000000000000355, -17.27491633377325186 ) ) ;
#69680 = DIRECTION ( 'NONE',  ( 0.000000000000000000, -1.000000000000000000, 0.000000000000000000 ) ) ;
#69681 = CARTESIAN_POINT ( 'NONE',  ( 6.123233995736766282E-16, 0.000000000000000000, -5.000000000000000000 ) ) ;
#69682 = EDGE_CURVE ( 'NONE', #31711, #100365, #101522, .T. ) ;
#69684 = SURFACE_STYLE_USAGE ( .BOTH. , #93435 ) ;
#69683 = CARTESIAN_POINT ( 'NONE',  ( 13.09999999999999787, 3.309500000000003439, 4.052968581778167743E-16 ) ) ;
#69685 = B_SPLINE_CURVE_WITH_KNOTS ( 'NONE', 3,
 ( #19554, #52391, #11389, #106237, #14047, #105718, #47479, #16180, #39940, #23241, #14573, #79851, #7543, #55035, #65269, #90073, #89021, #39420, #48004, #30814, #104662, #56079, #64228, #97617, #5446, #6489, #63700, #87967, #40459, #46951, #98159, #81429, #80377, #72295 ),
 .UNSPECIFIED., .F., .F.,
 ( 4, 2, 2, 2, 2, 2, 2, 2, 2, 2, 2, 2, 2, 2, 2, 2, 4 ),
 ( 0.01263964810480761557, 0.01342907106096845327, 0.01421849401712929097, 0.01500791697329012866, 0.01579733992945096810, 0.01658676288561180406, 0.01737618584177264350, 0.01816560879793347946, 0.01895503175409431890, 0.01974445471025515486, 0.02053387766641599430, 0.02132330062257683373, 0.02211272357873766969, 0.02290214653489850566, 0.02369156949105934509, 0.02448099244722018453, 0.02527041540338102049 ),
 .UNSPECIFIED. ) ;
#69686 = CIRCLE ( 'NONE', #105853, 8.400000000000000355 ) ;
#69687 = CARTESIAN_POINT ( 'NONE',  ( -7.188101187500002709, -24.31250000204838813, 2.977408999572648707 ) ) ;
#69688 = DIRECTION ( 'NONE',  ( 0.000000000000000000, 1.000000000000000000, -1.224646799147353207E-16 ) ) ;
#69689 = CONICAL_SURFACE ( 'NONE', #26682, 5.000000000000001776, 0.9599310885968803664 ) ;
#69690 = AXIS2_PLACEMENT_3D ( 'NONE', #90402, #74198, #32174 ) ;
#69691 = CARTESIAN_POINT ( 'NONE',  ( 7.996135855217748833, -5.000000000000000000, -6.145819459791736605 ) ) ;
#69692 = CARTESIAN_POINT ( 'NONE',  ( 12.79230769230769305, -4.171999999999999709, 0.000000000000000000 ) ) ;
#69693 = COLOUR_RGB ( '', 0.66274510, 0.83137255, 0.94901961) ;
#69694 = ITEM_DEFINED_TRANSFORMATION ( 'NONE', 'NONE', #40372,  #10728 ) ;
#69695 = ORIENTED_EDGE ( 'NONE', *, *, #4269, .F. ) ;
#69696 = EDGE_CURVE ( 'NONE', #19990, #43284, #80866, .T. ) ;
#69697 = CARTESIAN_POINT ( 'NONE',  ( -35.15980092189356299, 490.3457513104292502, 12.17002836721590953 ) ) ;
#69698 = DIRECTION ( 'NONE',  ( 0.000000000000000000, 0.000000000000000000, -1.000000000000000000 ) ) ;
#69699 = CARTESIAN_POINT ( 'NONE',  ( -9.248416039723647231, 11.93391985749765105, -3.173712385738878837E-13 ) ) ;
#69700 = SURFACE_STYLE_FILL_AREA ( #38406 ) ;
#69701 = ORIENTED_EDGE ( 'NONE', *, *, #65703, .F. ) ;
#69702 = CARTESIAN_POINT ( 'NONE',  ( 37.52433673132330938, 473.0012850594927727, 17.54962685244640141 ) ) ;
#69703 = CARTESIAN_POINT ( 'NONE',  ( -4.707696486725459373, 48.00000000000000000, -99.43546650845934209 ) ) ;
#69704 = VERTEX_POINT ( 'NONE', #6818 ) ;
#69705 = CARTESIAN_POINT ( 'NONE',  ( -27.86245019093637154, 34.24933485205252026, 9.804843171747192443 ) ) ;
#69706 = CARTESIAN_POINT ( 'NONE',  ( -0.1583024797166763253, 13.70447791526913939, -49.24999999999997158 ) ) ;
#69707 = DIRECTION ( 'NONE',  ( -0.5735764363510497121, 0.8191520442889892450, 1.003171929053521665E-16 ) ) ;
#69708 = CARTESIAN_POINT ( 'NONE',  ( -18.00376551885552345, 36.46870192104549346, 23.09987717863819157 ) ) ;
#69709 = CARTESIAN_POINT ( 'NONE',  ( -112.0091148159200856, -60.00000000000000000, 179.5044317187202125 ) ) ;
#69710 = CARTESIAN_POINT ( 'NONE',  ( 19.48249511158978464, 49.99632329422010457, 60.25369351552480168 ) ) ;
#69711 = CARTESIAN_POINT ( 'NONE',  ( 0.01688885742776657928, -7.321065037175427115, -3.319543390096029611 ) ) ;
#69712 = CARTESIAN_POINT ( 'NONE',  ( 5.623709101673032507, 53.42003182002678585, -8.497490178355675994 ) ) ;
#69713 = FILL_AREA_STYLE ('',( #4434 ) ) ;
#69714 = CARTESIAN_POINT ( 'NONE',  ( -86.00678846258095689, -21.65130990580026449, 173.2951746391152881 ) ) ;
#69715 = CARTESIAN_POINT ( 'NONE',  ( 34.58711029377568735, 42.66036566261906415, -62.95058470269599127 ) ) ;
#69716 =( BOUNDED_SURFACE ( )  B_SPLINE_SURFACE ( 3, 2, ( 
 ( #8853, #8323, #91390 ),
 ( #67108, #41227, #81662 ),
 ( #99449, #24551, #66036 ),
 ( #25624, #7256, #90851 ),
 ( #50369, #75173, #48770 ),
 ( #16969, #40166, #73040 ),
 ( #32095, #64975, #49845 ),
 ( #7785, #106481, #65511 ),
 ( #74644, #9369, #83280 ),
 ( #42285, #28276, #44973 ),
 ( #2882, #36900, #92424 ),
 ( #52499, #43362, #28819 ) ),
 .UNSPECIFIED., .F., .F., .T. ) 
 B_SPLINE_SURFACE_WITH_KNOTS ( ( 4, 2, 2, 2, 2, 4 ),
 ( 3, 3 ),
 ( 0.01002139624728706942, 0.01516190422318156386, 0.01580446772016837892, 0.01644703121715519051, 0.01773215821112881369, 0.02030241219907606004 ),
 ( 0.000000000000000000, 1.000000000000000000 ),
 .UNSPECIFIED. ) 
 GEOMETRIC_REPRESENTATION_ITEM ( )  RATIONAL_B_SPLINE_SURFACE ( (
 ( 1.000000000000000000, 0.7071066567438631933, 1.000000000000000000),
 ( 1.000000000000000000, 0.7071033631374191719, 1.000000000000000000),
 ( 1.000000000000000000, 0.7071056790687298976, 1.000000000000000000),
 ( 1.000000000000000000, 0.7071068249174177200, 1.000000000000000000),
 ( 1.000000000000000000, 0.7071068699167430971, 1.000000000000000000),
 ( 1.000000000000000000, 0.7071037064177418952, 1.000000000000000000),
 ( 1.000000000000000000, 0.7071011095179403627, 1.000000000000000000),
 ( 1.000000000000000000, 0.7070931123324023515, 1.000000000000000000),
 ( 1.000000000000000000, 0.7070878456073813600, 1.000000000000000000),
 ( 1.000000000000000000, 0.7070844322698651707, 1.000000000000000000),
 ( 1.000000000000000000, 0.7071028863112219787, 1.000000000000000000),
 ( 1.000000000000000000, 0.7071067811865477948, 1.000000000000000000) ) ) 
 REPRESENTATION_ITEM ( '' )  SURFACE ( )  );
#69717 = AXIS2_PLACEMENT_3D ( 'NONE', #50944, #83858, #77371 ) ;
#69718 = ORIENTED_EDGE ( 'NONE', *, *, #6613, .T. ) ;
#69719 = CARTESIAN_POINT ( 'NONE',  ( -1.469576158976823947E-15, -26.56250000409677270, 8.000000000000000000 ) ) ;
#69720 = EDGE_CURVE ( 'NONE', #27940, #78362, #85529, .T. ) ;
#69721 = FILL_AREA_STYLE ('',( #63226 ) ) ;
#69722 = CARTESIAN_POINT ( 'NONE',  ( -83.72505494025215000, -45.26660870684003868, 8.238952501196534328 ) ) ;
#69723 = CARTESIAN_POINT ( 'NONE',  ( 0.000000000000000000, 0.000000000000000000, -5.185501489199872083 ) ) ;
#69724 = CARTESIAN_POINT ( 'NONE',  ( 1.224646799147353256E-15, -1.500000000000000000, -10.00000000000000000 ) ) ;
#69725 = CARTESIAN_POINT ( 'NONE',  ( 3.996239228618861272, 136.8763022136764675, -4.999999999999999112 ) ) ;
#69726 = CARTESIAN_POINT ( 'NONE',  ( 109.3513501059324255, -30.00000000000000000, 179.6549720493207190 ) ) ;
#69727 = CARTESIAN_POINT ( 'NONE',  ( 59.23741894013591036, 42.00000000000000711, 7.754160006506985781 ) ) ;
#69728 = ADVANCED_FACE ( 'NONE', ( #38682 ), #88308, .F. ) ;
#69729 = CARTESIAN_POINT ( 'NONE',  ( 75.88724551625310255, -29.99999999999989697, 164.4338130987444231 ) ) ;
#69730 = CARTESIAN_POINT ( 'NONE',  ( -82.74168755217822024, -14.21045842199452203, -19.52755005266771349 ) ) ;
#69731 = CARTESIAN_POINT ( 'NONE',  ( -63.48454154046918774, -53.39210001124775573, 88.97591336427868214 ) ) ;
#69732 = EDGE_LOOP ( 'NONE', ( #76597, #103997, #97456, #102344 ) ) ;
#69733 = CARTESIAN_POINT ( 'NONE',  ( 104.0082629745172653, -14.21045842199441012, 192.0643512960946282 ) ) ;
#69734 = CARTESIAN_POINT ( 'NONE',  ( -14.79739047843293598, 40.83920300364216160, 63.36299633484923532 ) ) ;
#69735 = CARTESIAN_POINT ( 'NONE',  ( 31.23755223876165132, -60.00000000000493827, 46.45901925853441128 ) ) ;
#69736 = ORIENTED_EDGE ( 'NONE', *, *, #91290, .F. ) ;
#69737 = CARTESIAN_POINT ( 'NONE',  ( 5.833333333333329485, -46.00000000000000000, 103.8776713793258608 ) ) ;
#69738 = CARTESIAN_POINT ( 'NONE',  ( 7.188101187500000044, -24.03125000204838457, 0.000000000000000000 ) ) ;
#69739 = CARTESIAN_POINT ( 'NONE',  ( -5.191144708981717315, -7.359699144787327008, 3.015512395308848514 ) ) ;
#69740 = ORIENTED_EDGE ( 'NONE', *, *, #33526, .F. ) ;
#69741 = CARTESIAN_POINT ( 'NONE',  ( 58.92761780597729881, 6.856755485862130937E-15, 0.000000000000000000 ) ) ;
#69742 = ORIENTED_EDGE ( 'NONE', *, *, #25025, .F. ) ;
#69743 = DIRECTION ( 'NONE',  ( -0.000000000000000000, 1.000000000000000000, -0.000000000000000000 ) ) ;
#69744 = CARTESIAN_POINT ( 'NONE',  ( -38.63430842791193243, 485.8001267274091219, -4.834053598480790193 ) ) ;
#69745 = CARTESIAN_POINT ( 'NONE',  ( -79.05509554772149272, -60.00000000000000000, -28.49194458007684005 ) ) ;
#69746 = CARTESIAN_POINT ( 'NONE',  ( 21.85376215082057882, 304.0607632025936482, -9.955599711602641122 ) ) ;
#69747 = CARTESIAN_POINT ( 'NONE',  ( 7.188101187500001821, -34.43750000204838813, -2.977408999572650483 ) ) ;
#69748 = DIRECTION ( 'NONE',  ( 0.000000000000000000, -1.000000000000000000, 0.000000000000000000 ) ) ;
#69749 = SURFACE_STYLE_USAGE ( .BOTH. , #63256 ) ;
#69750 = CARTESIAN_POINT ( 'NONE',  ( -5.036189802309416486, 49.99999999999999289, -76.26213611588271135 ) ) ;
#69751 = CARTESIAN_POINT ( 'NONE',  ( -7.414346147791995634, 107.6458915766226312, -3.010818766110534117 ) ) ;
#69752 = CARTESIAN_POINT ( 'NONE',  ( 41.20010578034612081, 436.9751675121710832, 5.754626909168208293 ) ) ;
#69753 = ADVANCED_FACE ( 'NONE', ( #55873 ), #1632, .T. ) ;
#69754 = CONICAL_SURFACE ( 'NONE', #23262, 4.000000000000001776, 0.9599310885968774798 ) ;
#69755 = EDGE_LOOP ( 'NONE', ( #65760, #9883, #63359, #93416 ) ) ;
#69756 = CARTESIAN_POINT ( 'NONE',  ( 5.164787682159539983, -1.887557197826887689, 104.1470044518085416 ) ) ;
#69758 = CARTESIAN_POINT ( 'NONE',  ( 34.57993830756027620, -60.29654495889643329, 39.05213902588479158 ) ) ;
#69757 = CARTESIAN_POINT ( 'NONE',  ( 19.29515645702225868, 1.482358050883964840E-15, 0.000000000000000000 ) ) ;
#69759 = CARTESIAN_POINT ( 'NONE',  ( -6.601913983200961233, -4.285714285712858285, -24.56594385547797543 ) ) ;
#69760 = ORIENTED_EDGE ( 'NONE', *, *, #31519, .F. ) ;
#69762 = CARTESIAN_POINT ( 'NONE',  ( -23.13495288362992852, 25.26989808490225542, -33.20617127781031996 ) ) ;
#69761 = B_SPLINE_CURVE_WITH_KNOTS ( 'NONE', 3,
 ( #79414, #30357, #56715, #9228 ),
 .UNSPECIFIED., .F., .F.,
 ( 4, 4 ),
 ( 0.000000000000000000, 0.001949579373386174088 ),
 .UNSPECIFIED. ) ;
#69763 = CIRCLE ( 'NONE', #104156, 4.000000000000001776 ) ;
#69765 = FACE_OUTER_BOUND ( 'NONE', #1971, .T. ) ;
#69764 =( NAMED_UNIT ( * ) SI_UNIT ( $, .STERADIAN. ) SOLID_ANGLE_UNIT ( ) );
#69766 = CARTESIAN_POINT ( 'NONE',  ( 41.85000000000000142, 1.533819458162526451E-15, 0.000000000000000000 ) ) ;
#69767 = CARTESIAN_POINT ( 'NONE',  ( -43.68566140668959008, 485.0560336449534589, 1.938913452014765282 ) ) ;
#69768 = AXIS2_PLACEMENT_3D ( 'NONE', #20334, #53180, #15891 ) ;
#69769 = VECTOR ( 'NONE', #49671, 1000.000000000000227 ) ;
#69770 = AXIS2_PLACEMENT_3D ( 'NONE', #46229, #55354, #39732 ) ;
#69771 = CARTESIAN_POINT ( 'NONE',  ( 30.59999999999999787, 1.533819458162526451E-15, 0.000000000000000000 ) ) ;
#69772 = CARTESIAN_POINT ( 'NONE',  ( -7.500000000000000000, -7.155734338404329264E-15, -6.991905250253754645 ) ) ;
#69773 = ORIENTED_EDGE ( 'NONE', *, *, #135, .F. ) ;
#69774 = CARTESIAN_POINT ( 'NONE',  ( 92.43235373876116512, -60.00000000000000711, -0.2938010258920950579 ) ) ;
#69775 = CARTESIAN_POINT ( 'NONE',  ( -10.61203977153288136, 46.03732009579939444, -12.94024766200783993 ) ) ;
#69776 = VECTOR ( 'NONE', #104623, 1000.000000000000114 ) ;
#69777 = FACE_OUTER_BOUND ( 'NONE', #5250, .T. ) ;
#69778 = STYLED_ITEM ( 'NONE', ( #27931 ), #13402 ) ;
#69779 = CARTESIAN_POINT ( 'NONE',  ( -6.743821053489263306, 40.92373723432427113, -71.01439601632299059 ) ) ;
#69780 = CARTESIAN_POINT ( 'NONE',  ( -14.29190075644363489, 21.26710225492988116, -5.626279437295411689 ) ) ;
#69781 = EDGE_LOOP ( 'NONE', ( #52104, #43136 ) ) ;
#69782 = CARTESIAN_POINT ( 'NONE',  ( -89.68653756732776117, -29.99999999999227640, 199.1857044332254247 ) ) ;
#69783 = ORIENTED_EDGE ( 'NONE', *, *, #43186, .T. ) ;
#69784 = CARTESIAN_POINT ( 'NONE',  ( -9.677525045153895888, -57.01317935973843731, 24.47381311117452185 ) ) ;
#69785 = DIRECTION ( 'NONE',  ( -0.000000000000000000, -0.000000000000000000, 1.000000000000000000 ) ) ;
#69786 = CARTESIAN_POINT ( 'NONE',  ( 82.26020361419449500, -37.81322313179484951, -13.24491807084091555 ) ) ;
#69787 = CARTESIAN_POINT ( 'NONE',  ( 7.188101187500000044, -28.53125000204838813, 0.000000000000000000 ) ) ;
#69788 = CARTESIAN_POINT ( 'NONE',  ( -17.85455871053495969, 34.57759917020306517, 22.38743647938886383 ) ) ;
#69789 = CARTESIAN_POINT ( 'NONE',  ( -5.744562646538029504, 12.99999999999999289, 4.000000000000000000 ) ) ;
#69790 = ORIENTED_EDGE ( 'NONE', *, *, #33519, .T. ) ;
#69791 = CARTESIAN_POINT ( 'NONE',  ( 32.86203668624279572, 471.3274586220275069, 9.717589530844561452 ) ) ;
#69792 = ORIENTED_EDGE ( 'NONE', *, *, #21610, .F. ) ;
#69793 = CARTESIAN_POINT ( 'NONE',  ( 48.28084718957915555, 9.217476947337159388, -16.83779905917619502 ) ) ;
#69795 = ORIENTED_EDGE ( 'NONE', *, *, #89523, .F. ) ;
#69794 = DIRECTION ( 'NONE',  ( -0.9639005798656382629, -0.1664520902833319382, -0.2078205326116645268 ) ) ;
#69796 = CARTESIAN_POINT ( 'NONE',  ( 77.45305305485931058, -42.96330883344779039, 134.7310727137066522 ) ) ;
#69797 = ORIENTED_EDGE ( 'NONE', *, *, #68412, .F. ) ;
#69798 = CARTESIAN_POINT ( 'NONE',  ( 2.800738256643207524, -53.57001856701707965, 40.71845537227009970 ) ) ;
#69799 = CARTESIAN_POINT ( 'NONE',  ( -7.188101187500002709, -19.81250000204838457, 2.977408999572647819 ) ) ;
#69800 = VECTOR ( 'NONE', #74571, 1000.000000000000000 ) ;
#69801 = CARTESIAN_POINT ( 'NONE',  ( -80.45353917958989598, -57.50988970295517788, 199.2734438750461550 ) ) ;
#69802 = EDGE_CURVE ( 'NONE', #12254, #42044, #48147, .T. ) ;
#69803 = VERTEX_POINT ( 'NONE', #95848 ) ;
#69804 = CARTESIAN_POINT ( 'NONE',  ( -5.384233811324312668, -13.00217091344775255, 2.655407383564611923 ) ) ;
#69805 = CARTESIAN_POINT ( 'NONE',  ( -9.221346651730840449, 83.95165979931661582, -3.869102247876030631 ) ) ;
#69806 = EDGE_CURVE ( 'NONE', #87625, #101359, #61978, .T. ) ;
#69807 = CARTESIAN_POINT ( 'NONE',  ( 14.83349330513380337, 1.593028355512270567E-15, 0.000000000000000000 ) ) ;
#69808 = CARTESIAN_POINT ( 'NONE',  ( -8.000000000000000000, -16.43750000409677270, -9.797174393178825657E-16 ) ) ;
#69809 = CARTESIAN_POINT ( 'NONE',  ( -45.16073431462941556, -28.35099063806825725, 40.24582607710122062 ) ) ;
#69810 = CARTESIAN_POINT ( 'NONE',  ( 9.216463528758549018, 15.13241195026089692, 3.884543032214307079 ) ) ;
#69811 = CYLINDRICAL_SURFACE ( 'NONE', #29361, 7.000000000000000000 ) ;
#69812 = CARTESIAN_POINT ( 'NONE',  ( 0.000000000000000000, 8.660254037844390851, -0.9999999999999974465 ) ) ;
#69813 = CARTESIAN_POINT ( 'NONE',  ( -43.74985542820371620, 435.5770091380364306, 16.96136490515579354 ) ) ;
#69814 = VECTOR ( 'NONE', #17432, 1000.000000000000000 ) ;
#69815 =( LENGTH_UNIT ( ) NAMED_UNIT ( * ) SI_UNIT ( .MILLI., .METRE. ) );
#69816 = CARTESIAN_POINT ( 'NONE',  ( -12.37144696128342147, -4.000000000000003553, 20.44658103856077602 ) ) ;
#69817 = ORIENTED_EDGE ( 'NONE', *, *, #41743, .T. ) ;
#69818 = CARTESIAN_POINT ( 'NONE',  ( -5.715067606001751344, -50.89645767963700251, 39.78281718566972103 ) ) ;
#69819 = EDGE_CURVE ( 'NONE', #65536, #59024, #44718, .T. ) ;
#69820 = CARTESIAN_POINT ( 'NONE',  ( 12.29798915171414819, -4.463815859616105719, -12.75153713776963293 ) ) ;
#69821 = CARTESIAN_POINT ( 'NONE',  ( 0.8476627094018533981, 12.94087125257734350, 49.56336647345505497 ) ) ;
#69822 = CARTESIAN_POINT ( 'NONE',  ( 69.36755836386646479, -30.21241150966188016, -29.99922498068983145 ) ) ;
#69823 = CARTESIAN_POINT ( 'NONE',  ( -69.99800859030240474, -30.00000000000000355, 95.31859612160674544 ) ) ;
#69824 = CARTESIAN_POINT ( 'NONE',  ( 7.500000000000007105, 40.00000000000000000, -65.90297133634214788 ) ) ;
#69825 = CIRCLE ( 'NONE', #4375, 8.000000000000000000 ) ;
#69826 = ORIENTED_EDGE ( 'NONE', *, *, #27995, .T. ) ;
#69827 = CARTESIAN_POINT ( 'NONE',  ( -27.10511071441333542, 36.88665068479732412, -7.556984339679825524 ) ) ;
#69828 = CARTESIAN_POINT ( 'NONE',  ( 74.87226039639872965, -57.58023860409628725, 190.2883175146000383 ) ) ;
#69829 = CIRCLE ( 'NONE', #25033, 5.000000000000000888 ) ;
#69830 = CARTESIAN_POINT ( 'NONE',  ( 7.996668423981797780, 48.00000000000000711, -91.14546719974913458 ) ) ;
#69831 = CARTESIAN_POINT ( 'NONE',  ( -4.574783636564919931, -5.228990388887491569, -6.171384342982614513 ) ) ;
#69832 = CARTESIAN_POINT ( 'NONE',  ( 27.61650669486618881, 1.474610560812782335E-15, 0.000000000000000000 ) ) ;
#69833 = VECTOR ( 'NONE', #73812, 1000.000000000000000 ) ;
#69834 = DIRECTION ( 'NONE',  ( -1.000000000000000000, 0.000000000000000000, 0.000000000000000000 ) ) ;
#69835 = CARTESIAN_POINT ( 'NONE',  ( -50.05807582380210619, -60.00000000000000711, 71.95124345659672827 ) ) ;
#69836 = AXIS2_PLACEMENT_3D ( 'NONE', #51440, #59019, #67644 ) ;
#69837 = AXIS2_PLACEMENT_3D ( 'NONE', #54303, #60852, #79137 ) ;
#69838 = CIRCLE ( 'NONE', #62990, 4.000000000000001776 ) ;
#69839 = CARTESIAN_POINT ( 'NONE',  ( 0.000000000000000000, 152.0000000000000000, -5.000000000000000000 ) ) ;
#69840 = CIRCLE ( 'NONE', #19921, 8.000000000000000000 ) ;
#69841 = CARTESIAN_POINT ( 'NONE',  ( -86.09249853775514794, -31.93869936210829508, 184.2230114830187517 ) ) ;
#69842 = ORIENTED_EDGE ( 'NONE', *, *, #87171, .F. ) ;
#69843 = CARTESIAN_POINT ( 'NONE',  ( 35.52727618412238542, 408.9004372220593950, 7.035618409970155973 ) ) ;
#69844 = CARTESIAN_POINT ( 'NONE',  ( -3.977975743268641118, -22.06767091311041540, 27.56089423025632001 ) ) ;
#69845 = CIRCLE ( 'NONE', #49100, 2.000000000000000000 ) ;
#69846 = CARTESIAN_POINT ( 'NONE',  ( -6.592587276917421413, 41.82481063595618309, -59.20696655526094787 ) ) ;
#69847 = CARTESIAN_POINT ( 'NONE',  ( -3.400000000000000355, 4.163799117101001052E-16, -1.581124522925831499 ) ) ;
#69848 = DIRECTION ( 'NONE',  ( 0.000000000000000000, -1.000000000000000000, 0.000000000000000000 ) ) ;
#69849 = EDGE_CURVE ( 'NONE', #15839, #100346, #35304, .T. ) ;
#69850 = CARTESIAN_POINT ( 'NONE',  ( 29.87930712590254956, 10.71892156097790583, 14.93965356295126945 ) ) ;
#69851 = CARTESIAN_POINT ( 'NONE',  ( 37.62595466100172814, 491.2446780561967330, 12.18850516984547561 ) ) ;
#69852 = DIRECTION ( 'NONE',  ( 0.000000000000000000, -1.000000000000000000, 0.000000000000000000 ) ) ;
#69853 = DIRECTION ( 'NONE',  ( -1.000000000000000000, -1.224606353822377258E-16, -0.000000000000000000 ) ) ;
#69854 = ORIENTED_EDGE ( 'NONE', *, *, #66181, .F. ) ;
#69855 = CARTESIAN_POINT ( 'NONE',  ( 26.06898045364747318, 295.8628383591220086, -9.782693099516677648 ) ) ;
#69856 = CARTESIAN_POINT ( 'NONE',  ( 10.71636377871695700, 18.38929554378958287, 9.346910711729506716 ) ) ;
#69857 = EDGE_CURVE ( 'NONE', #6171, #80946, #98998, .T. ) ;
#69858 = EDGE_CURVE ( 'NONE', #44397, #70179, #17324, .T. ) ;
#69859 = CARTESIAN_POINT ( 'NONE',  ( -5.820808985964939453, -8.673617379884035472E-16, 21.65942590380532451 ) ) ;
#69860 = CARTESIAN_POINT ( 'NONE',  ( 80.40000000000000568, -4.171999999999998820, 5.616230220889773285E-16 ) ) ;
#69861 = CARTESIAN_POINT ( 'NONE',  ( 89.80793189580856506, -29.99999999999993250, 26.19443836851201723 ) ) ;
#69862 = CARTESIAN_POINT ( 'NONE',  ( -80.30188067886301440, -39.50080336238898582, 147.7263073883484310 ) ) ;
#69863 = ORIENTED_EDGE ( 'NONE', *, *, #61242, .F. ) ;
#69864 = DIRECTION ( 'NONE',  ( 0.000000000000000000, -1.000000000000000000, 0.000000000000000000 ) ) ;
#69865 = CARTESIAN_POINT ( 'NONE',  ( 4.472135954999579610, 249.9999999999999716, -4.000000000000002665 ) ) ;
#69866 = CARTESIAN_POINT ( 'NONE',  ( 46.16030844547664458, -57.68192973205171370, 67.73425372236864916 ) ) ;
#69867 = CARTESIAN_POINT ( 'NONE',  ( 0.01372220897661700217, 5.948365447239582160, 2.697128823393880825 ) ) ;
#69868 = CARTESIAN_POINT ( 'NONE',  ( 35.78055020979645207, 327.7515353362224459, -3.901225659782328492 ) ) ;
#69869 = DIRECTION ( 'NONE',  ( -1.000000000000000000, -0.000000000000000000, -0.000000000000000000 ) ) ;
#69870 = EDGE_LOOP ( 'NONE', ( #3368, #91720, #86671, #33262, #32224, #92809, #41369, #4637 ) ) ;
#69871 = CARTESIAN_POINT ( 'NONE',  ( -12.08334041755991706, 304.5866437775407007, -10.05636128505472549 ) ) ;
#69872 = CARTESIAN_POINT ( 'NONE',  ( 30.98507422220691154, 439.0250405275747880, 22.25274580565829297 ) ) ;
#69873 = CARTESIAN_POINT ( 'NONE',  ( 7.188101187500001821, -23.56250000204838813, -2.977408999572650483 ) ) ;
#69874 = ORIENTED_EDGE ( 'NONE', *, *, #62426, .F. ) ;
#69875 = VECTOR ( 'NONE', #87867, 1000.000000000000000 ) ;
#69876 = CARTESIAN_POINT ( 'NONE',  ( -5.656854249492379694, -23.93749999999999289, -5.656854249492380582 ) ) ;
#69877 = CARTESIAN_POINT ( 'NONE',  ( 6.804095789962234520, 41.75280167785350471, -69.96721248597626186 ) ) ;
#69878 = FACE_OUTER_BOUND ( 'NONE', #34090, .T. ) ;
#69879 = CARTESIAN_POINT ( 'NONE',  ( -5.656854249492381470, -17.56249999999999645, 5.656854249492379694 ) ) ;
#69880 = EDGE_CURVE ( 'NONE', #30792, #99128, #104986, .T. ) ;
#69881 = SURFACE_STYLE_FILL_AREA ( #4085 ) ;
#69882 = ORIENTED_EDGE ( 'NONE', *, *, #63996, .F. ) ;
#69883 = CARTESIAN_POINT ( 'NONE',  ( 92.74728809772592797, -60.00000000000000000, -7.135771891692349378 ) ) ;
#69885 = CARTESIAN_POINT ( 'NONE',  ( 27.03448325452836443, -18.62296646550320389, 28.59903465579650828 ) ) ;
#69884 = CARTESIAN_POINT ( 'NONE',  ( -68.99627713242672655, -30.00000000000000355, 123.4899896973233808 ) ) ;
#69886 = CARTESIAN_POINT ( 'NONE',  ( 2.291854088684162271E-15, 61.34242035161803841, -9.357204421225127078 ) ) ;
#69887 = ORIENTED_EDGE ( 'NONE', *, *, #93246, .T. ) ;
#69888 = EDGE_CURVE ( 'NONE', #101431, #41831, #27679, .T. ) ;
#69889 = CARTESIAN_POINT ( 'NONE',  ( -34.65605967281282318, -18.71474442840510477, 31.05779364914194929 ) ) ;
#69890 = UNCERTAINTY_MEASURE_WITH_UNIT (LENGTH_MEASURE( 1.000000000000000082E-05 ), #75813, 'distance_accuracy_value', 'NONE');
#69891 = EDGE_LOOP ( 'NONE', ( #39696, #97873, #24944, #66984, #77298 ) ) ;
#69892 = CARTESIAN_POINT ( 'NONE',  ( -20.05453516056601515, -4.285714285714296246, -15.38541618194247995 ) ) ;
#69893 = CARTESIAN_POINT ( 'NONE',  ( -43.70836520789971757, 463.8610993545743213, 7.295416580046127031 ) ) ;
#69894 = CARTESIAN_POINT ( 'NONE',  ( -33.21599328327232570, 465.5375697722676023, 9.463303254740058179 ) ) ;
#69895 = EDGE_CURVE ( 'NONE', #101817, #21035, #85513, .T. ) ;
#69896 = CARTESIAN_POINT ( 'NONE',  ( 7.800703710507054467, -61.41404307342057933, 1.791736796405273946 ) ) ;
#69897 = SURFACE_STYLE_FILL_AREA ( #68304 ) ;
#69898 = ORIENTED_EDGE ( 'NONE', *, *, #42692, .T. ) ;
#69899 = CARTESIAN_POINT ( 'NONE',  ( -68.79315106226179921, -38.33280406146015906, 128.9874879556798248 ) ) ;
#69900 = CARTESIAN_POINT ( 'NONE',  ( 95.57908735654217480, -29.99999999999999289, 121.4573267557989595 ) ) ;
#69901 = CARTESIAN_POINT ( 'NONE',  ( 23.97277878003368201, 41.62145744130984326, -74.34290485744733701 ) ) ;
#69902 = CARTESIAN_POINT ( 'NONE',  ( -5.910690929868580135, -81.13504093906810510, -1.065041252563905028 ) ) ;
#69903 = CARTESIAN_POINT ( 'NONE',  ( 81.43457655364417747, -30.00000000000000000, -9.796964337323872840 ) ) ;
#69904 = CARTESIAN_POINT ( 'NONE',  ( 106.4000000000000057, 0.000000000000000000, 4.171999999999999709 ) ) ;
#69905 = ORIENTED_EDGE ( 'NONE', *, *, #64251, .F. ) ;
#69906 = PRESENTATION_LAYER_ASSIGNMENT (  '', '', ( #61289 ) ) ;
#69907 = VERTEX_POINT ( 'NONE', #60195 ) ;
#69908 = ORIENTED_EDGE ( 'NONE', *, *, #61476, .F. ) ;
#69909 = FACE_BOUND ( 'NONE', #59276, .T. ) ;
#69910 = FACE_OUTER_BOUND ( 'NONE', #23628, .T. ) ;
#69911 = LINE ( 'NONE', #86119, #41427 ) ;
#69912 = CARTESIAN_POINT ( 'NONE',  ( -45.42662042998529159, 432.5755707651378543, 6.977826016421777133 ) ) ;
#69913 =( NAMED_UNIT ( * ) PLANE_ANGLE_UNIT ( ) SI_UNIT ( $, .RADIAN. ) );
#69914 = CARTESIAN_POINT ( 'NONE',  ( -7.896165657598944065, -88.78911131371972942, -1.307894402814545831 ) ) ;
#69915 = DIRECTION ( 'NONE',  ( -1.000000000000000000, -1.224606353822377258E-16, -0.000000000000000000 ) ) ;
#69916 = ORIENTED_EDGE ( 'NONE', *, *, #65158, .F. ) ;
#69917 = CARTESIAN_POINT ( 'NONE',  ( 30.29801405241549261, 7.759806510565452342, 41.94638970127574851 ) ) ;
#69918 = ORIENTED_EDGE ( 'NONE', *, *, #32974, .T. ) ;
#69919 =( LENGTH_UNIT ( ) NAMED_UNIT ( * ) SI_UNIT ( .MILLI., .METRE. ) );
#69920 = FILL_AREA_STYLE_COLOUR ( '', #96905 ) ;
#69921 = DIRECTION ( 'NONE',  ( 0.000000000000000000, 0.000000000000000000, 1.000000000000000000 ) ) ;
#69922 = MECHANICAL_DESIGN_GEOMETRIC_PRESENTATION_REPRESENTATION (  '', ( #19985 ), #30278 ) ;
#69923 = PRESENTATION_LAYER_ASSIGNMENT (  '', '', ( #42334 ) ) ;
#69924 = CARTESIAN_POINT ( 'NONE',  ( 22.21815059361560074, 303.2497477512824275, 10.02249569361740988 ) ) ;
#69925 = AXIS2_PLACEMENT_3D ( 'NONE', #68948, #36605, #94275 ) ;
#69926 = AXIS2_PLACEMENT_3D ( 'NONE', #80439, #4982, #55615 ) ;
#69927 = CARTESIAN_POINT ( 'NONE',  ( 4.690999466534710116, 301.0267511969297516, -10.01286717245164937 ) ) ;
#69928 = CARTESIAN_POINT ( 'NONE',  ( 63.57049037775179556, -36.00627426888244287, 80.25959675227277046 ) ) ;
#69929 = ORIENTED_EDGE ( 'NONE', *, *, #88311, .T. ) ;
#69930 = CARTESIAN_POINT ( 'NONE',  ( 28.49081357557730243, 13.12961590422140468, -40.46799408310457125 ) ) ;
#69931 = CARTESIAN_POINT ( 'NONE',  ( -55.68886407967555385, -36.67780875632375626, -35.12440533619799510 ) ) ;
#69932 = CARTESIAN_POINT ( 'NONE',  ( -40.30492368078586196, 437.3365155501883805, 5.155601643837083969 ) ) ;
#69933 = CARTESIAN_POINT ( 'NONE',  ( -9.540582173716337877, 51.45292987738289270, 1.989850725143638810 ) ) ;
#69934 = EDGE_CURVE ( 'NONE', #45750, #30642, #3525, .T. ) ;
#69935 = EDGE_LOOP ( 'NONE', ( #40706, #19360 ) ) ;
#69936 = CARTESIAN_POINT ( 'NONE',  ( 0.000000000000000000, 0.000000000000000000, 0.000000000000000000 ) ) ;
#69937 =( NAMED_UNIT ( * ) SI_UNIT ( $, .STERADIAN. ) SOLID_ANGLE_UNIT ( ) );
#69938 = VECTOR ( 'NONE', #71110, 1000.000000000000000 ) ;
#69939 = ADVANCED_FACE ( 'NONE', ( #92517 ), #53139, .T. ) ;
#69940 = DIRECTION ( 'NONE',  ( 0.000000000000000000, 0.000000000000000000, -1.000000000000000000 ) ) ;
#69941 = EDGE_CURVE ( 'NONE', #102936, #76301, #51527, .T. ) ;
#69942 = CARTESIAN_POINT ( 'NONE',  ( 28.17977184163764193, -5.000000000000000888, 6.123233995736769241E-16 ) ) ;
#69943 = FILL_AREA_STYLE_COLOUR ( '', #48514 ) ;
#69944 = CARTESIAN_POINT ( 'NONE',  ( 85.61863528710425442, -42.90344064078778530, 187.3753977056170470 ) ) ;
#69945 = CARTESIAN_POINT ( 'NONE',  ( -5.346335122799986905, 32.51462932279844864, -50.48019096095612923 ) ) ;
#69946 = CARTESIAN_POINT ( 'NONE',  ( -4.272176768629773136, 11.44367718774164189, 4.999999999999999112 ) ) ;
#69947 = EDGE_LOOP ( 'NONE', ( #32390, #61856, #102876, #71490, #27434, #26316 ) ) ;
#69948 = CARTESIAN_POINT ( 'NONE',  ( 28.03203034650283598, -57.67082107358243093, -43.15016037083558587 ) ) ;
#69949 = CARTESIAN_POINT ( 'NONE',  ( 71.80342808059911874, -29.99999999999997868, -19.71766482350836824 ) ) ;
#69950 = PLANE ( 'NONE',  #88337 ) ;
#69951 = CARTESIAN_POINT ( 'NONE',  ( -6.890281280090280625, 41.03680257558234246, -70.85895802555796763 ) ) ;
#69952 = EDGE_CURVE ( 'NONE', #25223, #32332, #3442, .T. ) ;
#69953 = CARTESIAN_POINT ( 'NONE',  ( 33.97359119245064818, 434.1099241184708148, 11.80501937577158600 ) ) ;
#69954 = AXIS2_PLACEMENT_3D ( 'NONE', #46517, #57773, #91766 ) ;
#69955 = CARTESIAN_POINT ( 'NONE',  ( -100.3088744048629906, -30.00000000000000000, 156.9982617682830153 ) ) ;
#69956 = DIRECTION ( 'NONE',  ( -0.000000000000000000, -1.000000000000000000, -0.000000000000000000 ) ) ;
#69957 = CARTESIAN_POINT ( 'NONE',  ( 19.17204277030731774, -57.67181344388957598, 42.10895013444159218 ) ) ;
#69958 = CARTESIAN_POINT ( 'NONE',  ( -9.380871178326144033, 247.9888362020166426, 3.467392232194195234 ) ) ;
#69959 = CARTESIAN_POINT ( 'NONE',  ( 4.869591400170317996, -52.05062436006488724, 40.13051080525804792 ) ) ;
#69960 = CARTESIAN_POINT ( 'NONE',  ( -18.84132143639387280, 50.00000000000000000, 60.80075852822654525 ) ) ;
#69961 = PRESENTATION_STYLE_ASSIGNMENT (( #37098 ) ) ;
#69962 = SURFACE_STYLE_USAGE ( .BOTH. , #62412 ) ;
#69963 = SURFACE_STYLE_USAGE ( .BOTH. , #44642 ) ;
#69964 = AXIS2_PLACEMENT_3D ( 'NONE', #105238, #72334, #56663 ) ;
#69965 = CARTESIAN_POINT ( 'NONE',  ( 29.68315524076926337, 8.302504244945327017, -42.10535821593530414 ) ) ;
#69966 = VERTEX_POINT ( 'NONE', #91991 ) ;
#69967 = PRESENTATION_STYLE_ASSIGNMENT (( #99668 ) ) ;
#69968 = CARTESIAN_POINT ( 'NONE',  ( -17.67175098956017010, -29.03273846940966507, 29.02266591207046531 ) ) ;
#69970 = CARTESIAN_POINT ( 'NONE',  ( 1.010790367957777658, 37.02275760693545692, -27.74671416529730905 ) ) ;
#69969 = CARTESIAN_POINT ( 'NONE',  ( -86.88889009608627134, -60.00000000000000711, -3.512934530641961928 ) ) ;
#69971 = STYLED_ITEM ( 'NONE', ( #24726 ), #64108 ) ;
#69972 = VERTEX_POINT ( 'NONE', #75808 ) ;
#69973 = SURFACE_SIDE_STYLE ('',( #95316 ) ) ;
#69974 = ORIENTED_EDGE ( 'NONE', *, *, #78187, .T. ) ;
#69975 = EDGE_CURVE ( 'NONE', #11751, #84900, #41299, .T. ) ;
#69976 = CARTESIAN_POINT ( 'NONE',  ( -0.4000000000000045186, 0.000000000000000000, 0.000000000000000000 ) ) ;
#69977 = DIRECTION ( 'NONE',  ( -1.000000000000000000, -0.000000000000000000, -0.000000000000000000 ) ) ;
#69978 = ORIENTED_EDGE ( 'NONE', *, *, #43782, .F. ) ;
#69979 = CARTESIAN_POINT ( 'NONE',  ( 43.30868969682389036, 6.123233995736770227E-16, -5.000000000000002665 ) ) ;
#69980 = CONICAL_SURFACE ( 'NONE', #30431, 4.000000000000001776, 0.9599310885968774798 ) ;
#69981 = STYLED_ITEM ( 'NONE', ( #94563 ), #57123 ) ;
#69982 = CARTESIAN_POINT ( 'NONE',  ( 101.8615519058133572, -52.72503690623052819, 192.2815353188802874 ) ) ;
#69983 = CONICAL_SURFACE ( 'NONE', #76830, 5.000000000000001776, 0.9599310885968803664 ) ;
#69985 = SURFACE_SIDE_STYLE ('',( #46243 ) ) ;
#69984 = CYLINDRICAL_SURFACE ( 'NONE', #90529, 5.000000000000002665 ) ;
#69986 = ORIENTED_EDGE ( 'NONE', *, *, #32601, .F. ) ;
#69987 = AXIS2_PLACEMENT_3D ( 'NONE', #29832, #44944, #5522 ) ;
#69988 = ORIENTED_EDGE ( 'NONE', *, *, #11015, .T. ) ;
#69989 = CIRCLE ( 'NONE', #23526, 3.309500000000007880 ) ;
#69990 = ORIENTED_EDGE ( 'NONE', *, *, #77286, .T. ) ;
#69991 = CARTESIAN_POINT ( 'NONE',  ( 27.85356646027182492, 315.4045181579393784, 12.51841259425152053 ) ) ;
#69992 = ADVANCED_FACE ( 'NONE', ( #28360 ), #34857, .T. ) ;
#69993 = DIRECTION ( 'NONE',  ( 0.000000000000000000, 0.000000000000000000, 1.000000000000000000 ) ) ;
#69994 = DIRECTION ( 'NONE',  ( 0.000000000000000000, -1.000000000000000000, 0.000000000000000000 ) ) ;
#69995 = ORIENTED_EDGE ( 'NONE', *, *, #57496, .F. ) ;
#69996 = CYLINDRICAL_SURFACE ( 'NONE', #41099, 1.250000000000000000 ) ;
#69997 = CARTESIAN_POINT ( 'NONE',  ( -6.546995956212704471, 41.93635053412784686, -69.23592160050631605 ) ) ;
#69998 = CARTESIAN_POINT ( 'NONE',  ( -22.48210626068904361, -59.99999999999999289, -44.04839377960101388 ) ) ;
#69999 = FACE_BOUND ( 'NONE', #51937, .T. ) ;
#70000 = CARTESIAN_POINT ( 'NONE',  ( 22.40836378693191477, -60.00000000001930545, -44.01644647174431668 ) ) ;
#70001 = CARTESIAN_POINT ( 'NONE',  ( 11.77492727325709332, -4.999999999999999112, -11.45403612798945403 ) ) ;
#70002 = CARTESIAN_POINT ( 'NONE',  ( -5.415855499685822139, 41.85405045957928394, -58.97635199008218621 ) ) ;
#70003 = AXIS2_PLACEMENT_3D ( 'NONE', #42035, #8071, #90593 ) ;
#70005 = CARTESIAN_POINT ( 'NONE',  ( 8.311083903413562624, -56.87791216858510523, 33.36314354383234360 ) ) ;
#70004 = CARTESIAN_POINT ( 'NONE',  ( -99.88998825557715122, -14.21045842199445808, 111.7645417027540304 ) ) ;
#70006 = CARTESIAN_POINT ( 'NONE',  ( -47.66079575541817803, -46.44466184579120949, 49.24308826707560627 ) ) ;
#70007 = ORIENTED_EDGE ( 'NONE', *, *, #40426, .F. ) ;
#70008 = CARTESIAN_POINT ( 'NONE',  ( -3.586915319853207773, 19.64184885895216937, 6.012318516684870495 ) ) ;
#70009 = PRODUCT ( 'hex flange bolt_din_DIN 6921 - M8 x 40 x 40-S', 'hex flange bolt_din_DIN 6921 - M8 x 40 x 40-S', '', ( #80541 ) ) ;
#70010 = EDGE_LOOP ( 'NONE', ( #9303, #58601, #25847, #1810 ) ) ;
#70011 = LINE ( 'NONE', #94295, #1281 ) ;
#70012 = CARTESIAN_POINT ( 'NONE',  ( 17.86230688873627415, 36.34004572609662631, 23.65428218925767112 ) ) ;
#70013 = EDGE_CURVE ( 'NONE', #76623, #9931, #93048, .T. ) ;
#70014 = CARTESIAN_POINT ( 'NONE',  ( 6.568242156162330758, 3.336471507263037761, 6.846117829660745890 ) ) ;
#70016 = ORIENTED_EDGE ( 'NONE', *, *, #46973, .F. ) ;
#70015 = MECHANICAL_DESIGN_GEOMETRIC_PRESENTATION_REPRESENTATION (  '', ( #1058 ), #4573 ) ;
#70017 = CARTESIAN_POINT ( 'NONE',  ( -12.37144696128342147, -3.999999999999995559, 20.44658103856077602 ) ) ;
#70018 = VERTEX_POINT ( 'NONE', #18127 ) ;
#70019 = CARTESIAN_POINT ( 'NONE',  ( 88.95789393506666443, -29.99999999999496936, -14.90288515927673174 ) ) ;
#70020 = CARTESIAN_POINT ( 'NONE',  ( 6.951447288752834019, 41.73217225470716585, -59.36631759480937376 ) ) ;
#70021 = CARTESIAN_POINT ( 'NONE',  ( 51.76085035121451483, 41.99999999999999289, 29.83308852632746522 ) ) ;
#70022 = CARTESIAN_POINT ( 'NONE',  ( 101.0502629568186421, -30.00000000000000000, 167.9018042051803263 ) ) ;
#70023 = CARTESIAN_POINT ( 'NONE',  ( -8.000000000000000000, 0.000000000000000000, -9.274828571428571422 ) ) ;
#70024 = ORIENTED_EDGE ( 'NONE', *, *, #68542, .T. ) ;
#70025 = ORIENTED_EDGE ( 'NONE', *, *, #66181, .T. ) ;
#70026 = ORIENTED_EDGE ( 'NONE', *, *, #33895, .T. ) ;
#70027 = CARTESIAN_POINT ( 'NONE',  ( 55.11625962268163192, -32.55886939003519132, 57.75275617000808381 ) ) ;
#70028 = DIRECTION ( 'NONE',  ( 0.000000000000000000, -1.000000000000000000, 0.000000000000000000 ) ) ;
#70029 = CARTESIAN_POINT ( 'NONE',  ( -46.00000000000000711, 460.1225022309920973, 6.748346813975271807 ) ) ;
#70030 = ORIENTED_EDGE ( 'NONE', *, *, #74282, .F. ) ;
#70031 = DIRECTION ( 'NONE',  ( -1.000000000000000000, 0.000000000000000000, 0.000000000000000000 ) ) ;
#70032 = ORIENTED_EDGE ( 'NONE', *, *, #18487, .T. ) ;
#70033 = CARTESIAN_POINT ( 'NONE',  ( 1.206569728928467589, 7.963640680051485177, -0.4524126574264484835 ) ) ;
#70034 = CARTESIAN_POINT ( 'NONE',  ( 105.3592957826458587, -38.38743339881243344, 197.1096209424719632 ) ) ;
#70035 = CARTESIAN_POINT ( 'NONE',  ( 12.03383601979006912, 21.77374900303325944, 6.997788882831823543 ) ) ;
#70036 = CARTESIAN_POINT ( 'NONE',  ( 83.82860702337691805, -45.28512348765533346, 5.649739562308606189 ) ) ;
#70037 = CARTESIAN_POINT ( 'NONE',  ( 6.750000000000017764, 11.69134295108991317, 0.000000000000000000 ) ) ;
#70038 = PLANE ( 'NONE',  #46443 ) ;
#70039 = CARTESIAN_POINT ( 'NONE',  ( 41.92130353534008691, 485.3101580674378397, -3.082360575775040523 ) ) ;
#70040 = DIRECTION ( 'NONE',  ( -0.5735764363510494901, -0.8191520442889894671, 0.000000000000000000 ) ) ;
#70041 = AXIS2_PLACEMENT_3D ( 'NONE', #103759, #29896, #13673 ) ;
#70042 = CARTESIAN_POINT ( 'NONE',  ( -38.73386039799279246, 460.3889633641963997, 2.371405894922581581 ) ) ;
#70043 =( LENGTH_UNIT ( ) NAMED_UNIT ( * ) SI_UNIT ( .MILLI., .METRE. ) );
#70045 = VERTEX_POINT ( 'NONE', #1904 ) ;
#70044 =( BOUNDED_SURFACE ( )  B_SPLINE_SURFACE ( 3, 3, ( 
 ( #48382, #30109, #14412, #56471 ),
 ( #63537, #88863, #47845, #32231 ),
 ( #105048, #38728, #71597, #73176 ),
 ( #55406, #105565, #80752, #31189 ) ),
 .UNSPECIFIED., .F., .F., .F. ) 
 B_SPLINE_SURFACE_WITH_KNOTS ( ( 4, 4 ),
 ( 4, 4 ),
 ( 0.02698643027831503644, 0.9670246242088337274 ),
 ( 0.000000000000000000, 1.000000000000000000 ),
 .UNSPECIFIED. ) 
 GEOMETRIC_REPRESENTATION_ITEM ( )  RATIONAL_B_SPLINE_SURFACE ( (
 ( 1.000000000000000000, 0.3333333333333334259, 0.3333333333333334259, 1.000000000000000000),
 ( 1.000000000000000000, 0.3333333333333334259, 0.3333333333333334259, 1.000000000000000000),
 ( 1.000000000000000000, 0.3333333333333334259, 0.3333333333333334259, 1.000000000000000000),
 ( 1.000000000000000000, 0.3333333333333334259, 0.3333333333333334259, 1.000000000000000000) ) ) 
 REPRESENTATION_ITEM ( '' )  SURFACE ( )  );
#70046 = LINE ( 'NONE', #21527, #34446 ) ;
#70047 = CARTESIAN_POINT ( 'NONE',  ( 15.67047892703660139, 36.78599904984204017, -23.70382416292494199 ) ) ;
#70048 = CARTESIAN_POINT ( 'NONE',  ( -3.058406714429998896, 44.99895710957036954, 5.000000000000000000 ) ) ;
#70049 = EDGE_LOOP ( 'NONE', ( #23584, #104081, #57140, #100817 ) ) ;
#70050 = CARTESIAN_POINT ( 'NONE',  ( -31.37855721874207404, 315.8766196183444777, -6.353910099583705673 ) ) ;
#70051 = CARTESIAN_POINT ( 'NONE',  ( -29.06740789737446207, 312.1932710927672474, 12.18869810040496660 ) ) ;
#70052 = CARTESIAN_POINT ( 'NONE',  ( -11.89158881072656193, -4.825170694069168320, -76.89278924248901603 ) ) ;
#70053 =( LENGTH_UNIT ( ) NAMED_UNIT ( * ) SI_UNIT ( .MILLI., .METRE. ) );
#70054 = CARTESIAN_POINT ( 'NONE',  ( 5.656854249492378806, -21.68749999999999645, 5.656854249492381470 ) ) ;
#70055 = CIRCLE ( 'NONE', #1097, 12.00000000000000711 ) ;
#70057 = CARTESIAN_POINT ( 'NONE',  ( -32.39494539084744673, -25.32206235645057646, 40.19353790443526009 ) ) ;
#70056 =( GEOMETRIC_REPRESENTATION_CONTEXT ( 3 ) GLOBAL_UNCERTAINTY_ASSIGNED_CONTEXT ( ( #86966 ) ) GLOBAL_UNIT_ASSIGNED_CONTEXT ( ( #30600, #102338, #63490 ) ) REPRESENTATION_CONTEXT ( 'NONE', 'WORKASPACE' ) );
#70058 = EDGE_CURVE ( 'NONE', #73133, #12603, #39636, .T. ) ;
#70059 = AXIS2_PLACEMENT_3D ( 'NONE', #92814, #18971, #50738 ) ;
#70060 = CARTESIAN_POINT ( 'NONE',  ( 0.000000000000000000, 49.50000000000000000, 0.000000000000000000 ) ) ;
#70061 = AXIS2_PLACEMENT_3D ( 'NONE', #50855, #92922, #77282 ) ;
#70062 = EDGE_LOOP ( 'NONE', ( #21373, #25087, #69908, #63108, #95326 ) ) ;
#70063 = CARTESIAN_POINT ( 'NONE',  ( 85.04864020517048573, -35.79319779513708966, 181.2967254180193777 ) ) ;
#70064 = CARTESIAN_POINT ( 'NONE',  ( -48.02835407290516656, 11.61227450977240494, 14.35535821593516559 ) ) ;
#70065 = CARTESIAN_POINT ( 'NONE',  ( -15.56772955930216185, 46.04746595587302238, 6.065209611211459517 ) ) ;
#70066 = ORIENTED_EDGE ( 'NONE', *, *, #36422, .T. ) ;
#70067 = CARTESIAN_POINT ( 'NONE',  ( -96.39296834135954839, -37.82067409071415653, 116.1803817724870100 ) ) ;
#70068 = SURFACE_STYLE_FILL_AREA ( #45275 ) ;
#70069 = CARTESIAN_POINT ( 'NONE',  ( 2.751706330279339863, -5.000000000000015987, -99.99999999999998579 ) ) ;
#70070 = CARTESIAN_POINT ( 'NONE',  ( 17.17069302877290582, -4.333298119783758118, 5.126212997540350536 ) ) ;
#70071 = AXIS2_PLACEMENT_3D ( 'NONE', #88150, #104859, #80031 ) ;
#70072 = EDGE_CURVE ( 'NONE', #26193, #20727, #87830, .T. ) ;
#70073 = CARTESIAN_POINT ( 'NONE',  ( -0.01393140247697588312, -21.31702117966834109, -38.55283400289633278 ) ) ;
#70074 = ADVANCED_FACE ( 'NONE', ( #53659 ), #6890, .T. ) ;
#70075 = SURFACE_STYLE_USAGE ( .BOTH. , #37206 ) ;
#70076 = CARTESIAN_POINT ( 'NONE',  ( 11.30126247058972666, -20.79179180331792054, 35.49637522244798760 ) ) ;
#70077 = CARTESIAN_POINT ( 'NONE',  ( 2.806188179629237833, -0.4213828545325281616, 102.9366787940491719 ) ) ;
#70078 = CARTESIAN_POINT ( 'NONE',  ( 50.01436079198998641, -29.69237965549699965, 46.63421092844703963 ) ) ;
#70080 = CARTESIAN_POINT ( 'NONE',  ( -10.42385298587354470, 17.26331716369242741, 9.797020416222427031 ) ) ;
#70079 = CARTESIAN_POINT ( 'NONE',  ( 58.67238219402268840, 4.000000000000014211, 0.000000000000000000 ) ) ;
#70081 = CARTESIAN_POINT ( 'NONE',  ( 4.691302026839834660, 301.0269659576850358, -10.01286862727946314 ) ) ;
#70082 = CARTESIAN_POINT ( 'NONE',  ( 40.73878143178837519, 486.4834083601638213, 16.46716573231486436 ) ) ;
#70083 = CARTESIAN_POINT ( 'NONE',  ( -7.126148247341459019, 41.12758119229484066, -58.55282700859728351 ) ) ;
#70084 = DIRECTION ( 'NONE',  ( -1.000000000000000000, -1.224606353822377258E-16, -0.000000000000000000 ) ) ;
#70085 = ORIENTED_EDGE ( 'NONE', *, *, #70232, .F. ) ;
#70086 = CARTESIAN_POINT ( 'NONE',  ( -82.94541017858439602, -38.00000000000004263, 0.2650007619690297189 ) ) ;
#70087 = AXIS2_PLACEMENT_3D ( 'NONE', #73553, #1241, #50342 ) ;
#70088 = ORIENTED_EDGE ( 'NONE', *, *, #79577, .T. ) ;
#70089 = CARTESIAN_POINT ( 'NONE',  ( -12.03429798983160914, 2.041993617203186506, 14.86077952815172054 ) ) ;
#70090 = AXIS2_PLACEMENT_3D ( 'NONE', #11099, #67247, #3028 ) ;
#70091 = CARTESIAN_POINT ( 'NONE',  ( 36.08349330513379982, 1.593028355512270567E-15, 0.000000000000000000 ) ) ;
#70093 = CARTESIAN_POINT ( 'NONE',  ( -3.132749564764621297, -34.58960321509062652, -32.63485548209730069 ) ) ;
#70092 = CARTESIAN_POINT ( 'NONE',  ( 9.537909130738297492, 252.6461483096339009, -3.010726932293859459 ) ) ;
#70094 = ORIENTED_EDGE ( 'NONE', *, *, #19305, .F. ) ;
#70095 = CARTESIAN_POINT ( 'NONE',  ( -43.84720509323437199, 462.5482003534952469, 5.191543507852187211 ) ) ;
#70096 = CARTESIAN_POINT ( 'NONE',  ( -44.48219397478413839, 478.0055753222136445, 1.937693161207713510 ) ) ;
#70097 = ORIENTED_EDGE ( 'NONE', *, *, #119, .F. ) ;
#70098 = ADVANCED_FACE ( 'NONE', ( #38560 ), #88160, .T. ) ;
#70099 = CARTESIAN_POINT ( 'NONE',  ( 6.169949891408088583, 6.308465495020067593, 2.073417244832475692 ) ) ;
#70100 = DIRECTION ( 'NONE',  ( 0.5735764363510490460, 0.8191520442889896891, 0.000000000000000000 ) ) ;
#70101 = CARTESIAN_POINT ( 'NONE',  ( -91.86565372589397782, -60.00000000000001421, 10.89366606999959330 ) ) ;
#70102 = ORIENTED_EDGE ( 'NONE', *, *, #37906, .T. ) ;
#70103 = CARTESIAN_POINT ( 'NONE',  ( 4.898587196589412829E-16, -27.31250000409677270, -8.000000000000000000 ) ) ;
#70104 = FACE_BOUND ( 'NONE', #39630, .T. ) ;
#70105 = DIRECTION ( 'NONE',  ( 0.000000000000000000, -1.000000000000000000, 0.000000000000000000 ) ) ;
#70106 = CARTESIAN_POINT ( 'NONE',  ( 13.61490394126797554, 294.5438152624074064, 1.871499044962292801 ) ) ;
#70107 = VECTOR ( 'NONE', #100721, 1000.000000000000000 ) ;
#70109 = DIRECTION ( 'NONE',  ( 0.000000000000000000, -1.000000000000000000, 0.000000000000000000 ) ) ;
#70108 = CARTESIAN_POINT ( 'NONE',  ( 43.00000000000000000, 487.1237704758250402, 9.497510897111922645 ) ) ;
#70110 = CARTESIAN_POINT ( 'NONE',  ( -85.21609695689519981, -22.03875263890091674, 162.9510693786682509 ) ) ;
#70111 = AXIS2_PLACEMENT_3D ( 'NONE', #58518, #75207, #34263 ) ;
#70112 = ORIENTED_EDGE ( 'NONE', *, *, #28403, .T. ) ;
#70113 = CARTESIAN_POINT ( 'NONE',  ( -1.113934713178898139, -0.000000000000000000, 17.01589776168603763 ) ) ;
#70114 = EDGE_LOOP ( 'NONE', ( #19797, #81302 ) ) ;
#70115 = ORIENTED_EDGE ( 'NONE', *, *, #75133, .F. ) ;
#70116 = CARTESIAN_POINT ( 'NONE',  ( -6.648792466258459655, -5.000000000000000000, 15.29529797603510488 ) ) ;
#70117 = EDGE_CURVE ( 'NONE', #13401, #72871, #32813, .T. ) ;
#70118 = CARTESIAN_POINT ( 'NONE',  ( -4.107027841300135762, -69.23752800445994637, 13.61032178755603361 ) ) ;
#70119 = FACE_OUTER_BOUND ( 'NONE', #81972, .T. ) ;
#70120 = ORIENTED_EDGE ( 'NONE', *, *, #67679, .T. ) ;
#70121 = CARTESIAN_POINT ( 'NONE',  ( -3.409519076813957649E-15, 51.11204936430951307, 27.84083606136722366 ) ) ;
#70122 = CARTESIAN_POINT ( 'NONE',  ( -96.68549010014578471, -57.67144976548149771, 46.95518404347522079 ) ) ;
#70123 = CARTESIAN_POINT ( 'NONE',  ( -5.190609988845226397, -67.63922286743593304, -3.016375611400011092 ) ) ;
#70124 = CARTESIAN_POINT ( 'NONE',  ( 8.595526037062774425E-16, 13.85270131633358304, 7.000000000000011546 ) ) ;
#70125 = MECHANICAL_DESIGN_GEOMETRIC_PRESENTATION_REPRESENTATION (  '', ( #49484 ), #16759 ) ;
#70126 = CARTESIAN_POINT ( 'NONE',  ( 23.84332598391564062, 27.93368204320126225, 30.86206213703118451 ) ) ;
#70127 = DIRECTION ( 'NONE',  ( 0.000000000000000000, 0.000000000000000000, 1.000000000000000000 ) ) ;
#70128 = AXIS2_PLACEMENT_3D ( 'NONE', #97687, #7607, #23849 ) ;
#70129 = CARTESIAN_POINT ( 'NONE',  ( 3.487646406148289913, 15.95332971149351842, -9.373884331925008695 ) ) ;
#70130 = CARTESIAN_POINT ( 'NONE',  ( 64.66821620130598092, -14.21045842199433373, -28.81313120037184916 ) ) ;
#70131 = CARTESIAN_POINT ( 'NONE',  ( -62.45630560627096628, -29.99999999999992184, 99.43668923270982418 ) ) ;
#70132 = CARTESIAN_POINT ( 'NONE',  ( -54.20616908285522584, -42.97143615225327551, 59.98809675918620599 ) ) ;
#70133 = ORIENTED_EDGE ( 'NONE', *, *, #62106, .T. ) ;
#70134 = CARTESIAN_POINT ( 'NONE',  ( 5.744562646538029504, 12.99999999999999112, -4.000000000000000000 ) ) ;
#70135 = CIRCLE ( 'NONE', #51172, 13.50000000000000000 ) ;
#70137 = ORIENTED_EDGE ( 'NONE', *, *, #3776, .T. ) ;
#70136 = VECTOR ( 'NONE', #29029, 1000.000000000000000 ) ;
#70138 = CARTESIAN_POINT ( 'NONE',  ( -103.2098837543867660, -60.16809070699064677, 192.4864521153085377 ) ) ;
#70140 = VECTOR ( 'NONE', #80726, 1000.000000000000000 ) ;
#70139 = CARTESIAN_POINT ( 'NONE',  ( 102.6011607304368027, -37.99999999999997868, 179.5962889347694613 ) ) ;
#70141 = CARTESIAN_POINT ( 'NONE',  ( -30.48515219902031603, 12.91670175270527210, -41.81704193310824991 ) ) ;
#70142 = EDGE_CURVE ( 'NONE', #58214, #30899, #17226, .T. ) ;
#70143 = VERTEX_POINT ( 'NONE', #55235 ) ;
#70144 = CARTESIAN_POINT ( 'NONE',  ( 18.96461344042381469, 49.39013151286044234, 61.98979294430989739 ) ) ;
#70145 = FACE_BOUND ( 'NONE', #24445, .T. ) ;
#70146 = CARTESIAN_POINT ( 'NONE',  ( 2.977408999572650927, -13.25000000204838280, -7.188101187500001821 ) ) ;
#70147 = DIRECTION ( 'NONE',  ( 0.5735764363510470476, -0.8191520442889911324, 1.003171929053524007E-16 ) ) ;
#70148 = COLOUR_RGB ( '', 0.31764706, 0.68627451, 0.89019608) ;
#70149 = CARTESIAN_POINT ( 'NONE',  ( 7.150053860865850375, -83.21734546086022988, 3.590189269391291571 ) ) ;
#70150 = CARTESIAN_POINT ( 'NONE',  ( 66.20789329592186334, -30.00000000000000355, 83.72596625502930578 ) ) ;
#70151 = TOROIDAL_SURFACE ( 'NONE', #23669, 11.00000000000000000, 1.000000000000000000 ) ;
#70152 = EDGE_CURVE ( 'NONE', #59988, #86797, #21330, .T. ) ;
#70153 = CARTESIAN_POINT ( 'NONE',  ( -9.414516558252268297, 10.25650596040859774, 0.000000000000000000 ) ) ;
#70154 = CARTESIAN_POINT ( 'NONE',  ( 13.50000000000000355, -6.526560492696113158, -12.16017290538970386 ) ) ;
#70155 = CARTESIAN_POINT ( 'NONE',  ( -12.50000000000000355, -79.93083296558610584, -76.70843802411151557 ) ) ;
#70156 = CARTESIAN_POINT ( 'NONE',  ( -28.53269844911218200, -53.39016512961349292, 35.08051764473837864 ) ) ;
#70157 = EDGE_LOOP ( 'NONE', ( #29091, #50014, #72233, #87917, #1107 ) ) ;
#70158 = CARTESIAN_POINT ( 'NONE',  ( 48.01372197413871845, -42.98097658514403463, 48.71122713025049222 ) ) ;
#70159 = ORIENTED_EDGE ( 'NONE', *, *, #3881, .T. ) ;
#70160 = CARTESIAN_POINT ( 'NONE',  ( -0.07795483430646524270, 13.70447791526909853, 49.25000000000002132 ) ) ;
#70161 = CARTESIAN_POINT ( 'NONE',  ( -6.924369423635565290, 16.86636905560499855, 1.059067681833820940 ) ) ;
#70162 = CARTESIAN_POINT ( 'NONE',  ( -94.01096082434968082, -38.49234416915790291, 201.1924522757551017 ) ) ;
#70163 = VERTEX_POINT ( 'NONE', #86591 ) ;
#70164 = CARTESIAN_POINT ( 'NONE',  ( 91.47297658247813956, -38.38308769809394505, -6.128389452813496341 ) ) ;
#70165 = CARTESIAN_POINT ( 'NONE',  ( 15.55338204050653594, 4.754590481644285660, -5.683686875341236622 ) ) ;
#70166 = CARTESIAN_POINT ( 'NONE',  ( -49.15082508851313037, 8.572194610415261096, -15.05005620232426722 ) ) ;
#70167 = DIRECTION ( 'NONE',  ( 1.000000000000000000, 1.224606353822377258E-16, 0.000000000000000000 ) ) ;
#70168 = CARTESIAN_POINT ( 'NONE',  ( 6.200188411027975022, 41.06054039277635326, -71.07396429817178785 ) ) ;
#70169 = CARTESIAN_POINT ( 'NONE',  ( -32.52877124674115805, 435.6736143190897792, 17.82210992056645438 ) ) ;
#70170 = CARTESIAN_POINT ( 'NONE',  ( 12.50000000000000711, -4.999999999999999112, -80.60844091781802945 ) ) ;
#70171 = AXIS2_PLACEMENT_3D ( 'NONE', #73962, #40019, #72890 ) ;
#70172 = CARTESIAN_POINT ( 'NONE',  ( 112.1739726238778161, -59.99999999999999289, 168.9510083732245675 ) ) ;
#70173 = EDGE_CURVE ( 'NONE', #104952, #64595, #90666, .T. ) ;
#70174 = AXIS2_PLACEMENT_3D ( 'NONE', #3462, #50921, #36406 ) ;
#70175 = CARTESIAN_POINT ( 'NONE',  ( -7.414346147791993857, -67.64589157662264540, -3.010818766110536338 ) ) ;
#70176 = ORIENTED_EDGE ( 'NONE', *, *, #72527, .T. ) ;
#70177 = DIRECTION ( 'NONE',  ( 0.000000000000000000, 0.000000000000000000, -1.000000000000000000 ) ) ;
#70178 = CARTESIAN_POINT ( 'NONE',  ( -80.87453322288685342, -30.00000000000003908, 6.258431868449455315 ) ) ;
#70179 = VERTEX_POINT ( 'NONE', #31016 ) ;
#70181 = CARTESIAN_POINT ( 'NONE',  ( 5.222379818299239140, 7.098635799589327888, -27.55850616374455697 ) ) ;
#70180 = CARTESIAN_POINT ( 'NONE',  ( -82.77499858381615638, -38.82538985791964592, 196.7482481615944891 ) ) ;
#70182 = LINE ( 'NONE', #62119, #54549 ) ;
#70183 = CARTESIAN_POINT ( 'NONE',  ( 24.34999999999999787, 1.533819458162526451E-15, 0.000000000000000000 ) ) ;
#70184 = DIRECTION ( 'NONE',  ( -1.000000000000000000, -1.224606353822377258E-16, -0.000000000000000000 ) ) ;
#70185 = CARTESIAN_POINT ( 'NONE',  ( -7.188101187500002709, -15.68750000204838457, 2.977408999572648707 ) ) ;
#70186 = CARTESIAN_POINT ( 'NONE',  ( 5.036189802310023111, -5.000000000000002665, -76.26213611588336505 ) ) ;
#70187 = SURFACE_STYLE_USAGE ( .BOTH. , #52939 ) ;
#70189 = ORIENTED_EDGE ( 'NONE', *, *, #13042, .T. ) ;
#70188 = CARTESIAN_POINT ( 'NONE',  ( 6.644028492724103785, -3.901260126079907575, 6.757180751914056316 ) ) ;
#70190 = CARTESIAN_POINT ( 'NONE',  ( 80.54825481451001679, -60.43138345613007800, 180.0438305313103058 ) ) ;
#70191 = CARTESIAN_POINT ( 'NONE',  ( -44.25901894362515065, 463.6537623376428314, 7.444378749523244743 ) ) ;
#70192 = AXIS2_PLACEMENT_3D ( 'NONE', #8226, #64872, #7682 ) ;
#70193 = CARTESIAN_POINT ( 'NONE',  ( 9.334514330295430540, 86.78622737681789090, -3.588704711590611218 ) ) ;
#70194 = ORIENTED_EDGE ( 'NONE', *, *, #9265, .F. ) ;
#70195 = CARTESIAN_POINT ( 'NONE',  ( -33.79347250503700906, 316.5797005500412524, -6.697218333849672689 ) ) ;
#70196 = CARTESIAN_POINT ( 'NONE',  ( 94.84444444444443434, 4.172000000000019249, 0.000000000000000000 ) ) ;
#70197 = CARTESIAN_POINT ( 'NONE',  ( 8.673617379884035472E-16, 7.505553499465148271, -0.7999999999999977129 ) ) ;
#70198 = SURFACE_STYLE_USAGE ( .BOTH. , #62651 ) ;
#70199 = CARTESIAN_POINT ( 'NONE',  ( 16.64348903516523848, 43.47556584774768851, 6.657797401561421857 ) ) ;
#70200 = EDGE_CURVE ( 'NONE', #40622, #11109, #99895, .T. ) ;
#70201 = ORIENTED_EDGE ( 'NONE', *, *, #62777, .T. ) ;
#70202 = FILL_AREA_STYLE ('',( #37343 ) ) ;
#70203 = AXIS2_PLACEMENT_3D ( 'NONE', #27849, #100082, #52591 ) ;
#70204 = MECHANICAL_DESIGN_GEOMETRIC_PRESENTATION_REPRESENTATION (  '', ( #16861 ), #58179 ) ;
#70205 = CARTESIAN_POINT ( 'NONE',  ( -9.384414461224938719, 294.8111600184428767, 3.468918321496474721 ) ) ;
#70206 = EDGE_CURVE ( 'NONE', #69452, #51816, #19031, .T. ) ;
#70208 = DIRECTION ( 'NONE',  ( 0.000000000000000000, -1.000000000000000000, 0.000000000000000000 ) ) ;
#70207 = SHAPE_REPRESENTATION ( '6. Link', ( #10728 ), #2257 ) ;
#70209 = CARTESIAN_POINT ( 'NONE',  ( 12.13034742782427955, -79.93083296558610584, -93.82352941176471006 ) ) ;
#70211 = CARTESIAN_POINT ( 'NONE',  ( -14.35785620000810958, 3.948300967435982578, -4.282865182293815742 ) ) ;
#70210 = FACE_OUTER_BOUND ( 'NONE', #8124, .T. ) ;
#70212 = CARTESIAN_POINT ( 'NONE',  ( 5.082755093536325930, -21.96875000204838457, -5.082755093536325042 ) ) ;
#70213 = CIRCLE ( 'NONE', #68454, 4.000000000000000000 ) ;
#70214 = CARTESIAN_POINT ( 'NONE',  ( 46.00000000000000000, 438.2046082539382610, 15.52554165154988475 ) ) ;
#70215 = COLOUR_RGB ( '', 0.08235294, 0.09019608, 0.10196078) ;
#70216 = AXIS2_PLACEMENT_3D ( 'NONE', #92953, #42806, #84335 ) ;
#70217 = CARTESIAN_POINT ( 'NONE',  ( 2.583889972060055218, -5.000000000000000000, 9.742892617415389367 ) ) ;
#70218 = CARTESIAN_POINT ( 'NONE',  ( 6.061808134833448491, -5.000000000000000000, -74.52203418564995729 ) ) ;
#70219 = VERTEX_POINT ( 'NONE', #104324 ) ;
#70220 = CARTESIAN_POINT ( 'NONE',  ( -36.50247448621189506, 490.9911319642687317, 12.47041065747709965 ) ) ;
#70221 = CARTESIAN_POINT ( 'NONE',  ( 5.363597346073513350, 41.33266196706048845, -58.39526881795627844 ) ) ;
#70222 = CARTESIAN_POINT ( 'NONE',  ( -3.994958879817047226, 15.13994505928113377, -5.000000000000000000 ) ) ;
#70223 = AXIS2_PLACEMENT_3D ( 'NONE', #10574, #90982, #82878 ) ;
#70224 = EDGE_CURVE ( 'NONE', #87124, #80842, #58564, .T. ) ;
#70225 = DIRECTION ( 'NONE',  ( -0.5735764363510494901, -0.8191520442889894671, 0.000000000000000000 ) ) ;
#70226 = ORIENTED_EDGE ( 'NONE', *, *, #103922, .T. ) ;
#70227 = AXIS2_PLACEMENT_3D ( 'NONE', #56664, #74441, #7576 ) ;
#70228 = CARTESIAN_POINT ( 'NONE',  ( -7.939867041329224939, 52.04605724232908415, -1.683498186040722544 ) ) ;
#70229 =( LENGTH_UNIT ( ) NAMED_UNIT ( * ) SI_UNIT ( .MILLI., .METRE. ) );
#70230 = ORIENTED_EDGE ( 'NONE', *, *, #104685, .F. ) ;
#70231 = CARTESIAN_POINT ( 'NONE',  ( 22.61650669486618526, 4.898587196589411843E-16, -4.000000000000000888 ) ) ;
#70232 = EDGE_CURVE ( 'NONE', #13600, #47740, #12130, .T. ) ;
#70233 = DIRECTION ( 'NONE',  ( -1.000000000000000000, -0.000000000000000000, -0.000000000000000000 ) ) ;
#70234 = CARTESIAN_POINT ( 'NONE',  ( 9.842473135306409660, 101.4106818288640994, 1.785129593756277666 ) ) ;
#70235 =( NAMED_UNIT ( * ) SI_UNIT ( $, .STERADIAN. ) SOLID_ANGLE_UNIT ( ) );
#70236 = CARTESIAN_POINT ( 'NONE',  ( -103.5078833138821182, -59.99999999999999289, 200.3335383992328786 ) ) ;
#70237 = CARTESIAN_POINT ( 'NONE',  ( 17.50000000000007105, 48.00000000000153477, 62.61753806507839926 ) ) ;
#70238 = CARTESIAN_POINT ( 'NONE',  ( 3.809068165403731943, 5.306386968807657034, 1.196857554470325985E-15 ) ) ;
#70239 = DIRECTION ( 'NONE',  ( 0.000000000000000000, 1.000000000000000000, 0.000000000000000000 ) ) ;
#70240 = AXIS2_PLACEMENT_3D ( 'NONE', #11497, #19663, #27210 ) ;
#70241 = CARTESIAN_POINT ( 'NONE',  ( -83.18122759319267345, -46.51677116687196190, 180.8298306939889812 ) ) ;
#70242 = CARTESIAN_POINT ( 'NONE',  ( 25.59175815610272764, 43.61275438026441975, -75.31714932479673053 ) ) ;
#70243 = ORIENTED_EDGE ( 'NONE', *, *, #45983, .T. ) ;
#70244 = CARTESIAN_POINT ( 'NONE',  ( 6.231493956936416723, 147.8264543773111654, 0.000000000000000000 ) ) ;
#70245 = EDGE_CURVE ( 'NONE', #105730, #58641, #91295, .T. ) ;
#70246 = CARTESIAN_POINT ( 'NONE',  ( 4.904566723942681783, -67.02242702470746849, 3.460360782932704549 ) ) ;
#70247 = CARTESIAN_POINT ( 'NONE',  ( -83.66823586964305548, -45.26509719214853078, 13.41398437886814143 ) ) ;
#70248 = CARTESIAN_POINT ( 'NONE',  ( 99.75754961941544252, -2.002967142162725287E-29, 5.000000000000011546 ) ) ;
#70249 = VECTOR ( 'NONE', #14752, 1000.000000000000341 ) ;
#70250 = EDGE_CURVE ( 'NONE', #82202, #46114, #65487, .T. ) ;
#70251 = CARTESIAN_POINT ( 'NONE',  ( 9.609486011791064541, 143.0915023496501419, 0.000000000000000000 ) ) ;
#70252 = CARTESIAN_POINT ( 'NONE',  ( 2.499999999999997335, -30.00000000000000000, 30.00000000000000000 ) ) ;
#70253 = CARTESIAN_POINT ( 'NONE',  ( -1.233923992984923027E-14, 18.64316884711714195, -38.36535705883633085 ) ) ;
#70254 = AXIS2_PLACEMENT_3D ( 'NONE', #57124, #14534, #38847 ) ;
#70255 = CARTESIAN_POINT ( 'NONE',  ( 93.93534938131868728, -14.21045842199442433, 198.1410878059230072 ) ) ;
#70256 = DIRECTION ( 'NONE',  ( 0.000000000000000000, 0.000000000000000000, -1.000000000000000000 ) ) ;
#70257 = CARTESIAN_POINT ( 'NONE',  ( -95.23228170574914486, -59.99999999999995737, 30.92731164540345645 ) ) ;
#70258 = CARTESIAN_POINT ( 'NONE',  ( -63.91133421294225059, -36.00889000299856235, 81.23570399580073342 ) ) ;
#70259 = VERTEX_POINT ( 'NONE', #55750 ) ;
#70260 = CARTESIAN_POINT ( 'NONE',  ( 80.26999927900735088, -59.99999999999982947, 200.1019127161866606 ) ) ;
#70261 = CARTESIAN_POINT ( 'NONE',  ( -54.95213656779772293, 38.95432885865245254, -32.68837454861606773 ) ) ;
#70262 = CARTESIAN_POINT ( 'NONE',  ( 89.69739047552775446, -59.99999999999509015, 204.4076188194097483 ) ) ;
#70263 = ORIENTED_EDGE ( 'NONE', *, *, #43312, .F. ) ;
#70264 = CARTESIAN_POINT ( 'NONE',  ( -32.85155332502863246, 463.8111683108725174, 7.359358840565855431 ) ) ;
#70265 = CARTESIAN_POINT ( 'NONE',  ( -1.320432766682874540E-15, -18.40625000204838457, 7.188101187500000044 ) ) ;
#70266 =( GEOMETRIC_REPRESENTATION_CONTEXT ( 3 ) GLOBAL_UNCERTAINTY_ASSIGNED_CONTEXT ( ( #37350 ) ) GLOBAL_UNIT_ASSIGNED_CONTEXT ( ( #105788, #22783, #16246 ) ) REPRESENTATION_CONTEXT ( 'NONE', 'WORKASPACE' ) );
#70267 = EDGE_CURVE ( 'NONE', #3027, #59923, #60351, .T. ) ;
#70268 = CARTESIAN_POINT ( 'NONE',  ( -4.472135954999581386, -10.00000000000000888, -4.000000000000000000 ) ) ;
#70269 = ORIENTED_EDGE ( 'NONE', *, *, #63182, .T. ) ;
#70271 = FACE_OUTER_BOUND ( 'NONE', #8114, .T. ) ;
#70270 = CIRCLE ( 'NONE', #56466, 4.000000000000007105 ) ;
#70272 = VERTEX_POINT ( 'NONE', #96784 ) ;
#70273 = CARTESIAN_POINT ( 'NONE',  ( 1.735558044530975508, 39.99999999999999289, -69.74083754113327416 ) ) ;
#70274 = CARTESIAN_POINT ( 'NONE',  ( -39.30650688511865809, 485.8522658471748628, -4.984147873724826816 ) ) ;
#70275 = CARTESIAN_POINT ( 'NONE',  ( -92.73282884694502570, -60.00000000000001421, -8.836575342051251170 ) ) ;
#70276 = DIRECTION ( 'NONE',  ( 0.000000000000000000, 0.000000000000000000, -1.000000000000000000 ) ) ;
#70277 = CARTESIAN_POINT ( 'NONE',  ( 4.401442555609581635E-16, -32.65625000204838813, -7.188101187500000044 ) ) ;
#70278 = DIRECTION ( 'NONE',  ( 0.000000000000000000, -1.000000000000000000, 0.000000000000000000 ) ) ;
#70279 = DIRECTION ( 'NONE',  ( 0.000000000000000000, -1.000000000000000000, 0.000000000000000000 ) ) ;
#70280 = CARTESIAN_POINT ( 'NONE',  ( 5.000000000000000888, -64.69017754626541716, 10.12118620290157978 ) ) ;
#70281 = DIRECTION ( 'NONE',  ( 0.000000000000000000, 0.000000000000000000, 1.000000000000000000 ) ) ;
#70282 = EDGE_CURVE ( 'NONE', #68161, #29601, #103800, .T. ) ;
#70283 = DIRECTION ( 'NONE',  ( 1.000000000000000000, -0.000000000000000000, -0.000000000000000000 ) ) ;
#70284 = FACE_OUTER_BOUND ( 'NONE', #3500, .T. ) ;
#70285 = CARTESIAN_POINT ( 'NONE',  ( 1.044083592157493498E-15, 70.00000000000000000, 7.025805963803935406 ) ) ;
#70286 = VERTEX_POINT ( 'NONE', #63366 ) ;
#70287 = CARTESIAN_POINT ( 'NONE',  ( 6.400000000000000355, 0.000000000000000000, 0.000000000000000000 ) ) ;
#70288 =( NAMED_UNIT ( * ) SI_UNIT ( $, .STERADIAN. ) SOLID_ANGLE_UNIT ( ) );
#70289 = AXIS2_PLACEMENT_3D ( 'NONE', #85116, #20442, #94278 ) ;
#70290 = CIRCLE ( 'NONE', #37610, 1.000000000000009104 ) ;
#70291 = CARTESIAN_POINT ( 'NONE',  ( 36.59678287535385266, -32.58377898008321694, 34.88015138182827712 ) ) ;
#70292 = VERTEX_POINT ( 'NONE', #102748 ) ;
#70293 = EDGE_CURVE ( 'NONE', #86482, #64980, #44791, .T. ) ;
#70294 = CARTESIAN_POINT ( 'NONE',  ( -5.036189803708997381, 48.00000000000000711, -76.26213611645745516 ) ) ;
#70296 = CARTESIAN_POINT ( 'NONE',  ( 98.59800593614012598, 5.000000000000042633, 6.123233995736805725E-16 ) ) ;
#70295 = CARTESIAN_POINT ( 'NONE',  ( 88.20199406385988539, 6.123233995736568081E-16, -5.000000000000011546 ) ) ;
#70297 = PRESENTATION_LAYER_ASSIGNMENT (  '', '', ( #1347 ) ) ;
#70298 = CARTESIAN_POINT ( 'NONE',  ( 85.31310517497098544, 1.030564683017419500E-14, 0.000000000000000000 ) ) ;
#70299 = DIRECTION ( 'NONE',  ( -0.000000000000000000, -0.000000000000000000, 1.000000000000000000 ) ) ;
#70300 = CIRCLE ( 'NONE', #22042, 10.00000000000000000 ) ;
#70301 = FACE_OUTER_BOUND ( 'NONE', #64681, .T. ) ;
#70302 = CARTESIAN_POINT ( 'NONE',  ( -42.34430797738168195, 436.4403912042762954, 6.776599765004717391 ) ) ;
#70303 = DIRECTION ( 'NONE',  ( -0.5735764363510459374, -0.8191520442889919096, 0.000000000000000000 ) ) ;
#70304 =( NAMED_UNIT ( * ) SI_UNIT ( $, .STERADIAN. ) SOLID_ANGLE_UNIT ( ) );
#70305 = VERTEX_POINT ( 'NONE', #95719 ) ;
#70306 = CARTESIAN_POINT ( 'NONE',  ( 92.68036264477171926, -60.00000000000002132, -4.335246237957126603 ) ) ;
#70307 =( NAMED_UNIT ( * ) PLANE_ANGLE_UNIT ( ) SI_UNIT ( $, .RADIAN. ) );
#70308 = DIRECTION ( 'NONE',  ( 0.000000000000000000, -1.000000000000000000, 0.000000000000000000 ) ) ;
#70309 = CARTESIAN_POINT ( 'NONE',  ( -6.804948495083388949, 41.03925908421396684, -70.91872536974180719 ) ) ;
#70310 = FACE_OUTER_BOUND ( 'NONE', #55711, .T. ) ;
#70311 = VERTEX_POINT ( 'NONE', #22914 ) ;
#70312 = VECTOR ( 'NONE', #73245, 1000.000000000000341 ) ;
#70313 = CARTESIAN_POINT ( 'NONE',  ( -92.59962393262327396, -29.99999999998227551, 199.7669230624210002 ) ) ;
#70314 = ORIENTED_EDGE ( 'NONE', *, *, #7938, .T. ) ;
#70315 = SURFACE_STYLE_USAGE ( .BOTH. , #95131 ) ;
#70316 = LINE ( 'NONE', #103734, #39126 ) ;
#70317 = DIRECTION ( 'NONE',  ( -1.000000000000000000, -1.224606353822377258E-16, -0.000000000000000000 ) ) ;
#70318 = CARTESIAN_POINT ( 'NONE',  ( 16.13463197906254720, 21.11076038461946425, 3.387067249047301498 ) ) ;
#70319 = CARTESIAN_POINT ( 'NONE',  ( 81.77433114748801302, -37.82765095025914093, -14.17082202020662152 ) ) ;
#70320 = CARTESIAN_POINT ( 'NONE',  ( -5.082755093536326818, -32.09375000204838813, 5.082755093536325042 ) ) ;
#70321 = DIRECTION ( 'NONE',  ( 0.000000000000000000, 0.000000000000000000, 1.000000000000000000 ) ) ;
#70322 = SURFACE_STYLE_FILL_AREA ( #78399 ) ;
#70323 = FACE_OUTER_BOUND ( 'NONE', #82094, .T. ) ;
#70324 = ORIENTED_EDGE ( 'NONE', *, *, #66217, .F. ) ;
#70325 = COLOUR_RGB ( '', 0.09019608, 0.27058824, 0.51372549) ;
#70327 = VERTEX_POINT ( 'NONE', #45060 ) ;
#70326 = DIRECTION ( 'NONE',  ( 0.000000000000000000, 0.000000000000000000, 1.000000000000000000 ) ) ;
#70328 = CARTESIAN_POINT ( 'NONE',  ( 79.32494501487229854, -39.49602140262202710, 141.5487238132834023 ) ) ;
#70329 = FILL_AREA_STYLE ('',( #103227 ) ) ;
#70330 = EDGE_LOOP ( 'NONE', ( #51982, #25307 ) ) ;
#70331 = CARTESIAN_POINT ( 'NONE',  ( -12.50000000000000000, 20.38384220063782593, -37.91620629977019519 ) ) ;
#70332 = CARTESIAN_POINT ( 'NONE',  ( 7.188101187499999156, -16.25000000204838457, 2.977408999572654924 ) ) ;
#70333 = CARTESIAN_POINT ( 'NONE',  ( -104.1916751217198822, -57.64030415157957066, 202.2041723927455905 ) ) ;
#70334 = ADVANCED_FACE ( 'NONE', ( #54698 ), #51689, .T. ) ;
#70335 = EDGE_LOOP ( 'NONE', ( #73955, #43489, #90513, #86936, #37599 ) ) ;
#70336 =( LENGTH_UNIT ( ) NAMED_UNIT ( * ) SI_UNIT ( .MILLI., .METRE. ) );
#70337 = AXIS2_PLACEMENT_3D ( 'NONE', #23830, #30859, #15689 ) ;
#70338 = CARTESIAN_POINT ( 'NONE',  ( -4.521127550501230274, -10.67610240527664800, 3.944701057164354818 ) ) ;
#70339 = EDGE_CURVE ( 'NONE', #717, #82973, #62306, .T. ) ;
#70340 = VECTOR ( 'NONE', #88735, 1000.000000000000000 ) ;
#70341 = CARTESIAN_POINT ( 'NONE',  ( 7.130799530010651921, 41.48519058599254805, -59.01258828833805836 ) ) ;
#70342 = DIRECTION ( 'NONE',  ( 0.8191520442889975717, 1.003171929053531773E-16, -0.5735764363510378328 ) ) ;
#70343 = CARTESIAN_POINT ( 'NONE',  ( -3.313708498984760720, -18.21875000409676915, -8.000000000000000000 ) ) ;
#70344 = CARTESIAN_POINT ( 'NONE',  ( -49.53127930048969318, -29.59600273485972366, 45.87288584322060103 ) ) ;
#70345 = FILL_AREA_STYLE_COLOUR ( '', #30231 ) ;
#70346 = CARTESIAN_POINT ( 'NONE',  ( -43.71503333927389434, 486.3083204931239152, 5.911991965207118227 ) ) ;
#70347 = CIRCLE ( 'NONE', #99665, 4.000000000000000000 ) ;
#70348 = CARTESIAN_POINT ( 'NONE',  ( -9.165151389911681434, 84.99999999999998579, -4.000000000000000000 ) ) ;
#70349 = APPLICATION_PROTOCOL_DEFINITION ( 'draft international standard', 'automotive_design', 1998, #94869 ) ;
#70350 = CARTESIAN_POINT ( 'NONE',  ( 37.56673239365870387, 27.60449318992555945, 13.45617127780999134 ) ) ;
#70351 = VERTEX_POINT ( 'NONE', #23987 ) ;
#70352 = CARTESIAN_POINT ( 'NONE',  ( -1.341815878753393809, -50.03007620914304709, 40.96301477866974494 ) ) ;
#70353 = CARTESIAN_POINT ( 'NONE',  ( 0.000000000000000000, 48.00000000000000000, 62.00000000000000000 ) ) ;
#70355 = CARTESIAN_POINT ( 'NONE',  ( 31.46253585067004721, 6.123233995736770227E-16, -5.000000000000002665 ) ) ;
#70354 =( BOUNDED_CURVE ( )  B_SPLINE_CURVE ( 2, ( #29057, #69470, #70527, #30083, #13327, #46251, #87778, #13860, #4730 ),
 .UNSPECIFIED., .F., .F. ) 
 B_SPLINE_CURVE_WITH_KNOTS ( ( 3, 2, 2, 2, 3 ),
 ( 0.7500000000000000000, 0.7573529411764705621, 0.7647058823529411242, 0.7720588235294117974, 0.7794117647058823595 ),
 .UNSPECIFIED. ) 
 CURVE ( )  GEOMETRIC_REPRESENTATION_ITEM ( )  RATIONAL_B_SPLINE_CURVE ( ( 1.000000000000000000, 0.9238795325112867385, 1.000000000000000000, 0.9238795325112867385, 1.000000000000000000, 0.9238795325112867385, 1.000000000000000000, 0.9238795325112867385, 1.000000000000000000 ) ) 
 REPRESENTATION_ITEM ( '' )  );
#70356 = CARTESIAN_POINT ( 'NONE',  ( 54.29649119386410661, -29.25829085814808650, -34.21479539254390545 ) ) ;
#70357 = CARTESIAN_POINT ( 'NONE',  ( -82.84466124429486911, -30.00000000000000355, 151.7715457259677976 ) ) ;
#70358 = CARTESIAN_POINT ( 'NONE',  ( 43.55333112596303380, 465.2342844084865874, 9.238213423009675296 ) ) ;
#70359 = EDGE_CURVE ( 'NONE', #36055, #62753, #22309, .T. ) ;
#70360 = ORIENTED_EDGE ( 'NONE', *, *, #100708, .F. ) ;
#70361 = CONICAL_SURFACE ( 'NONE', #84134, 3.309500000000007880, 0.9599310885968770357 ) ;
#70362 = CARTESIAN_POINT ( 'NONE',  ( -14.93248505786663038, -4.333298119783897562, 9.906141972585356115 ) ) ;
#70363 = CARTESIAN_POINT ( 'NONE',  ( 81.75912227876649752, -57.51972024110150983, 200.3275499453189070 ) ) ;
#70364 = CARTESIAN_POINT ( 'NONE',  ( 74.86755951436030898, -60.22812835740788273, -24.22374349095017365 ) ) ;
#70365 = CARTESIAN_POINT ( 'NONE',  ( -4.424031367839510231, -4.951337798339865870, -6.056431503346049183 ) ) ;
#70366 = B_SPLINE_CURVE_WITH_KNOTS ( 'NONE', 3,
 ( #67419, #90086, #106250, #73894 ),
 .UNSPECIFIED., .F., .F.,
 ( 4, 4 ),
 ( 0.000000000000000000, 0.003511374632867239783 ),
 .UNSPECIFIED. ) ;
#70367 = CARTESIAN_POINT ( 'NONE',  ( 12.61650669486618881, 1.474610560812782335E-15, 0.000000000000000000 ) ) ;
#70368 = DIRECTION ( 'NONE',  ( -0.000000000000000000, 1.000000000000000000, -0.000000000000000000 ) ) ;
#70369 = CARTESIAN_POINT ( 'NONE',  ( -55.88924746550470957, -60.00000000000000711, 87.85475180783302562 ) ) ;
#70370 = AXIS2_PLACEMENT_3D ( 'NONE', #100961, #43265, #20103 ) ;
#70371 = CARTESIAN_POINT ( 'NONE',  ( -4.574783636564536238, 5.228990388887307716, -6.171384342982487503 ) ) ;
#70372 = FACE_OUTER_BOUND ( 'NONE', #1092, .T. ) ;
#70373 = CARTESIAN_POINT ( 'NONE',  ( 60.62677696744211175, 49.99999999997998401, 24.18439665018642870 ) ) ;
#70374 = CARTESIAN_POINT ( 'NONE',  ( -86.09514901757498251, -28.33536443523890114, 182.5650114012098300 ) ) ;
#70375 = EDGE_LOOP ( 'NONE', ( #84580, #70066, #75547, #16284, #71109, #64120 ) ) ;
#70376 = CARTESIAN_POINT ( 'NONE',  ( 36.71487963708168678, 414.8037251387460742, 6.149495645048446590 ) ) ;
#70377 = CARTESIAN_POINT ( 'NONE',  ( 4.364333581248146211E-05, -49.92101465095216639, 32.20981906809440432 ) ) ;
#70378 = CARTESIAN_POINT ( 'NONE',  ( -6.611591191889651498, 41.87945138500480624, -59.42330386243895646 ) ) ;
#70379 = CARTESIAN_POINT ( 'NONE',  ( 36.66272501222901781, 491.8430924522251075, 12.58828741394580497 ) ) ;
#70380 = CARTESIAN_POINT ( 'NONE',  ( -8.559508646656370345, 53.96349637827587031, 1.531152949374564365 ) ) ;
#70381 = CARTESIAN_POINT ( 'NONE',  ( -20.84783826651100114, 303.9031953955430367, -9.989077431537761953 ) ) ;
#70382 = LINE ( 'NONE', #45058, #89166 ) ;
#70383 = VECTOR ( 'NONE', #50700, 1000.000000000000000 ) ;
#70384 = DIRECTION ( 'NONE',  ( -1.000000000000000000, -1.224606353822377258E-16, -0.000000000000000000 ) ) ;
#70385 = CARTESIAN_POINT ( 'NONE',  ( 65.52222222222222570, 6.915964383211875250E-15, 0.000000000000000000 ) ) ;
#70386 = ORIENTED_EDGE ( 'NONE', *, *, #48459, .T. ) ;
#70387 = CARTESIAN_POINT ( 'NONE',  ( 19.36108815078635814, 50.00000000000000711, 60.09752357988048033 ) ) ;
#70388 = CARTESIAN_POINT ( 'NONE',  ( 10.03807929566702839, 14.08216048671749476, 10.50070806742469642 ) ) ;
#70389 = CARTESIAN_POINT ( 'NONE',  ( 20.16952962162617879, -4.285714285716217375, 15.50035291838605467 ) ) ;
#70390 = AXIS2_PLACEMENT_3D ( 'NONE', #17108, #8988, #34380 ) ;
#70391 = CARTESIAN_POINT ( 'NONE',  ( 9.812601528912281879, 53.40226535921740236, -2.922597654565728398 ) ) ;
#70392 = AXIS2_PLACEMENT_3D ( 'NONE', #75234, #100051, #36436 ) ;
#70393 = CARTESIAN_POINT ( 'NONE',  ( 94.21232436905559382, -59.99999999999992895, 13.85190642028294761 ) ) ;
#70394 = CARTESIAN_POINT ( 'NONE',  ( -80.01377271962273596, -32.56088685926365400, 138.7306771739739588 ) ) ;
#70395 = ORIENTED_EDGE ( 'NONE', *, *, #100852, .T. ) ;
#70396 = CARTESIAN_POINT ( 'NONE',  ( 35.59999999999999432, 1.533819458162526451E-15, 0.000000000000000000 ) ) ;
#70397 = DIRECTION ( 'NONE',  ( 1.000000000000000000, 1.224606353822377258E-16, 0.000000000000000000 ) ) ;
#70398 = CARTESIAN_POINT ( 'NONE',  ( 79.02477813168630405, -57.50590731851511350, 197.8598049514260708 ) ) ;
#70399 = CARTESIAN_POINT ( 'NONE',  ( 59.92186310548196815, 49.99999999999997868, -19.49309254038931272 ) ) ;
#70400 = UNCERTAINTY_MEASURE_WITH_UNIT (LENGTH_MEASURE( 1.000000000000000082E-05 ), #16557, 'distance_accuracy_value', 'NONE');
#70402 = VECTOR ( 'NONE', #79586, 1000.000000000000000 ) ;
#70401 = CARTESIAN_POINT ( 'NONE',  ( 44.56450693767920512, 340.0210625335878376, 0.8280807651409033410 ) ) ;
#70403 = CARTESIAN_POINT ( 'NONE',  ( 58.67238219402268840, 6.975173280561618775E-15, 0.000000000000000000 ) ) ;
#70404 = EDGE_LOOP ( 'NONE', ( #74749, #39361, #65481, #14571, #53064, #15827 ) ) ;
#70405 = CARTESIAN_POINT ( 'NONE',  ( -18.69420657816679210, 304.6310092840336097, -10.04693110555010982 ) ) ;
#70406 = DIRECTION ( 'NONE',  ( -0.000000000000000000, -0.000000000000000000, -1.000000000000000000 ) ) ;
#70407 = CARTESIAN_POINT ( 'NONE',  ( 5.082755093536325930, -27.96875000204838457, -5.082755093536325042 ) ) ;
#70408 = VERTEX_POINT ( 'NONE', #89218 ) ;
#70409 =( NAMED_UNIT ( * ) SI_UNIT ( $, .STERADIAN. ) SOLID_ANGLE_UNIT ( ) );
#70410 = CARTESIAN_POINT ( 'NONE',  ( 46.85000000000000142, 0.000000000000000000, 0.000000000000000000 ) ) ;
#70411 = CARTESIAN_POINT ( 'NONE',  ( 6.746994761561826870, 41.86978728249054882, -69.53909782334804390 ) ) ;
#70412 = EDGE_CURVE ( 'NONE', #29177, #40203, #74090, .T. ) ;
#70414 = DIRECTION ( 'NONE',  ( 1.000000000000000000, -0.000000000000000000, -0.000000000000000000 ) ) ;
#70413 = B_SPLINE_CURVE_WITH_KNOTS ( 'NONE', 3,
 ( #26400, #2060, #92138, #41466 ),
 .UNSPECIFIED., .F., .F.,
 ( 4, 4 ),
 ( 0.0005604261988817112747, 0.02562827970630954244 ),
 .UNSPECIFIED. ) ;
#70415 = CARTESIAN_POINT ( 'NONE',  ( -29.68315524077005207, 13.12249633091091816, -39.60535821593474282 ) ) ;
#70416 = EDGE_CURVE ( 'NONE', #27128, #79201, #55069, .T. ) ;
#70417 = DIRECTION ( 'NONE',  ( 0.000000000000000000, 0.000000000000000000, -1.000000000000000000 ) ) ;
#70418 = ORIENTED_EDGE ( 'NONE', *, *, #26591, .T. ) ;
#70419 = CARTESIAN_POINT ( 'NONE',  ( 38.79242140487948376, -60.00000000000000000, -39.81019021691462001 ) ) ;
#70421 = CARTESIAN_POINT ( 'NONE',  ( 24.64265655959308177, -32.51917606842599184, 30.48593585286307928 ) ) ;
#70420 = CARTESIAN_POINT ( 'NONE',  ( -44.76022593139747840, -29.99999999999992539, 54.38475608328532473 ) ) ;
#70422 = CARTESIAN_POINT ( 'NONE',  ( -7.499174415388573091E-15, 1.499999999999992450, 61.23540616453487218 ) ) ;
#70423 = VERTEX_POINT ( 'NONE', #10275 ) ;
#70424 = EDGE_CURVE ( 'NONE', #64595, #6722, #98192, .T. ) ;
#70425 = ORIENTED_EDGE ( 'NONE', *, *, #6649, .T. ) ;
#70426 = CARTESIAN_POINT ( 'NONE',  ( -19.00223544648544305, -4.285714285714295357, -16.66764709352488083 ) ) ;
#70427 = CARTESIAN_POINT ( 'NONE',  ( 47.33333333333330728, 59.99999999999999289, 23.66666666666666785 ) ) ;
#70428 = CARTESIAN_POINT ( 'NONE',  ( 0.000000000000000000, 79.50000000000000000, 0.000000000000000000 ) ) ;
#70429 = DIRECTION ( 'NONE',  ( 0.000000000000000000, -1.000000000000000000, 0.000000000000000000 ) ) ;
#70430 = FACE_OUTER_BOUND ( 'NONE', #79386, .T. ) ;
#70431 = CARTESIAN_POINT ( 'NONE',  ( -16.14595037822608603, 7.274337365576361236, 6.616591826368398266 ) ) ;
#70432 = ORIENTED_EDGE ( 'NONE', *, *, #8277, .T. ) ;
#70433 =( GEOMETRIC_REPRESENTATION_CONTEXT ( 3 ) GLOBAL_UNCERTAINTY_ASSIGNED_CONTEXT ( ( #35406 ) ) GLOBAL_UNIT_ASSIGNED_CONTEXT ( ( #81083, #74580, #56803 ) ) REPRESENTATION_CONTEXT ( 'NONE', 'WORKASPACE' ) );
#70434 = FACE_OUTER_BOUND ( 'NONE', #33923, .T. ) ;
#70435 = CARTESIAN_POINT ( 'NONE',  ( 98.10535912706410500, -29.99999999999996447, 190.4157711056429889 ) ) ;
#70436 = CARTESIAN_POINT ( 'NONE',  ( -10.38059036996056861, 10.84158485851692788, 10.42428711140174080 ) ) ;
#70438 = EDGE_CURVE ( 'NONE', #93666, #16458, #105071, .T. ) ;
#70437 = CARTESIAN_POINT ( 'NONE',  ( -6.000208918519490453, -80.99968662210035575, -0.2646532170642273973 ) ) ;
#70439 = CARTESIAN_POINT ( 'NONE',  ( 78.36382142249493654, -29.99999999999999645, -15.57094275508443815 ) ) ;
#70440 = PLANE ( 'NONE',  #72588 ) ;
#70441 = ORIENTED_EDGE ( 'NONE', *, *, #77644, .F. ) ;
#70442 = ORIENTED_EDGE ( 'NONE', *, *, #104047, .T. ) ;
#70443 = ORIENTED_EDGE ( 'NONE', *, *, #100761, .T. ) ;
#70444 = CARTESIAN_POINT ( 'NONE',  ( 100.0424503805845831, -2.002967142162725287E-29, 5.000000000000011546 ) ) ;
#70445 = LINE ( 'NONE', #30534, #35600 ) ;
#70446 = DIRECTION ( 'NONE',  ( 0.000000000000000000, 0.000000000000000000, 1.000000000000000000 ) ) ;
#70447 = FACE_OUTER_BOUND ( 'NONE', #49023, .T. ) ;
#70448 = CARTESIAN_POINT ( 'NONE',  ( -1.964652754746246677, -70.01532877525617948, 13.13671012408558347 ) ) ;
#70450 = CARTESIAN_POINT ( 'NONE',  ( -7.150053860865850375, -86.78265453913975591, 3.590189269391291571 ) ) ;
#70449 =( GEOMETRIC_REPRESENTATION_CONTEXT ( 3 ) GLOBAL_UNCERTAINTY_ASSIGNED_CONTEXT ( ( #87406 ) ) GLOBAL_UNIT_ASSIGNED_CONTEXT ( ( #16586, #96978, #24705 ) ) REPRESENTATION_CONTEXT ( 'NONE', 'WORKASPACE' ) );
#70451 = CARTESIAN_POINT ( 'NONE',  ( 38.86650669486618881, 1.474610560812782335E-15, 0.000000000000000000 ) ) ;
#70452 = ORIENTED_EDGE ( 'NONE', *, *, #95678, .F. ) ;
#70453 = CARTESIAN_POINT ( 'NONE',  ( 30.11650669486618881, 4.000000000000003553, 4.898587196589414801E-16 ) ) ;
#70454 = ORIENTED_EDGE ( 'NONE', *, *, #11747, .F. ) ;
#70455 = CARTESIAN_POINT ( 'NONE',  ( -4.497472161260644086, -64.45777453374053323, -3.972129482042465298 ) ) ;
#70456 = CARTESIAN_POINT ( 'NONE',  ( 44.47534377888507606, -38.31160956920668070, 57.00192013341546016 ) ) ;
#70457 = CARTESIAN_POINT ( 'NONE',  ( 0.000000000000000000, 0.000000000000000000, 5.000000000000002665 ) ) ;
#70458 = CARTESIAN_POINT ( 'NONE',  ( 28.24208341650309961, 297.1533231554286090, 10.44100024085842904 ) ) ;
#70459 =( GEOMETRIC_REPRESENTATION_CONTEXT ( 3 ) GLOBAL_UNCERTAINTY_ASSIGNED_CONTEXT ( ( #34414 ) ) GLOBAL_UNIT_ASSIGNED_CONTEXT ( ( #38276, #22083, #13951 ) ) REPRESENTATION_CONTEXT ( 'NONE', 'WORKASPACE' ) );
#70460 = DIRECTION ( 'NONE',  ( -1.000000000000000000, -1.224606353822377258E-16, -0.000000000000000000 ) ) ;
#70461 = CARTESIAN_POINT ( 'NONE',  ( 64.34760809152027150, -29.05394656327659675, 78.93212883145818637 ) ) ;
#70462 = ORIENTED_EDGE ( 'NONE', *, *, #24419, .T. ) ;
#70463 = DIRECTION ( 'NONE',  ( 0.000000000000000000, -1.000000000000000000, 0.000000000000000000 ) ) ;
#70464 = CARTESIAN_POINT ( 'NONE',  ( -46.37470752763751847, -34.70867711623044016, -36.69855284394721195 ) ) ;
#70465 = DIRECTION ( 'NONE',  ( -0.000000000000000000, 1.000000000000000000, -0.000000000000000000 ) ) ;
#70466 = CARTESIAN_POINT ( 'NONE',  ( -9.807756029461570435, 51.30004223800749941, 2.674464121017646967 ) ) ;
#70467 = EDGE_CURVE ( 'NONE', #21786, #66070, #72332, .T. ) ;
#70468 = EDGE_LOOP ( 'NONE', ( #76387, #32336, #8680, #39027, #7402 ) ) ;
#70469 = PRESENTATION_STYLE_ASSIGNMENT (( #86144 ) ) ;
#70470 = DIRECTION ( 'NONE',  ( -1.000000000000000000, -0.000000000000000000, -0.000000000000000000 ) ) ;
#70471 = CARTESIAN_POINT ( 'NONE',  ( 42.90606796463281825, 465.0680163536576401, 12.12009592768376898 ) ) ;
#70472 = EDGE_CURVE ( 'NONE', #43441, #25659, #79257, .T. ) ;
#70473 = EDGE_CURVE ( 'NONE', #73270, #958, #27477, .T. ) ;
#70474 = DIRECTION ( 'NONE',  ( -0.5735764363510497121, 0.8191520442889892450, 1.003171929053521665E-16 ) ) ;
#70475 = B_SPLINE_CURVE_WITH_KNOTS ( 'NONE', 3,
 ( #387, #74832, #50036, #8514, #48438, #97510 ),
 .UNSPECIFIED., .F., .F.,
 ( 4, 2, 4 ),
 ( 2.380733003137416059E-07, 0.001898835937927372897, 0.003797433802554431997 ),
 .UNSPECIFIED. ) ;
#70476 = CARTESIAN_POINT ( 'NONE',  ( -40.73953790046563483, -18.92596047533412573, 20.36976895023282452 ) ) ;
#70477 = DIRECTION ( 'NONE',  ( -0.5735764363510512664, 0.8191520442889881348, 1.003171929053520309E-16 ) ) ;
#70478 = CARTESIAN_POINT ( 'NONE',  ( 85.54013868611671967, -53.83156724899034629, 191.4350006523445984 ) ) ;
#70479 = AXIS2_PLACEMENT_3D ( 'NONE', #54194, #87133, #13207 ) ;
#70480 = DIRECTION ( 'NONE',  ( -1.000000000000000000, -1.224606353822377258E-16, -0.000000000000000000 ) ) ;
#70481 = CARTESIAN_POINT ( 'NONE',  ( -9.971054622642887111, 7.543597282511679047, 0.000000000000000000 ) ) ;
#70482 = CARTESIAN_POINT ( 'NONE',  ( 7.743982712349854580, -6.537869852392644177, 2.020119794285907044 ) ) ;
#70483 = CARTESIAN_POINT ( 'NONE',  ( -43.71297783477847787, 485.1278128289774827, -1.116606130290708876 ) ) ;
#70484 = CARTESIAN_POINT ( 'NONE',  ( 13.45844672282477816, -53.47313501769576050, 23.14344092887451154 ) ) ;
#70485 = DIRECTION ( 'NONE',  ( 0.000000000000000000, 0.000000000000000000, -1.000000000000000000 ) ) ;
#70486 = CARTESIAN_POINT ( 'NONE',  ( -97.58969750147805655, -30.00000000000000355, 134.6660703783357746 ) ) ;
#70487 = EDGE_CURVE ( 'NONE', #88742, #58039, #32060, .T. ) ;
#70488 = COLOUR_RGB ( '', 0.09019608, 0.27058824, 0.51372549) ;
#70489 = DIRECTION ( 'NONE',  ( 0.000000000000000000, -1.000000000000000000, 0.000000000000000000 ) ) ;
#70490 = CARTESIAN_POINT ( 'NONE',  ( 19.90515936436859334, -57.67199060621977225, 42.19861848689678396 ) ) ;
#70491 = AXIS2_PLACEMENT_3D ( 'NONE', #92384, #35251, #25582 ) ;
#70493 = LINE ( 'NONE', #63473, #41347 ) ;
#70492 = CARTESIAN_POINT ( 'NONE',  ( 9.032162165387472186, 43.92599673635245949, 14.03290463794137999 ) ) ;
#70494 = EDGE_CURVE ( 'NONE', #98741, #54371, #34497, .T. ) ;
#70495 = CARTESIAN_POINT ( 'NONE',  ( -37.55250343708862459, 42.26547160929953151, -58.87384313933568336 ) ) ;
#70496 = CARTESIAN_POINT ( 'NONE',  ( -17.64199176884268283, 50.00000000000000000, 62.53729709305390116 ) ) ;
#70497 = CARTESIAN_POINT ( 'NONE',  ( 18.91791044776121211, 47.00000000000000000, 62.18611311450883505 ) ) ;
#70498 = CARTESIAN_POINT ( 'NONE',  ( 3.454253436624935336, -0.8414180287960453253, 103.7259032015043232 ) ) ;
#70499 = ADVANCED_FACE ( 'NONE', ( #27040 ), #48220, .T. ) ;
#70500 = CARTESIAN_POINT ( 'NONE',  ( 0.2878250504871184279, -70.51393066051385006, 12.99060018351242540 ) ) ;
#70501 = VECTOR ( 'NONE', #97655, 1000.000000000000000 ) ;
#70502 = DIRECTION ( 'NONE',  ( 0.000000000000000000, -1.000000000000000000, 0.000000000000000000 ) ) ;
#70503 = CARTESIAN_POINT ( 'NONE',  ( -86.89094463637313481, -60.98404555833182172, 194.8809632880474680 ) ) ;
#70504 = EDGE_LOOP ( 'NONE', ( #2907, #21760, #22273, #9589, #73396, #30655 ) ) ;
#70505 = CARTESIAN_POINT ( 'NONE',  ( 41.32135724059154569, 485.4908763545889201, -3.838542627836866394 ) ) ;
#70506 = DIRECTION ( 'NONE',  ( 1.000000000000000000, 1.224606353822377258E-16, 0.000000000000000000 ) ) ;
#70507 = CARTESIAN_POINT ( 'NONE',  ( -13.71681562663793841, -56.88406381427680003, 33.46245320680461788 ) ) ;
#70509 = CARTESIAN_POINT ( 'NONE',  ( -42.77491504005183032, 436.8063544398164595, 20.35369978044113992 ) ) ;
#70508 = CARTESIAN_POINT ( 'NONE',  ( -103.3239848065108930, -60.00000000000002842, 136.7923039559513825 ) ) ;
#70510 = ORIENTED_EDGE ( 'NONE', *, *, #77867, .F. ) ;
#70511 = B_SPLINE_CURVE_WITH_KNOTS ( 'NONE', 3,
 ( #66257, #43058, #415, #26908, #59782, #92658, #84583, #18818, #43579, #58713, #58160, #76466, #33382, #99142, #25302, #91088, #17195, #82977, #53792, #52728, #87238, #30075, #94810, #37122, #71039, #45197, #77547, #20432, #4186, #13317, #94267, #29562, #86193, #103930 ),
 .UNSPECIFIED., .F., .F.,
 ( 4, 2, 2, 2, 2, 2, 2, 2, 2, 2, 2, 2, 2, 2, 2, 2, 4 ),
 ( 0.06792443330486737374, 0.06987512198849422929, 0.07182581067212108483, 0.07572718803937480980, 0.07962856540662852090, 0.08352994277388223199, 0.09133269750838966805, 0.09913545224289710411, 0.1010861409265239735, 0.1030368296101508430, 0.1069382069774045818, 0.1108395843446583068, 0.1127902730282851762, 0.1147409617119120595, 0.1225437164464195927, 0.1264450938136733593, 0.1303464711809270982 ),
 .UNSPECIFIED. ) ;
#70512 = CARTESIAN_POINT ( 'NONE',  ( -14.75116209839011994, 43.55504285526384933, -90.22050492866908655 ) ) ;
#70513 = VECTOR ( 'NONE', #55827, 1000.000000000000000 ) ;
#70514 = CARTESIAN_POINT ( 'NONE',  ( 16.01290064681821335, 3.743845801208731672, 0.6463026410229945062 ) ) ;
#70515 = CARTESIAN_POINT ( 'NONE',  ( -32.16694665535142406, 298.7751107022914425, -9.134474995493537364 ) ) ;
#70516 = VERTEX_POINT ( 'NONE', #73005 ) ;
#70517 = SURFACE_SIDE_STYLE ('',( #29047 ) ) ;
#70518 = CARTESIAN_POINT ( 'NONE',  ( 7.360438360688435822, 50.00000000000000711, -94.60993813358487614 ) ) ;
#70519 = TOROIDAL_SURFACE ( 'NONE', #32671, 15.43455230191221261, 0.5000000000000000000 ) ;
#70520 = CONICAL_SURFACE ( 'NONE', #60233, 4.172000000000001485, 0.9599310885968750373 ) ;
#70521 = PRESENTATION_STYLE_ASSIGNMENT (( #20959 ) ) ;
#70522 = LINE ( 'NONE', #38182, #20074 ) ;
#70523 = ORIENTED_EDGE ( 'NONE', *, *, #105401, .T. ) ;
#70524 = ORIENTED_EDGE ( 'NONE', *, *, #104404, .T. ) ;
#70525 = ORIENTED_EDGE ( 'NONE', *, *, #29407, .F. ) ;
#70526 = CARTESIAN_POINT ( 'NONE',  ( 0.000000000000000000, 80.00000000000000000, 0.000000000000000000 ) ) ;
#70527 = CARTESIAN_POINT ( 'NONE',  ( 5.656854249492378806, -14.37500000409677092, 5.656854249492381470 ) ) ;
#70528 = CARTESIAN_POINT ( 'NONE',  ( 23.58349330513380337, 1.593028355512270962E-15, 0.000000000000000000 ) ) ;
#70529 = ORIENTED_EDGE ( 'NONE', *, *, #55082, .T. ) ;
#70530 = EDGE_CURVE ( 'NONE', #62962, #91741, #62049, .T. ) ;
#70531 = CARTESIAN_POINT ( 'NONE',  ( -6.441911206406983226, 41.95837094207923457, -69.50559752220233634 ) ) ;
#70532 = B_SPLINE_CURVE_WITH_KNOTS ( 'NONE', 3,
 ( #68053, #101493, #99888, #3324 ),
 .UNSPECIFIED., .F., .F.,
 ( 4, 4 ),
 ( 9.813077866773594792E-18, 0.001950293525757634773 ),
 .UNSPECIFIED. ) ;
#70533 = CONICAL_SURFACE ( 'NONE', #92917, 3.309500000000001663, 0.9599310885968770357 ) ;
#70534 = CARTESIAN_POINT ( 'NONE',  ( -99.84173967043324183, -59.99999999999388223, 204.4316739029779342 ) ) ;
#70535 = CARTESIAN_POINT ( 'NONE',  ( 43.40712426123182865, 434.3590067275469551, 15.37327885490085499 ) ) ;
#70536 = AXIS2_PLACEMENT_3D ( 'NONE', #100575, #59072, #91957 ) ;
#70537 = CARTESIAN_POINT ( 'NONE',  ( 75.93419637478046980, -59.99999999999036504, -32.67258319081769713 ) ) ;
#70538 = CARTESIAN_POINT ( 'NONE',  ( 3.981862520314373377, 0.000000000000000000, -0.01269999999999786924 ) ) ;
#70539 = CARTESIAN_POINT ( 'NONE',  ( -6.249702485612488978, 41.65323702329418865, -58.70056700059317478 ) ) ;
#70541 = CARTESIAN_POINT ( 'NONE',  ( 10.08504398947854064, -22.06746529747525187, 27.57661867756857532 ) ) ;
#70540 = CARTESIAN_POINT ( 'NONE',  ( -98.01432676219248208, -59.99999999999999289, 53.56972733528865405 ) ) ;
#70542 = ADVANCED_FACE ( 'NONE', ( #32599 ), #25001, .T. ) ;
#70543 = DIRECTION ( 'NONE',  ( 0.000000000000000000, -1.000000000000000000, 0.000000000000000000 ) ) ;
#70544 = PRESENTATION_LAYER_ASSIGNMENT (  '', '', ( #25784 ) ) ;
#70545 = EDGE_CURVE ( 'NONE', #68161, #45532, #88429, .T. ) ;
#70546 = CARTESIAN_POINT ( 'NONE',  ( -48.47199924648073477, -29.14092461735632966, 45.10971830478670341 ) ) ;
#70547 = DIRECTION ( 'NONE',  ( 1.000000000000000000, -0.000000000000000000, -0.000000000000000000 ) ) ;
#70548 = VERTEX_POINT ( 'NONE', #63634 ) ;
#70549 = DIRECTION ( 'NONE',  ( 0.000000000000000000, 1.000000000000000000, 0.000000000000000000 ) ) ;
#70550 = CARTESIAN_POINT ( 'NONE',  ( 17.07807050392529291, 37.03766137757074972, 21.83949354139796029 ) ) ;
#70551 = VECTOR ( 'NONE', #13077, 1000.000000000000000 ) ;
#70552 = ADVANCED_FACE ( 'NONE', ( #7475 ), #38309, .T. ) ;
#70553 = DIRECTION ( 'NONE',  ( 0.000000000000000000, 0.000000000000000000, 1.000000000000000000 ) ) ;
#70554 = ORIENTED_EDGE ( 'NONE', *, *, #84476, .T. ) ;
#70555 = CARTESIAN_POINT ( 'NONE',  ( -5.893532595998363099, -15.73385846051533044, 14.28825528099932818 ) ) ;
#70556 = EDGE_LOOP ( 'NONE', ( #7426, #20419, #80826 ) ) ;
#70557 = CARTESIAN_POINT ( 'NONE',  ( 86.11313230656898554, -29.99999999999747047, -19.76934824123757295 ) ) ;
#70558 = PRESENTATION_STYLE_ASSIGNMENT (( #76503 ) ) ;
#70560 = EDGE_CURVE ( 'NONE', #48477, #49781, #5653, .T. ) ;
#70559 = CARTESIAN_POINT ( 'NONE',  ( -1.444753424442138723, -6.061373582658561077, -13.74655991887425088 ) ) ;
#70561 = CARTESIAN_POINT ( 'NONE',  ( -36.40416150969235787, 41.99999999991774757, -47.37019975554808582 ) ) ;
#70562 = CARTESIAN_POINT ( 'NONE',  ( 99.08546831463196725, -30.00000000000000000, 188.6244390898592087 ) ) ;
#70563 = B_SPLINE_SURFACE_WITH_KNOTS ( 'NONE', 3, 3, ( 
 ( #23476, #63403, #32087, #64963, #39117, #38082, #70938, #103831 ),
 ( #29976, #26152, #57920, #34762, #34224, #41747, #50356, #90839 ),
 ( #90301, #91897, #713, #8312, #89778, #82739, #66556, #74634 ),
 ( #16410, #16957, #25063, #25613, #41215, #49834, #49290, #91378 ),
 ( #99434, #58473, #98903, #82195, #191, #9903, #74101, #42813 ),
 ( #33154, #8842, #66024, #67635, #17496, #33683, #83270, #9360 ),
 ( #50887, #26668, #42273, #75164, #75708, #83792, #59008, #1255 ),
 ( #100512, #18022, #67097, #99981, #24538, #1803, #15882, #106470 ),
 ( #7776, #48757, #81651, #40681, #73567, #32628, #65501, #98390 ),
 ( #57388, #94026, #93509, #51429, #44417, #36889, #102650, #11491 ) ),
 .UNSPECIFIED., .F., .F., .F.,
 ( 4, 2, 2, 2, 4 ),
 ( 4, 2, 2, 4 ),
 ( 0.000000000000000000, 0.1250000000000000000, 0.2500000000000000000, 0.5000000000000000000, 1.000000000000000000 ),
 ( 0.000000000000000000, 0.2500000000000000000, 0.5000000000000000000, 1.000000000000000000 ),
 .UNSPECIFIED. ) ;
#70564 = CARTESIAN_POINT ( 'NONE',  ( -80.00000000000000000, -60.00000000000000000, -21.09707704303352926 ) ) ;
#70565 = EDGE_LOOP ( 'NONE', ( #4188, #66718, #22646, #94891 ) ) ;
#70566 = VECTOR ( 'NONE', #43801, 999.9999999999998863 ) ;
#70567 = EDGE_LOOP ( 'NONE', ( #65430, #58376 ) ) ;
#70568 = VERTEX_POINT ( 'NONE', #55492 ) ;
#70569 = CARTESIAN_POINT ( 'NONE',  ( 54.06147519409380919, -46.43629282806927705, 61.05405196347986418 ) ) ;
#70570 = FACE_OUTER_BOUND ( 'NONE', #84103, .T. ) ;
#70571 = DIRECTION ( 'NONE',  ( 1.000000000000000000, 0.000000000000000000, 0.000000000000000000 ) ) ;
#70572 = VERTEX_POINT ( 'NONE', #29692 ) ;
#70573 = CARTESIAN_POINT ( 'NONE',  ( -16.01537606005192771, 3.832707337346620502, -1.292662844555364066 ) ) ;
#70574 = TOROIDAL_SURFACE ( 'NONE', #24086, 10.00000000000000000, 5.000000000000000000 ) ;
#70575 = VERTEX_POINT ( 'NONE', #46888 ) ;
#70576 = CARTESIAN_POINT ( 'NONE',  ( 22.25669491856071858, 5.000000000000003553, 0.000000000000000000 ) ) ;
#70577 = CARTESIAN_POINT ( 'NONE',  ( 95.33069953613802738, -38.48758898485506563, 201.2218942298954403 ) ) ;
#70578 = CARTESIAN_POINT ( 'NONE',  ( 14.52498819721216705, 21.59802860051696172, 5.113706971753962272 ) ) ;
#70579 = CARTESIAN_POINT ( 'NONE',  ( 85.20578200364217025, -52.71162868700685777, 3.232510328549902834 ) ) ;
#70580 = LINE ( 'NONE', #102942, #2914 ) ;
#70581 = CARTESIAN_POINT ( 'NONE',  ( 42.70315986187589630, 433.3238984461618770, 18.58428708097476445 ) ) ;
#70582 = DIRECTION ( 'NONE',  ( 0.000000000000000000, -1.000000000000000000, 0.000000000000000000 ) ) ;
#70583 = AXIS2_PLACEMENT_3D ( 'NONE', #31140, #96904, #79120 ) ;
#70584 = CARTESIAN_POINT ( 'NONE',  ( -42.29287336469099046, 486.6964296286192280, 8.722237745847708723 ) ) ;
#70585 = VERTEX_POINT ( 'NONE', #15583 ) ;
#70586 = DIRECTION ( 'NONE',  ( -0.5735764363510510444, -0.8191520442889883569, 0.000000000000000000 ) ) ;
#70587 = DIRECTION ( 'NONE',  ( 0.1946996363168976285, 0.08778327892717602277, 0.9769268895669018793 ) ) ;
#70588 = ORIENTED_EDGE ( 'NONE', *, *, #101340, .T. ) ;
#70589 = CARTESIAN_POINT ( 'NONE',  ( -20.59205717438620553, 304.8780392497436651, -8.994432684286490343 ) ) ;
#70590 = CARTESIAN_POINT ( 'NONE',  ( -36.33898061045209715, 308.9542109619496841, 13.29915945452285442 ) ) ;
#70591 = CARTESIAN_POINT ( 'NONE',  ( -12.07109306393920178, -4.718911993881638622, -76.83903857454983211 ) ) ;
#70592 = CARTESIAN_POINT ( 'NONE',  ( 0.1061556211655303172, -4.836380039389409191, 4.623144047065555817 ) ) ;
#70593 = CARTESIAN_POINT ( 'NONE',  ( -3.313708498984760720, -22.53124999999999289, -8.000000000000000000 ) ) ;
#70594 = CARTESIAN_POINT ( 'NONE',  ( 36.53097960655163234, -27.14942307569473812, 43.41884094172100106 ) ) ;
#70595 = CIRCLE ( 'NONE', #91234, 0.5999999999999980904 ) ;
#70596 = EDGE_CURVE ( 'NONE', #30663, #67595, #46373, .T. ) ;
#70597 = CARTESIAN_POINT ( 'NONE',  ( 4.699999999999999289, 0.000000000000000000, 0.000000000000000000 ) ) ;
#70598 = ORIENTED_EDGE ( 'NONE', *, *, #46491, .F. ) ;
#70599 = CARTESIAN_POINT ( 'NONE',  ( 86.13523834728314910, -21.45781864377238080, 175.8968767354805891 ) ) ;
#70600 = CARTESIAN_POINT ( 'NONE',  ( -48.87659302348963308, 8.116727071898555579, 16.52478270335610944 ) ) ;
#70601 = EDGE_LOOP ( 'NONE', ( #18292, #16346, #21632, #94965, #54431, #41238 ) ) ;
#70602 = CARTESIAN_POINT ( 'NONE',  ( 93.83738680290022671, -57.67473493691561970, 11.13690244224351744 ) ) ;
#70603 = DIRECTION ( 'NONE',  ( -1.000000000000000000, 0.000000000000000000, 0.000000000000000000 ) ) ;
#70604 = CARTESIAN_POINT ( 'NONE',  ( -8.831401106173711213, -5.000000000000002665, -94.83329464149440469 ) ) ;
#70605 = CARTESIAN_POINT ( 'NONE',  ( -30.63612296757520070, 10.92940684821784991, 40.03790167141636402 ) ) ;
#70606 = CARTESIAN_POINT ( 'NONE',  ( -10.39125135082022133, -22.71708686573491676, -38.54243321615867046 ) ) ;
#70607 = EDGE_CURVE ( 'NONE', #673, #44445, #48294, .T. ) ;
#70608 = VECTOR ( 'NONE', #53295, 1000.000000000000227 ) ;
#70609 = CIRCLE ( 'NONE', #51652, 4.000000000000007105 ) ;
#70610 = CARTESIAN_POINT ( 'NONE',  ( 14.34351097178316792, -22.32601165078034100, 35.84233650071320909 ) ) ;
#70611 = SURFACE_STYLE_USAGE ( .BOTH. , #52286 ) ;
#70612 = CARTESIAN_POINT ( 'NONE',  ( 40.88865618426756754, -26.70336337441984398, 36.55245364840668287 ) ) ;
#70615 = CARTESIAN_POINT ( 'NONE',  ( -10.13439797861699709, 12.24732348816224459, 10.56111555127041335 ) ) ;
#70614 = CIRCLE ( 'NONE', #75765, 5.000000000000002665 ) ;
#70613 = CARTESIAN_POINT ( 'NONE',  ( -20.00000000000000000, 12.99999999999999289, 4.000000000000000000 ) ) ;
#70616 = CARTESIAN_POINT ( 'NONE',  ( 9.720388148916125459, 294.7585724938356293, -10.04291177961258974 ) ) ;
#70617 = CARTESIAN_POINT ( 'NONE',  ( -15.45459933393545704, 44.08658193089431165, -5.012668390913509242 ) ) ;
#70618 = CARTESIAN_POINT ( 'NONE',  ( 42.97989905721253479, 343.7189603545139676, 9.566017304031658952 ) ) ;
#70619 = CARTESIAN_POINT ( 'NONE',  ( 0.000000000000000000, -79.93083296558610584, -85.00000000000000000 ) ) ;
#70620 = CONICAL_SURFACE ( 'NONE', #44763, 3.309500000000001663, 0.9599310885968770357 ) ;
#70621 = EDGE_CURVE ( 'NONE', #9016, #21775, #20812, .T. ) ;
#70622 = CARTESIAN_POINT ( 'NONE',  ( -82.92878276329815890, -38.00000000000002132, -11.27138431556246445 ) ) ;
#70623 = ORIENTED_EDGE ( 'NONE', *, *, #88646, .T. ) ;
#70624 = CARTESIAN_POINT ( 'NONE',  ( -9.720412966709314873, -3.400720061511772307, 14.97537720455055421 ) ) ;
#70625 = CARTESIAN_POINT ( 'NONE',  ( 4.472135954999577834, -64.72588149001673230, -4.000000000000002665 ) ) ;
#70627 = CARTESIAN_POINT ( 'NONE',  ( -3.091876355183101222, -21.77033853492639892, -30.49856546722038075 ) ) ;
#70626 = SURFACE_STYLE_FILL_AREA ( #80823 ) ;
#70628 = ORIENTED_EDGE ( 'NONE', *, *, #64066, .F. ) ;
#70629 = CIRCLE ( 'NONE', #58633, 8.000000000000000000 ) ;
#70630 = CARTESIAN_POINT ( 'NONE',  ( 5.335963852944037633, 6.035591050531996515, -7.593821156097438241 ) ) ;
#70631 = CARTESIAN_POINT ( 'NONE',  ( 33.86650669486618881, 4.898587196589411843E-16, -4.000000000000000888 ) ) ;
#70632 = ORIENTED_EDGE ( 'NONE', *, *, #17205, .T. ) ;
#70633 = FACE_BOUND ( 'NONE', #34139, .T. ) ;
#70634 = AXIS2_PLACEMENT_3D ( 'NONE', #578, #82606, #41086 ) ;
#70635 = DIRECTION ( 'NONE',  ( 0.000000000000000000, 0.000000000000000000, -1.000000000000000000 ) ) ;
#70636 = CARTESIAN_POINT ( 'NONE',  ( -92.72129515489801577, -59.99999999999999289, -5.456489434213922074 ) ) ;
#70637 = ORIENTED_EDGE ( 'NONE', *, *, #12175, .F. ) ;
#70638 = DIRECTION ( 'NONE',  ( -1.000000000000000000, -1.224606353822377258E-16, -0.000000000000000000 ) ) ;
#70639 = CARTESIAN_POINT ( 'NONE',  ( 30.00000000000000000, 488.7759337287082531, 4.253621113605315252 ) ) ;
#70640 = CYLINDRICAL_SURFACE ( 'NONE', #59847, 5.000000000000002665 ) ;
#70642 = DIRECTION ( 'NONE',  ( 0.000000000000000000, -1.000000000000000000, 0.000000000000000000 ) ) ;
#70641 = CARTESIAN_POINT ( 'NONE',  ( 0.000000000000000000, -4.000000000000003553, 118.0000000000000000 ) ) ;
#70643 = AXIS2_PLACEMENT_3D ( 'NONE', #95198, #21858, #54167 ) ;
#70644 = CARTESIAN_POINT ( 'NONE',  ( -84.90416487719758720, -22.08403841940192791, 159.8761325681244898 ) ) ;
#70645 = VERTEX_POINT ( 'NONE', #22655 ) ;
#70646 = CARTESIAN_POINT ( 'NONE',  ( 6.499999999999996447, 3.752776749732559036, -6.177805531629057434 ) ) ;
#70647 = ORIENTED_EDGE ( 'NONE', *, *, #12563, .F. ) ;
#70648 = ORIENTED_EDGE ( 'NONE', *, *, #26457, .F. ) ;
#70649 = CARTESIAN_POINT ( 'NONE',  ( 13.20528892216484707, -4.332661967058641928, 12.52414413171604046 ) ) ;
#70650 = DIRECTION ( 'NONE',  ( 0.000000000000000000, -1.000000000000000000, 0.000000000000000000 ) ) ;
#70651 = FILL_AREA_STYLE_COLOUR ( '', #141 ) ;
#70652 = ORIENTED_EDGE ( 'NONE', *, *, #51710, .T. ) ;
#70653 = CARTESIAN_POINT ( 'NONE',  ( -31.88312667699394609, 463.8062602911185195, 15.68962056581293041 ) ) ;
#70654 = DIRECTION ( 'NONE',  ( 0.000000000000000000, -1.000000000000000000, 0.000000000000000000 ) ) ;
#70655 = CARTESIAN_POINT ( 'NONE',  ( -77.41886385744251697, -57.67119865640713527, -31.55546021046578531 ) ) ;
#70656 = CARTESIAN_POINT ( 'NONE',  ( 1.889565883275343694, -49.90613408882943247, 101.9317875358934486 ) ) ;
#70657 = EDGE_CURVE ( 'NONE', #53673, #102845, #29138, .T. ) ;
#70658 = CYLINDRICAL_SURFACE ( 'NONE', #102988, 4.000000000000000000 ) ;
#70659 = CARTESIAN_POINT ( 'NONE',  ( 24.42523734047254891, 27.59258781593598542, 31.59665717925384243 ) ) ;
#70660 = CARTESIAN_POINT ( 'NONE',  ( 46.00000000000000000, 500.0000000000002274, 0.000000000000000000 ) ) ;
#70661 = CARTESIAN_POINT ( 'NONE',  ( 3.572352985695238292, 15.21714514899076143, -9.341953373612907896 ) ) ;
#70662 = AXIS2_PLACEMENT_3D ( 'NONE', #61074, #62666, #11422 ) ;
#70663 = CARTESIAN_POINT ( 'NONE',  ( 89.66268371970539874, -30.00000000000002487, 1.291492552605954858 ) ) ;
#70664 = EDGE_CURVE ( 'NONE', #78629, #34141, #28827, .T. ) ;
#70665 = CARTESIAN_POINT ( 'NONE',  ( -70.37903440132366484, -60.00000000000007816, 160.1141433014324207 ) ) ;
#70666 = ADVANCED_FACE ( 'NONE', ( #54970 ), #86222, .F. ) ;
#70667 = CARTESIAN_POINT ( 'NONE',  ( -55.11144128549652521, -42.97100987774245340, 61.94656224094574526 ) ) ;
#70668 = ORIENTED_EDGE ( 'NONE', *, *, #46495, .F. ) ;
#70669 = ORIENTED_EDGE ( 'NONE', *, *, #31759, .T. ) ;
#70670 = CARTESIAN_POINT ( 'NONE',  ( -100.8738977265185639, -45.26319457549800518, 191.5258224205792601 ) ) ;
#70671 = CARTESIAN_POINT ( 'NONE',  ( -1.009927083827795835, 51.97655585224438113, 8.245822313973391715 ) ) ;
#70672 = ORIENTED_EDGE ( 'NONE', *, *, #1136, .F. ) ;
#70673 = CARTESIAN_POINT ( 'NONE',  ( 18.94211536943317142, 49.24611979230877523, 62.05162962396204307 ) ) ;
#70674 = CARTESIAN_POINT ( 'NONE',  ( 11.36650669486618881, -3.999999999999998224, 0.000000000000000000 ) ) ;
#70675 = CARTESIAN_POINT ( 'NONE',  ( 5.082755093536325930, -13.34375000204838457, -5.082755093536325042 ) ) ;
#70676 = CARTESIAN_POINT ( 'NONE',  ( 34.95237279327285762, 304.8277712208536627, 12.26231981495593537 ) ) ;
#70678 = EDGE_CURVE ( 'NONE', #14310, #46925, #31792, .T. ) ;
#70677 = FILL_AREA_STYLE_COLOUR ( '', #52937 ) ;
#70679 = DIRECTION ( 'NONE',  ( 0.000000000000000000, 1.000000000000000000, 0.000000000000000000 ) ) ;
#70680 = CARTESIAN_POINT ( 'NONE',  ( -27.18908553330205180, 296.5274986157688772, 10.30015177545897842 ) ) ;
#70681 =( BOUNDED_SURFACE ( )  B_SPLINE_SURFACE ( 3, 2, ( 
 ( #96044, #14035, #64217 ),
 ( #104113, #4909, #37840 ),
 ( #23230, #21647, #104649 ),
 ( #103075, #80900, #80363 ) ),
 .UNSPECIFIED., .F., .F., .F. ) 
 B_SPLINE_SURFACE_WITH_KNOTS ( ( 4, 4 ),
 ( 3, 3 ),
 ( 0.01376892490370208375, 0.01435419950459561333 ),
 ( 0.000000000000000000, 0.8308924645139164067 ),
 .UNSPECIFIED. ) 
 GEOMETRIC_REPRESENTATION_ITEM ( )  RATIONAL_B_SPLINE_SURFACE ( (
 ( 1.000000000000000000, 0.7566372315800875548, 0.9176910440068761776),
 ( 1.000000000000000000, 0.7618160164815166446, 0.9194425871098625969),
 ( 1.000000000000000000, 0.7669224193548869195, 0.9211696495200920598),
 ( 1.000000000000000000, 0.7719586918116361218, 0.9228729927664867105) ) ) 
 REPRESENTATION_ITEM ( '' )  SURFACE ( )  );
#70682 = ADVANCED_FACE ( 'NONE', ( #54429 ), #94628, .T. ) ;
#70683 = FACE_OUTER_BOUND ( 'NONE', #79410, .T. ) ;
#70684 = CYLINDRICAL_SURFACE ( 'NONE', #58282, 5.000000000000000888 ) ;
#70685 = CARTESIAN_POINT ( 'NONE',  ( -33.81613602126189022, 485.0484310908490784, 1.468412048120518509 ) ) ;
#70686 = UNCERTAINTY_MEASURE_WITH_UNIT (LENGTH_MEASURE( 1.000000000000000082E-05 ), #101775, 'distance_accuracy_value', 'NONE');
#70687 = CARTESIAN_POINT ( 'NONE',  ( -29.33270313108591054, -42.96186199998404476, 33.51438719604331595 ) ) ;
#70688 = CIRCLE ( 'NONE', #24205, 18.00000000000000000 ) ;
#70689 = ORIENTED_EDGE ( 'NONE', *, *, #102592, .F. ) ;
#70690 = ORIENTED_EDGE ( 'NONE', *, *, #75502, .F. ) ;
#70691 = CARTESIAN_POINT ( 'NONE',  ( 48.13898221510520159, -25.68296270444842833, 43.60581086135196216 ) ) ;
#70692 = CARTESIAN_POINT ( 'NONE',  ( -0.3597357069889666747, 7.865396870477057156, 51.69868941200407164 ) ) ;
#70693 = CARTESIAN_POINT ( 'NONE',  ( -6.880814520906026743, 16.78853395715312757, -1.310034959478670658 ) ) ;
#70694 = CIRCLE ( 'NONE', #84475, 4.172000000000009479 ) ;
#70695 = CARTESIAN_POINT ( 'NONE',  ( -108.9040701096337642, -38.35651194470214165, 190.4373969938603750 ) ) ;
#70696 = ORIENTED_EDGE ( 'NONE', *, *, #75342, .T. ) ;
#70697 = CARTESIAN_POINT ( 'NONE',  ( 90.70450050837293077, -38.34778541823943243, 17.01427291654408691 ) ) ;
#70698 = CARTESIAN_POINT ( 'NONE',  ( 14.63753376598433142, 5.968491795188165305, -7.115311643837329392 ) ) ;
#70699 = CARTESIAN_POINT ( 'NONE',  ( 18.13561277374696701, 1.340359594676612611E-15, 0.000000000000000000 ) ) ;
#70700 = SURFACE_SIDE_STYLE ('',( #102535 ) ) ;
#70701 = CARTESIAN_POINT ( 'NONE',  ( 5.582554291377552325, 41.37363159368051413, -70.85834491557551473 ) ) ;
#70702 = CARTESIAN_POINT ( 'NONE',  ( -31.55677019160819796, 436.6743556880023789, 19.26287365877006152 ) ) ;
#70703 = CARTESIAN_POINT ( 'NONE',  ( -32.04888029241991632, 435.5715400069649945, 16.73152881174828366 ) ) ;
#70704 = CARTESIAN_POINT ( 'NONE',  ( 95.81331084581961477, -60.00000000000000711, 202.5570423909187241 ) ) ;
#70705 = COLOUR_RGB ( '', 0.66274510, 0.83137255, 0.94901961) ;
#70706 = CYLINDRICAL_SURFACE ( 'NONE', #81803, 4.000000000000000888 ) ;
#70707 = VECTOR ( 'NONE', #37966, 1000.000000000000000 ) ;
#70708 = ORIENTED_EDGE ( 'NONE', *, *, #26695, .F. ) ;
#70709 = CARTESIAN_POINT ( 'NONE',  ( -33.89998135744182406, 300.3151453263810140, -8.778418284323066700 ) ) ;
#70710 = CARTESIAN_POINT ( 'NONE',  ( 3.214365674769854575, -48.98477521967217285, 104.3190434908433559 ) ) ;
#70711 = CARTESIAN_POINT ( 'NONE',  ( -6.928203230275510549, 30.00000000000000000, 4.000000000000000000 ) ) ;
#70712 = ORIENTED_EDGE ( 'NONE', *, *, #76927, .T. ) ;
#70713 = AXIS2_PLACEMENT_3D ( 'NONE', #88916, #80271, #63598 ) ;
#70715 = DIRECTION ( 'NONE',  ( -1.000000000000000000, 0.000000000000000000, 0.000000000000000000 ) ) ;
#70714 = CARTESIAN_POINT ( 'NONE',  ( -104.7804267488673702, -38.39777790597128160, 197.7088218984990249 ) ) ;
#70716 = CARTESIAN_POINT ( 'NONE',  ( 0.000000000000000000, 0.000000000000000000, 0.000000000000000000 ) ) ;
#70717 = CARTESIAN_POINT ( 'NONE',  ( -9.797174393178825657E-16, -3.000000000000000000, 8.000000000000000000 ) ) ;
#70718 = CARTESIAN_POINT ( 'NONE',  ( 7.188101187500001821, -11.93750000204838457, -2.977408999572650483 ) ) ;
#70719 = CARTESIAN_POINT ( 'NONE',  ( 0.000000000000000000, -5.000000000000002665, -73.00000000000001421 ) ) ;
#70720 = ADVANCED_FACE ( 'NONE', ( #96920 ), #5286, .T. ) ;
#70721 = FILL_AREA_STYLE_COLOUR ( '', #100038 ) ;
#70722 = ORIENTED_EDGE ( 'NONE', *, *, #75458, .F. ) ;
#70723 = CARTESIAN_POINT ( 'NONE',  ( 82.82554601665236760, -42.97346742193234093, 173.7275920582182209 ) ) ;
#70724 = CARTESIAN_POINT ( 'NONE',  ( 9.269703125412263489, 140.3128462412892929, 1.540743955509799543E-30 ) ) ;
#70725 = CARTESIAN_POINT ( 'NONE',  ( 36.58643307874533690, 27.99658350115647565, 12.99814384291319769 ) ) ;
#70726 = EDGE_LOOP ( 'NONE', ( #78944, #96818, #102466, #38287 ) ) ;
#70727 = CARTESIAN_POINT ( 'NONE',  ( -35.93449038250053462, 329.4584288211232774, -3.491322705308419483 ) ) ;
#70728 = CARTESIAN_POINT ( 'NONE',  ( 0.000000000000000000, 0.000000000000000000, 0.000000000000000000 ) ) ;
#70729 = CARTESIAN_POINT ( 'NONE',  ( -30.00000000000000000, 0.000000000000000000, 0.000000000000000000 ) ) ;
#70730 = EDGE_CURVE ( 'NONE', #72311, #41058, #39705, .T. ) ;
#70731 = EDGE_LOOP ( 'NONE', ( #100693, #71122, #56587, #56559, #33716, #102991 ) ) ;
#70732 = SURFACE_STYLE_USAGE ( .BOTH. , #93428 ) ;
#70733 = CARTESIAN_POINT ( 'NONE',  ( -76.70973338117516960, -29.99999999999999645, -16.85903177628167171 ) ) ;
#70734 = AXIS2_PLACEMENT_3D ( 'NONE', #19590, #102583, #28731 ) ;
#70735 = CARTESIAN_POINT ( 'NONE',  ( -5.000000000000000000, -8.792118119421601818, -8.558778717960986882 ) ) ;
#70736 = CARTESIAN_POINT ( 'NONE',  ( -15.00099999999999767, 12.99999999999999289, 4.000000000000000000 ) ) ;
#70738 = DIRECTION ( 'NONE',  ( 0.000000000000000000, -0.8784936690177097551, 0.4777539884666615055 ) ) ;
#70737 = DIRECTION ( 'NONE',  ( 0.000000000000000000, 0.000000000000000000, 1.000000000000000000 ) ) ;
#70739 = VECTOR ( 'NONE', #98022, 999.9999999999998863 ) ;
#70740 = CARTESIAN_POINT ( 'NONE',  ( 4.401442555609581635E-16, -18.78125000204838457, -7.188101187500000044 ) ) ;
#70741 = CARTESIAN_POINT ( 'NONE',  ( 72.11682663846713126, -4.000000000000000000, 4.898587196589421703E-16 ) ) ;
#70742 =( REPRESENTATION_RELATIONSHIP ('NONE','NONE', #69581, #81203 ) REPRESENTATION_RELATIONSHIP_WITH_TRANSFORMATION ( #84808 )SHAPE_REPRESENTATION_RELATIONSHIP( ) );
#70743 = CARTESIAN_POINT ( 'NONE',  ( -9.165151389911679658, 30.00000000000000000, 4.000000000000000000 ) ) ;
#70744 = ADVANCED_FACE ( 'NONE', ( #95868 ), #39232, .T. ) ;
#70745 = ORIENTED_EDGE ( 'NONE', *, *, #27257, .F. ) ;
#70746 = FACE_OUTER_BOUND ( 'NONE', #62034, .T. ) ;
#70747 = CARTESIAN_POINT ( 'NONE',  ( 43.43869229197127169, 464.9661605157749591, 13.42065392471465834 ) ) ;
#70748 = CARTESIAN_POINT ( 'NONE',  ( -3.573159493689508803, 23.91665737286602678, -5.000000000000000000 ) ) ;
#70750 = EDGE_CURVE ( 'NONE', #16756, #93278, #6953, .T. ) ;
#70749 = B_SPLINE_CURVE_WITH_KNOTS ( 'NONE', 3,
 ( #100231, #58730, #26398, #91629 ),
 .UNSPECIFIED., .F., .F.,
 ( 4, 4 ),
 ( 1.886626427905286316E-16, 0.002002602941640114435 ),
 .UNSPECIFIED. ) ;
#70751 = CARTESIAN_POINT ( 'NONE',  ( 3.249999999999998668, 5.629165124598852543, -5.592027715088707218 ) ) ;
#70752 = CIRCLE ( 'NONE', #105243, 1.000000000000000888 ) ;
#70753 = ORIENTED_EDGE ( 'NONE', *, *, #93557, .F. ) ;
#70754 = DIRECTION ( 'NONE',  ( 0.000000000000000000, 1.000000000000000000, 0.000000000000000000 ) ) ;
#70755 = CIRCLE ( 'NONE', #100008, 5.000000000000000000 ) ;
#70756 = DIRECTION ( 'NONE',  ( -1.000000000000000000, -1.224606353822377258E-16, -0.000000000000000000 ) ) ;
#70757 = ORIENTED_EDGE ( 'NONE', *, *, #80750, .T. ) ;
#70758 = CARTESIAN_POINT ( 'NONE',  ( 24.63846153846153797, -4.171999999999999709, 0.000000000000000000 ) ) ;
#70759 = CARTESIAN_POINT ( 'NONE',  ( -39.50046859269861699, 39.85910268592828487, -53.63619651269492294 ) ) ;
#70760 = CARTESIAN_POINT ( 'NONE',  ( -17.51195277503164149, 36.87917477456677062, 22.05183216906712929 ) ) ;
#70761 = UNCERTAINTY_MEASURE_WITH_UNIT (LENGTH_MEASURE( 1.000000000000000082E-05 ), #14790, 'distance_accuracy_value', 'NONE');
#70762 = CARTESIAN_POINT ( 'NONE',  ( -102.8445772722775757, -60.00000000000001421, 200.7018563251100716 ) ) ;
#70763 = DIRECTION ( 'NONE',  ( -0.000000000000000000, -0.000000000000000000, -1.000000000000000000 ) ) ;
#70764 = LINE ( 'NONE', #37377, #57009 ) ;
#70765 = CYLINDRICAL_SURFACE ( 'NONE', #49415, 3.400000000000000355 ) ;
#70766 = CARTESIAN_POINT ( 'NONE',  ( 43.18779636046989623, 464.9503604947623217, 14.53715779820238829 ) ) ;
#70767 = CARTESIAN_POINT ( 'NONE',  ( -85.74133566425317099, -25.15092753419028426, 175.6283754751043205 ) ) ;
#70768 = ADVANCED_FACE ( 'NONE', ( #80718 ), #55890, .F. ) ;
#70769 = DIRECTION ( 'NONE',  ( 0.000000000000000000, 0.000000000000000000, 1.000000000000000000 ) ) ;
#70770 =( GEOMETRIC_REPRESENTATION_CONTEXT ( 3 ) GLOBAL_UNCERTAINTY_ASSIGNED_CONTEXT ( ( #36237 ) ) GLOBAL_UNIT_ASSIGNED_CONTEXT ( ( #84288, #69186, #93978 ) ) REPRESENTATION_CONTEXT ( 'NONE', 'WORKASPACE' ) );
#70771 = TOROIDAL_SURFACE ( 'NONE', #39834, 5.400000000000001243, 0.4000000000000000222 ) ;
#70772 = CIRCLE ( 'NONE', #32918, 4.000000000000000888 ) ;
#70773 = EDGE_LOOP ( 'NONE', ( #10607, #77468, #79007, #71439, #37194, #10166 ) ) ;
#70774 = CARTESIAN_POINT ( 'NONE',  ( -0.01393140247697588312, -21.31702117966834109, -38.55283400289633278 ) ) ;
#70775 = CARTESIAN_POINT ( 'NONE',  ( 1.000000000000000000, -64.45248229067139789, 10.00070197187728738 ) ) ;
#70776 = CARTESIAN_POINT ( 'NONE',  ( -85.09173559602810144, -52.70611635879131285, 20.05387495587346791 ) ) ;
#70777 = VECTOR ( 'NONE', #70225, 1000.000000000000000 ) ;
#70778 = CARTESIAN_POINT ( 'NONE',  ( 0.000000000000000000, -15.00000000000000000, 0.000000000000000000 ) ) ;
#70779 = PRESENTATION_STYLE_ASSIGNMENT (( #21725 ) ) ;
#70780 = CARTESIAN_POINT ( 'NONE',  ( 8.361452242971985527, 121.1754334411840830, 0.000000000000000000 ) ) ;
#70781 = DIRECTION ( 'NONE',  ( 0.000000000000000000, 1.000000000000000000, 0.000000000000000000 ) ) ;
#70782 = CARTESIAN_POINT ( 'NONE',  ( -38.36535705883633085, 18.64316884711714195, 5.022013495247505510 ) ) ;
#70783 = CARTESIAN_POINT ( 'NONE',  ( 83.30384756245543088, -14.21045842199437992, 194.5080389997825137 ) ) ;
#70784 = CARTESIAN_POINT ( 'NONE',  ( -55.68167212273443312, 51.11204936430952017, 27.84083606136721656 ) ) ;
#70785 = VECTOR ( 'NONE', #62639, 1000.000000000000000 ) ;
#70786 = CARTESIAN_POINT ( 'NONE',  ( -93.38368407206768040, -29.99999999999995026, 56.44986585522355682 ) ) ;
#70787 = CARTESIAN_POINT ( 'NONE',  ( -63.36831511047880383, -60.34524114802070471, 92.29660992010968812 ) ) ;
#70788 = ORIENTED_EDGE ( 'NONE', *, *, #95989, .T. ) ;
#70789 = CARTESIAN_POINT ( 'NONE',  ( -64.71212909754572706, 39.42531715955912830, 6.807929623798474772 ) ) ;
#70790 = CARTESIAN_POINT ( 'NONE',  ( 83.02744550429022752, -59.99999999998394884, 201.8714438680229080 ) ) ;
#70791 = VERTEX_POINT ( 'NONE', #45714 ) ;
#70792 = DIRECTION ( 'NONE',  ( -0.8191520442889974607, 0.000000000000000000, -0.5735764363510379438 ) ) ;
#70793 = CARTESIAN_POINT ( 'NONE',  ( -2.977408999572654480, -17.00000000204838813, 7.188101187499999156 ) ) ;
#70794 = CARTESIAN_POINT ( 'NONE',  ( 32.86259851300461321, 485.9239370913662697, 5.440925357812796292 ) ) ;
#70795 = VERTEX_POINT ( 'NONE', #103418 ) ;
#70796 = CARTESIAN_POINT ( 'NONE',  ( -5.656854249492381470, -26.75000000409677625, 5.656854249492379694 ) ) ;
#70797 = EDGE_LOOP ( 'NONE', ( #75866, #69277, #41008, #81676 ) ) ;
#70798 = CYLINDRICAL_SURFACE ( 'NONE', #106104, 4.000000000000000000 ) ;
#70799 = CARTESIAN_POINT ( 'NONE',  ( -41.28039629891594586, 485.7122505962499872, -4.568292046899058434 ) ) ;
#70800 = CARTESIAN_POINT ( 'NONE',  ( -92.44597693169667707, -60.00000000000000000, -0.4208892430063501111 ) ) ;
#70801 = CYLINDRICAL_SURFACE ( 'NONE', #81185, 24.55262289886175964 ) ;
#70802 = CARTESIAN_POINT ( 'NONE',  ( 7.188101187500000044, -34.53125000204838813, 0.000000000000000000 ) ) ;
#70803 = CARTESIAN_POINT ( 'NONE',  ( 0.000000000000000000, 0.000000000000000000, -3.024963890361733743 ) ) ;
#70804 = ADVANCED_FACE ( 'NONE', ( #62440 ), #55207, .F. ) ;
#70805 = DIRECTION ( 'NONE',  ( 0.000000000000000000, -1.000000000000000000, 0.000000000000000000 ) ) ;
#70806 = CARTESIAN_POINT ( 'NONE',  ( 5.000000000000000000, -41.55966127977662694, 4.049904920148556187 ) ) ;
#70807 = CARTESIAN_POINT ( 'NONE',  ( 2.617478844989858722, 48.00000000000000000, -94.73972676610448218 ) ) ;
#70808 = EDGE_CURVE ( 'NONE', #26114, #83820, #41863, .T. ) ;
#70809 = CARTESIAN_POINT ( 'NONE',  ( -7.046289519167720172, 106.3059181994437949, -3.789821819998815400 ) ) ;
#70810 = DIRECTION ( 'NONE',  ( 0.000000000000000000, 1.000000000000000000, 0.000000000000000000 ) ) ;
#70811 = CARTESIAN_POINT ( 'NONE',  ( 28.32844991613795926, 306.0388488792111161, -9.289596639994890381 ) ) ;
#70812 = CONICAL_SURFACE ( 'NONE', #15918, 5.000000000000000000, 0.9599310885968913576 ) ;
#70813 = ORIENTED_EDGE ( 'NONE', *, *, #60908, .F. ) ;
#70814 = CARTESIAN_POINT ( 'NONE',  ( 4.852941176470595863, 39.99999999999999289, -70.80672828634229177 ) ) ;
#70815 = CARTESIAN_POINT ( 'NONE',  ( -16.52732684424166010, 43.98685724163156863, -87.77868211029608858 ) ) ;
#70816 = CARTESIAN_POINT ( 'NONE',  ( 33.65780094057635097, -42.96203205001530279, 35.30807191987746307 ) ) ;
#70817 = TOROIDAL_SURFACE ( 'NONE', #161, 12.00000000000001066, 3.000000000000000000 ) ;
#70818 = CARTESIAN_POINT ( 'NONE',  ( 2.227375807148842313, -1.734723475976807094E-15, -17.01589776168603407 ) ) ;
#70819 = ADVANCED_FACE ( 'NONE', ( #74750 ), #60427, .T. ) ;
#70820 = ORIENTED_EDGE ( 'NONE', *, *, #67144, .F. ) ;
#70821 = CARTESIAN_POINT ( 'NONE',  ( 6.289692432696817548, -6.589071317540658335, 2.245373559999283231 ) ) ;
#70822 = VECTOR ( 'NONE', #96854, 1000.000000000000000 ) ;
#70824 = CARTESIAN_POINT ( 'NONE',  ( -8.000000000000000000, 0.000000000000000000, -5.575057142857143155 ) ) ;
#70823 = CARTESIAN_POINT ( 'NONE',  ( -10.00000000000000000, 15.00000000000000000, 10.00000000000000000 ) ) ;
#70825 = FACE_OUTER_BOUND ( 'NONE', #33085, .T. ) ;
#70826 = CARTESIAN_POINT ( 'NONE',  ( 0.000000000000000000, 0.000000000000000000, -9.226681596905679683 ) ) ;
#70827 =( LENGTH_UNIT ( ) NAMED_UNIT ( * ) SI_UNIT ( .MILLI., .METRE. ) );
#70828 = PLANE ( 'NONE',  #96270 ) ;
#70829 = LINE ( 'NONE', #78909, #70707 ) ;
#70830 = CARTESIAN_POINT ( 'NONE',  ( -1.558121094280061403, -49.97010080782105490, 44.88317974245237707 ) ) ;
#70831 = VERTEX_POINT ( 'NONE', #81243 ) ;
#70832 = CARTESIAN_POINT ( 'NONE',  ( 92.00147787190707049, -59.99999999999999289, 6.177437106672091005 ) ) ;
#70833 = DIRECTION ( 'NONE',  ( 0.000000000000000000, -1.000000000000000000, 0.000000000000000000 ) ) ;
#70834 = DIRECTION ( 'NONE',  ( -0.4804656623127168125, 0.6318279369468263740, 0.6082320325598773447 ) ) ;
#70835 = LINE ( 'NONE', #103727, #80127 ) ;
#70836 = CARTESIAN_POINT ( 'NONE',  ( -12.43846442553448917, 9.605310817031497805, -9.412495108624300499 ) ) ;
#70837 = ORIENTED_EDGE ( 'NONE', *, *, #79000, .T. ) ;
#70838 = CIRCLE ( 'NONE', #62244, 3.309500000000001663 ) ;
#70839 = CARTESIAN_POINT ( 'NONE',  ( -75.51516288543771793, -30.00000000000000000, -27.33247042156349593 ) ) ;
#70840 = ORIENTED_EDGE ( 'NONE', *, *, #96554, .F. ) ;
#70841 = CARTESIAN_POINT ( 'NONE',  ( 1.464720647026959308E-15, 47.77514352166374323, 11.96035173608223090 ) ) ;
#70842 =( NAMED_UNIT ( * ) PLANE_ANGLE_UNIT ( ) SI_UNIT ( $, .RADIAN. ) );
#70843 = FACE_OUTER_BOUND ( 'NONE', #27428, .T. ) ;
#70844 = CARTESIAN_POINT ( 'NONE',  ( 14.81450998444705114, 22.88381389413250133, -2.101451306568737909 ) ) ;
#70845 = CARTESIAN_POINT ( 'NONE',  ( 81.92498789339509813, -37.82295742025830521, -13.91723281769504261 ) ) ;
#70846 = CARTESIAN_POINT ( 'NONE',  ( -5.082755093536325042, -30.96875000204838813, -5.082755093536325930 ) ) ;
#70847 = CARTESIAN_POINT ( 'NONE',  ( -18.28710009642425760, 45.00000000000000711, 62.41242308437181663 ) ) ;
#70848 = CARTESIAN_POINT ( 'NONE',  ( 1.163414459189985485E-15, -14.49999999999999822, -9.500000000000000000 ) ) ;
#70849 =( BOUNDED_SURFACE ( )  B_SPLINE_SURFACE ( 2, 3, ( 
 ( #34921, #36000, #60778, #84510, #77481, #42986, #68327, #52654, #43517, #101745, #1433, #1972, #67788, #44047, #101222, #93667, #20364, #68872, #9528, #10599, #27913, #19818, #3592, #36529, #11661, #61303, #44591, #26839, #69394, #75873, #19299, #102277, #85039, #34394 ),
 ( #28425, #59710, #94195, #18743, #53205, #2508, #100675, #27379, #42441, #52123, #67269, #75331, #60259, #18192, #100148, #10076, #26315, #76937, #3050, #92587, #51049, #93125, #83966, #59176, #51591, #76394, #11121, #79591, #29496, #94743, #102818, #22458, #72036, #80114 ),
 ( #22978, #62896, #38627, #45127, #63436, #21920, #55301, #88228, #61846, #12196, #62372, #6218, #13252, #20892, #71491, #104389, #21394, #30539, #13781, #95263, #5700, #95787, #4656, #53726, #54231, #96330, #86655, #12725, #54769, #78004, #28980, #39154, #14309, #46176 ) ),
 .UNSPECIFIED., .F., .T., .F. ) 
 B_SPLINE_SURFACE_WITH_KNOTS ( ( 3, 3 ),
 ( 4, 2, 2, 2, 2, 2, 2, 2, 2, 2, 2, 2, 2, 2, 2, 2, 4 ),
 ( 0.000000000000000000, 1.000000000000000000 ),
 ( -3.141592653589793116, -2.748893571891068976, -2.356194490192344837, -1.963495408493620697, -1.570796326794896558, -1.178097245096172418, -0.7853981633974482790, -0.3926990816987241395, 0.000000000000000000, 0.3926990816987241395, 0.7853981633974482790, 1.178097245096172418, 1.570796326794896558, 1.963495408493620697, 2.356194490192344837, 2.748893571891068976, 3.141592653589793116 ),
 .UNSPECIFIED. ) 
 GEOMETRIC_REPRESENTATION_ITEM ( )  RATIONAL_B_SPLINE_SURFACE ( (
 ( 1.000000000000000000, 1.000000000000000000, 1.000000000000000000, 1.000000000000000000, 1.000000000000000000, 1.000000000000000000, 1.000000000000000000, 1.000000000000000000, 1.000000000000000000, 1.000000000000000000, 1.000000000000000000, 1.000000000000000000, 1.000000000000000000, 1.000000000000000000, 1.000000000000000000, 1.000000000000000000, 1.000000000000000000, 1.000000000000000000, 1.000000000000000000, 1.000000000000000000, 1.000000000000000000, 1.000000000000000000, 1.000000000000000000, 1.000000000000000000, 1.000000000000000000, 1.000000000000000000, 1.000000000000000000, 1.000000000000000000, 1.000000000000000000, 1.000000000000000000, 1.000000000000000000, 1.000000000000000000, 1.000000000000000000, 1.000000000000000000),
 ( 1.857142857142858317, 1.857142857142858317, 1.857142857142858317, 1.857142857142858317, 1.857142857142858317, 1.857142857142858317, 1.857142857142858317, 1.857142857142858317, 1.857142857142858317, 1.857142857142858317, 1.857142857142858317, 1.857142857142858317, 1.857142857142858317, 1.857142857142858317, 1.857142857142858317, 1.857142857142858317, 1.857142857142858317, 1.857142857142858317, 1.857142857142858317, 1.857142857142858317, 1.857142857142858317, 1.857142857142858317, 1.857142857142858317, 1.857142857142858317, 1.857142857142858317, 1.857142857142858317, 1.857142857142858317, 1.857142857142858317, 1.857142857142858317, 1.857142857142858317, 1.857142857142858317, 1.857142857142858317, 1.857142857142858317, 1.857142857142858317),
 ( 1.000000000000000000, 1.000000000000000000, 1.000000000000000000, 1.000000000000000000, 1.000000000000000000, 1.000000000000000000, 1.000000000000000000, 1.000000000000000000, 1.000000000000000000, 1.000000000000000000, 1.000000000000000000, 1.000000000000000000, 1.000000000000000000, 1.000000000000000000, 1.000000000000000000, 1.000000000000000000, 1.000000000000000000, 1.000000000000000000, 1.000000000000000000, 1.000000000000000000, 1.000000000000000000, 1.000000000000000000, 1.000000000000000000, 1.000000000000000000, 1.000000000000000000, 1.000000000000000000, 1.000000000000000000, 1.000000000000000000, 1.000000000000000000, 1.000000000000000000, 1.000000000000000000, 1.000000000000000000, 1.000000000000000000, 1.000000000000000000) ) ) 
 REPRESENTATION_ITEM ( '' )  SURFACE ( )  );
#70850 = DIRECTION ( 'NONE',  ( -0.000000000000000000, 0.5000000000000008882, 0.8660254037844381525 ) ) ;
#70851 = ORIENTED_EDGE ( 'NONE', *, *, #6254, .T. ) ;
#70852 = EDGE_CURVE ( 'NONE', #73133, #27254, #17131, .T. ) ;
#70853 =( BOUNDED_CURVE ( )  B_SPLINE_CURVE ( 2, ( #68342, #18210, #76409, #70857, #51606, #52138, #84526, #37995, #59190 ),
 .UNSPECIFIED., .F., .F. ) 
 B_SPLINE_CURVE_WITH_KNOTS ( ( 3, 2, 2, 2, 3 ),
 ( 0.5441176470588235947, 0.5514705882352942679, 0.5588235294117648300, 0.5661764705882353921, 0.5735294117647059542 ),
 .UNSPECIFIED. ) 
 CURVE ( )  GEOMETRIC_REPRESENTATION_ITEM ( )  RATIONAL_B_SPLINE_CURVE ( ( 0.9999999999999988898, 0.9238795325112878487, 1.000000000000000000, 0.9238795325112867385, 1.000000000000000000, 0.9238795325112867385, 1.000000000000000000, 0.9238795325112856283, 1.000000000000001110 ) ) 
 REPRESENTATION_ITEM ( '' )  );
#70854 = VERTEX_POINT ( 'NONE', #73691 ) ;
#70855 = CARTESIAN_POINT ( 'NONE',  ( 78.02883230765388589, -60.30886709744162744, 156.3352327953801932 ) ) ;
#70856 = EDGE_CURVE ( 'NONE', #81142, #83206, #98496, .T. ) ;
#70857 = CARTESIAN_POINT ( 'NONE',  ( -8.000000000000000000, -20.84374999999998934, -3.313708498984762496 ) ) ;
#70858 = EDGE_LOOP ( 'NONE', ( #27523, #34985, #34662, #28966, #74130 ) ) ;
#70859 = AXIS2_PLACEMENT_3D ( 'NONE', #53743, #11136, #36015 ) ;
#70860 = LINE ( 'NONE', #13129, #27295 ) ;
#70861 = CARTESIAN_POINT ( 'NONE',  ( 7.188101187499999156, -20.75000000204839523, 2.977408999572654924 ) ) ;
#70862 = VECTOR ( 'NONE', #55687, 1000.000000000000000 ) ;
#70863 = CARTESIAN_POINT ( 'NONE',  ( -97.80441453946778552, -57.62343821539597855, 204.4198989768915453 ) ) ;
#70864 = EDGE_CURVE ( 'NONE', #82194, #16556, #16525, .T. ) ;
#70865 = ORIENTED_EDGE ( 'NONE', *, *, #89741, .T. ) ;
#70866 = AXIS2_PLACEMENT_3D ( 'NONE', #99123, #89989, #17180 ) ;
#70868 = CARTESIAN_POINT ( 'NONE',  ( 0.000000000000000000, 50.00000000000000000, -97.00000000000000000 ) ) ;
#70867 = CIRCLE ( 'NONE', #103582, 4.000000000000001776 ) ;
#70869 = CARTESIAN_POINT ( 'NONE',  ( 7.090506028190232790, 41.24768140130692728, -58.61601156502441512 ) ) ;
#70870 = CIRCLE ( 'NONE', #27803, 2.999999999999998668 ) ;
#70871 = CARTESIAN_POINT ( 'NONE',  ( 5.656854249492380582, -14.00000000409677092, -5.656854249492379694 ) ) ;
#70872 = CARTESIAN_POINT ( 'NONE',  ( -4.628935241158544933, -12.82406801309825362, 32.11820816612952711 ) ) ;
#70873 = DIRECTION ( 'NONE',  ( -0.5735764363510494901, -0.8191520442889894671, 0.000000000000000000 ) ) ;
#70874 = CARTESIAN_POINT ( 'NONE',  ( 7.500000000000001776, 13.44157116919690331, -32.95552552993890316 ) ) ;
#70875 = DIRECTION ( 'NONE',  ( -1.000000000000000000, -1.224606353822377258E-16, -0.000000000000000000 ) ) ;
#70876 = CARTESIAN_POINT ( 'NONE',  ( -9.948513602187993854, 33.86977943343858044, 1.045942665286128115 ) ) ;
#70877 = ORIENTED_EDGE ( 'NONE', *, *, #90048, .F. ) ;
#70878 = CARTESIAN_POINT ( 'NONE',  ( 36.08349330513379982, -4.000000000000000000, 4.898587196589415787E-16 ) ) ;
#70879 = CARTESIAN_POINT ( 'NONE',  ( -2.652798497180052895, 14.84807361897902567, -6.480854662599507598 ) ) ;
#70880 = CARTESIAN_POINT ( 'NONE',  ( -58.44719103041130381, -29.04876852297121204, -25.50753101827990577 ) ) ;
#70881 = CARTESIAN_POINT ( 'NONE',  ( -81.05591908368936060, -29.99999999999999645, 140.3178133568220005 ) ) ;
#70882 = EDGE_CURVE ( 'NONE', #86664, #97763, #27729, .T. ) ;
#70883 = CARTESIAN_POINT ( 'NONE',  ( 5.500000000000006217, 42.00000000000000000, -62.89165061482969321 ) ) ;
#70884 = ORIENTED_EDGE ( 'NONE', *, *, #79895, .T. ) ;
#70885 = DIRECTION ( 'NONE',  ( -0.5735764363510494901, -0.8191520442889894671, 0.000000000000000000 ) ) ;
#70886 = CARTESIAN_POINT ( 'NONE',  ( 106.5916955408424371, -57.65224678697860128, 200.4434517509536988 ) ) ;
#70887 = VECTOR ( 'NONE', #82478, 1000.000000000000000 ) ;
#70888 = CARTESIAN_POINT ( 'NONE',  ( 65.15535363651697764, -60.22825919689577034, -28.17460905593080511 ) ) ;
#70889 = CARTESIAN_POINT ( 'NONE',  ( 74.41005759311713064, -38.35600211243141899, -29.42050377152623497 ) ) ;
#70890 = PRESENTATION_LAYER_ASSIGNMENT (  '', '', ( #14053 ) ) ;
#70891 = CARTESIAN_POINT ( 'NONE',  ( -15.74152552778569181, 22.22013712430564780, 3.418714015797057471 ) ) ;
#70892 = B_SPLINE_CURVE_WITH_KNOTS ( 'NONE', 3,
 ( #3759, #94364, #31755, #55457, #98055, #66219, #80804, #15006, #6919, #106674, #105616, #33350, #23671, #49502, #73774, #32822, #41413, #64636, #56520, #89972, #7976, #57579, #16076, #55978, #97507, #88912, #24729, #39840, #14463, #90501, #48434, #47898, #31241, #73230, #22624, #81327 ),
 .UNSPECIFIED., .F., .F.,
 ( 4, 2, 2, 2, 2, 2, 2, 2, 2, 2, 2, 2, 2, 2, 2, 2, 2, 4 ),
 ( 0.2332227355109234568, 0.2353943896690517124, 0.2375660438271799679, 0.2419093521434364791, 0.2462526604596929902, 0.2505959687759495291, 0.2592825854084624404, 0.2679692020409754072, 0.2766558186734883185, 0.2853424353060012852, 0.3027156685710271078, 0.3200889018360528748, 0.3287755184685657861, 0.3374621351010786974, 0.3461487517335915531, 0.3548353683661044644, 0.3635219849986173202, 0.3722086016311302314 ),
 .UNSPECIFIED. ) ;
#70893 = CARTESIAN_POINT ( 'NONE',  ( 1.262844703064978993E-15, -3.000000000000002665, -95.00000000000000000 ) ) ;
#70894 = CARTESIAN_POINT ( 'NONE',  ( -53.50019290532922156, -60.00000000000001421, 81.03251237504147753 ) ) ;
#70895 = ADVANCED_FACE ( 'NONE', ( #99559 ), #1789, .T. ) ;
#70896 = CARTESIAN_POINT ( 'NONE',  ( -2.055025722541619526, 6.319083845364129814, -5.720331885005969674 ) ) ;
#70897 = DIRECTION ( 'NONE',  ( 0.000000000000000000, -1.000000000000000000, 0.000000000000000000 ) ) ;
#70898 = CARTESIAN_POINT ( 'NONE',  ( -51.78317192863611496, 49.99999999999999289, 39.73656039226784742 ) ) ;
#70899 = CARTESIAN_POINT ( 'NONE',  ( -86.13874000985406099, -31.92344543271792645, 184.4244860863919655 ) ) ;
#70900 = VERTEX_POINT ( 'NONE', #74222 ) ;
#70901 = CARTESIAN_POINT ( 'NONE',  ( 35.48039044674744247, 426.6879373334400043, 6.207493775911908429 ) ) ;
#70902 = CARTESIAN_POINT ( 'NONE',  ( -14.91271302809441401, 41.98564543112699710, -86.62215342991694911 ) ) ;
#70903 = CARTESIAN_POINT ( 'NONE',  ( -5.935764392945439560, 41.97455565604287386, -59.37421952392686819 ) ) ;
#70904 = DIRECTION ( 'NONE',  ( 0.000000000000000000, -1.000000000000000000, 0.000000000000000000 ) ) ;
#70905 = CARTESIAN_POINT ( 'NONE',  ( 12.04168909130320841, -4.749806419314886341, -76.84810691751602008 ) ) ;
#70906 =( LENGTH_UNIT ( ) NAMED_UNIT ( * ) SI_UNIT ( .MILLI., .METRE. ) );
#70907 = CARTESIAN_POINT ( 'NONE',  ( 41.86630687591735267, 487.3337178530820211, 9.520545777472943172 ) ) ;
#70908 = LINE ( 'NONE', #36984, #51086 ) ;
#70909 = DIRECTION ( 'NONE',  ( 0.000000000000000000, -1.000000000000000000, 0.000000000000000000 ) ) ;
#70910 = ORIENTED_EDGE ( 'NONE', *, *, #64126, .T. ) ;
#70911 = CARTESIAN_POINT ( 'NONE',  ( 10.07813983907271904, 12.78063534312769178, 10.57220526254674375 ) ) ;
#70912 = CARTESIAN_POINT ( 'NONE',  ( -21.65942590379792776, -9.659702761776270386E-13, -5.820808985972203864 ) ) ;
#70913 = CARTESIAN_POINT ( 'NONE',  ( 102.6464385083043283, 1.030564683017419500E-14, 0.000000000000000000 ) ) ;
#70914 = CARTESIAN_POINT ( 'NONE',  ( 86.49463782384169974, -14.21045842199436215, 11.84774393978288742 ) ) ;
#70915 = CARTESIAN_POINT ( 'NONE',  ( -76.86963417182471403, -56.84750332144378149, 144.4150324011044120 ) ) ;
#70916 = ORIENTED_EDGE ( 'NONE', *, *, #1488, .T. ) ;
#70917 = FACE_OUTER_BOUND ( 'NONE', #94989, .T. ) ;
#70918 = DIRECTION ( 'NONE',  ( 0.5735764363510442720, -0.8191520442889930198, 1.003171929053526349E-16 ) ) ;
#70919 = CARTESIAN_POINT ( 'NONE',  ( 70.80457761868248667, -57.68231074300476990, 160.5472033026200336 ) ) ;
#70920 = CARTESIAN_POINT ( 'NONE',  ( 59.10635875623282232, 49.99999999999999289, -21.83939464513134610 ) ) ;
#70921 = CARTESIAN_POINT ( 'NONE',  ( 36.07326600438810260, 304.1116406225798983, 0.1331827052438417924 ) ) ;
#70922 = CARTESIAN_POINT ( 'NONE',  ( 0.000000000000000000, -15.00000000000000000, 0.000000000000000000 ) ) ;
#70923 = EDGE_LOOP ( 'NONE', ( #76577, #96836, #35164, #61704, #2461 ) ) ;
#70924 = AXIS2_PLACEMENT_3D ( 'NONE', #103005, #13965, #46873 ) ;
#70925 = VECTOR ( 'NONE', #101506, 1000.000000000000000 ) ;
#70926 = CARTESIAN_POINT ( 'NONE',  ( -15.98857071195793367, 36.61411899915854207, 24.05954505250353392 ) ) ;
#70927 = CARTESIAN_POINT ( 'NONE',  ( 5.082755093536325930, -26.46875000204838813, -5.082755093536325042 ) ) ;
#70928 = ORIENTED_EDGE ( 'NONE', *, *, #34496, .T. ) ;
#70929 = FACE_OUTER_BOUND ( 'NONE', #43516, .T. ) ;
#70930 = CIRCLE ( 'NONE', #5483, 5.000000000000000000 ) ;
#70931 = DIRECTION ( 'NONE',  ( -1.000000000000000000, -1.224606353822377258E-16, -0.000000000000000000 ) ) ;
#70932 = FACE_OUTER_BOUND ( 'NONE', #104686, .T. ) ;
#70933 = EDGE_CURVE ( 'NONE', #68266, #2138, #77578, .T. ) ;
#70934 = CARTESIAN_POINT ( 'NONE',  ( 0.1306530452038122403, -7.903938623646872941, -2.309976723937608778 ) ) ;
#70935 = LINE ( 'NONE', #78487, #80060 ) ;
#70936 = CARTESIAN_POINT ( 'NONE',  ( -37.88504238421052861, 463.4171042825119002, 19.90923349044181379 ) ) ;
#70937 = ORIENTED_EDGE ( 'NONE', *, *, #82271, .F. ) ;
#70938 = CARTESIAN_POINT ( 'NONE',  ( -7.036764705886677795, 40.29466777512107001, -71.06385277390548083 ) ) ;
#70939 = AXIS2_PLACEMENT_3D ( 'NONE', #25608, #7772, #50352 ) ;
#70941 = CARTESIAN_POINT ( 'NONE',  ( 28.03697802430866659, -56.86230969446410910, 35.51620881315012923 ) ) ;
#70940 = CARTESIAN_POINT ( 'NONE',  ( -64.23299091672136285, -59.99999999999999289, 125.0187485388276656 ) ) ;
#70942 = CARTESIAN_POINT ( 'NONE',  ( 23.97799606807651429, 27.87796489320410132, -30.95132209396242473 ) ) ;
#70943 = ADVANCED_FACE ( 'NONE', ( #7359 ), #40271, .F. ) ;
#70944 = ORIENTED_EDGE ( 'NONE', *, *, #98738, .T. ) ;
#70945 = VECTOR ( 'NONE', #70477, 1000.000000000000227 ) ;
#70946 = UNCERTAINTY_MEASURE_WITH_UNIT (LENGTH_MEASURE( 1.000000000000000082E-05 ), #38052, 'distance_accuracy_value', 'NONE');
#70947 = VERTEX_POINT ( 'NONE', #77433 ) ;
#70948 = CARTESIAN_POINT ( 'NONE',  ( -4.919733272805022928, -48.43781863848563773, 104.2477112191710802 ) ) ;
#70949 = CARTESIAN_POINT ( 'NONE',  ( -43.72375837489616401, 464.7599263999740060, 7.850687543227762077 ) ) ;
#70950 = CARTESIAN_POINT ( 'NONE',  ( -33.77559172535808329, 464.7834715296605737, 7.192701217093241617 ) ) ;
#70951 = CARTESIAN_POINT ( 'NONE',  ( 14.91858118607497374, 2.271260765197548532E-16, 15.00000000000000000 ) ) ;
#70952 = CARTESIAN_POINT ( 'NONE',  ( -7.500000000000000000, 4.330127018922188320, -0.9999999999999904521 ) ) ;
#70953 = ORIENTED_EDGE ( 'NONE', *, *, #47468, .T. ) ;
#70954 = CARTESIAN_POINT ( 'NONE',  ( 20.00000000000000000, 12.99999999999999289, 0.000000000000000000 ) ) ;
#70955 = CARTESIAN_POINT ( 'NONE',  ( 61.04765681913714559, -30.00000000000000000, 69.49378535683561608 ) ) ;
#70956 = CARTESIAN_POINT ( 'NONE',  ( -10.03922187546495515, 13.76626433127010962, -10.52687670776041884 ) ) ;
#70957 = CARTESIAN_POINT ( 'NONE',  ( 81.10659294315915702, -29.99999999999999645, 2.312534082856741779 ) ) ;
#70958 = CARTESIAN_POINT ( 'NONE',  ( 6.500000000000000000, -3.155218591052682875, -0.5622968210053850280 ) ) ;
#70959 = EDGE_LOOP ( 'NONE', ( #65941, #25230, #90876, #72833, #80304, #77939 ) ) ;
#70960 = EDGE_CURVE ( 'NONE', #75683, #45384, #44001, .T. ) ;
#70961 = CIRCLE ( 'NONE', #38268, 2.999999999999974687 ) ;
#70962 = ORIENTED_EDGE ( 'NONE', *, *, #28690, .F. ) ;
#70963 = VERTEX_POINT ( 'NONE', #67746 ) ;
#70964 = DIRECTION ( 'NONE',  ( -0.5735764363510512664, 0.8191520442889881348, 1.003171929053520309E-16 ) ) ;
#70965 = PRESENTATION_STYLE_ASSIGNMENT (( #62364 ) ) ;
#70966 = CARTESIAN_POINT ( 'NONE',  ( 6.683837171061802529, 3.955946848495962787, 6.851900933636986935 ) ) ;
#70967 = VECTOR ( 'NONE', #65763, 1000.000000000000000 ) ;
#70968 = CARTESIAN_POINT ( 'NONE',  ( 34.12349128637390550, 490.8027302422246407, 11.84948222508928062 ) ) ;
#70969 = DIRECTION ( 'NONE',  ( -1.000000000000000000, -0.000000000000000000, -0.000000000000000000 ) ) ;
#70970 = CARTESIAN_POINT ( 'NONE',  ( 0.000000000000000000, 0.000000000000000000, -11.82492182392400437 ) ) ;
#70971 = ORIENTED_EDGE ( 'NONE', *, *, #56964, .F. ) ;
#70972 = CARTESIAN_POINT ( 'NONE',  ( 29.68315524077034340, 8.302504244945382084, 42.10535821593451544 ) ) ;
#70973 = AXIS2_PLACEMENT_3D ( 'NONE', #5103, #38545, #95184 ) ;
#70974 = VERTEX_POINT ( 'NONE', #101175 ) ;
#70975 = ADVANCED_FACE ( 'NONE', ( #42938 ), #102769, .T. ) ;
#70976 = CARTESIAN_POINT ( 'NONE',  ( 0.000000000000000000, 0.000000000000000000, -4.987924522925830217 ) ) ;
#70977 = PRESENTATION_STYLE_ASSIGNMENT (( #5189 ) ) ;
#70978 = CARTESIAN_POINT ( 'NONE',  ( 7.000000000000000000, 0.000000000000000000, -0.7256075382097185722 ) ) ;
#70979 = CARTESIAN_POINT ( 'NONE',  ( 21.08349330513380337, 1.593028355512270567E-15, 0.000000000000000000 ) ) ;
#70980 = CARTESIAN_POINT ( 'NONE',  ( 61.92817443706537972, -56.86333258057452156, 86.14193829594731255 ) ) ;
#70981 = ORIENTED_EDGE ( 'NONE', *, *, #89847, .T. ) ;
#70982 = CARTESIAN_POINT ( 'NONE',  ( 41.59783515517239039, 465.5823253716133081, 15.80626774175417104 ) ) ;
#70983 = CYLINDRICAL_SURFACE ( 'NONE', #88909, 4.250000000000000000 ) ;
#70984 = CARTESIAN_POINT ( 'NONE',  ( -6.924577185163238724, 9.133260498430180618, -1.057577261889347309 ) ) ;
#70985 =( BOUNDED_SURFACE ( )  B_SPLINE_SURFACE ( 3, 2, ( 
 ( #1205, #44362, #34709 ),
 ( #50832, #83736, #75108 ),
 ( #92363, #59494, #60042 ),
 ( #84287, #42761, #19067 ),
 ( #68657, #101536, #36316 ),
 ( #92900, #75651, #102056 ),
 ( #68096, #28217, #1753 ),
 ( #27689, #93455, #100462 ),
 ( #19603, #18512, #10381 ),
 ( #60567, #77260, #3373 ),
 ( #43298, #27153, #67583 ),
 ( #61087, #17447, #76181 ),
 ( #26622, #83217, #9312 ),
 ( #42222, #34173, #26104 ) ),
 .UNSPECIFIED., .F., .F., .F. ) 
 B_SPLINE_SURFACE_WITH_KNOTS ( ( 4, 2, 2, 2, 2, 2, 4 ),
 ( 3, 3 ),
 ( 6.166074595359560817E-15, 0.003029187982864252251, 0.004543781974293295556, 0.006058375965722338427, 0.007572969957151381298, 0.009087563948580424170, 0.01211675193143850991 ),
 ( 0.000000000000000000, 1.000000000000000000 ),
 .UNSPECIFIED. ) 
 GEOMETRIC_REPRESENTATION_ITEM ( )  RATIONAL_B_SPLINE_SURFACE ( (
 ( 1.000000000000000000, 0.8805984182415752537, 1.000000000000000000),
 ( 1.000000000000000000, 0.8693720018072552680, 1.000000000000000000),
 ( 1.000000000000000000, 0.8577088968917530032, 1.000000000000000000),
 ( 1.000000000000000000, 0.8393117846167141849, 1.000000000000000000),
 ( 1.000000000000000000, 0.8329887351665841155, 1.000000000000000000),
 ( 1.000000000000000000, 0.8202097823163787549, 1.000000000000000000),
 ( 1.000000000000000000, 0.8137563009269630498, 1.000000000000000000),
 ( 1.000000000000000000, 0.8006738836228965983, 1.000000000000000000),
 ( 1.000000000000000000, 0.7940450693277653071, 1.000000000000000000),
 ( 1.000000000000000000, 0.7805580043346841412, 1.000000000000000000),
 ( 1.000000000000000000, 0.7736606729360994139, 1.000000000000000000),
 ( 1.000000000000000000, 0.7528757204727521968, 1.000000000000000000),
 ( 1.000000000000000000, 0.7389027884188499318, 1.000000000000000000),
 ( 1.000000000000000000, 0.7246213771201909237, 1.000000000000000000) ) ) 
 REPRESENTATION_ITEM ( '' )  SURFACE ( )  );
#70986 = DIRECTION ( 'NONE',  ( 0.000000000000000000, 0.000000000000000000, 1.000000000000000000 ) ) ;
#70987 = ADVANCED_FACE ( 'NONE', ( #84993 ), #92884, .T. ) ;
#70988 = ORIENTED_EDGE ( 'NONE', *, *, #2312, .F. ) ;
#70989 = B_SPLINE_CURVE_WITH_KNOTS ( 'NONE', 3,
 ( #96573, #86899, #63146, #96043, #46939, #5435, #29742, #70703, #103593, #71219, #94996, #38871, #103074, #71739 ),
 .UNSPECIFIED., .F., .F.,
 ( 4, 2, 2, 2, 2, 2, 4 ),
 ( 0.000000000000000000, 0.002832064884716075162, 0.004248097327074075447, 0.005664129769432076598, 0.007080162211790077750, 0.008496194654148081504, 0.01132825953886409769 ),
 .UNSPECIFIED. ) ;
#70990 = CARTESIAN_POINT ( 'NONE',  ( -32.76922047444635666, 484.1128301720479499, 1.839745883406933569 ) ) ;
#70991 = CARTESIAN_POINT ( 'NONE',  ( 52.47345282232834762, -59.99999999999999289, -31.55443244153824267 ) ) ;
#70992 = FACE_BOUND ( 'NONE', #86752, .T. ) ;
#70993 = CARTESIAN_POINT ( 'NONE',  ( 3.313708498984762052, -30.40625000409677270, -8.000000000000000000 ) ) ;
#70994 = CARTESIAN_POINT ( 'NONE',  ( 86.71742706962844238, -20.66538005307103987, 185.1322602298917843 ) ) ;
#70995 = B_SPLINE_CURVE_WITH_KNOTS ( 'NONE', 3,
 ( #3246, #100863, #50696, #66922, #58833, #76582, #52313, #44241, #2155, #77129, #1621, #91728, #17846, #35108, #67455, #100332, #67975, #26497, #78703, #20557, #3781, #12904, #45831, #79246, #54956, #71153, #30185, #53392 ),
 .UNSPECIFIED., .F., .F.,
 ( 4, 2, 2, 2, 2, 2, 2, 2, 2, 2, 2, 2, 2, 4 ),
 ( 0.007813944516173556773, 0.008738276158831416451, 0.009662607801489277864, 0.01058693944414713928, 0.01151127108680499896, 0.01243560272946285863, 0.01289776855079178761, 0.01335993437212071658, 0.01382210019344964208, 0.01405318310411410830, 0.01428426601477857452, 0.01451534892544303901, 0.01474643183610750523, 0.01520859765743644634 ),
 .UNSPECIFIED. ) ;
#70996 = CARTESIAN_POINT ( 'NONE',  ( -5.235346568409651624, 8.628330344405153340, -28.94746872473582400 ) ) ;
#70997 = CARTESIAN_POINT ( 'NONE',  ( -5.894985479084318136, 4.645370767574111603, 5.000000000000000000 ) ) ;
#70998 = AXIS2_PLACEMENT_3D ( 'NONE', #67424, #92745, #98695 ) ;
#70999 = SURFACE_SIDE_STYLE ('',( #88317 ) ) ;
#71000 = CARTESIAN_POINT ( 'NONE',  ( 2.153051538919528525E-10, 304.8518027762758607, 9.936999415352289589 ) ) ;
#71001 = VERTEX_POINT ( 'NONE', #11076 ) ;
#71002 = CARTESIAN_POINT ( 'NONE',  ( 6.162888688655344005, 3.752776749732565253, 6.499999999999997335 ) ) ;
#71003 = CARTESIAN_POINT ( 'NONE',  ( 5.000000000000000000, -14.43154361897128091, 12.18621392300911133 ) ) ;
#71004 = CIRCLE ( 'NONE', #83015, 61.00000000000000000 ) ;
#71005 = CARTESIAN_POINT ( 'NONE',  ( -99.82224909337540453, -29.99999999999999645, 186.3256874041514948 ) ) ;
#71006 = EDGE_CURVE ( 'NONE', #88800, #51129, #89504, .T. ) ;
#71007 = COLOUR_RGB ( '', 0.09019608, 0.27058824, 0.51372549) ;
#71008 = CARTESIAN_POINT ( 'NONE',  ( 28.11522601640037777, -57.67959711521903898, 44.33298562067892590 ) ) ;
#71010 = DIRECTION ( 'NONE',  ( 1.000000000000000000, 1.224606353822377258E-16, 0.000000000000000000 ) ) ;
#71009 = CARTESIAN_POINT ( 'NONE',  ( 9.274304459112276078, 44.06289711030127165, 13.41925210190729345 ) ) ;
#71011 = EDGE_CURVE ( 'NONE', #2234, #57214, #96372, .T. ) ;
#71012 = CIRCLE ( 'NONE', #5572, 5.000000000000002665 ) ;
#71013 = CARTESIAN_POINT ( 'NONE',  ( -38.83522905902818678, 469.0596193260172981, 0.4591931294767716554 ) ) ;
#71014 = CARTESIAN_POINT ( 'NONE',  ( -19.02605628674608340, 50.00000000000000000, 60.55087752146327773 ) ) ;
#71015 = FACE_OUTER_BOUND ( 'NONE', #74948, .T. ) ;
#71016 = FILL_AREA_STYLE_COLOUR ( '', #87315 ) ;
#71017 = CARTESIAN_POINT ( 'NONE',  ( 0.9578037757747321912, -15.40093288537109295, -35.22475077049247005 ) ) ;
#71018 = LINE ( 'NONE', #5233, #51055 ) ;
#71019 = EDGE_CURVE ( 'NONE', #86174, #56691, #5140, .T. ) ;
#71020 = ORIENTED_EDGE ( 'NONE', *, *, #31116, .T. ) ;
#71021 = CARTESIAN_POINT ( 'NONE',  ( 39.78276460673486525, 485.2153259665875566, -4.379159006359480522 ) ) ;
#71022 = DIRECTION ( 'NONE',  ( 0.000000000000000000, 1.000000000000000000, 0.000000000000000000 ) ) ;
#71023 = CARTESIAN_POINT ( 'NONE',  ( -15.60285226952893822, -35.99487615058492906, 30.06479306797814743 ) ) ;
#71025 = CARTESIAN_POINT ( 'NONE',  ( 73.33904886068935980, -4.000000000000000888, 4.898587196589422689E-16 ) ) ;
#71024 = CARTESIAN_POINT ( 'NONE',  ( -102.0018013446515681, -60.00000000000001421, 127.8252749486858448 ) ) ;
#71026 = ORIENTED_EDGE ( 'NONE', *, *, #83369, .F. ) ;
#71027 = CARTESIAN_POINT ( 'NONE',  ( -43.55333112596419909, 465.2342844084849389, 9.238213423004411951 ) ) ;
#71028 = COLOUR_RGB ( '', 0.40784314, 0.44705882, 0.49803922) ;
#71029 = CARTESIAN_POINT ( 'NONE',  ( 16.10173312979610216, 5.477053992169538255, -4.739458514411119872 ) ) ;
#71030 = DIRECTION ( 'NONE',  ( -0.000000000000000000, 0.000000000000000000, -1.000000000000000000 ) ) ;
#71031 = CIRCLE ( 'NONE', #55532, 4.000000000000001776 ) ;
#71032 = CARTESIAN_POINT ( 'NONE',  ( 16.02187926457672873, 4.033883445130388878, -2.088897399353103257 ) ) ;
#71033 = CARTESIAN_POINT ( 'NONE',  ( 66.39989526219071081, -59.99999999999998579, 124.0569035276217136 ) ) ;
#71034 = CARTESIAN_POINT ( 'NONE',  ( -43.74855578046756222, 328.6220886837048170, -1.765109843966993441 ) ) ;
#71035 = ORIENTED_EDGE ( 'NONE', *, *, #25067, .T. ) ;
#71036 = CARTESIAN_POINT ( 'NONE',  ( 32.09911992168216699, 438.9232547152092252, 23.66653216045978780 ) ) ;
#71037 = CARTESIAN_POINT ( 'NONE',  ( -33.97359119245066239, 434.1099241184709285, 11.80501937577158778 ) ) ;
#71038 = CONICAL_SURFACE ( 'NONE', #79658, 8.000000000000000000, 0.9599310885968911355 ) ;
#71040 = CARTESIAN_POINT ( 'NONE',  ( 6.764423792815447811, 41.48989066009205118, -70.49176070406230110 ) ) ;
#71039 = CARTESIAN_POINT ( 'NONE',  ( 41.09910603910869042, -35.58342714853350230, 38.74414947838628365 ) ) ;
#71041 = CARTESIAN_POINT ( 'NONE',  ( 6.936184427528457874, 1.053834543709838281E-15, 8.605212085995399107 ) ) ;
#71042 = CARTESIAN_POINT ( 'NONE',  ( -5.688569873206696492, -2.951204850235074062, 103.9352763293502733 ) ) ;
#71043 = ORIENTED_EDGE ( 'NONE', *, *, #55616, .F. ) ;
#71044 = ORIENTED_EDGE ( 'NONE', *, *, #14502, .T. ) ;
#71045 = CARTESIAN_POINT ( 'NONE',  ( -29.42120653936339281, 324.0310542480657432, 13.66637059004188792 ) ) ;
#71046 = VERTEX_POINT ( 'NONE', #21352 ) ;
#71047 = CARTESIAN_POINT ( 'NONE',  ( 20.39043067447545710, 304.8923525889808843, 9.945639527452529549 ) ) ;
#71048 = FACE_OUTER_BOUND ( 'NONE', #48911, .T. ) ;
#71049 = CARTESIAN_POINT ( 'NONE',  ( 4.898587196589412829E-16, -12.31250000409676915, -8.000000000000000000 ) ) ;
#71050 = ORIENTED_EDGE ( 'NONE', *, *, #81040, .T. ) ;
#71051 = EDGE_CURVE ( 'NONE', #72025, #80543, #69040, .T. ) ;
#71052 = SURFACE_SIDE_STYLE ('',( #37670 ) ) ;
#71053 = CARTESIAN_POINT ( 'NONE',  ( -6.629186135610700248, 41.56975587227380942, -70.49374930908771830 ) ) ;
#71054 = CARTESIAN_POINT ( 'NONE',  ( -101.4188503834094774, -59.99999999999139533, 203.9653219413819727 ) ) ;
#71055 = CARTESIAN_POINT ( 'NONE',  ( 6.692429545713704186, 4.002214399422197033, -6.852332219948825021 ) ) ;
#71056 = CARTESIAN_POINT ( 'NONE',  ( 84.85800574570012600, -59.99999999999998579, -27.63310012610692823 ) ) ;
#71057 = CARTESIAN_POINT ( 'NONE',  ( 6.523983739925002467, -5.000000000000001776, 15.07216758675048318 ) ) ;
#71058 = CARTESIAN_POINT ( 'NONE',  ( -5.666914945001757964, 41.34312461251444404, -58.37679809223642025 ) ) ;
#71060 = CARTESIAN_POINT ( 'NONE',  ( 11.36735780710606392, -42.95370621829134450, 31.07683940958586888 ) ) ;
#71059 = CARTESIAN_POINT ( 'NONE',  ( -96.14371828217340976, -60.00000000000000711, 39.43406270914149303 ) ) ;
#71062 = ADVANCED_FACE ( 'NONE', ( #70929 ), #22414, .F. ) ;
#71061 = CARTESIAN_POINT ( 'NONE',  ( -30.00000000000000000, 450.0000000000002274, 13.20242257375370976 ) ) ;
#71063 = CARTESIAN_POINT ( 'NONE',  ( -48.40688107547297392, -36.06281915256160886, 47.15551163693150727 ) ) ;
#71064 = CARTESIAN_POINT ( 'NONE',  ( 18.58349330513380693, -4.000000000000000000, 4.898587196589415787E-16 ) ) ;
#71065 = ORIENTED_EDGE ( 'NONE', *, *, #31589, .T. ) ;
#71066 = CARTESIAN_POINT ( 'NONE',  ( 0.1555215442364585587, 13.68570359899996447, -49.25768108662912681 ) ) ;
#71067 = STYLED_ITEM ( 'NONE', ( #27058 ), #53370 ) ;
#71068 = CARTESIAN_POINT ( 'NONE',  ( 17.95946947111420045, 36.59397683629514830, 22.69701383365348590 ) ) ;
#71069 = DIRECTION ( 'NONE',  ( 0.000000000000000000, 0.000000000000000000, 1.000000000000000000 ) ) ;
#71070 = VERTEX_POINT ( 'NONE', #29966 ) ;
#71071 = SURFACE_STYLE_FILL_AREA ( #37691 ) ;
#71072 = EDGE_LOOP ( 'NONE', ( #75664, #55092, #88453, #97895 ) ) ;
#71073 = CARTESIAN_POINT ( 'NONE',  ( 82.77223023685738212, -30.00000000002606271, 195.2202738952123582 ) ) ;
#71074 = CARTESIAN_POINT ( 'NONE',  ( 32.62207953394533178, 1.482358050883964840E-15, 0.000000000000000000 ) ) ;
#71075 = CIRCLE ( 'NONE', #79694, 4.000000000000001776 ) ;
#71076 = CARTESIAN_POINT ( 'NONE',  ( 5.469234054728515204, 41.99717949937266326, -59.59612150530382735 ) ) ;
#71077 = CARTESIAN_POINT ( 'NONE',  ( 98.38941629421586299, -30.00000000000000711, 190.0212863901236346 ) ) ;
#71078 = AXIS2_PLACEMENT_3D ( 'NONE', #25284, #59231, #17177 ) ;
#71079 = CARTESIAN_POINT ( 'NONE',  ( -0.1697044463282662841, 36.30024107553216339, 29.74999999999999645 ) ) ;
#71080 = ORIENTED_EDGE ( 'NONE', *, *, #8078, .T. ) ;
#71081 = EDGE_CURVE ( 'NONE', #30721, #18822, #32634, .T. ) ;
#71082 = VERTEX_POINT ( 'NONE', #62855 ) ;
#71083 = VERTEX_POINT ( 'NONE', #21883 ) ;
#71084 = DIRECTION ( 'NONE',  ( -0.000000000000000000, 1.000000000000000000, -0.000000000000000000 ) ) ;
#71085 = CARTESIAN_POINT ( 'NONE',  ( 25.59999999999999787, -3.309499999999999886, 0.000000000000000000 ) ) ;
#71086 = MECHANICAL_DESIGN_GEOMETRIC_PRESENTATION_REPRESENTATION (  '', ( #7314 ), #62546 ) ;
#71087 = DIRECTION ( 'NONE',  ( 0.000000000000000000, 0.000000000000000000, 1.000000000000000000 ) ) ;
#71088 = EDGE_CURVE ( 'NONE', #63343, #4655, #6799, .T. ) ;
#71089 = B_SPLINE_CURVE_WITH_KNOTS ( 'NONE', 3,
 ( #106738, #56588, #445, #80868, #8577, #65229, #6979, #57117, #50101, #81389, #98642, #40417, #24792, #73296, #41479, #90031, #57645, #39896, #16137, #90566, #16676, #91119, #33414, #9101 ),
 .UNSPECIFIED., .F., .F.,
 ( 4, 2, 2, 2, 2, 2, 2, 2, 2, 2, 2, 4 ),
 ( 0.007008940962998030239, 0.007512207565765160328, 0.008015474168532290417, 0.008518740771299420506, 0.008770374072682987285, 0.009022007374066552329, 0.009273640675450119109, 0.009525273976833684153, 0.01002854057960081424, 0.01028017388098438623, 0.01053180718236795821, 0.01103507378513509524 ),
 .UNSPECIFIED. ) ;
#71090 = ORIENTED_EDGE ( 'NONE', *, *, #65205, .T. ) ;
#71091 = CARTESIAN_POINT ( 'NONE',  ( 9.253500431420432548, 106.2977154991770874, 3.792688295761953210 ) ) ;
#71092 = ORIENTED_EDGE ( 'NONE', *, *, #16762, .T. ) ;
#71093 = DIRECTION ( 'NONE',  ( 0.000000000000000000, -0.9591753627731794962, 0.2828119931136929832 ) ) ;
#71094 = CARTESIAN_POINT ( 'NONE',  ( 87.97245158076984239, -38.55863593782331122, 199.9496566671098776 ) ) ;
#71095 = CARTESIAN_POINT ( 'NONE',  ( 12.34269817833570215, 7.431323128372670617, 8.323352676710362275 ) ) ;
#71096 = CARTESIAN_POINT ( 'NONE',  ( 82.43075110611209766, -37.85957831011834429, 10.65854084798032986 ) ) ;
#71097 = CARTESIAN_POINT ( 'NONE',  ( 6.445370176742032164, -7.262437273739264398, 1.101027156348664215 ) ) ;
#71098 = CARTESIAN_POINT ( 'NONE',  ( 40.87654627980526811, 372.4006569927854571, 25.86602250413524473 ) ) ;
#71099 = CARTESIAN_POINT ( 'NONE',  ( -42.74850648162922084, 465.8913842138921950, 12.61550125122446531 ) ) ;
#71100 = B_SPLINE_CURVE_WITH_KNOTS ( 'NONE', 3,
 ( #50474, #52081, #1382, #92543, #3005, #10556 ),
 .UNSPECIFIED., .F., .F.,
 ( 4, 2, 4 ),
 ( 2.380729204837650980E-07, 0.003943479449179637664, 0.007886720825438791813 ),
 .UNSPECIFIED. ) ;
#71101 = DIRECTION ( 'NONE',  ( 0.000000000000000000, 0.000000000000000000, 1.000000000000000000 ) ) ;
#71102 = CARTESIAN_POINT ( 'NONE',  ( -38.85446894546543462, 460.8903912184119349, 2.218456751109336267 ) ) ;
#71103 = VERTEX_POINT ( 'NONE', #13740 ) ;
#71104 = PRESENTATION_LAYER_ASSIGNMENT (  '', '', ( #31492 ) ) ;
#71105 = PRESENTATION_STYLE_ASSIGNMENT (( #22049 ) ) ;
#71106 = CARTESIAN_POINT ( 'NONE',  ( -36.52792128174517927, 461.3883473947829543, 3.418819814388621925 ) ) ;
#71107 = MECHANICAL_DESIGN_GEOMETRIC_PRESENTATION_REPRESENTATION (  '', ( #10796 ), #19493 ) ;
#71108 = CARTESIAN_POINT ( 'NONE',  ( -4.314913995129422197, 141.0309651098860684, 5.000000000000000000 ) ) ;
#71109 = ORIENTED_EDGE ( 'NONE', *, *, #16114, .F. ) ;
#71110 = DIRECTION ( 'NONE',  ( -0.8191520442889900222, 1.003171929053522528E-16, 0.5735764363510486019 ) ) ;
#71111 = CARTESIAN_POINT ( 'NONE',  ( -32.49055694945669615, 299.9956992945637353, 3.090866007574196939 ) ) ;
#71112 = CARTESIAN_POINT ( 'NONE',  ( -12.32841007366266162, -4.394465204955733562, -76.76276077223093353 ) ) ;
#71113 = CARTESIAN_POINT ( 'NONE',  ( 0.4037800551813686689, -4.058962678540087410, 5.969670414742687115 ) ) ;
#71114 = CARTESIAN_POINT ( 'NONE',  ( 8.000000000000000000, -12.49999999999999289, 0.000000000000000000 ) ) ;
#71115 = VECTOR ( 'NONE', #43250, 1000.000000000000000 ) ;
#71116 = CARTESIAN_POINT ( 'NONE',  ( -35.32368133270053079, -35.72353222546922780, 44.44765049649346622 ) ) ;
#71117 = CARTESIAN_POINT ( 'NONE',  ( 15.17407431220850533, 0.000000000000000000, 5.000000000000002665 ) ) ;
#71118 = EDGE_LOOP ( 'NONE', ( #21274, #31232, #954, #42612, #34374 ) ) ;
#71119 = CARTESIAN_POINT ( 'NONE',  ( 84.07839313513588309, -57.41987416485399365, 190.7915766117616556 ) ) ;
#71120 = CARTESIAN_POINT ( 'NONE',  ( -49.15776748649652461, 8.563726824893079126, 15.04013919214055939 ) ) ;
#71121 = DIRECTION ( 'NONE',  ( 0.000000000000000000, -1.000000000000000000, 0.000000000000000000 ) ) ;
#71122 = ORIENTED_EDGE ( 'NONE', *, *, #18993, .F. ) ;
#71123 = CARTESIAN_POINT ( 'NONE',  ( 95.57197061297391372, -57.67170093465097125, 37.80234372629790585 ) ) ;
#71124 = CARTESIAN_POINT ( 'NONE',  ( 42.61140200160144786, 465.9030374194822457, 13.21253569360410829 ) ) ;
#71125 = CARTESIAN_POINT ( 'NONE',  ( -30.75967547141130609, 7.962001144779934592, 41.50359925574495179 ) ) ;
#71126 = FACE_OUTER_BOUND ( 'NONE', #74676, .T. ) ;
#71127 = EDGE_CURVE ( 'NONE', #33604, #89525, #102803, .T. ) ;
#71128 = ADVANCED_FACE ( 'NONE', ( #30493 ), #80098, .F. ) ;
#71129 = DIRECTION ( 'NONE',  ( 0.000000000000000000, 0.000000000000000000, -1.000000000000000000 ) ) ;
#71130 = CARTESIAN_POINT ( 'NONE',  ( 0.9999999999999941158, -1.734723475976807094E-15, 101.0455488498966758 ) ) ;
#71131 = CARTESIAN_POINT ( 'NONE',  ( 49.51030389795987219, -29.59163284775611302, 45.84054346467660679 ) ) ;
#71133 = PLANE ( 'NONE',  #20700 ) ;
#71132 = DIRECTION ( 'NONE',  ( 0.000000000000000000, 0.000000000000000000, -1.000000000000000000 ) ) ;
#71134 = EDGE_CURVE ( 'NONE', #74736, #21068, #81131, .T. ) ;
#71135 = CARTESIAN_POINT ( 'NONE',  ( 43.31290673312265227, 487.3457497296887482, 8.045183856868069583 ) ) ;
#71136 = DIRECTION ( 'NONE',  ( -0.000000000000000000, -1.000000000000000000, -0.000000000000000000 ) ) ;
#71137 = CARTESIAN_POINT ( 'NONE',  ( 43.59756234217316972, 434.3244621007173123, 14.55946156040339368 ) ) ;
#71138 = DIRECTION ( 'NONE',  ( 0.000000000000000000, 1.000000000000000000, 0.000000000000000000 ) ) ;
#71139 = CIRCLE ( 'NONE', #60784, 4.000000000000000888 ) ;
#71140 = CARTESIAN_POINT ( 'NONE',  ( -82.71960126402635183, -38.00000000000000711, 3.558503230223199143 ) ) ;
#71141 = AXIS2_PLACEMENT_3D ( 'NONE', #94646, #76300, #78425 ) ;
#71142 = EDGE_CURVE ( 'NONE', #73863, #14310, #44711, .T. ) ;
#71143 = EDGE_LOOP ( 'NONE', ( #81421, #99118, #39465, #32092 ) ) ;
#71144 = CARTESIAN_POINT ( 'NONE',  ( -11.22550744430827407, -1.339777127611723628, 20.46120208494560089 ) ) ;
#71145 = CARTESIAN_POINT ( 'NONE',  ( 0.000000000000000000, 0.000000000000000000, 4.000000000000000888 ) ) ;
#71146 = VECTOR ( 'NONE', #98469, 1000.000000000000000 ) ;
#71147 = CYLINDRICAL_SURFACE ( 'NONE', #56172, 5.000000000000002665 ) ;
#71149 = CARTESIAN_POINT ( 'NONE',  ( -1.605081721621855584, -60.22810981620649784, -36.92765560991468732 ) ) ;
#71148 = FACE_OUTER_BOUND ( 'NONE', #32412, .T. ) ;
#71150 = ORIENTED_EDGE ( 'NONE', *, *, #74158, .F. ) ;
#71151 = CARTESIAN_POINT ( 'NONE',  ( 6.484173630541964606, 4.916614646777613729, -7.642786413608825491 ) ) ;
#71152 = EDGE_LOOP ( 'NONE', ( #68503, #93775, #62735, #99625 ) ) ;
#71153 = CARTESIAN_POINT ( 'NONE',  ( 29.87373162892120249, 8.058069557479617728, -42.09632259471328553 ) ) ;
#71154 = DIRECTION ( 'NONE',  ( 0.000000000000000000, -1.000000000000000000, 0.000000000000000000 ) ) ;
#71155 = CARTESIAN_POINT ( 'NONE',  ( -92.56479762031210612, -60.00000000000000711, -2.220767633544127762 ) ) ;
#71156 = ORIENTED_EDGE ( 'NONE', *, *, #47428, .F. ) ;
#71157 = CARTESIAN_POINT ( 'NONE',  ( 23.58349330513380337, 4.898587196589411843E-16, -4.000000000000001776 ) ) ;
#71158 = DIRECTION ( 'NONE',  ( -0.000000000000000000, -1.000000000000000000, -0.000000000000000000 ) ) ;
#71159 = CARTESIAN_POINT ( 'NONE',  ( -9.989113211954165905, 26.02700726451005764, 0.5334031035449032787 ) ) ;
#71161 = FACE_OUTER_BOUND ( 'NONE', #73635, .T. ) ;
#71160 = CARTESIAN_POINT ( 'NONE',  ( 4.898587196589412829E-16, -27.12499999999999645, -8.000000000000000000 ) ) ;
#71162 = CARTESIAN_POINT ( 'NONE',  ( -81.41430060195118301, -49.93828882406421599, 171.6694044221305830 ) ) ;
#71163 = VERTEX_POINT ( 'NONE', #25056 ) ;
#71164 = CARTESIAN_POINT ( 'NONE',  ( -16.46930219882042934, 0.000000000000000000, -4.418206560268989058 ) ) ;
#71165 = VECTOR ( 'NONE', #39823, 1000.000000000000341 ) ;
#71166 = ORIENTED_EDGE ( 'NONE', *, *, #47551, .F. ) ;
#71167 = ORIENTED_EDGE ( 'NONE', *, *, #76380, .F. ) ;
#71168 = CARTESIAN_POINT ( 'NONE',  ( 41.72774289521763791, 484.6318496107524538, -3.104024719554764555 ) ) ;
#71169 = VECTOR ( 'NONE', #83473, 1000.000000000000000 ) ;
#71170 = FILL_AREA_STYLE ('',( #96525 ) ) ;
#71171 = VERTEX_POINT ( 'NONE', #105933 ) ;
#71172 = ADVANCED_FACE ( 'NONE', ( #73561 ), #17486, .F. ) ;
#71173 = CARTESIAN_POINT ( 'NONE',  ( 15.66258511614954507, 45.99742480776468057, -6.198981311147548467 ) ) ;
#71174 = DIRECTION ( 'NONE',  ( -1.000000000000000000, -0.000000000000000000, -0.000000000000000000 ) ) ;
#71175 = CARTESIAN_POINT ( 'NONE',  ( -100.1205506810183152, -57.62746089781320791, 203.8952656938035091 ) ) ;
#71176 = CARTESIAN_POINT ( 'NONE',  ( -44.08840282922865583, 485.7747746244177165, 4.178803824087112595 ) ) ;
#71177 = CARTESIAN_POINT ( 'NONE',  ( -3.220999722221654600E-16, 7.895640089090876224, -6.564402953523721607 ) ) ;
#71178 = VECTOR ( 'NONE', #2105, 1000.000000000000000 ) ;
#71179 = CYLINDRICAL_SURFACE ( 'NONE', #64900, 1.250000000000001110 ) ;
#71180 = CARTESIAN_POINT ( 'NONE',  ( 87.61417445234833679, -14.21045842199449716, -10.69449287335903342 ) ) ;
#71181 = ADVANCED_FACE ( 'NONE', ( #99426 ), #47010, .F. ) ;
#71183 = EDGE_CURVE ( 'NONE', #80260, #22089, #48226, .T. ) ;
#71182 = CARTESIAN_POINT ( 'NONE',  ( -70.38749560794603610, -14.21045842199435860, 117.5518806561683078 ) ) ;
#71184 = CARTESIAN_POINT ( 'NONE',  ( -55.26730358396395815, -39.50059391399134512, 60.87172762752346955 ) ) ;
#71185 = ORIENTED_EDGE ( 'NONE', *, *, #102503, .T. ) ;
#71186 = DIRECTION ( 'NONE',  ( 0.000000000000000000, 1.000000000000000000, 1.224646799147353207E-16 ) ) ;
#71187 = ORIENTED_EDGE ( 'NONE', *, *, #8549, .F. ) ;
#71188 = CARTESIAN_POINT ( 'NONE',  ( -101.0485842489931940, -52.73349511294460967, 193.3212840139921127 ) ) ;
#71189 = CARTESIAN_POINT ( 'NONE',  ( -29.68315524077005207, 18.29184282782459547, -39.60535821593474282 ) ) ;
#71190 = EDGE_LOOP ( 'NONE', ( #45771, #43855, #95353, #82024, #78324 ) ) ;
#71191 = CARTESIAN_POINT ( 'NONE',  ( 19.45753456193933673, 49.98217452750294143, 60.55466515883400547 ) ) ;
#71192 = FACE_OUTER_BOUND ( 'NONE', #86654, .T. ) ;
#71193 = SURFACE_STYLE_FILL_AREA ( #55516 ) ;
#71194 = DIRECTION ( 'NONE',  ( 0.000000000000000000, -1.000000000000000000, 0.000000000000000000 ) ) ;
#71195 = CARTESIAN_POINT ( 'NONE',  ( 47.33349330513379982, 1.593028355512270567E-15, 0.000000000000000000 ) ) ;
#71196 = CARTESIAN_POINT ( 'NONE',  ( 0.000000000000000000, 1.089935651241144357E-15, 8.900000000000000355 ) ) ;
#71197 = CARTESIAN_POINT ( 'NONE',  ( 66.18720266095957072, -30.00000000000000000, 83.66546625751099953 ) ) ;
#71198 = EDGE_CURVE ( 'NONE', #19129, #44923, #67103, .T. ) ;
#71199 = CARTESIAN_POINT ( 'NONE',  ( -8.209867939952777860, 114.8553993246446652, 1.301042606982606307E-15 ) ) ;
#71200 = CARTESIAN_POINT ( 'NONE',  ( 4.284822031654949015, -48.90716638558772900, 104.4267991316944943 ) ) ;
#71201 = CARTESIAN_POINT ( 'NONE',  ( 7.999999999999998224, -24.59374999999999289, 3.313708498984766049 ) ) ;
#71202 = EDGE_CURVE ( 'NONE', #10651, #104924, #33676, .T. ) ;
#71203 = CARTESIAN_POINT ( 'NONE',  ( -27.89559576334529467, -53.39171285254504795, 34.87437243777274176 ) ) ;
#71204 = ORIENTED_EDGE ( 'NONE', *, *, #92479, .T. ) ;
#71205 = ORIENTED_EDGE ( 'NONE', *, *, #71088, .F. ) ;
#71206 = CARTESIAN_POINT ( 'NONE',  ( 47.77420556706847066, -22.22698538295941262, 42.11322263999190341 ) ) ;
#71207 = CARTESIAN_POINT ( 'NONE',  ( -0.9601284218943312299, 8.766929892175371108, 51.31273321731734427 ) ) ;
#71208 = CARTESIAN_POINT ( 'NONE',  ( -5.744562646538029504, 13.27032591418342378, -4.000000000000000000 ) ) ;
#71209 = ADVANCED_FACE ( 'NONE', ( #91372 ), #27740, .F. ) ;
#71210 = CARTESIAN_POINT ( 'NONE',  ( -110.8389214075725988, -38.35618062369555759, 166.4464234148499031 ) ) ;
#71211 = ORIENTED_EDGE ( 'NONE', *, *, #33574, .F. ) ;
#71212 = CARTESIAN_POINT ( 'NONE',  ( 91.34032523538760984, -38.39886032400823268, -9.955676214931663992 ) ) ;
#71213 = CARTESIAN_POINT ( 'NONE',  ( 14.22499876634535809, 6.546626909046912246, -7.657221783520114400 ) ) ;
#71214 = DIRECTION ( 'NONE',  ( 0.000000000000000000, -1.000000000000000000, 0.000000000000000000 ) ) ;
#71215 = CARTESIAN_POINT ( 'NONE',  ( -2.100000000000004530, 0.000000000000000000, 8.500000000000000000 ) ) ;
#71216 = CARTESIAN_POINT ( 'NONE',  ( 0.000000000000000000, 195.0000000000000000, 0.000000000000000000 ) ) ;
#71217 = CARTESIAN_POINT ( 'NONE',  ( 5.385673916453011856, 3.157894736842104866, 14.66382285868950675 ) ) ;
#71218 = CARTESIAN_POINT ( 'NONE',  ( 23.05203244996646106, 28.15092755562140425, 30.71439907890176357 ) ) ;
#71219 = CARTESIAN_POINT ( 'NONE',  ( -32.30721550124390973, 435.2323396810500071, 15.38116828642125533 ) ) ;
#71220 = EDGE_CURVE ( 'NONE', #52615, #37041, #77304, .T. ) ;
#71221 = CARTESIAN_POINT ( 'NONE',  ( 92.68958050770518753, -60.00000000000001421, 202.4387916161230692 ) ) ;
#71222 = AXIS2_PLACEMENT_3D ( 'NONE', #29168, #11312, #101933 ) ;
#71223 = CIRCLE ( 'NONE', #5775, 0.9999999999999902300 ) ;
#71224 = CARTESIAN_POINT ( 'NONE',  ( 18.61015277268172952, 45.00000000000002842, 62.28407730500863693 ) ) ;
#71225 = ORIENTED_EDGE ( 'NONE', *, *, #54336, .F. ) ;
#71226 = CARTESIAN_POINT ( 'NONE',  ( 58.23846566418407633, -53.38279051962974364, 74.09562710507131555 ) ) ;
#71227 = CARTESIAN_POINT ( 'NONE',  ( -33.13312975063780641, 300.2747487025878286, -0.7832785892000783123 ) ) ;
#71228 = CARTESIAN_POINT ( 'NONE',  ( 0.000000000000000000, 44.84115912518001323, 0.000000000000000000 ) ) ;
#71229 = CARTESIAN_POINT ( 'NONE',  ( -7.801642220026310248, 26.41203173850967900, 1.787233835843583751 ) ) ;
#71230 = ORIENTED_EDGE ( 'NONE', *, *, #15844, .T. ) ;
#71232 = CARTESIAN_POINT ( 'NONE',  ( -14.29190075644363489, 21.26710225492988116, -5.626279437295411689 ) ) ;
#71231 = CARTESIAN_POINT ( 'NONE',  ( -104.2759569493203458, -38.40773243213855892, 198.1659664498641860 ) ) ;
#71233 = CARTESIAN_POINT ( 'NONE',  ( 13.58349330513380160, -7.703719777548943412E-31, 4.000000000000001776 ) ) ;
#71234 = DIRECTION ( 'NONE',  ( 1.000000000000000000, -0.000000000000000000, -0.000000000000000000 ) ) ;
#71235 = VECTOR ( 'NONE', #10995, 1000.000000000000000 ) ;
#71236 = CARTESIAN_POINT ( 'NONE',  ( -2.977408999572650039, -13.06250000204838280, -7.188101187500001821 ) ) ;
#71237 = CARTESIAN_POINT ( 'NONE',  ( 1.308996937480706890, -4.999999999999988454, -95.00000000000001421 ) ) ;
#71238 = CARTESIAN_POINT ( 'NONE',  ( 29.87369781377603317, 13.22774345441024302, -42.09617408282285567 ) ) ;
#71240 = VERTEX_POINT ( 'NONE', #60610 ) ;
#71239 = PRESENTATION_STYLE_ASSIGNMENT (( #36798 ) ) ;
#71241 = CARTESIAN_POINT ( 'NONE',  ( 82.39478451168702122, -46.46901798477522050, 175.1825464717589398 ) ) ;
#71242 = CARTESIAN_POINT ( 'NONE',  ( -44.17170837311727638, 464.2817441679981698, 9.201374799661154569 ) ) ;
#71243 = CARTESIAN_POINT ( 'NONE',  ( -35.03806997136413059, 439.1562646609019680, 24.08350753705479974 ) ) ;
#71244 = ORIENTED_EDGE ( 'NONE', *, *, #9406, .T. ) ;
#71245 = CARTESIAN_POINT ( 'NONE',  ( -35.78063128285121053, 328.0132667276978395, -3.841611872727749954 ) ) ;
#71246 = AXIS2_PLACEMENT_3D ( 'NONE', #8367, #50936, #26202 ) ;
#71247 = CARTESIAN_POINT ( 'NONE',  ( 17.99627583047975676, 34.41216799978017349, 22.85523091777987759 ) ) ;
#71248 = CARTESIAN_POINT ( 'NONE',  ( 26.10623851654674610, 35.05815521469033769, -8.037091760151625408 ) ) ;
#71249 = SURFACE_STYLE_FILL_AREA ( #46972 ) ;
#71250 = AXIS2_PLACEMENT_3D ( 'NONE', #33181, #9935, #92440 ) ;
#71251 = VERTEX_POINT ( 'NONE', #84333 ) ;
#71252 = EDGE_CURVE ( 'NONE', #17049, #28856, #20179, .T. ) ;
#71253 =( GEOMETRIC_REPRESENTATION_CONTEXT ( 3 ) GLOBAL_UNCERTAINTY_ASSIGNED_CONTEXT ( ( #98512 ) ) GLOBAL_UNIT_ASSIGNED_CONTEXT ( ( #44885, #95030, #69678 ) ) REPRESENTATION_CONTEXT ( 'NONE', 'WORKASPACE' ) );
#71254 = SURFACE_STYLE_USAGE ( .BOTH. , #32419 ) ;
#71255 = AXIS2_PLACEMENT_3D ( 'NONE', #25525, #51340, #84253 ) ;
#71256 = CARTESIAN_POINT ( 'NONE',  ( -79.94288123161219062, -30.00000000000000000, -13.90860458798707633 ) ) ;
#71257 = DIRECTION ( 'NONE',  ( -1.000000000000000000, -1.224606353822377258E-16, -0.000000000000000000 ) ) ;
#71258 = LINE ( 'NONE', #102578, #49339 ) ;
#71259 = EDGE_CURVE ( 'NONE', #101681, #14947, #9447, .T. ) ;
#71261 = CARTESIAN_POINT ( 'NONE',  ( -10.06188242486691209, 12.95829428950482232, -10.57356846006649320 ) ) ;
#71260 = CARTESIAN_POINT ( 'NONE',  ( -0.2244703346847722603, -18.03092902646604756, 35.00512146036130900 ) ) ;
#71262 = EDGE_CURVE ( 'NONE', #37867, #25171, #63649, .T. ) ;
#71263 = CARTESIAN_POINT ( 'NONE',  ( -7.188101187500000044, -19.90625000204838457, -8.802885111219163269E-16 ) ) ;
#71264 = CARTESIAN_POINT ( 'NONE',  ( 16.12932323837952708, 294.5641184806675028, -2.061087533654167192 ) ) ;
#71265 = ITEM_DEFINED_TRANSFORMATION ( 'NONE', 'NONE', #93821,  #10728 ) ;
#71266 = ORIENTED_EDGE ( 'NONE', *, *, #75581, .F. ) ;
#71267 = SURFACE_STYLE_FILL_AREA ( #54531 ) ;
#71268 = EDGE_CURVE ( 'NONE', #19223, #74776, #77416, .T. ) ;
#71269 = EDGE_CURVE ( 'NONE', #94312, #79080, #61128, .T. ) ;
#71270 = FACE_OUTER_BOUND ( 'NONE', #95945, .T. ) ;
#71271 = CARTESIAN_POINT ( 'NONE',  ( -4.597609114482794190, 8.581307559369470539, -5.000000000000000000 ) ) ;
#71272 = PRESENTATION_STYLE_ASSIGNMENT (( #6000 ) ) ;
#71273 = FACE_OUTER_BOUND ( 'NONE', #67240, .T. ) ;
#71274 = AXIS2_PLACEMENT_3D ( 'NONE', #69615, #92266, #102509 ) ;
#71275 = ORIENTED_EDGE ( 'NONE', *, *, #86149, .F. ) ;
#71276 = DIRECTION ( 'NONE',  ( -1.000000000000000000, -1.224606353822377258E-16, -0.000000000000000000 ) ) ;
#71277 = CYLINDRICAL_SURFACE ( 'NONE', #77185, 4.000000000000000000 ) ;
#71278 = VERTEX_POINT ( 'NONE', #94019 ) ;
#71279 = CARTESIAN_POINT ( 'NONE',  ( -7.000000000000000000, -15.62228920881133298, 12.61250543006184088 ) ) ;
#71280 = SURFACE_STYLE_USAGE ( .BOTH. , #96630 ) ;
#71281 = CARTESIAN_POINT ( 'NONE',  ( 6.951447288752834019, 41.73217225470716585, -59.36631759480938086 ) ) ;
#71282 = CARTESIAN_POINT ( 'NONE',  ( 86.75754961941542831, 5.000000000000020428, 0.000000000000000000 ) ) ;
#71283 = CARTESIAN_POINT ( 'NONE',  ( -110.1690392527196565, -60.00000000000001421, 144.8104088435783012 ) ) ;
#71284 = CIRCLE ( 'NONE', #23045, 2.000000000000000000 ) ;
#71285 = SURFACE_STYLE_FILL_AREA ( #38422 ) ;
#71286 = FACE_OUTER_BOUND ( 'NONE', #76373, .T. ) ;
#71287 = CARTESIAN_POINT ( 'NONE',  ( 17.53752536966238651, 34.16832498362924753, -24.04387053720026657 ) ) ;
#71288 = B_SPLINE_CURVE_WITH_KNOTS ( 'NONE', 3,
 ( #44585, #35451, #10071, #3587, #60774, #18187, #34918, #2504, #59172, #76933, #85033, #44041, #84506, #1428, #9524, #27908, #42982, #11116, #34389, #3044 ),
 .UNSPECIFIED., .F., .F.,
 ( 4, 2, 2, 2, 2, 2, 2, 2, 2, 4 ),
 ( 6.938893903907228378E-18, 0.001523487669260046272, 0.003046975338520085605, 0.004570463007780124938, 0.005332206842410133762, 0.006093950677040142587, 0.007617438346300116868, 0.009140926015560092016, 0.01066441368482006630, 0.01218790135408004058 ),
 .UNSPECIFIED. ) ;
#71289 = CARTESIAN_POINT ( 'NONE',  ( -85.21113657438505129, -32.24608462764727079, 179.1484755246043505 ) ) ;
#71290 = EDGE_LOOP ( 'NONE', ( #100225, #78265, #39638, #104511 ) ) ;
#71291 = AXIS2_PLACEMENT_3D ( 'NONE', #99138, #25300, #16644 ) ;
#71292 = CARTESIAN_POINT ( 'NONE',  ( 26.76898821255671379, 43.52124955778052140, -73.69872557157349036 ) ) ;
#71293 = CIRCLE ( 'NONE', #79758, 8.331345277524542681 ) ;
#71294 = ORIENTED_EDGE ( 'NONE', *, *, #58322, .F. ) ;
#71295 = DIRECTION ( 'NONE',  ( -0.2043693274459711939, 0.2793933298620141503, 0.9381751143725232112 ) ) ;
#71296 =( BOUNDED_SURFACE ( )  B_SPLINE_SURFACE ( 3, 2, ( 
 ( #79189, #100408, #2227 ),
 ( #38233, #92845, #71097 ),
 ( #84764, #54351, #19008 ),
 ( #10329, #78640, #17919 ),
 ( #4243, #10848, #92306 ),
 ( #95379, #100939, #43765 ) ),
 .UNSPECIFIED., .F., .F., .F. ) 
 B_SPLINE_SURFACE_WITH_KNOTS ( ( 4, 2, 4 ),
 ( 3, 3 ),
 ( 0.003199762745115993304, 0.007302762474435750203, 0.01140576220375550710 ),
 ( 0.000000000000000000, 1.000000000000000000 ),
 .UNSPECIFIED. ) 
 GEOMETRIC_REPRESENTATION_ITEM ( )  RATIONAL_B_SPLINE_SURFACE ( (
 ( 1.000000000000000000, 0.8047731410850428313, 1.000000000000000000),
 ( 1.000000000000000000, 0.8125552299157410285, 1.000000000000000000),
 ( 1.000000000000000000, 0.8191520442888361453, 1.000000000000000000),
 ( 1.000000000000000000, 0.8191520442891434550, 1.000000000000000000),
 ( 1.000000000000000000, 0.8125552299155105462, 1.000000000000000000),
 ( 1.000000000000000000, 0.8047731410850427203, 1.000000000000000000) ) ) 
 REPRESENTATION_ITEM ( '' )  SURFACE ( )  );
#71297 = CARTESIAN_POINT ( 'NONE',  ( 62.33904886068935980, 6.975173280561618775E-15, 0.000000000000000000 ) ) ;
#71298 = CARTESIAN_POINT ( 'NONE',  ( -86.28712359338396709, -52.70879326618576499, 35.16763926569588961 ) ) ;
#71299 = FACE_OUTER_BOUND ( 'NONE', #67143, .T. ) ;
#71300 = SURFACE_STYLE_USAGE ( .BOTH. , #24383 ) ;
#71301 = CARTESIAN_POINT ( 'NONE',  ( 3.836943873308563013, 134.0483964974777393, -4.999999999999999112 ) ) ;
#71302 = DIRECTION ( 'NONE',  ( -1.000000000000000000, -1.224606353822377258E-16, -0.000000000000000000 ) ) ;
#71303 = CARTESIAN_POINT ( 'NONE',  ( 106.4941418293696387, -60.00000000000010658, 201.1229827202191984 ) ) ;
#71304 = EDGE_CURVE ( 'NONE', #70286, #103221, #50472, .T. ) ;
#71305 = CARTESIAN_POINT ( 'NONE',  ( -104.4271118349969498, -14.21045842199436926, 141.4138186051453090 ) ) ;
#71306 = CARTESIAN_POINT ( 'NONE',  ( -65.12520086583974432, -53.39111017842260765, 93.95656328253419076 ) ) ;
#71307 = EDGE_LOOP ( 'NONE', ( #23624, #34593, #93117, #48721, #58991, #60132, #84832 ) ) ;
#71308 = CARTESIAN_POINT ( 'NONE',  ( -63.73076471685384803, 38.95251052932829339, 0.7990814525311284999 ) ) ;
#71309 = CARTESIAN_POINT ( 'NONE',  ( 91.24502176991838098, -60.00000000000494538, 204.7032358451281482 ) ) ;
#71310 = EDGE_LOOP ( 'NONE', ( #17985, #38673, #37813, #92486 ) ) ;
#71311 = CARTESIAN_POINT ( 'NONE',  ( 13.49954484221011519, -55.77516891766431684, 30.71121296612578888 ) ) ;
#71312 = CARTESIAN_POINT ( 'NONE',  ( -2.977408999572654480, -21.50000000204839523, 7.188101187499999156 ) ) ;
#71313 = CARTESIAN_POINT ( 'NONE',  ( 32.20052651336786198, 485.9558351764605391, 4.953748807559890110 ) ) ;
#71314 = ORIENTED_EDGE ( 'NONE', *, *, #4634, .T. ) ;
#71315 = CARTESIAN_POINT ( 'NONE',  ( -30.00000000000000000, 7.347880794884117764E-16, -5.999999999999998224 ) ) ;
#71316 = VERTEX_POINT ( 'NONE', #18557 ) ;
#71317 = CARTESIAN_POINT ( 'NONE',  ( -13.00000000000003730, -10.00000000000000888, 0.000000000000000000 ) ) ;
#71318 = CIRCLE ( 'NONE', #7627, 4.000000000000001776 ) ;
#71319 = CARTESIAN_POINT ( 'NONE',  ( 47.90320435033614643, 17.06740859345636352, -14.35535821593550665 ) ) ;
#71320 = CARTESIAN_POINT ( 'NONE',  ( -91.98242746288742921, -60.00000000000001421, -14.02575605693079375 ) ) ;
#71321 = DIRECTION ( 'NONE',  ( 0.000000000000000000, 1.000000000000000000, 0.000000000000000000 ) ) ;
#71322 = CARTESIAN_POINT ( 'NONE',  ( 4.401442555609581635E-16, -25.15625000204838813, -7.188101187500000044 ) ) ;
#71323 = LINE ( 'NONE', #36881, #20659 ) ;
#71324 = CIRCLE ( 'NONE', #45485, 8.500000000000000000 ) ;
#71325 = DIRECTION ( 'NONE',  ( -1.000000000000000000, -1.224606353822377258E-16, -0.000000000000000000 ) ) ;
#71326 = SURFACE_STYLE_USAGE ( .BOTH. , #62214 ) ;
#71327 = CARTESIAN_POINT ( 'NONE',  ( -6.145467200826166376, 48.00000000000000000, -92.99666842290478996 ) ) ;
#71328 = CARTESIAN_POINT ( 'NONE',  ( -7.896165657598942289, 108.7891113137197152, -1.307894402814546941 ) ) ;
#71329 = LINE ( 'NONE', #38981, #49587 ) ;
#71330 = CARTESIAN_POINT ( 'NONE',  ( 20.96573260866662736, 302.9095451584354919, -9.987686131446045223 ) ) ;
#71331 = AXIS2_PLACEMENT_3D ( 'NONE', #27107, #60522, #75067 ) ;
#71332 = ORIENTED_EDGE ( 'NONE', *, *, #60660, .F. ) ;
#71333 = DIRECTION ( 'NONE',  ( -1.000000000000000000, -0.000000000000000000, 0.000000000000000000 ) ) ;
#71334 = CARTESIAN_POINT ( 'NONE',  ( 33.27692946845811406, -36.02636644479590444, 33.82109768178349896 ) ) ;
#71335 = CARTESIAN_POINT ( 'NONE',  ( -8.569529079657698389, -1.734723475976807094E-15, -14.86825985027703290 ) ) ;
#71336 = VERTEX_POINT ( 'NONE', #76227 ) ;
#71337 = CARTESIAN_POINT ( 'NONE',  ( 34.68490551323709070, 463.9993046474231733, 18.60480341024938511 ) ) ;
#71338 = EDGE_LOOP ( 'NONE', ( #9199, #46844, #66049, #37784 ) ) ;
#71340 = CARTESIAN_POINT ( 'NONE',  ( 45.29905483467455696, 497.0732240353902398, -8.041250874568902418 ) ) ;
#71339 = CARTESIAN_POINT ( 'NONE',  ( 8.716845791011509803, -5.000000000000000000, -16.74192973251932415 ) ) ;
#71341 = CARTESIAN_POINT ( 'NONE',  ( -33.12944332324993013, 439.4248878830265994, 23.85028906779292868 ) ) ;
#71342 = FACE_OUTER_BOUND ( 'NONE', #69490, .T. ) ;
#71344 = ADVANCED_FACE ( 'NONE', ( #13609 ), #55225, .T. ) ;
#71343 = CARTESIAN_POINT ( 'NONE',  ( -48.28161701412196294, 14.38519811849624119, -16.83766359355620779 ) ) ;
#71345 = FILL_AREA_STYLE_COLOUR ( '', #81379 ) ;
#71346 = EDGE_CURVE ( 'NONE', #106160, #95837, #101518, .T. ) ;
#71347 = CARTESIAN_POINT ( 'NONE',  ( 97.98312614813336552, -59.99999999999999289, 68.82170008167646813 ) ) ;
#71348 = DIRECTION ( 'NONE',  ( 0.5735764363510462704, 0.8191520442889915765, 0.000000000000000000 ) ) ;
#71349 = CARTESIAN_POINT ( 'NONE',  ( 63.56127108291158123, 6.975173280561618775E-15, 0.000000000000000000 ) ) ;
#71350 = FACE_BOUND ( 'NONE', #37317, .T. ) ;
#71351 = ORIENTED_EDGE ( 'NONE', *, *, #101121, .T. ) ;
#71352 = CARTESIAN_POINT ( 'NONE',  ( -82.18314241283663080, -30.00000000000575184, -23.35998342603787137 ) ) ;
#71353 = ORIENTED_EDGE ( 'NONE', *, *, #101481, .T. ) ;
#71354 = DIRECTION ( 'NONE',  ( 0.000000000000000000, 0.000000000000000000, 1.000000000000000000 ) ) ;
#71355 = DIRECTION ( 'NONE',  ( 0.000000000000000000, 0.000000000000000000, 1.000000000000000000 ) ) ;
#71356 = CARTESIAN_POINT ( 'NONE',  ( 8.642223818518250056, 22.39656424817031422, 4.999999999999385381 ) ) ;
#71357 = CARTESIAN_POINT ( 'NONE',  ( 15.79338834186268592, 22.74219270459462194, 1.000334277943696337 ) ) ;
#71358 = CYLINDRICAL_SURFACE ( 'NONE', #63309, 5.000000000000000888 ) ;
#71359 = CARTESIAN_POINT ( 'NONE',  ( -1.320432766682874540E-15, -31.90625000204838813, 7.188101187500000044 ) ) ;
#71360 = LINE ( 'NONE', #15253, #53608 ) ;
#71361 = SURFACE_STYLE_USAGE ( .BOTH. , #15254 ) ;
#71362 = ORIENTED_EDGE ( 'NONE', *, *, #19474, .F. ) ;
#71363 = AXIS2_PLACEMENT_3D ( 'NONE', #51999, #92453, #43918 ) ;
#71364 = CIRCLE ( 'NONE', #93787, 5.000000000000010658 ) ;
#71365 = AXIS2_PLACEMENT_3D ( 'NONE', #17845, #9714, #43694 ) ;
#71366 = APPLICATION_CONTEXT ( 'automotive_design' ) ;
#71367 = ORIENTED_EDGE ( 'NONE', *, *, #65918, .T. ) ;
#71368 = CARTESIAN_POINT ( 'NONE',  ( 81.82597684722991005, -22.15511354699349411, 138.5255780189167751 ) ) ;
#71369 = AXIS2_PLACEMENT_3D ( 'NONE', #88718, #73032, #105942 ) ;
#71370 = CARTESIAN_POINT ( 'NONE',  ( 14.27029591641832518, 3.391655494167657103, -4.551126452496739638 ) ) ;
#71371 = ORIENTED_EDGE ( 'NONE', *, *, #1013, .T. ) ;
#71372 = CARTESIAN_POINT ( 'NONE',  ( 6.849999999999999645, 9.237604307034018802, 0.000000000000000000 ) ) ;
#71373 = CARTESIAN_POINT ( 'NONE',  ( 5.500000000000641265, 42.00000000000000000, -59.88032989331720302 ) ) ;
#71374 = CARTESIAN_POINT ( 'NONE',  ( -2.977408999572650039, -20.18750000204838813, -7.188101187500000933 ) ) ;
#71375 = CARTESIAN_POINT ( 'NONE',  ( -49.73192663144240555, -57.67846088945594829, 76.49129250627629517 ) ) ;
#71376 = CARTESIAN_POINT ( 'NONE',  ( 10.01505413391482868, 294.6430545872282778, 9.892628616759090221 ) ) ;
#71377 = ORIENTED_EDGE ( 'NONE', *, *, #42472, .F. ) ;
#71378 = FILL_AREA_STYLE ('',( #55189 ) ) ;
#71379 = CARTESIAN_POINT ( 'NONE',  ( 72.11682663846713126, 6.975173280561618775E-15, 0.000000000000000000 ) ) ;
#71380 = CARTESIAN_POINT ( 'NONE',  ( 7.409230219490164693, 40.77747305847753267, -58.95054515628400083 ) ) ;
#71381 = CARTESIAN_POINT ( 'NONE',  ( -46.00000000000000000, 488.3725375423296668, 3.127739281037489771 ) ) ;
#71382 = CARTESIAN_POINT ( 'NONE',  ( -3.313708498984765161, -13.15625000409676915, 7.999999999999998224 ) ) ;
#71383 = CARTESIAN_POINT ( 'NONE',  ( -34.94743244184756037, -24.04089725522681320, 33.47236368172110588 ) ) ;
#71384 = CARTESIAN_POINT ( 'NONE',  ( -36.94420904047371579, 25.95859750996718063, 11.10997783219646351 ) ) ;
#71385 = CARTESIAN_POINT ( 'NONE',  ( 0.8333333341588072818, -30.00000000000000355, -31.89470715492279140 ) ) ;
#71386 = CARTESIAN_POINT ( 'NONE',  ( 7.500000000000007105, 41.91230289050422186, -61.59623549333881698 ) ) ;
#71387 = CARTESIAN_POINT ( 'NONE',  ( 23.73746414932995208, 3.851859888774471706E-31, 5.000000000000001776 ) ) ;
#71388 = VECTOR ( 'NONE', #56919, 1000.000000000000114 ) ;
#71389 = CARTESIAN_POINT ( 'NONE',  ( -8.084562802546505722, -14.50028042835467978, 15.55702922181462000 ) ) ;
#71390 = ORIENTED_EDGE ( 'NONE', *, *, #40516, .F. ) ;
#71391 = CARTESIAN_POINT ( 'NONE',  ( 0.000000000000000000, -30.00000000000000000, -8.000000000000000000 ) ) ;
#71392 = CARTESIAN_POINT ( 'NONE',  ( -0.7768758660234635904, 15.00000000000000000, 9.999999999999998224 ) ) ;
#71393 = EDGE_CURVE ( 'NONE', #71455, #93427, #96598, .T. ) ;
#71394 = DIRECTION ( 'NONE',  ( -1.000000000000000000, -0.000000000000000000, -0.000000000000000000 ) ) ;
#71395 = VECTOR ( 'NONE', #102023, 1000.000000000000000 ) ;
#71396 = CARTESIAN_POINT ( 'NONE',  ( -58.50943875393205929, -29.71222703585479863, -33.25288336754142904 ) ) ;
#71397 = CARTESIAN_POINT ( 'NONE',  ( -66.67257040218905217, -30.00000000000000000, 85.09162466317252438 ) ) ;
#71398 = EDGE_CURVE ( 'NONE', #97567, #34125, #82802, .T. ) ;
#71399 = CARTESIAN_POINT ( 'NONE',  ( 7.500000000000007105, 40.00000000000000000, -70.16688272716299934 ) ) ;
#71400 = AXIS2_PLACEMENT_3D ( 'NONE', #2941, #35896, #34289 ) ;
#71401 = AXIS2_PLACEMENT_3D ( 'NONE', #30689, #49482, #23649 ) ;
#71402 = ORIENTED_EDGE ( 'NONE', *, *, #63567, .F. ) ;
#71403 = DIRECTION ( 'NONE',  ( -0.000000000000000000, 1.000000000000000000, -0.000000000000000000 ) ) ;
#71404 = CARTESIAN_POINT ( 'NONE',  ( 91.20819292822160662, -57.61347045221073415, 204.2086795226624076 ) ) ;
#71405 = CARTESIAN_POINT ( 'NONE',  ( 16.64348903516512834, 45.60392139269950462, -6.657797401561770911 ) ) ;
#71406 = CARTESIAN_POINT ( 'NONE',  ( 4.699999999999999289, 5.629165124598849879, 3.250000000000002665 ) ) ;
#71407 = CARTESIAN_POINT ( 'NONE',  ( -14.88719829190656796, 23.11045037498637100, 0.5284321866101354681 ) ) ;
#71408 = CARTESIAN_POINT ( 'NONE',  ( 64.91565662652978119, 40.83906611471883963, 6.815324757212413154 ) ) ;
#71409 = CARTESIAN_POINT ( 'NONE',  ( -74.32166848140413151, -59.99999999999999289, 175.4192060893726364 ) ) ;
#71410 = CARTESIAN_POINT ( 'NONE',  ( 0.2813450144774501949, 7.667988119308862593, -6.122077150241858057 ) ) ;
#71411 = DIRECTION ( 'NONE',  ( -1.000000000000000000, -1.224606353822377258E-16, -0.000000000000000000 ) ) ;
#71412 = CARTESIAN_POINT ( 'NONE',  ( 61.09659575456475977, 50.00000000000000000, -16.41787579823443366 ) ) ;
#71413 = CARTESIAN_POINT ( 'NONE',  ( -85.54972613292714811, -42.91353616863772658, 187.2157232925927133 ) ) ;
#71414 = ORIENTED_EDGE ( 'NONE', *, *, #6733, .T. ) ;
#71415 = CARTESIAN_POINT ( 'NONE',  ( 31.71589149226793936, 316.4455846392050375, -7.213176056726631202 ) ) ;
#71416 = CARTESIAN_POINT ( 'NONE',  ( -6.928203230275508773, -10.00000000000000711, -4.000000000000000000 ) ) ;
#71417 = VECTOR ( 'NONE', #15091, 1000.000000000000000 ) ;
#71418 = CARTESIAN_POINT ( 'NONE',  ( 41.15077806939486749, 488.9683316695932831, 10.18452886344066322 ) ) ;
#71419 = CARTESIAN_POINT ( 'NONE',  ( 3.400000000000000355, 0.000000000000000000, -4.147675477074182382 ) ) ;
#71420 = DIRECTION ( 'NONE',  ( 0.5735764363510490460, 0.8191520442889896891, 0.000000000000000000 ) ) ;
#71421 = VERTEX_POINT ( 'NONE', #71848 ) ;
#71422 = DIRECTION ( 'NONE',  ( -1.000000000000000000, -0.000000000000000000, -0.000000000000000000 ) ) ;
#71423 = FACE_OUTER_BOUND ( 'NONE', #8589, .T. ) ;
#71424 = CARTESIAN_POINT ( 'NONE',  ( -25.22241582816893413, -4.285714285714287364, -3.301606509427108982 ) ) ;
#71425 = CYLINDRICAL_SURFACE ( 'NONE', #42781, 4.000000000000000000 ) ;
#71426 = ADVANCED_FACE ( 'NONE', ( #104217 ), #66238, .F. ) ;
#71427 = CARTESIAN_POINT ( 'NONE',  ( 91.01458086108723933, -60.00000000000020606, -21.64996939806972520 ) ) ;
#71428 = CARTESIAN_POINT ( 'NONE',  ( -80.72224628703636995, -25.62261740639140584, 135.9075979048819249 ) ) ;
#71429 = CIRCLE ( 'NONE', #80053, 5.000000000000001776 ) ;
#71430 = ORIENTED_EDGE ( 'NONE', *, *, #17612, .F. ) ;
#71431 = CARTESIAN_POINT ( 'NONE',  ( 39.73542184579525838, -14.21045842199450782, 43.02758494329003014 ) ) ;
#71432 = DIRECTION ( 'NONE',  ( 0.000000000000000000, -1.000000000000000000, 0.000000000000000000 ) ) ;
#71433 = CARTESIAN_POINT ( 'NONE',  ( 102.9288018374504077, -57.63504169932654264, 202.8890457415012634 ) ) ;
#71434 = CIRCLE ( 'NONE', #726, 4.172000000000001485 ) ;
#71435 = CIRCLE ( 'NONE', #9442, 0.5999999999999980904 ) ;
#71436 = COLOUR_RGB ( '', 0.66274510, 0.83137255, 0.94901961) ;
#71437 = CARTESIAN_POINT ( 'NONE',  ( 33.21822485389247959, 314.5903571069972031, -7.199009675068519520 ) ) ;
#71438 = CARTESIAN_POINT ( 'NONE',  ( 31.87080426956109136, 439.0384429942135966, 24.63328115755081882 ) ) ;
#71439 = ORIENTED_EDGE ( 'NONE', *, *, #25794, .T. ) ;
#71440 = VECTOR ( 'NONE', #11875, 1000.000000000000000 ) ;
#71441 = SURFACE_STYLE_FILL_AREA ( #38068 ) ;
#71442 = DIRECTION ( 'NONE',  ( 0.000000000000000000, 0.000000000000000000, 1.000000000000000000 ) ) ;
#71444 = CARTESIAN_POINT ( 'NONE',  ( -102.6920302767066318, -37.82049116696702384, 167.9539667898588959 ) ) ;
#71443 = CARTESIAN_POINT ( 'NONE',  ( -15.49776003473001929, 37.05489105806098138, 22.93080861416538241 ) ) ;
#71445 = CARTESIAN_POINT ( 'NONE',  ( 7.188101187500001821, -26.56250000204838457, -2.977408999572650483 ) ) ;
#71446 = AXIS2_PLACEMENT_3D ( 'NONE', #72031, #87166, #6213 ) ;
#71447 = CARTESIAN_POINT ( 'NONE',  ( 30.00000000000000000, 0.000000000000000000, 0.000000000000000000 ) ) ;
#71448 = CARTESIAN_POINT ( 'NONE',  ( 5.787483263666111100, 41.99999999999999289, -68.91429206946564534 ) ) ;
#71449 = ADVANCED_FACE ( 'NONE', ( #79419 ), #79939, .T. ) ;
#71450 = EDGE_CURVE ( 'NONE', #26344, #80736, #25812, .T. ) ;
#71451 = CARTESIAN_POINT ( 'NONE',  ( 25.85691572190012621, 37.17365521382656368, 8.914359746511365756 ) ) ;
#71452 = DIRECTION ( 'NONE',  ( 0.000000000000000000, -1.000000000000000000, 0.000000000000000000 ) ) ;
#71453 = B_SPLINE_CURVE_WITH_KNOTS ( 'NONE', 3,
 ( #47231, #7296, #38643, #81184, #56367, #31616, #72573, #105989, #13801, #14862, #6235, #6778, #39698, #7826, #96347, #104958, #80129, #55833, #96865, #40737, #88768, #47754, #24586, #48286, #64503, #22995, #88244, #48812, #63452, #73622 ),
 .UNSPECIFIED., .F., .F.,
 ( 4, 2, 2, 2, 2, 2, 2, 2, 2, 2, 2, 2, 2, 2, 4 ),
 ( 0.004426540215022530672, 0.005358602402234739076, 0.005824633495840844145, 0.006290664589446949215, 0.006523680136250001316, 0.006756695683053053417, 0.006989711229856105518, 0.007222726776659157619, 0.007455742323462209720, 0.007688757870265261821, 0.008154788963871379900, 0.009086851151083614325, 0.01001891333829584702, 0.01095097552550807971, 0.01188303771272031933 ),
 .UNSPECIFIED. ) ;
#71454 = CARTESIAN_POINT ( 'NONE',  ( -36.02493936428357557, 463.3371199957071553, 20.06709031638035157 ) ) ;
#71455 = VERTEX_POINT ( 'NONE', #77838 ) ;
#71456 = CARTESIAN_POINT ( 'NONE',  ( -6.916167714701083824, 41.81554662627394237, -59.83173445090647391 ) ) ;
#71458 = CARTESIAN_POINT ( 'NONE',  ( 27.25886883392396953, -53.38735016083550988, 34.68802301658027432 ) ) ;
#71457 = CARTESIAN_POINT ( 'NONE',  ( -17.10644827616429708, -60.00000000000001421, 42.25319189086976479 ) ) ;
#71459 = CARTESIAN_POINT ( 'NONE',  ( -24.41540814755808242, 25.25641607359507290, 32.32280296090762306 ) ) ;
#71461 = VERTEX_POINT ( 'NONE', #87005 ) ;
#71460 =( BOUNDED_SURFACE ( )  B_SPLINE_SURFACE ( 3, 2, ( 
 ( #94370, #69558, #44759 ),
 ( #92757, #28067, #76563 ),
 ( #52290, #78165, #43675 ),
 ( #18916, #60940, #84674 ),
 ( #10757, #93830, #12887 ),
 ( #45809, #101391, #53371 ),
 ( #85756, #4285, #19984 ),
 ( #78684, #36695, #68500 ),
 ( #27542, #2673, #52829 ),
 ( #86815, #101910, #102448 ),
 ( #11829, #35626, #60422 ),
 ( #86290, #85201, #77648 ),
 ( #12362, #3225, #102984 ),
 ( #3763, #37212, #69036 ),
 ( #93300, #27003, #29144 ),
 ( #28593, #45286, #35086 ),
 ( #61477, #19455, #20532 ),
 ( #70081, #44218, #62014 ),
 ( #11286, #94909, #21048 ),
 ( #77110, #53882, #67956 ),
 ( #100839, #59884, #36167 ),
 ( #51760, #80273, #88919 ),
 ( #21557, #31247, #15013 ),
 ( #46339, #47906, #22082 ),
 ( #63055, #56526, #5861 ),
 ( #29660, #72719, #71653 ),
 ( #46859, #70616, #23144 ),
 ( #79754, #105621, #63600 ) ),
 .UNSPECIFIED., .F., .F., .F. ) 
 B_SPLINE_SURFACE_WITH_KNOTS ( ( 4, 2, 2, 2, 2, 2, 2, 2, 2, 2, 2, 2, 2, 4 ),
 ( 3, 3 ),
 ( -1.788854400193778127E-05, 0.0008258451467879519836, 0.001669578837577841840, 0.002513312528367731696, 0.003357046219157621553, 0.004200779909947511409, 0.005044513600737401265, 0.006731980982317180978, 0.007575714673107070835, 0.008419448363896960691, 0.01010691574547674040, 0.01095064943626663026, 0.01179438312705652012, 0.01348185050863629983 ),
 ( 0.000000000000000000, 1.000000000000000000 ),
 .UNSPECIFIED. ) 
 GEOMETRIC_REPRESENTATION_ITEM ( )  RATIONAL_B_SPLINE_SURFACE ( (
 ( 1.000000000000000000, 1.000000000000000000, 1.000000000000000000),
 ( 1.000000000000000000, 1.000005597033407190, 1.000000000000000000),
 ( 1.000000000000000000, 0.9981174035066882055, 1.000000000000000000),
 ( 1.000000000000000000, 0.9910941550147043255, 1.000000000000000000),
 ( 1.000000000000000000, 0.9859587391847201010, 1.000000000000000000),
 ( 1.000000000000000000, 0.9732073139058156075, 1.000000000000000000),
 ( 1.000000000000000000, 0.9655956055858216924, 1.000000000000000000),
 ( 1.000000000000000000, 0.9487954604333295183, 1.000000000000000000),
 ( 1.000000000000000000, 0.9396125312399712382, 1.000000000000000000),
 ( 1.000000000000000000, 0.9205547400792526425, 1.000000000000000000),
 ( 1.000000000000000000, 0.9106598259530991335, 1.000000000000000000),
 ( 1.000000000000000000, 0.8910166268726569250, 1.000000000000000000),
 ( 1.000000000000000000, 0.8812839758801553902, 1.000000000000000000),
 ( 1.000000000000000000, 0.8530381836209635082, 1.000000000000000000),
 ( 1.000000000000000000, 0.8355499924318912086, 1.000000000000000000),
 ( 1.000000000000000000, 0.8121180734289953351, 1.000000000000000000),
 ( 1.000000000000000000, 0.8047528071578063935, 1.000000000000000000),
 ( 1.000000000000000000, 0.7908772856467519707, 1.000000000000000000),
 ( 1.000000000000000000, 0.7843397418777237062, 1.000000000000000000),
 ( 1.000000000000000000, 0.7662143347357434076, 1.000000000000000000),
 ( 1.000000000000000000, 0.7560053113367869448, 1.000000000000000000),
 ( 1.000000000000000000, 0.7426428230161424837, 1.000000000000000000),
 ( 1.000000000000000000, 0.7385160411531185298, 1.000000000000000000),
 ( 1.000000000000000000, 0.7308023910627007291, 1.000000000000000000),
 ( 1.000000000000000000, 0.7272503285415187202, 1.000000000000000000),
 ( 1.000000000000000000, 0.7174350756271979934, 1.000000000000000000),
 ( 1.000000000000000000, 0.7119478818691705735, 1.000000000000000000),
 ( 1.000000000000000000, 0.7071066567438651917, 1.000000000000000000) ) ) 
 REPRESENTATION_ITEM ( '' )  SURFACE ( )  );
#71462 = ORIENTED_EDGE ( 'NONE', *, *, #40686, .F. ) ;
#71463 = FACE_OUTER_BOUND ( 'NONE', #82051, .T. ) ;
#71464 = CARTESIAN_POINT ( 'NONE',  ( 5.000000000000000000, 0.000000000000000000, 0.000000000000000000 ) ) ;
#71465 = FILL_AREA_STYLE ('',( #88728 ) ) ;
#71466 = CARTESIAN_POINT ( 'NONE',  ( 8.835895239905601883, 2.942464897321981798, 14.70886157470553712 ) ) ;
#71467 = DIRECTION ( 'NONE',  ( -1.000000000000000000, 0.000000000000000000, 0.000000000000000000 ) ) ;
#71468 = ORIENTED_EDGE ( 'NONE', *, *, #3541, .F. ) ;
#71469 = EDGE_CURVE ( 'NONE', #73679, #54417, #30362, .T. ) ;
#71470 = DIRECTION ( 'NONE',  ( 0.000000000000000000, 0.000000000000000000, -1.000000000000000000 ) ) ;
#71471 = CARTESIAN_POINT ( 'NONE',  ( 90.17098323280204397, -29.99999999999950617, 190.0045134580199999 ) ) ;
#71472 = CARTESIAN_POINT ( 'NONE',  ( -10.71234647142379259, 18.37622138056130083, 9.353201953075975794 ) ) ;
#71473 = CARTESIAN_POINT ( 'NONE',  ( -81.98196232622828461, -37.99999999999996447, -13.86369433938586582 ) ) ;
#71474 = DIRECTION ( 'NONE',  ( 1.000000000000000000, 0.000000000000000000, -0.000000000000000000 ) ) ;
#71475 = AXIS2_PLACEMENT_3D ( 'NONE', #11273, #62004, #28056 ) ;
#71476 = EDGE_CURVE ( 'NONE', #69405, #36646, #71323, .T. ) ;
#71477 = CARTESIAN_POINT ( 'NONE',  ( -2.100000000000004530, 0.000000000000000000, 8.500000000000000000 ) ) ;
#71478 = ORIENTED_EDGE ( 'NONE', *, *, #4360, .T. ) ;
#71479 = EDGE_CURVE ( 'NONE', #76326, #59773, #81325, .T. ) ;
#71480 = ORIENTED_EDGE ( 'NONE', *, *, #30875, .F. ) ;
#71481 = ORIENTED_EDGE ( 'NONE', *, *, #19505, .F. ) ;
#71482 = FACE_BOUND ( 'NONE', #99287, .T. ) ;
#71483 = DIRECTION ( 'NONE',  ( 0.000000000000000000, -1.000000000000000000, 0.000000000000000000 ) ) ;
#71484 = DIRECTION ( 'NONE',  ( 1.150791560227848297E-16, -0.3420201433256725987, 0.9396926207859068736 ) ) ;
#71485 = DIRECTION ( 'NONE',  ( -0.000000000000000000, 1.000000000000000000, -0.000000000000000000 ) ) ;
#71486 = PRESENTATION_STYLE_ASSIGNMENT (( #78001 ) ) ;
#71487 = EDGE_CURVE ( 'NONE', #104354, #81388, #20720, .T. ) ;
#71488 = LINE ( 'NONE', #106506, #100998 ) ;
#71489 = CARTESIAN_POINT ( 'NONE',  ( -33.21583695389851698, 487.8294359878406681, 10.09122741356614128 ) ) ;
#71490 = ORIENTED_EDGE ( 'NONE', *, *, #82986, .F. ) ;
#71491 = CARTESIAN_POINT ( 'NONE',  ( -5.036189802313092656, 48.00000000000000000, -93.73786388412078452 ) ) ;
#71492 = B_SPLINE_CURVE_WITH_KNOTS ( 'NONE', 3,
 ( #60124, #92988, #90871, #25641, #19150, #76794 ),
 .UNSPECIFIED., .F., .F.,
 ( 4, 2, 4 ),
 ( 0.000000000000000000, 0.002307655110370370865, 0.004615310220740741730 ),
 .UNSPECIFIED. ) ;
#71493 = ORIENTED_EDGE ( 'NONE', *, *, #45758, .F. ) ;
#71494 = DIRECTION ( 'NONE',  ( 1.000000000000000000, 1.224606353822377258E-16, 0.000000000000000000 ) ) ;
#71495 = PRESENTATION_STYLE_ASSIGNMENT (( #7286 ) ) ;
#71496 = CARTESIAN_POINT ( 'NONE',  ( -81.86715632375494067, -59.99999999999992895, 186.9285674509132207 ) ) ;
#71497 = CARTESIAN_POINT ( 'NONE',  ( 63.65739376113187120, -29.05497423747783259, 76.99861434842904373 ) ) ;
#71498 = AXIS2_PLACEMENT_3D ( 'NONE', #104972, #31113, #64001 ) ;
#71499 = VERTEX_POINT ( 'NONE', #14661 ) ;
#71500 = CARTESIAN_POINT ( 'NONE',  ( 38.06305853432018438, 464.2388122684127438, 19.21895763407759006 ) ) ;
#71501 = CARTESIAN_POINT ( 'NONE',  ( -72.67455277886013221, -38.32345021738819923, -30.15491327014585821 ) ) ;
#71502 = FACE_OUTER_BOUND ( 'NONE', #25970, .T. ) ;
#71503 = CARTESIAN_POINT ( 'NONE',  ( 6.162888688655347558, -3.752776749732574135, -6.500000000000001776 ) ) ;
#71504 = COLOUR_RGB ( '', 0.09019608, 0.27058824, 0.51372549) ;
#71505 = ORIENTED_EDGE ( 'NONE', *, *, #60362, .T. ) ;
#71506 = FILL_AREA_STYLE_COLOUR ( '', #66086 ) ;
#71507 = CARTESIAN_POINT ( 'NONE',  ( -2.275180367705706086, -60.00000000000001421, -36.87650252253413186 ) ) ;
#71508 = VECTOR ( 'NONE', #49991, 999.9999999999998863 ) ;
#71509 = DIRECTION ( 'NONE',  ( 0.000000000000000000, 0.000000000000000000, 1.000000000000000000 ) ) ;
#71510 = CIRCLE ( 'NONE', #99071, 3.309500000000001663 ) ;
#71511 = CARTESIAN_POINT ( 'NONE',  ( 5.656854249492378806, -32.37500000409676915, 5.656854249492381470 ) ) ;
#71512 = STYLED_ITEM ( 'NONE', ( #102789 ), #22353 ) ;
#71513 = CARTESIAN_POINT ( 'NONE',  ( 10.00000000000000000, -5.000000000000000000, 2.617993873628172263 ) ) ;
#71514 = CIRCLE ( 'NONE', #883, 4.000000000000001776 ) ;
#71515 = CARTESIAN_POINT ( 'NONE',  ( 85.88596471057849158, -57.44479720796045541, 193.0254570140299961 ) ) ;
#71516 = CARTESIAN_POINT ( 'NONE',  ( -5.284247479666474234, 16.54466108722069251, -36.10555915917339576 ) ) ;
#71517 = CARTESIAN_POINT ( 'NONE',  ( -5.618500397171760419, 5.062260283225303859, 5.000000000000000888 ) ) ;
#71518 = AXIS2_PLACEMENT_3D ( 'NONE', #25892, #74895, #75977 ) ;
#71519 = CARTESIAN_POINT ( 'NONE',  ( 7.151217271224852290, -8.212505995542866088, -3.587901469523287368 ) ) ;
#71520 = ORIENTED_EDGE ( 'NONE', *, *, #94575, .F. ) ;
#71521 = CARTESIAN_POINT ( 'NONE',  ( 13.53382989543471560, -51.99084025137695875, 30.58576288564093915 ) ) ;
#71522 = CARTESIAN_POINT ( 'NONE',  ( -6.082437715114721581E-15, 5.469921996229787808, -3.525817189091417170 ) ) ;
#71523 = CARTESIAN_POINT ( 'NONE',  ( 37.16605791060757724, -60.00000000000000000, 48.55182899660729845 ) ) ;
#71524 = CARTESIAN_POINT ( 'NONE',  ( -99.16645489262339197, -30.00000000000001066, 146.3472804026664278 ) ) ;
#71525 = EDGE_CURVE ( 'NONE', #7125, #14406, #94685, .T. ) ;
#71526 = DIRECTION ( 'NONE',  ( -1.000000000000000000, -0.000000000000000000, -0.000000000000000000 ) ) ;
#71527 = CARTESIAN_POINT ( 'NONE',  ( 45.01508081842917619, -57.68314626598579054, 65.19425546680545835 ) ) ;
#71528 = EDGE_CURVE ( 'NONE', #24694, #29313, #48143, .T. ) ;
#71530 = CARTESIAN_POINT ( 'NONE',  ( 70.89460441624491693, -4.000000000000000000, 4.898587196589421703E-16 ) ) ;
#71529 = CARTESIAN_POINT ( 'NONE',  ( -0.7860077071742745947, 25.26175349633248857, -40.48553591025817866 ) ) ;
#71531 = FILL_AREA_STYLE ('',( #61890 ) ) ;
#71532 = CARTESIAN_POINT ( 'NONE',  ( -17.69721706678098627, 50.00000000000000711, 62.38211090070038267 ) ) ;
#71533 = CARTESIAN_POINT ( 'NONE',  ( 3.704240196697786924, -1.051219065192640079, 103.3230214382351022 ) ) ;
#71534 = CARTESIAN_POINT ( 'NONE',  ( -0.2874569003302878678, -60.00000000000002842, 39.63907912791243859 ) ) ;
#71535 = CARTESIAN_POINT ( 'NONE',  ( 94.26467260280679739, 1.016364837396684119E-14, 0.000000000000000000 ) ) ;
#71536 = DIRECTION ( 'NONE',  ( 0.000000000000000000, 0.000000000000000000, -1.000000000000000000 ) ) ;
#71537 = EDGE_LOOP ( 'NONE', ( #103561, #31196, #69986 ) ) ;
#71538 = CARTESIAN_POINT ( 'NONE',  ( 17.50000000000004619, 50.30551795521390801, 63.70247084374984325 ) ) ;
#71539 = DIRECTION ( 'NONE',  ( -0.5735764363510510444, -0.8191520442889883569, 0.000000000000000000 ) ) ;
#71540 = CARTESIAN_POINT ( 'NONE',  ( -13.52097269965777571, -42.95778303387159269, 31.13366671246901163 ) ) ;
#71541 = VECTOR ( 'NONE', #100448, 1000.000000000000000 ) ;
#71543 = CARTESIAN_POINT ( 'NONE',  ( 40.89305344739098302, 461.0673237560015423, 2.333915627062251197 ) ) ;
#71542 = CARTESIAN_POINT ( 'NONE',  ( -105.7334699303116849, -59.99999999999997868, 184.1712277148149610 ) ) ;
#71544 = EDGE_CURVE ( 'NONE', #91520, #17308, #61969, .T. ) ;
#71545 = VERTEX_POINT ( 'NONE', #5011 ) ;
#71546 = CARTESIAN_POINT ( 'NONE',  ( 26.48397582124719207, 34.96050029299994577, 7.710214323866814823 ) ) ;
#71547 = PRESENTATION_STYLE_ASSIGNMENT (( #62951 ) ) ;
#71548 = CARTESIAN_POINT ( 'NONE',  ( -14.36708347031724564, 43.38383075969758806, -90.74852574445671394 ) ) ;
#71549 = CARTESIAN_POINT ( 'NONE',  ( 31.08349330513380693, 1.593028355512270962E-15, 0.000000000000000000 ) ) ;
#71550 = CARTESIAN_POINT ( 'NONE',  ( 73.61179401698619529, -60.00000000000000711, 168.2994255929738756 ) ) ;
#71551 = EDGE_CURVE ( 'NONE', #95902, #20011, #37944, .T. ) ;
#71552 = CARTESIAN_POINT ( 'NONE',  ( -45.17824257314219949, 354.4244853104167987, 3.762393652172960845 ) ) ;
#71553 = EDGE_LOOP ( 'NONE', ( #84850, #10057, #100125, #104457, #8337, #82897 ) ) ;
#71554 = SURFACE_STYLE_USAGE ( .BOTH. , #70517 ) ;
#71555 = CARTESIAN_POINT ( 'NONE',  ( 0.000000000000000000, 0.000000000000000000, -8.000000000000000000 ) ) ;
#71557 = FILL_AREA_STYLE ('',( #95858 ) ) ;
#71556 = CARTESIAN_POINT ( 'NONE',  ( 39.49823726628140719, -30.00000000000007461, 47.07845324830893929 ) ) ;
#71558 = CARTESIAN_POINT ( 'NONE',  ( 2.955793532184392003, 98.65757386076514024, -5.000000000000000000 ) ) ;
#71559 = CARTESIAN_POINT ( 'NONE',  ( -4.051286199644067665, -1.398729870307594769, 103.8758286790404810 ) ) ;
#71560 = ORIENTED_EDGE ( 'NONE', *, *, #6867, .T. ) ;
#71561 = TOROIDAL_SURFACE ( 'NONE', #12975, 12.00000000000000711, 3.000000000000000000 ) ;
#71562 = ORIENTED_EDGE ( 'NONE', *, *, #58649, .T. ) ;
#71563 = CARTESIAN_POINT ( 'NONE',  ( -24.69131919313263523, 306.9777677896850605, 9.416086620544890096 ) ) ;
#71564 = EDGE_LOOP ( 'NONE', ( #22565, #46306, #4761, #46047, #106711 ) ) ;
#71565 = FILL_AREA_STYLE ('',( #30619 ) ) ;
#71566 = SURFACE_STYLE_FILL_AREA ( #89889 ) ;
#71568 = ADVANCED_FACE ( 'NONE', ( #47040 ), #77503, .T. ) ;
#71567 = ORIENTED_EDGE ( 'NONE', *, *, #31728, .F. ) ;
#71569 = CARTESIAN_POINT ( 'NONE',  ( 5.000000000000000000, -13.79684580107986314, 10.70524563036420673 ) ) ;
#71570 = CARTESIAN_POINT ( 'NONE',  ( -104.4110070364954623, -59.99999999999994316, 202.5758496764194945 ) ) ;
#71571 = CARTESIAN_POINT ( 'NONE',  ( 46.00000000000000000, 488.0504108836742603, 1.820875518052046171 ) ) ;
#71572 = CARTESIAN_POINT ( 'NONE',  ( 94.45509314101606435, -59.99999999999993605, 202.5749630227759326 ) ) ;
#71573 = LINE ( 'NONE', #99428, #97672 ) ;
#71574 = CARTESIAN_POINT ( 'NONE',  ( -33.00000000000000000, 500.0000000000002274, 0.000000000000000000 ) ) ;
#71575 = AXIS2_PLACEMENT_3D ( 'NONE', #97997, #88853, #56994 ) ;
#71577 = CARTESIAN_POINT ( 'NONE',  ( 12.39938652094127036, -39.47271121152019902, 30.52336634656487035 ) ) ;
#71576 = CARTESIAN_POINT ( 'NONE',  ( -97.37795077744138439, -14.21045842199441722, 96.97852642953840530 ) ) ;
#71578 = FILL_AREA_STYLE_COLOUR ( '', #24134 ) ;
#71579 = CARTESIAN_POINT ( 'NONE',  ( -46.25826378782726778, -32.61579050286022863, 43.25093016562399839 ) ) ;
#71580 = CARTESIAN_POINT ( 'NONE',  ( -6.913779242700421435, 41.73441082398074542, -59.30275289623196500 ) ) ;
#71581 = EDGE_LOOP ( 'NONE', ( #56060, #81314, #101024, #50343, #66580 ) ) ;
#71582 = AXIS2_PLACEMENT_3D ( 'NONE', #21247, #61146, #44972 ) ;
#71583 = CARTESIAN_POINT ( 'NONE',  ( 0.5289635065121225388, 13.43332938984680780, -49.36106157705717123 ) ) ;
#71584 = AXIS2_PLACEMENT_3D ( 'NONE', #6294, #38701, #7360 ) ;
#71585 = AXIS2_PLACEMENT_3D ( 'NONE', #69197, #100475, #36329 ) ;
#71586 = CARTESIAN_POINT ( 'NONE',  ( 17.77153375527972301, 36.31766862386357531, 23.79949801963309142 ) ) ;
#71587 = CARTESIAN_POINT ( 'NONE',  ( 5.093234209761993370, -7.555322265350923772, 3.176141468578050908 ) ) ;
#71588 = CARTESIAN_POINT ( 'NONE',  ( 22.18906107735381283, 305.1406206946286943, -9.938500898754245583 ) ) ;
#71589 = VERTEX_POINT ( 'NONE', #49155 ) ;
#71590 = CARTESIAN_POINT ( 'NONE',  ( -11.63039212333523231, -10.74677606290342524, 10.46692874658227979 ) ) ;
#71591 = ORIENTED_EDGE ( 'NONE', *, *, #69165, .F. ) ;
#71592 = CARTESIAN_POINT ( 'NONE',  ( 103.7182182521570013, -29.99999999999979750, 196.8382105665609743 ) ) ;
#71593 = CARTESIAN_POINT ( 'NONE',  ( 20.59999999999999787, -3.309499999999999886, 4.475777889183790779E-16 ) ) ;
#71594 = AXIS2_PLACEMENT_3D ( 'NONE', #66008, #24528, #64948 ) ;
#71595 = CARTESIAN_POINT ( 'NONE',  ( 6.232496355896457452, 41.83455062734740437, -59.02481358918409171 ) ) ;
#71596 = AXIS2_PLACEMENT_3D ( 'NONE', #104151, #4945, #20654 ) ;
#71597 = CARTESIAN_POINT ( 'NONE',  ( -29.87930712590254956, 10.71892156097790583, -14.93965356295126945 ) ) ;
#71598 = CARTESIAN_POINT ( 'NONE',  ( 99.09559260544375547, -29.99999999999999645, 188.5993032172692381 ) ) ;
#71599 =( BOUNDED_CURVE ( )  B_SPLINE_CURVE ( 2, ( #5944, #46427, #79312, #53961, #4908, #86380, #61567, #55021, #30257 ),
 .UNSPECIFIED., .F., .F. ) 
 B_SPLINE_CURVE_WITH_KNOTS ( ( 3, 2, 2, 2, 3 ),
 ( 0.6323529411764705621, 0.6397058823529411242, 0.6470588235294116863, 0.6544117647058822484, 0.6617647058823528106 ),
 .UNSPECIFIED. ) 
 CURVE ( )  GEOMETRIC_REPRESENTATION_ITEM ( )  RATIONAL_B_SPLINE_CURVE ( ( 1.000000000000000000, 0.9238795325112867385, 1.000000000000000000, 0.9238795325112867385, 1.000000000000000000, 0.9238795325112867385, 1.000000000000000000, 0.9238795325112878487, 0.9999999999999988898 ) ) 
 REPRESENTATION_ITEM ( '' )  );
#71600 = EDGE_CURVE ( 'NONE', #99841, #91137, #90166, .T. ) ;
#71601 = CARTESIAN_POINT ( 'NONE',  ( 38.58349330513380693, 1.593028355512270567E-15, 0.000000000000000000 ) ) ;
#71602 = ORIENTED_EDGE ( 'NONE', *, *, #68224, .T. ) ;
#71603 = EDGE_LOOP ( 'NONE', ( #17712, #57240, #36461, #14283 ) ) ;
#71604 = ORIENTED_EDGE ( 'NONE', *, *, #60022, .T. ) ;
#71605 = DIRECTION ( 'NONE',  ( -1.000000000000000000, -1.224606353822377258E-16, -0.000000000000000000 ) ) ;
#71606 = DIRECTION ( 'NONE',  ( -1.000000000000000000, -1.224606353822377258E-16, -0.000000000000000000 ) ) ;
#71607 = FACE_OUTER_BOUND ( 'NONE', #64454, .T. ) ;
#71608 = ADVANCED_FACE ( 'NONE', ( #91252 ), #6881, .T. ) ;
#71609 = VERTEX_POINT ( 'NONE', #73434 ) ;
#71610 = CARTESIAN_POINT ( 'NONE',  ( -16.01290373797195699, 3.743961321038779655, -0.6473776100927145505 ) ) ;
#71611 = ORIENTED_EDGE ( 'NONE', *, *, #80372, .F. ) ;
#71612 = DIRECTION ( 'NONE',  ( 0.000000000000000000, -1.000000000000000000, 0.000000000000000000 ) ) ;
#71613 = CARTESIAN_POINT ( 'NONE',  ( 97.81756293420689019, -38.47728072526631138, 201.0337594294088888 ) ) ;
#71614 = CARTESIAN_POINT ( 'NONE',  ( 11.09032228048933888, 10.58111460472058951, 9.723575691952698108 ) ) ;
#71615 = CARTESIAN_POINT ( 'NONE',  ( 86.74466300583080169, -60.15137282943332764, -0.9961456128505913332 ) ) ;
#71616 = CARTESIAN_POINT ( 'NONE',  ( 53.26377392596668159, -38.00000000000000000, 56.03167726914934121 ) ) ;
#71617 = CARTESIAN_POINT ( 'NONE',  ( 28.62265479722442763, 310.7111749469181632, 11.81549357303394743 ) ) ;
#71618 = CARTESIAN_POINT ( 'NONE',  ( 8.000000000000000000, -24.68750000409677270, 0.000000000000000000 ) ) ;
#71619 = DIRECTION ( 'NONE',  ( -1.000000000000000000, -1.224606353822377258E-16, -0.000000000000000000 ) ) ;
#71620 = ADVANCED_FACE ( 'NONE', ( #57778 ), #58697, .T. ) ;
#71621 = CIRCLE ( 'NONE', #57834, 3.309500000000001663 ) ;
#71622 = CARTESIAN_POINT ( 'NONE',  ( 1.561520857470387602, -0.03805639397032387072, 101.5970913444665911 ) ) ;
#71623 = EDGE_LOOP ( 'NONE', ( #96049, #60551, #44404, #71462 ) ) ;
#71624 = CARTESIAN_POINT ( 'NONE',  ( -12.39938211290231784, -4.333194019920661333, -12.81742571336049075 ) ) ;
#71625 = CARTESIAN_POINT ( 'NONE',  ( -36.23923339644125008, 462.2853740901311994, 3.478454459919455122 ) ) ;
#71626 = CARTESIAN_POINT ( 'NONE',  ( -2.983137620783093524, 50.82020749530228443, 5.000000000000000000 ) ) ;
#71627 = VERTEX_POINT ( 'NONE', #23330 ) ;
#71628 = CARTESIAN_POINT ( 'NONE',  ( -35.53650496371267309, 390.2108302089691279, 6.619629604413060697 ) ) ;
#71629 = CARTESIAN_POINT ( 'NONE',  ( -31.99696324403842596, 299.5158792032175370, 2.978889298943153907 ) ) ;
#71630 = DIRECTION ( 'NONE',  ( -0.000000000000000000, 1.000000000000000000, 0.000000000000000000 ) ) ;
#71631 = CARTESIAN_POINT ( 'NONE',  ( 3.313708498984762496, -14.28124999999999289, 7.999999999999998224 ) ) ;
#71632 = CARTESIAN_POINT ( 'NONE',  ( 7.451599765851676160, -15.61856177235541487, 34.59380785664056646 ) ) ;
#71633 = DIRECTION ( 'NONE',  ( -1.000000000000000000, -0.000000000000000000, -0.000000000000000000 ) ) ;
#71634 = EDGE_LOOP ( 'NONE', ( #32149, #51943 ) ) ;
#71635 = CARTESIAN_POINT ( 'NONE',  ( 83.62748053872782350, -57.37324410372879413, 189.9579150913779699 ) ) ;
#71636 = CARTESIAN_POINT ( 'NONE',  ( -48.80588606933632434, 9.656672550839656921, 14.61916856843029144 ) ) ;
#71637 = CIRCLE ( 'NONE', #99201, 0.9999999999999998890 ) ;
#71638 = CARTESIAN_POINT ( 'NONE',  ( 36.08349330513379982, 1.593028355512270567E-15, 0.000000000000000000 ) ) ;
#71639 = VERTEX_POINT ( 'NONE', #72385 ) ;
#71640 = CARTESIAN_POINT ( 'NONE',  ( 95.57056055828975616, -57.67170150759548619, 37.78996498690358408 ) ) ;
#71641 = CARTESIAN_POINT ( 'NONE',  ( 24.83349330513380693, -3.851859888774471706E-31, 4.000000000000001776 ) ) ;
#71642 = DIRECTION ( 'NONE',  ( 0.000000000000000000, -1.000000000000000000, 0.000000000000000000 ) ) ;
#71643 = CARTESIAN_POINT ( 'NONE',  ( 28.45466774515011821, 11.90937068246397779, 41.11752270887368610 ) ) ;
#71644 = EDGE_CURVE ( 'NONE', #34393, #89859, #80940, .T. ) ;
#71645 = PRESENTATION_LAYER_ASSIGNMENT (  '', '', ( #90606 ) ) ;
#71646 = CIRCLE ( 'NONE', #25193, 64.50000000000000000 ) ;
#71647 = CARTESIAN_POINT ( 'NONE',  ( 4.761285474643048410, -18.53359912731012216, 35.08063092172267261 ) ) ;
#71648 = CARTESIAN_POINT ( 'NONE',  ( -2.617993873628327250, -5.000000000000000000, 10.00000000000000000 ) ) ;
#71649 = CARTESIAN_POINT ( 'NONE',  ( 26.84999999999999787, 3.309500000000003439, 4.052968581778167743E-16 ) ) ;
#71650 = EDGE_CURVE ( 'NONE', #15655, #97120, #87802, .T. ) ;
#71652 = CARTESIAN_POINT ( 'NONE',  ( -13.77096284681266170, 4.875919819223138774, 5.864315561264231924 ) ) ;
#71651 = CARTESIAN_POINT ( 'NONE',  ( 42.57785895164496992, 484.8808303102439936, 8.276426683567752463 ) ) ;
#71653 = CARTESIAN_POINT ( 'NONE',  ( 9.738398295825046347, 294.6500605438458820, -2.277702036928785034 ) ) ;
#71654 = VECTOR ( 'NONE', #39151, 1000.000000000000000 ) ;
#71655 = CARTESIAN_POINT ( 'NONE',  ( -16.24848081785642506, 43.88994330808112920, -4.219092678288193454 ) ) ;
#71656 = CARTESIAN_POINT ( 'NONE',  ( 9.999999999998589573, 15.11700796859322260, -0.7408669144231687653 ) ) ;
#71657 = DIRECTION ( 'NONE',  ( 0.5735764363510470476, -0.8191520442889911324, 1.003171929053524007E-16 ) ) ;
#71658 = AXIS2_PLACEMENT_3D ( 'NONE', #42132, #8704, #75017 ) ;
#71659 = VECTOR ( 'NONE', #84179, 1000.000000000000000 ) ;
#71660 = CARTESIAN_POINT ( 'NONE',  ( -100.9479196034361905, -37.99999999999996447, 146.8164339967658236 ) ) ;
#71661 = ORIENTED_EDGE ( 'NONE', *, *, #43505, .T. ) ;
#71662 = CARTESIAN_POINT ( 'NONE',  ( -9.885149946167103963, -3.299727015031442168, 15.11772029901440462 ) ) ;
#71663 = DIRECTION ( 'NONE',  ( 0.000000000000000000, 1.000000000000000000, -0.000000000000000000 ) ) ;
#71664 = DIRECTION ( 'NONE',  ( 0.2230022920436083578, -0.09894799074349157342, 0.9697831060969888117 ) ) ;
#71666 = CARTESIAN_POINT ( 'NONE',  ( -58.43662215619989553, -47.40888653656140406, -27.93294337827289908 ) ) ;
#71665 = DIRECTION ( 'NONE',  ( -1.000000000000000000, -0.000000000000000000, -0.000000000000000000 ) ) ;
#71667 = EDGE_CURVE ( 'NONE', #37934, #70163, #75789, .T. ) ;
#71668 = VERTEX_POINT ( 'NONE', #43216 ) ;
#71669 = CARTESIAN_POINT ( 'NONE',  ( 0.6169862416619652512, 8.783631307151134493, -7.913704048099899246 ) ) ;
#71670 = AXIS2_PLACEMENT_3D ( 'NONE', #69530, #94342, #61988 ) ;
#71671 = ORIENTED_EDGE ( 'NONE', *, *, #85921, .F. ) ;
#71672 = CARTESIAN_POINT ( 'NONE',  ( 5.975663821521244756, 4.257391242883541871, 5.625982059626890575 ) ) ;
#71673 = FACE_OUTER_BOUND ( 'NONE', #96507, .T. ) ;
#71674 = CARTESIAN_POINT ( 'NONE',  ( -92.35218344474584740, -59.99999999999998579, 0.8031026304253716663 ) ) ;
#71675 = ORIENTED_EDGE ( 'NONE', *, *, #94307, .F. ) ;
#71676 = DIRECTION ( 'NONE',  ( 0.000000000000000000, 0.000000000000000000, -1.000000000000000000 ) ) ;
#71677 = CARTESIAN_POINT ( 'NONE',  ( 97.42904766945321171, -60.35211980451472158, 196.6984442979972982 ) ) ;
#71679 = DIRECTION ( 'NONE',  ( -1.000000000000000000, -0.000000000000000000, -0.000000000000000000 ) ) ;
#71678 = LINE ( 'NONE', #20015, #102555 ) ;
#71680 = TOROIDAL_SURFACE ( 'NONE', #92402, 7.999999999999998224, 2.000000000000000000 ) ;
#71681 = CARTESIAN_POINT ( 'NONE',  ( -84.05660459919248240, -22.13859885683705286, 152.7253703305752879 ) ) ;
#71682 = VERTEX_POINT ( 'NONE', #28131 ) ;
#71683 = CARTESIAN_POINT ( 'NONE',  ( -9.537291425704626846, 252.6440437733276099, 3.012810007365998022 ) ) ;
#71684 = ORIENTED_EDGE ( 'NONE', *, *, #5716, .F. ) ;
#71685 = VECTOR ( 'NONE', #61676, 1000.000000000000000 ) ;
#71686 = ORIENTED_EDGE ( 'NONE', *, *, #10161, .T. ) ;
#71687 = CARTESIAN_POINT ( 'NONE',  ( 9.340818716798185979E-16, -4.999999999999999112, -8.000000000000000000 ) ) ;
#71688 = CARTESIAN_POINT ( 'NONE',  ( -5.000000000000000000, -14.21727251090714361, 9.320362779988990098 ) ) ;
#71689 = FILL_AREA_STYLE_COLOUR ( '', #34642 ) ;
#71690 = VERTEX_POINT ( 'NONE', #52354 ) ;
#71691 = CARTESIAN_POINT ( 'NONE',  ( -9.090909090909093493, 16.00000000000000000, -4.165977904505303364 ) ) ;
#71692 = CARTESIAN_POINT ( 'NONE',  ( -109.9801870187163644, -57.66844046886203756, 196.1568551196091903 ) ) ;
#71693 = DIRECTION ( 'NONE',  ( -1.000000000000000000, -1.224606353822377258E-16, -0.000000000000000000 ) ) ;
#71694 = CARTESIAN_POINT ( 'NONE',  ( -52.27951051746360633, 48.00000000000000711, 38.96734372144650393 ) ) ;
#71695 = FACE_OUTER_BOUND ( 'NONE', #10048, .T. ) ;
#71696 = CARTESIAN_POINT ( 'NONE',  ( 0.1688296452888967958, 28.20649408426941562, -38.25000000000001421 ) ) ;
#71697 = CARTESIAN_POINT ( 'NONE',  ( 88.92118937161633596, -29.99999999999996092, -15.18954496189254755 ) ) ;
#71698 = CARTESIAN_POINT ( 'NONE',  ( -48.02140427201592132, -30.00000000000008527, 60.50294052774201958 ) ) ;
#71699 = CARTESIAN_POINT ( 'NONE',  ( -52.04820441236028472, -49.90957493855300697, 58.16687430699108319 ) ) ;
#71700 = ORIENTED_EDGE ( 'NONE', *, *, #103543, .F. ) ;
#71701 = LINE ( 'NONE', #104613, #76451 ) ;
#71702 = VERTEX_POINT ( 'NONE', #9763 ) ;
#71703 = CARTESIAN_POINT ( 'NONE',  ( -102.2352430864713284, -60.20054222074153927, 193.9234359043284428 ) ) ;
#71704 = CARTESIAN_POINT ( 'NONE',  ( -30.10055902053746379, 13.03130292445769634, -42.03558690210238780 ) ) ;
#71705 = ORIENTED_EDGE ( 'NONE', *, *, #31053, .F. ) ;
#71706 = CARTESIAN_POINT ( 'NONE',  ( 18.91820918444131649, 48.57558852673482619, 62.17047227842536472 ) ) ;
#71707 =( GEOMETRIC_REPRESENTATION_CONTEXT ( 3 ) GLOBAL_UNCERTAINTY_ASSIGNED_CONTEXT ( ( #36482 ) ) GLOBAL_UNIT_ASSIGNED_CONTEXT ( ( #97775, #48157, #47100 ) ) REPRESENTATION_CONTEXT ( 'NONE', 'WORKASPACE' ) );
#71708 = CARTESIAN_POINT ( 'NONE',  ( 91.32429202933356294, -38.35421070491497630, 28.90131162905761286 ) ) ;
#71709 =( NAMED_UNIT ( * ) PLANE_ANGLE_UNIT ( ) SI_UNIT ( $, .RADIAN. ) );
#71710 = CARTESIAN_POINT ( 'NONE',  ( -4.000000000000000000, 0.000000000000000000, -1.161000000000000032 ) ) ;
#71711 = CARTESIAN_POINT ( 'NONE',  ( -2.627668993003716480, 302.8385116830480683, 9.934221043902621062 ) ) ;
#71712 = CARTESIAN_POINT ( 'NONE',  ( -39.84233570596349949, 333.3323931548420660, 19.23895789620553032 ) ) ;
#71713 = DIRECTION ( 'NONE',  ( -1.000000000000000000, -1.224606353822377258E-16, -0.000000000000000000 ) ) ;
#71714 = CARTESIAN_POINT ( 'NONE',  ( 4.658343928564455894, 51.51306124665670438, -8.372077115008158543 ) ) ;
#71715 = DIRECTION ( 'NONE',  ( 0.5401002696852920115, 0.5464483025172063302, 0.6400671459791846818 ) ) ;
#71716 = EDGE_CURVE ( 'NONE', #58911, #44820, #74016, .T. ) ;
#71717 = AXIS2_PLACEMENT_3D ( 'NONE', #2414, #26742, #1328 ) ;
#71718 = CARTESIAN_POINT ( 'NONE',  ( -33.86867596911223188, 484.1347864990148082, 1.565332731471725136 ) ) ;
#71719 = UNCERTAINTY_MEASURE_WITH_UNIT (LENGTH_MEASURE( 1.000000000000000082E-05 ), #85879, 'distance_accuracy_value', 'NONE');
#71720 = EDGE_CURVE ( 'NONE', #100006, #65882, #94765, .T. ) ;
#71721 = ORIENTED_EDGE ( 'NONE', *, *, #52085, .T. ) ;
#71722 = EDGE_LOOP ( 'NONE', ( #90491, #76209, #14831, #63207 ) ) ;
#71723 = CARTESIAN_POINT ( 'NONE',  ( 50.96143459282708221, -32.58239369279106512, 49.99714469605078193 ) ) ;
#71724 = CARTESIAN_POINT ( 'NONE',  ( -0.9432067108799188082, 12.66774627894649363, 49.67605769803894589 ) ) ;
#71725 = DIRECTION ( 'NONE',  ( -0.000000000000000000, -1.000000000000000000, -0.000000000000000000 ) ) ;
#71726 = ADVANCED_FACE ( 'NONE', ( #83650 ), #87821, .T. ) ;
#71727 = CARTESIAN_POINT ( 'NONE',  ( -110.7820348957689305, -38.35618030932103295, 179.6175950015601757 ) ) ;
#71728 = ORIENTED_EDGE ( 'NONE', *, *, #72017, .F. ) ;
#71729 = CARTESIAN_POINT ( 'NONE',  ( 89.37870489931546558, -38.38696938715336415, -17.35345262173043679 ) ) ;
#71730 = CARTESIAN_POINT ( 'NONE',  ( 10.43175756363495488, 17.29745240936010120, -9.784780675101240277 ) ) ;
#71731 = DIRECTION ( 'NONE',  ( 0.000000000000000000, -1.000000000000000000, 0.000000000000000000 ) ) ;
#71732 = CARTESIAN_POINT ( 'NONE',  ( 13.50000000000000355, -2.625659737069745869, -0.1132121849006624686 ) ) ;
#71734 = CARTESIAN_POINT ( 'NONE',  ( 97.56555718646720265, -60.15121296667719264, 100.7618488147239333 ) ) ;
#71733 = AXIS2_PLACEMENT_3D ( 'NONE', #46169, #79583, #5178 ) ;
#71735 = CIRCLE ( 'NONE', #23579, 3.000000000000000000 ) ;
#71736 = CARTESIAN_POINT ( 'NONE',  ( -31.96652969245341325, 438.9664737494705378, 23.62269400183483725 ) ) ;
#71738 = CIRCLE ( 'NONE', #70061, 4.000000000000000000 ) ;
#71737 = LINE ( 'NONE', #35849, #37614 ) ;
#71739 = CARTESIAN_POINT ( 'NONE',  ( -33.00000000000000000, 435.0774731480752848, 11.67986145722080948 ) ) ;
#71740 = CARTESIAN_POINT ( 'NONE',  ( 90.23526155271706273, -60.00000000000000000, 202.0276669837681709 ) ) ;
#71741 = AXIS2_PLACEMENT_3D ( 'NONE', #45198, #96913, #53275 ) ;
#71742 = EDGE_CURVE ( 'NONE', #88131, #83796, #31022, .T. ) ;
#71743 = AXIS2_PLACEMENT_3D ( 'NONE', #66514, #56816, #25569 ) ;
#71744 = CARTESIAN_POINT ( 'NONE',  ( -16.75187969033532553, 34.99134772383131065, 21.80698433968612093 ) ) ;
#71745 = ORIENTED_EDGE ( 'NONE', *, *, #19382, .T. ) ;
#71746 = CARTESIAN_POINT ( 'NONE',  ( 59.20395090875183541, -36.01664205692539866, 68.56248700397097195 ) ) ;
#71747 = CARTESIAN_POINT ( 'NONE',  ( -34.00613029049673486, 301.2164055778219449, -0.5617985262917791767 ) ) ;
#71748 = CARTESIAN_POINT ( 'NONE',  ( 7.551560007654698481, 33.00910351806991372, -2.648022159607831938 ) ) ;
#71749 = ADVANCED_FACE ( 'NONE', ( #34095 ), #61009, .T. ) ;
#71750 = DIRECTION ( 'NONE',  ( 0.000000000000000000, 1.000000000000000000, 0.000000000000000000 ) ) ;
#71751 = ORIENTED_EDGE ( 'NONE', *, *, #99230, .T. ) ;
#71753 = DIRECTION ( 'NONE',  ( 1.000000000000000000, 0.000000000000000000, -0.000000000000000000 ) ) ;
#71752 = CARTESIAN_POINT ( 'NONE',  ( -105.3108324701758107, -38.38841466978784212, 197.1710578805450211 ) ) ;
#71754 = CARTESIAN_POINT ( 'NONE',  ( 4.916373759799321341, -3.000000000000000444, -6.397334739185440711 ) ) ;
#71755 = CYLINDRICAL_SURFACE ( 'NONE', #12245, 4.000000000000002665 ) ;
#71756 = LINE ( 'NONE', #28702, #66176 ) ;
#71757 = CARTESIAN_POINT ( 'NONE',  ( 5.656854249492378806, -33.68749999999999289, 5.656854249492381470 ) ) ;
#71758 = CARTESIAN_POINT ( 'NONE',  ( -9.999999999999996447, -3.000000000000002665, -86.30899693747677759 ) ) ;
#71759 = CARTESIAN_POINT ( 'NONE',  ( -42.09158233638504498, 465.7816406625409513, 14.79318349170026892 ) ) ;
#71760 = ORIENTED_EDGE ( 'NONE', *, *, #40564, .F. ) ;
#71761 = CARTESIAN_POINT ( 'NONE',  ( 85.73810161015232723, -21.86527338768217632, 169.1334664433469754 ) ) ;
#71763 = CIRCLE ( 'NONE', #21848, 0.9999999999999998890 ) ;
#71762 = CARTESIAN_POINT ( 'NONE',  ( 9.413036185852410753, 141.7043030661344858, -0.000000000000000000 ) ) ;
#71764 = CARTESIAN_POINT ( 'NONE',  ( -36.95591949233575946, 439.3722685534989409, 23.79946508175408937 ) ) ;
#71765 = ORIENTED_EDGE ( 'NONE', *, *, #642, .T. ) ;
#71766 = DIRECTION ( 'NONE',  ( 1.224646799147349509E-16, 0.000000000000000000, -1.000000000000000000 ) ) ;
#71767 = CARTESIAN_POINT ( 'NONE',  ( 2.971071886220384428, 5.790204346174069983, 1.217186345204429587E-15 ) ) ;
#71768 = CARTESIAN_POINT ( 'NONE',  ( -1.590636543732056873, 50.00000000000000711, -96.99986829839870950 ) ) ;
#71769 = CARTESIAN_POINT ( 'NONE',  ( -34.55014207014404093, 42.66529688316376223, -63.00140760762604231 ) ) ;
#71770 = VECTOR ( 'NONE', #8706, 999.9999999999998863 ) ;
#71771 = DIRECTION ( 'NONE',  ( 0.000000000000000000, 0.000000000000000000, 1.000000000000000000 ) ) ;
#71772 = VERTEX_POINT ( 'NONE', #17892 ) ;
#71773 = ADVANCED_FACE ( 'NONE', ( #17360, #26019, #60488, #35694, #1670 ), #18937, .F. ) ;
#71774 =( NAMED_UNIT ( * ) SI_UNIT ( $, .STERADIAN. ) SOLID_ANGLE_UNIT ( ) );
#71775 = CARTESIAN_POINT ( 'NONE',  ( -81.74144244633359335, -29.99999999999999645, 31.24147803549975677 ) ) ;
#71776 = CARTESIAN_POINT ( 'NONE',  ( 38.65303601453097571, 25.17668755055779428, 12.83022762705334330 ) ) ;
#71777 = CARTESIAN_POINT ( 'NONE',  ( 71.63333333333333997, 3.309500000000014541, 4.052968581778174646E-16 ) ) ;
#71778 = EDGE_CURVE ( 'NONE', #58722, #92197, #67498, .T. ) ;
#71779 = EDGE_CURVE ( 'NONE', #67879, #106068, #45400, .T. ) ;
#71781 = CARTESIAN_POINT ( 'NONE',  ( -11.21715996676264737, 19.86009903824175638, -8.535609670724019438 ) ) ;
#71780 = CARTESIAN_POINT ( 'NONE',  ( 7.439123282901347167, 41.00341550150766068, -68.91429205944716330 ) ) ;
#71782 = CARTESIAN_POINT ( 'NONE',  ( 5.082755093536325930, -18.96875000204838457, -5.082755093536325042 ) ) ;
#71783 = CARTESIAN_POINT ( 'NONE',  ( -28.52992520858366632, 16.51490304376828178, -41.35306031657921011 ) ) ;
#71784 = FACE_OUTER_BOUND ( 'NONE', #68442, .T. ) ;
#71785 = B_SPLINE_CURVE_WITH_KNOTS ( 'NONE', 3,
 ( #95124, #6084, #104246, #63814, #62240, #64343 ),
 .UNSPECIFIED., .F., .F.,
 ( 4, 2, 4 ),
 ( 0.006874058789394425426, 0.008773169699889938472, 0.01067228061038544978 ),
 .UNSPECIFIED. ) ;
#71786 = CIRCLE ( 'NONE', #13201, 3.400000000000000355 ) ;
#71787 = ORIENTED_EDGE ( 'NONE', *, *, #67743, .T. ) ;
#71788 = PLANE ( 'NONE',  #11346 ) ;
#71789 = CARTESIAN_POINT ( 'NONE',  ( 10.41054107240687188, -5.000000000000000000, 6.123233995736768255E-16 ) ) ;
#71790 = CARTESIAN_POINT ( 'NONE',  ( -7.860352320341752019, 85.38611325936935259, 5.079056458989159063E-12 ) ) ;
#71791 = LINE ( 'NONE', #28740, #84273 ) ;
#71792 = LINE ( 'NONE', #22228, #20881 ) ;
#71793 = EDGE_CURVE ( 'NONE', #78511, #40136, #43740, .T. ) ;
#71794 = ORIENTED_EDGE ( 'NONE', *, *, #104587, .F. ) ;
#71795 = CARTESIAN_POINT ( 'NONE',  ( 44.39546657021049469, 435.2018463496405047, 12.64356380809994995 ) ) ;
#71796 = CYLINDRICAL_SURFACE ( 'NONE', #3111, 4.250000000000000000 ) ;
#71797 = COLOUR_RGB ( '', 0.72549020, 0.75294118, 0.79215686) ;
#71798 = EDGE_LOOP ( 'NONE', ( #70722, #61837, #63029, #10066 ) ) ;
#71799 = EDGE_CURVE ( 'NONE', #3167, #94772, #72327, .T. ) ;
#71800 = SURFACE_STYLE_FILL_AREA ( #78310 ) ;
#71801 = CARTESIAN_POINT ( 'NONE',  ( -1.509171067931242671, -0.02491874495535326833, 101.6143504438094851 ) ) ;
#71802 = CARTESIAN_POINT ( 'NONE',  ( 6.750000000000017764, 11.69134295108991317, 0.000000000000000000 ) ) ;
#71803 = SURFACE_STYLE_USAGE ( .BOTH. , #55603 ) ;
#71804 = UNCERTAINTY_MEASURE_WITH_UNIT (LENGTH_MEASURE( 1.000000000000000082E-05 ), #55870, 'distance_accuracy_value', 'NONE');
#71805 = CARTESIAN_POINT ( 'NONE',  ( -111.1441913338302356, -59.99999999999999289, 153.5661079110527680 ) ) ;
#71806 = PRODUCT_DEFINITION_SHAPE ( 'NONE', 'NONE',  #106819 ) ;
#71807 = AXIS2_PLACEMENT_3D ( 'NONE', #26702, #19149, #59575 ) ;
#71808 = AXIS2_PLACEMENT_3D ( 'NONE', #99662, #27423, #19342 ) ;
#71809 = CARTESIAN_POINT ( 'NONE',  ( 96.86866073052655679, 1.030564683017419500E-14, 0.000000000000000000 ) ) ;
#71810 = CIRCLE ( 'NONE', #73580, 1.999999999999999334 ) ;
#71811 = CIRCLE ( 'NONE', #82131, 0.9999999999999968914 ) ;
#71812 = CARTESIAN_POINT ( 'NONE',  ( 24.60488647473181345, 306.9835580411500473, 10.41807558718820914 ) ) ;
#71813 = DIRECTION ( 'NONE',  ( 0.000000000000000000, 0.000000000000000000, -1.000000000000000000 ) ) ;
#71814 = EDGE_CURVE ( 'NONE', #93762, #43590, #76628, .T. ) ;
#71815 = CARTESIAN_POINT ( 'NONE',  ( 71.63333333333333997, 3.309500000000014541, 0.000000000000000000 ) ) ;
#71816 = CARTESIAN_POINT ( 'NONE',  ( -83.24037337117431434, -42.98078370665466963, 177.1168375766181384 ) ) ;
#71817 = ORIENTED_EDGE ( 'NONE', *, *, #21063, .T. ) ;
#71818 = CARTESIAN_POINT ( 'NONE',  ( 25.63492787469831313, 43.60956991405247862, -75.25780077383848266 ) ) ;
#71819 = AXIS2_PLACEMENT_3D ( 'NONE', #71980, #104889, #7230 ) ;
#71820 =( GEOMETRIC_REPRESENTATION_CONTEXT ( 3 ) GLOBAL_UNCERTAINTY_ASSIGNED_CONTEXT ( ( #80343 ) ) GLOBAL_UNIT_ASSIGNED_CONTEXT ( ( #92908, #84829, #43827 ) ) REPRESENTATION_CONTEXT ( 'NONE', 'WORKASPACE' ) );
#71821 = ORIENTED_EDGE ( 'NONE', *, *, #65543, .F. ) ;
#71822 = CARTESIAN_POINT ( 'NONE',  ( 26.08349330513380693, -4.000000000000000888, 4.898587196589416773E-16 ) ) ;
#71823 = CARTESIAN_POINT ( 'NONE',  ( 4.497472161260645862, -65.54222546625949519, -3.972129482042466186 ) ) ;
#71824 = CARTESIAN_POINT ( 'NONE',  ( -83.68625982447714762, -45.26552441130044713, 14.69813845894242199 ) ) ;
#71825 = CARTESIAN_POINT ( 'NONE',  ( -13.27220259399123314, 304.5542592310576993, 9.873754584668670731 ) ) ;
#71826 = CARTESIAN_POINT ( 'NONE',  ( -14.83882035797429566, 4.620392632309972214, -5.701545570398202756 ) ) ;
#71827 = CARTESIAN_POINT ( 'NONE',  ( 3.168333439190436529, 39.18265495645905361, -5.000000000000000000 ) ) ;
#71828 = CARTESIAN_POINT ( 'NONE',  ( 23.57730434123481800, 18.64316884710268596, -30.67950393663962672 ) ) ;
#71829 = CARTESIAN_POINT ( 'NONE',  ( 80.78816237064734196, -29.99999999999997513, 192.9482874834278903 ) ) ;
#71830 = CARTESIAN_POINT ( 'NONE',  ( -93.27866288726950472, -14.21045842199433373, 72.78127944122930160 ) ) ;
#71831 = CARTESIAN_POINT ( 'NONE',  ( -62.59898750523465338, -56.86926829012708851, 88.13743897392122051 ) ) ;
#71832 = ORIENTED_EDGE ( 'NONE', *, *, #99818, .F. ) ;
#71833 = CARTESIAN_POINT ( 'NONE',  ( -52.56491209535032993, 39.42572890908716943, -38.23519342730719472 ) ) ;
#71834 = CARTESIAN_POINT ( 'NONE',  ( 47.96672227968453939, -59.99999999998527045, 73.04161892766875042 ) ) ;
#71835 = ORIENTED_EDGE ( 'NONE', *, *, #68656, .F. ) ;
#71836 = CARTESIAN_POINT ( 'NONE',  ( 2.027295390931008967, -46.43466668287893384, 31.62625868155275555 ) ) ;
#71837 = CARTESIAN_POINT ( 'NONE',  ( -7.188101187500000933, -17.37500000204838813, -2.977408999572651371 ) ) ;
#71838 = CARTESIAN_POINT ( 'NONE',  ( 40.34715123528543046, 0.000000000000000000, 5.000000000000002665 ) ) ;
#71839 = ORIENTED_EDGE ( 'NONE', *, *, #36390, .F. ) ;
#71840 = CIRCLE ( 'NONE', #15019, 4.000000000000000888 ) ;
#71841 = DIRECTION ( 'NONE',  ( 0.000000000000000000, 0.000000000000000000, 1.000000000000000000 ) ) ;
#71842 = EDGE_LOOP ( 'NONE', ( #84587, #55968, #30812, #19776, #77957 ) ) ;
#71843 = CARTESIAN_POINT ( 'NONE',  ( 11.30587238908012360, 45.32085087904604848, -14.90049756856787866 ) ) ;
#71844 = CARTESIAN_POINT ( 'NONE',  ( -5.082755093536326818, -29.09375000204838813, 5.082755093536325042 ) ) ;
#71845 = CARTESIAN_POINT ( 'NONE',  ( -93.99879809186631974, -60.00000000000000000, 41.63443083181508797 ) ) ;
#71846 = FACE_OUTER_BOUND ( 'NONE', #47056, .T. ) ;
#71847 = CARTESIAN_POINT ( 'NONE',  ( -1.320432766682874540E-15, -24.40625000204838813, 7.188101187500000044 ) ) ;
#71848 = CARTESIAN_POINT ( 'NONE',  ( 0.7145311798163216377, 4.618802153517004960, 7.999999999999998224 ) ) ;
#71849 = CONICAL_SURFACE ( 'NONE', #59787, 8.000000000000000000, 0.9599310885968911355 ) ;
#71850 = CARTESIAN_POINT ( 'NONE',  ( -5.615632394126207849, 54.12034592349190376, -6.063825715703227814 ) ) ;
#71851 = CARTESIAN_POINT ( 'NONE',  ( 5.000000000000000000, -61.56619815149595354, 13.02652999465270511 ) ) ;
#71852 = CARTESIAN_POINT ( 'NONE',  ( 7.996668422911924701, 48.00000000000000000, -91.14546720081904141 ) ) ;
#71853 = CARTESIAN_POINT ( 'NONE',  ( -6.928203230275509661, 105.2652615693258724, 4.000000000000001776 ) ) ;
#71854 = CARTESIAN_POINT ( 'NONE',  ( -40.86217775602844426, 319.2309035517266693, 3.920900997671151078 ) ) ;
#71855 = EDGE_CURVE ( 'NONE', #11400, #234, #63729, .T. ) ;
#71856 = CARTESIAN_POINT ( 'NONE',  ( 27.46788371183871291, 305.3393767471599176, -9.450502104329384423 ) ) ;
#71857 = B_SPLINE_CURVE_WITH_KNOTS ( 'NONE', 3,
 ( #8748, #105847, #24965, #32532 ),
 .UNSPECIFIED., .F., .F.,
 ( 4, 4 ),
 ( 1.170938346284344789E-17, 0.003511374632863300226 ),
 .UNSPECIFIED. ) ;
#71858 = CARTESIAN_POINT ( 'NONE',  ( -36.59723990820980788, -53.36088228589063931, 39.00306241562584830 ) ) ;
#71859 = ORIENTED_EDGE ( 'NONE', *, *, #81424, .T. ) ;
#71860 = CARTESIAN_POINT ( 'NONE',  ( -5.385673916453011856, 3.157894736842104866, 14.66382285868950675 ) ) ;
#71861 = CARTESIAN_POINT ( 'NONE',  ( 36.40464493058440354, -29.12080053541245661, 34.06312112947962589 ) ) ;
#71862 = CARTESIAN_POINT ( 'NONE',  ( -17.01589776168603407, -1.734723475976807094E-15, -2.227375807157456755 ) ) ;
#71863 = EDGE_LOOP ( 'NONE', ( #4835, #40457, #42391, #29482 ) ) ;
#71864 = ADVANCED_FACE ( 'NONE', ( #89391 ), #1717, .T. ) ;
#71866 = AXIS2_PLACEMENT_3D ( 'NONE', #11899, #102517, #61546 ) ;
#71865 = CARTESIAN_POINT ( 'NONE',  ( 6.169949891409288512, -6.308465495019287772, 2.073417244830710437 ) ) ;
#71867 = EDGE_CURVE ( 'NONE', #42316, #88009, #105728, .T. ) ;
#71868 = CARTESIAN_POINT ( 'NONE',  ( -67.51048420570765529, -38.33477690727864484, 123.4165462485304658 ) ) ;
#71869 = ORIENTED_EDGE ( 'NONE', *, *, #54468, .T. ) ;
#71871 = CARTESIAN_POINT ( 'NONE',  ( -30.12932728364529922, 334.4140447340107585, 17.11298374841474867 ) ) ;
#71870 = CARTESIAN_POINT ( 'NONE',  ( 8.599968422084343089, -5.000000000000000888, -16.55615795282379921 ) ) ;
#71872 = DIRECTION ( 'NONE',  ( -1.000000000000000000, -1.224606353822377258E-16, -0.000000000000000000 ) ) ;
#71873 = CARTESIAN_POINT ( 'NONE',  ( 15.75384615384615294, -4.171999999999999709, 5.616230220889763424E-16 ) ) ;
#71874 = EDGE_CURVE ( 'NONE', #21594, #84503, #9260, .T. ) ;
#71875 = SURFACE_STYLE_USAGE ( .BOTH. , #62743 ) ;
#71877 = CIRCLE ( 'NONE', #73552, 0.9999999999999941158 ) ;
#71876 = CARTESIAN_POINT ( 'NONE',  ( -48.76802610285282924, 13.46002349908751050, -16.61772763643321582 ) ) ;
#71878 = CARTESIAN_POINT ( 'NONE',  ( -5.559924265777227426E-15, -7.321656987762867885, 3.318518101603013193 ) ) ;
#71879 = EDGE_CURVE ( 'NONE', #29099, #74232, #42706, .T. ) ;
#71880 = CARTESIAN_POINT ( 'NONE',  ( 95.43964957209735189, -60.00000000000000000, 52.17412195945332343 ) ) ;
#71881 = ADVANCED_FACE ( 'NONE', ( #53436 ), #103570, .F. ) ;
#71882 = FACE_OUTER_BOUND ( 'NONE', #21243, .T. ) ;
#71883 = EDGE_CURVE ( 'NONE', #58211, #27928, #56459, .T. ) ;
#71884 = CARTESIAN_POINT ( 'NONE',  ( 9.797174393178825657E-16, -100.0000000000000000, 8.000000000000000000 ) ) ;
#71885 = CARTESIAN_POINT ( 'NONE',  ( 43.75401118688382951, 486.3173572309547694, 5.908089951475070656 ) ) ;
#71886 = ORIENTED_EDGE ( 'NONE', *, *, #79500, .T. ) ;
#71887 = CARTESIAN_POINT ( 'NONE',  ( -77.54319449862920521, -29.99999999999670308, -26.30707014989112125 ) ) ;
#71888 = ORIENTED_EDGE ( 'NONE', *, *, #58675, .T. ) ;
#71889 = CARTESIAN_POINT ( 'NONE',  ( 72.85555555555556850, 6.915964383211875250E-15, 0.000000000000000000 ) ) ;
#71890 = CARTESIAN_POINT ( 'NONE',  ( -15.93251508686752160, 3.184445033434176509, 1.451444771606926754 ) ) ;
#71891 = FILL_AREA_STYLE ('',( #98292 ) ) ;
#71892 = DIRECTION ( 'NONE',  ( 0.000000000000000000, -1.000000000000000000, 0.000000000000000000 ) ) ;
#71894 = DIRECTION ( 'NONE',  ( 0.000000000000000000, 1.000000000000000000, 0.000000000000000000 ) ) ;
#71893 = CIRCLE ( 'NONE', #85697, 0.7733184030943203169 ) ;
#71895 = CIRCLE ( 'NONE', #61527, 3.309500000000001663 ) ;
#71896 = CARTESIAN_POINT ( 'NONE',  ( -7.188101187500001821, -23.37500000204839168, -2.977408999572651371 ) ) ;
#71897 = CYLINDRICAL_SURFACE ( 'NONE', #38165, 8.000000000000000000 ) ;
#71898 = CARTESIAN_POINT ( 'NONE',  ( 86.17777777777776294, 1.023464760207051730E-14, 0.000000000000000000 ) ) ;
#71899 = CARTESIAN_POINT ( 'NONE',  ( 6.974441890915084485, 41.03925908523778077, -70.79755109270119817 ) ) ;
#71900 = VERTEX_POINT ( 'NONE', #77712 ) ;
#71901 = AXIS2_PLACEMENT_3D ( 'NONE', #38885, #96057, #15648 ) ;
#71902 = AXIS2_PLACEMENT_3D ( 'NONE', #68787, #35915, #101668 ) ;
#71903 = AXIS2_PLACEMENT_3D ( 'NONE', #9599, #52729, #75409 ) ;
#71904 = VECTOR ( 'NONE', #78354, 1000.000000000000000 ) ;
#71906 = EDGE_LOOP ( 'NONE', ( #84981, #101210, #33730, #99269 ) ) ;
#71905 = DIRECTION ( 'NONE',  ( 0.000000000000000000, 0.000000000000000000, 1.000000000000000000 ) ) ;
#71907 = CARTESIAN_POINT ( 'NONE',  ( 80.77733221968003363, -42.96683419437847107, 155.3669859002530700 ) ) ;
#71908 = PRESENTATION_STYLE_ASSIGNMENT (( #6101 ) ) ;
#71909 = ORIENTED_EDGE ( 'NONE', *, *, #7797, .T. ) ;
#71910 = CARTESIAN_POINT ( 'NONE',  ( -12.50000000000000355, 27.18132204066968427, -44.72105335469841947 ) ) ;
#71911 = DIRECTION ( 'NONE',  ( 1.000000000000000000, 0.000000000000000000, -0.000000000000000000 ) ) ;
#71912 = CARTESIAN_POINT ( 'NONE',  ( -7.188101187500002709, -13.81250000204838457, 2.977408999572647819 ) ) ;
#71913 = CARTESIAN_POINT ( 'NONE',  ( 6.928203230275512325, 29.73473843067414890, 4.000000000000002665 ) ) ;
#71914 = CARTESIAN_POINT ( 'NONE',  ( 11.42604336269065612, 45.35830052782391419, 14.67759751612675423 ) ) ;
#71915 = CARTESIAN_POINT ( 'NONE',  ( 15.66780019633566567, 294.5588774916458306, 1.874735905060328056 ) ) ;
#71916 = ORIENTED_EDGE ( 'NONE', *, *, #43854, .F. ) ;
#71917 = B_SPLINE_CURVE_WITH_KNOTS ( 'NONE', 3,
 ( #98882, #98372, #82178, #16939, #64946, #56839, #89764, #73015, #15861, #25043, #8294, #34207, #66538, #8826, #99412, #57899, #48739, #90823, #25594, #49817, #41200, #58452, #82722, #42251, #81632, #7756, #40664, #73548, #41730, #74614, #106452, #83248, #57365, #48216 ),
 .UNSPECIFIED., .F., .F.,
 ( 4, 2, 2, 2, 2, 2, 2, 2, 2, 2, 2, 2, 2, 2, 2, 2, 4 ),
 ( 0.01272238763756221303, 0.01351613129786393037, 0.01430987495816564946, 0.01510361861846736681, 0.01589736227876908589, 0.01669110593907080498, 0.01748484959937252059, 0.01827859325967423967, 0.01907233691997595876, 0.01986608058027767437, 0.02065982424057939346, 0.02145356790088111254, 0.02224731156118282815, 0.02304105522148454724, 0.02383479888178626632, 0.02462854254208798194, 0.02542228620238970102 ),
 .UNSPECIFIED. ) ;
#71918 =( NAMED_UNIT ( * ) SI_UNIT ( $, .STERADIAN. ) SOLID_ANGLE_UNIT ( ) );
#71919 = AXIS2_PLACEMENT_3D ( 'NONE', #17964, #75098, #42215 ) ;
#71920 = PRESENTATION_STYLE_ASSIGNMENT (( #105353 ) ) ;
#71921 = CARTESIAN_POINT ( 'NONE',  ( 0.000000000000000000, 15.00000000000000000, 0.000000000000000000 ) ) ;
#71922 = CARTESIAN_POINT ( 'NONE',  ( 7.126148245860624009, 41.12758397993106030, -58.55282951229288102 ) ) ;
#71923 = ADVANCED_FACE ( 'NONE', ( #78748 ), #22385, .F. ) ;
#71924 = CARTESIAN_POINT ( 'NONE',  ( 7.500000000000000000, -4.330127018922200755, -10.00000000000000000 ) ) ;
#71925 = VECTOR ( 'NONE', #35852, 1000.000000000000000 ) ;
#71926 = ORIENTED_EDGE ( 'NONE', *, *, #64772, .F. ) ;
#71927 = CARTESIAN_POINT ( 'NONE',  ( 4.898587196589412829E-16, -13.81250000409676915, -8.000000000000000000 ) ) ;
#71928 = CARTESIAN_POINT ( 'NONE',  ( -12.33464901170365380, -14.37923961157706998, 31.77351814907940053 ) ) ;
#71929 = CARTESIAN_POINT ( 'NONE',  ( -40.69416551809789695, 490.1135946711737006, 11.28307282940560086 ) ) ;
#71930 = DIRECTION ( 'NONE',  ( 0.000000000000000000, 0.000000000000000000, -1.000000000000000000 ) ) ;
#71931 = DIRECTION ( 'NONE',  ( -1.000000000000000000, -0.000000000000000000, -0.000000000000000000 ) ) ;
#71932 = CARTESIAN_POINT ( 'NONE',  ( 4.650141638649412990, 52.18144075392523717, 6.194407870437166785 ) ) ;
#71933 = APPLICATION_PROTOCOL_DEFINITION ( 'draft international standard', 'automotive_design', 1998, #47261 ) ;
#71934 = CARTESIAN_POINT ( 'NONE',  ( -12.24528424494010714, -5.249243268855193989, 20.21143042290738734 ) ) ;
#71935 = EDGE_LOOP ( 'NONE', ( #67077, #1553, #14202, #31541, #21262, #66174 ) ) ;
#71936 = CARTESIAN_POINT ( 'NONE',  ( -4.955398898941148822, -46.70857795648188926, 40.29592611768291022 ) ) ;
#71937 = CARTESIAN_POINT ( 'NONE',  ( -1.404490565849160877, 15.46725112412266334, 9.926810856659404436 ) ) ;
#71938 = VECTOR ( 'NONE', #47083, 1000.000000000000000 ) ;
#71939 = CARTESIAN_POINT ( 'NONE',  ( -39.83065760000179267, 436.5763539059782374, 5.509783410167077733 ) ) ;
#71940 = CARTESIAN_POINT ( 'NONE',  ( -43.99399868446376871, 464.5851102538602504, 10.32278593049915649 ) ) ;
#71941 = CARTESIAN_POINT ( 'NONE',  ( -81.07140313541336241, -30.00000000000001421, 140.4064320514307553 ) ) ;
#71942 =( BOUNDED_SURFACE ( )  B_SPLINE_SURFACE ( 3, 2, ( 
 ( #89894, #58048, #25190 ),
 ( #67229, #82328, #24655 ),
 ( #32207, #41339, #57507 ),
 ( #836, #99027, #25745 ),
 ( #26271, #33807, #66685 ),
 ( #99566, #9487, #17081 ),
 ( #42398, #75293, #16533 ),
 ( #82866, #59134, #73154 ),
 ( #90430, #92016, #49958 ),
 ( #91503, #56980, #65085 ) ),
 .UNSPECIFIED., .F., .F., .F. ) 
 B_SPLINE_SURFACE_WITH_KNOTS ( ( 4, 2, 2, 2, 4 ),
 ( 3, 3 ),
 ( 0.007286154432480726126, 0.008335500519281571763, 0.009384846606082415665, 0.01043419269288325957, 0.01148353877968410347 ),
 ( 0.1485529662656749350, 1.000000000000000000 ),
 .UNSPECIFIED. ) 
 GEOMETRIC_REPRESENTATION_ITEM ( )  RATIONAL_B_SPLINE_SURFACE ( (
 ( 0.9428520994613440731, 0.8076514324310039017, 1.000000000000000000),
 ( 0.9457545067941961481, 0.8174203633578406292, 1.000000000000000000),
 ( 0.9476060023041493752, 0.8236521322564903658, 1.000000000000000000),
 ( 0.9488932852697182785, 0.8279848729547364394, 1.000000000000000000),
 ( 0.9483224819758968582, 0.8260636615909705549, 1.000000000000000000),
 ( 0.9449873596068385506, 0.8148382971539733788, 1.000000000000000000),
 ( 0.9422359404858332566, 0.8055775627836994079, 1.000000000000000000),
 ( 0.9351232435981660096, 0.7816376271955178812, 1.000000000000000000),
 ( 0.9307673920762341568, 0.7669766896476877260, 1.000000000000000000),
 ( 0.9259068126999906445, 0.7506169376399400850, 1.000000000000000000) ) ) 
 REPRESENTATION_ITEM ( '' )  SURFACE ( )  );
#71943 = CARTESIAN_POINT ( 'NONE',  ( 5.500000000000007994, 42.00000000000000000, -71.41947339647144588 ) ) ;
#71944 = VERTEX_POINT ( 'NONE', #42958 ) ;
#71945 = CARTESIAN_POINT ( 'NONE',  ( -1.469576158976823947E-15, -10.06250000409677092, 8.000000000000000000 ) ) ;
#71946 = CARTESIAN_POINT ( 'NONE',  ( 106.7290742229372853, -57.65299249569456208, 200.3188922580204689 ) ) ;
#71947 = CARTESIAN_POINT ( 'NONE',  ( 60.63806777930422243, -34.58949756339826820, -25.09002054893269573 ) ) ;
#71948 = TOROIDAL_SURFACE ( 'NONE', #70254, 8.500000000000000000, 0.5000000000000000000 ) ;
#71949 = CARTESIAN_POINT ( 'NONE',  ( -80.00000000000000000, -60.00000000000000000, -21.09707704303352926 ) ) ;
#71950 = CARTESIAN_POINT ( 'NONE',  ( -16.14327244186403476, 20.71081664949755918, 4.173128809987454169 ) ) ;
#71951 = CARTESIAN_POINT ( 'NONE',  ( 39.04923757959249286, 40.83906611472210102, 52.30342408726538395 ) ) ;
#71952 = CARTESIAN_POINT ( 'NONE',  ( -73.64776945840979749, -60.00000000000000711, 168.6562425123320565 ) ) ;
#71953 = CARTESIAN_POINT ( 'NONE',  ( -27.47093694407817210, 296.2799286419132727, -9.692114557243211692 ) ) ;
#71954 = DIRECTION ( 'NONE',  ( 0.000000000000000000, 0.000000000000000000, -1.000000000000000000 ) ) ;
#71955 = EDGE_CURVE ( 'NONE', #71499, #13645, #67160, .T. ) ;
#71956 = CARTESIAN_POINT ( 'NONE',  ( 55.22048556082879145, 50.00000000002004441, 34.80214219306057544 ) ) ;
#71957 = COLOUR_RGB ( '', 0.40784314, 0.44705882, 0.49803922) ;
#71958 = CARTESIAN_POINT ( 'NONE',  ( -84.39490293580904279, -57.45156777692785965, 191.2983715192742409 ) ) ;
#71959 = ORIENTED_EDGE ( 'NONE', *, *, #42428, .F. ) ;
#71960 = CARTESIAN_POINT ( 'NONE',  ( 36.68219968559907329, 426.6315103464384038, 5.464024069355958524 ) ) ;
#71961 = VERTEX_POINT ( 'NONE', #34898 ) ;
#71962 = LINE ( 'NONE', #31534, #21587 ) ;
#71963 = CARTESIAN_POINT ( 'NONE',  ( -28.97859824875257218, 308.1531040660597682, -9.025514053728203478 ) ) ;
#71964 = CARTESIAN_POINT ( 'NONE',  ( 41.74356089131816816, 489.2821409585033621, 10.50625248545157753 ) ) ;
#71965 = CARTESIAN_POINT ( 'NONE',  ( -42.99999999999998579, 464.8825480873695710, 15.07585856869430607 ) ) ;
#71966 = DIRECTION ( 'NONE',  ( 0.000000000000000000, -1.000000000000000000, 0.000000000000000000 ) ) ;
#71967 = AXIS2_PLACEMENT_3D ( 'NONE', #53284, #2588, #60855 ) ;
#71968 = EDGE_LOOP ( 'NONE', ( #70230, #80000, #53799, #38716, #22792 ) ) ;
#71969 = AXIS2_PLACEMENT_3D ( 'NONE', #21085, #37259, #37793 ) ;
#71970 = FACE_OUTER_BOUND ( 'NONE', #50845, .T. ) ;
#71971 = CARTESIAN_POINT ( 'NONE',  ( 10.03941004420479466, 13.75456597456546781, 10.52769693539611495 ) ) ;
#71972 = CARTESIAN_POINT ( 'NONE',  ( 17.78317311657530553, -8.673617379884035472E-16, -13.66642973271117256 ) ) ;
#71973 = CARTESIAN_POINT ( 'NONE',  ( -33.70841932975964284, 485.0774894644218875, 1.934193826885682199 ) ) ;
#71974 = CARTESIAN_POINT ( 'NONE',  ( 65.67877680238373728, -29.99999999999995026, -31.25179767064105363 ) ) ;
#71975 = CARTESIAN_POINT ( 'NONE',  ( -81.42972324512007276, -18.68455707043344205, 133.0837277777090435 ) ) ;
#71976 = VERTEX_POINT ( 'NONE', #19274 ) ;
#71977 = CARTESIAN_POINT ( 'NONE',  ( 17.10696384799877379, -59.99999999999999289, 42.25337809451749393 ) ) ;
#71978 = CARTESIAN_POINT ( 'NONE',  ( 72.25192046840727755, -57.67049155165763352, 174.5922148356693810 ) ) ;
#71979 = VECTOR ( 'NONE', #100736, 1000.000000000000000 ) ;
#71980 = CARTESIAN_POINT ( 'NONE',  ( 27.61650669486618881, 1.474610560812782335E-15, 0.000000000000000000 ) ) ;
#71981 = CARTESIAN_POINT ( 'NONE',  ( 39.15257853886765105, 311.4970519361567654, 1.970299295586781962 ) ) ;
#71982 = CARTESIAN_POINT ( 'NONE',  ( -13.09726150444772053, 8.332934222693051396, 8.848836478249873849 ) ) ;
#71983 = ORIENTED_EDGE ( 'NONE', *, *, #1490, .F. ) ;
#71984 = DIRECTION ( 'NONE',  ( 1.000000000000000000, 1.224606353822377258E-16, 0.000000000000000000 ) ) ;
#71985 = DIRECTION ( 'NONE',  ( 0.000000000000000000, -1.000000000000000000, 0.000000000000000000 ) ) ;
#71987 = CARTESIAN_POINT ( 'NONE',  ( -101.8255872164643989, -52.71004081795416596, 134.8513848411543279 ) ) ;
#71986 = CARTESIAN_POINT ( 'NONE',  ( -16.11174065067163852, 37.20923313995303516, 21.98001889856140068 ) ) ;
#71988 = CARTESIAN_POINT ( 'NONE',  ( 5.082755093536324154, -20.84375000204838813, 5.082755093536326818 ) ) ;
#71989 = CARTESIAN_POINT ( 'NONE',  ( 43.09948196127356823, 484.9577458347779384, -0.8563396247094318126 ) ) ;
#71990 = CARTESIAN_POINT ( 'NONE',  ( 0.000000000000000000, 0.000000000000000000, 9.500000000000000000 ) ) ;
#71991 = CARTESIAN_POINT ( 'NONE',  ( 0.8412457115897011839, 34.28465343340348426, 29.42821019032353291 ) ) ;
#71992 = CARTESIAN_POINT ( 'NONE',  ( 67.22793774957824553, 6.975173280561618775E-15, 0.000000000000000000 ) ) ;
#71993 = DIRECTION ( 'NONE',  ( 0.000000000000000000, 0.000000000000000000, 1.000000000000000000 ) ) ;
#71994 = TOROIDAL_SURFACE ( 'NONE', #25537, 10.00000000000000000, 4.000000000000000000 ) ;
#71995 = ORIENTED_EDGE ( 'NONE', *, *, #67384, .T. ) ;
#71996 = EDGE_CURVE ( 'NONE', #26262, #57008, #94167, .T. ) ;
#71997 = CARTESIAN_POINT ( 'NONE',  ( 43.75401118688384372, 486.3173572309546557, 5.908089951475091084 ) ) ;
#71999 = CARTESIAN_POINT ( 'NONE',  ( 28.67944596121853706, -56.86006578928314070, 35.73029098294846051 ) ) ;
#71998 = CARTESIAN_POINT ( 'NONE',  ( -34.32536616635837845, -30.00000000000003553, 42.48815186199111338 ) ) ;
#72000 = CARTESIAN_POINT ( 'NONE',  ( 23.86089617542257457, 27.29447341560884510, -33.04113357524870054 ) ) ;
#72001 = VERTEX_POINT ( 'NONE', #27888 ) ;
#72002 = EDGE_CURVE ( 'NONE', #87076, #12223, #106731, .T. ) ;
#72003 = AXIS2_PLACEMENT_3D ( 'NONE', #53564, #4481, #44415 ) ;
#72004 = UNCERTAINTY_MEASURE_WITH_UNIT (LENGTH_MEASURE( 1.000000000000000082E-05 ), #64316, 'distance_accuracy_value', 'NONE');
#72005 = ORIENTED_EDGE ( 'NONE', *, *, #26050, .T. ) ;
#72007 = DIRECTION ( 'NONE',  ( 0.000000000000000000, -0.000000000000000000, -1.000000000000000000 ) ) ;
#72006 = CARTESIAN_POINT ( 'NONE',  ( 41.08349330513380693, -4.000000000000000888, 4.898587196589416773E-16 ) ) ;
#72008 = CARTESIAN_POINT ( 'NONE',  ( 91.95555555555554861, 4.172000000000019249, 0.000000000000000000 ) ) ;
#72009 = CARTESIAN_POINT ( 'NONE',  ( -43.54570344706581153, 464.5919001249989719, 9.427857144823894586 ) ) ;
#72010 = CARTESIAN_POINT ( 'NONE',  ( -1.469576158976823947E-15, -19.06250000409677270, 8.000000000000000000 ) ) ;
#72011 = CARTESIAN_POINT ( 'NONE',  ( 5.385673916453011856, 3.157894736842104866, 14.66382285868950675 ) ) ;
#72013 = VERTEX_POINT ( 'NONE', #10576 ) ;
#72012 = AXIS2_PLACEMENT_3D ( 'NONE', #59829, #52241, #84624 ) ;
#72014 = CARTESIAN_POINT ( 'NONE',  ( 48.62243493482748846, -60.00000000000000711, -38.17079728251586346 ) ) ;
#72015 = CARTESIAN_POINT ( 'NONE',  ( 88.69399320309210566, -29.99999999999992539, 188.2041074686423485 ) ) ;
#72016 = DIRECTION ( 'NONE',  ( -0.8191520442889884679, 1.003171929053520679E-16, 0.5735764363510508224 ) ) ;
#72017 = EDGE_CURVE ( 'NONE', #56114, #88353, #56819, .T. ) ;
#72018 = FACE_OUTER_BOUND ( 'NONE', #7479, .T. ) ;
#72019 = ADVANCED_FACE ( 'NONE', ( #45626 ), #43566, .F. ) ;
#72020 = CARTESIAN_POINT ( 'NONE',  ( 0.000000000000000000, -99.99999999999997158, 6.000000000000000888 ) ) ;
#72021 = VERTEX_POINT ( 'NONE', #103840 ) ;
#72022 = ORIENTED_EDGE ( 'NONE', *, *, #35413, .F. ) ;
#72024 = EDGE_CURVE ( 'NONE', #90625, #75208, #13227, .T. ) ;
#72023 = AXIS2_PLACEMENT_3D ( 'NONE', #57330, #25010, #58955 ) ;
#72025 = VERTEX_POINT ( 'NONE', #5678 ) ;
#72026 = FACE_OUTER_BOUND ( 'NONE', #87449, .T. ) ;
#72027 = CARTESIAN_POINT ( 'NONE',  ( 44.12472801211155371, 485.7238370326410859, 3.975897585125152123 ) ) ;
#72028 = CARTESIAN_POINT ( 'NONE',  ( -37.24606932108090973, 27.99441749650426559, 10.98714381882859215 ) ) ;
#72029 = CYLINDRICAL_SURFACE ( 'NONE', #103414, 4.000000000000000888 ) ;
#72030 = CARTESIAN_POINT ( 'NONE',  ( -36.56870781681114835, 337.1622652273130711, -1.695314226153411763 ) ) ;
#72031 = CARTESIAN_POINT ( 'NONE',  ( 37.56673239365841255, -1.200000000000000030E-05, -12.20617127781092215 ) ) ;
#72032 = CARTESIAN_POINT ( 'NONE',  ( -46.00000000000000000, 486.2666530176200581, 2.948218630481520997 ) ) ;
#72033 = LINE ( 'NONE', #96848, #58777 ) ;
#72034 = CIRCLE ( 'NONE', #53007, 4.000000000000007105 ) ;
#72035 = ORIENTED_EDGE ( 'NONE', *, *, #85149, .F. ) ;
#72036 = CARTESIAN_POINT ( 'NONE',  ( 1.308996937480704004, 49.99999999999999289, -75.00000000000001421 ) ) ;
#72037 = ORIENTED_EDGE ( 'NONE', *, *, #13511, .F. ) ;
#72038 = CARTESIAN_POINT ( 'NONE',  ( 43.10000000000000142, 1.533819458162526451E-15, 0.000000000000000000 ) ) ;
#72039 = CARTESIAN_POINT ( 'NONE',  ( -39.14057804813676000, 485.8491723118624463, -4.975388520154326422 ) ) ;
#72040 = AXIS2_PLACEMENT_3D ( 'NONE', #74477, #51262, #17336 ) ;
#72041 = CARTESIAN_POINT ( 'NONE',  ( 4.023876337984799711, 300.5161520203807299, -10.00978828653755315 ) ) ;
#72042 = CARTESIAN_POINT ( 'NONE',  ( 63.30499805623622223, -29.05601916271744756, 76.03110060700105066 ) ) ;
#72043 = AXIS2_PLACEMENT_3D ( 'NONE', #54521, #71257, #102033 ) ;
#72044 = ORIENTED_EDGE ( 'NONE', *, *, #72686, .F. ) ;
#72045 = DIRECTION ( 'NONE',  ( 1.000000000000000000, 1.224606353822377258E-16, 0.000000000000000000 ) ) ;
#72046 = CARTESIAN_POINT ( 'NONE',  ( -1.320432766682874540E-15, -28.53125000204838813, 7.188101187500000044 ) ) ;
#72047 = ORIENTED_EDGE ( 'NONE', *, *, #40524, .T. ) ;
#72048 =( LENGTH_UNIT ( ) NAMED_UNIT ( * ) SI_UNIT ( .MILLI., .METRE. ) );
#72049 = CIRCLE ( 'NONE', #11677, 1.000000000000000000 ) ;
#72050 = AXIS2_PLACEMENT_3D ( 'NONE', #9084, #24776, #92134 ) ;
#72051 = AXIS2_PLACEMENT_3D ( 'NONE', #70913, #7223, #104328 ) ;
#72052 = VECTOR ( 'NONE', #79198, 1000.000000000000000 ) ;
#72053 = FACE_OUTER_BOUND ( 'NONE', #51854, .T. ) ;
#72054 = ADVANCED_FACE ( 'NONE', ( #87677 ), #13725, .T. ) ;
#72055 = CARTESIAN_POINT ( 'NONE',  ( -3.313708498984765161, -28.15625000409677270, 7.999999999999998224 ) ) ;
#72056 = VECTOR ( 'NONE', #45537, 1000.000000000000000 ) ;
#72057 = CARTESIAN_POINT ( 'NONE',  ( 86.95935682309162473, -39.09230861363683118, 189.0019964014885261 ) ) ;
#72058 = PRESENTATION_STYLE_ASSIGNMENT (( #39177 ) ) ;
#72059 = CARTESIAN_POINT ( 'NONE',  ( -5.057453041531906557, 6.382334271672433168, 5.000000000000000000 ) ) ;
#72060 = CARTESIAN_POINT ( 'NONE',  ( 13.27219118062621561, 304.5542594574499162, 9.873754632660967090 ) ) ;
#72061 = ORIENTED_EDGE ( 'NONE', *, *, #16176, .T. ) ;
#72062 = CARTESIAN_POINT ( 'NONE',  ( 9.349999999999997868, 1.533819458162526451E-15, 0.000000000000000000 ) ) ;
#72063 = DIRECTION ( 'NONE',  ( 0.000000000000000000, -1.000000000000000000, 0.000000000000000000 ) ) ;
#72064 = CARTESIAN_POINT ( 'NONE',  ( 30.54863829050838220, -60.00000000000000000, 43.31763207389616355 ) ) ;
#72065 = CARTESIAN_POINT ( 'NONE',  ( -100.3740574807695651, -30.00000000000000355, 157.7342760147397769 ) ) ;
#72066 = DIRECTION ( 'NONE',  ( 0.000000000000000000, 0.000000000000000000, 1.000000000000000000 ) ) ;
#72067 = CARTESIAN_POINT ( 'NONE',  ( 35.88008981787920959, -57.69592402444057200, 50.07942547625698637 ) ) ;
#72069 = FACE_OUTER_BOUND ( 'NONE', #84620, .T. ) ;
#72068 = CARTESIAN_POINT ( 'NONE',  ( -9.482856158761299170, 247.5569288414526739, 3.177891129109637891 ) ) ;
#72070 = STYLED_ITEM ( 'NONE', ( #4638 ), #42818 ) ;
#72071 = PLANE ( 'NONE',  #105705 ) ;
#72072 = CARTESIAN_POINT ( 'NONE',  ( -30.00000000000000711, 464.1495552126472148, 11.87789752000373156 ) ) ;
#72073 = DIRECTION ( 'NONE',  ( 0.000000000000000000, 0.000000000000000000, 1.000000000000000000 ) ) ;
#72074 = B_SPLINE_CURVE_WITH_KNOTS ( 'NONE', 3,
 ( #8416, #66124, #91482, #16511 ),
 .UNSPECIFIED., .F., .F.,
 ( 4, 4 ),
 ( 2.069507657746056223E-16, 0.001795780652478906267 ),
 .UNSPECIFIED. ) ;
#72075 = CARTESIAN_POINT ( 'NONE',  ( -20.85295009280099876, -60.00000000000000000, 40.33826634902553110 ) ) ;
#72076 = CARTESIAN_POINT ( 'NONE',  ( 0.8750000000000039968, -70.58759490697437400, 13.02737050516259210 ) ) ;
#72077 = PRESENTATION_LAYER_ASSIGNMENT (  '', '', ( #11788 ) ) ;
#72078 = EDGE_CURVE ( 'NONE', #21912, #67484, #72308, .T. ) ;
#72079 = CARTESIAN_POINT ( 'NONE',  ( -86.36538439990067673, -61.02622103470842774, 194.5654814187428201 ) ) ;
#72080 = ORIENTED_EDGE ( 'NONE', *, *, #34197, .T. ) ;
#72081 = CARTESIAN_POINT ( 'NONE',  ( 17.50000000000003908, 51.99573851567223670, 60.30773471722763190 ) ) ;
#72082 = CARTESIAN_POINT ( 'NONE',  ( -12.62263043180945665, -56.88413384736368528, 33.43217295346193652 ) ) ;
#72083 = EDGE_CURVE ( 'NONE', #81954, #30642, #58558, .T. ) ;
#72085 = CARTESIAN_POINT ( 'NONE',  ( 39.33042632267689953, 460.7392826591629387, 2.124562382290182239 ) ) ;
#72084 = DIRECTION ( 'NONE',  ( 0.5735764363510557073, -0.8191520442889850262, 1.003171929053516612E-16 ) ) ;
#72086 = ORIENTED_EDGE ( 'NONE', *, *, #75675, .T. ) ;
#72087 = CARTESIAN_POINT ( 'NONE',  ( 25.97942814979532145, 35.07822400896434090, 8.256891463089578664 ) ) ;
#72088 = CARTESIAN_POINT ( 'NONE',  ( -7.498343863768531570, -2.970317092013120774, -20.23009517154971348 ) ) ;
#72089 = CARTESIAN_POINT ( 'NONE',  ( 43.63930228698950486, 486.5321682126036080, 6.480714085081864972 ) ) ;
#72090 = CARTESIAN_POINT ( 'NONE',  ( 7.500000000000006217, 39.99999999999942446, -59.88032989331673406 ) ) ;
#72091 =( BOUNDED_SURFACE ( )  B_SPLINE_SURFACE ( 3, 2, ( 
 ( #50044, #73242, #90511 ),
 ( #48446, #49514, #7448 ),
 ( #106146, #16087, #66230 ),
 ( #25836, #81864, #65712 ) ),
 .UNSPECIFIED., .F., .F., .F. ) 
 B_SPLINE_SURFACE_WITH_KNOTS ( ( 4, 4 ),
 ( 3, 3 ),
 ( 1.084202172485504434E-17, 0.0008582108274410138026 ),
 ( 0.000000000000000000, 1.000000000000000000 ),
 .UNSPECIFIED. ) 
 GEOMETRIC_REPRESENTATION_ITEM ( )  RATIONAL_B_SPLINE_SURFACE ( (
 ( 1.000000000000000000, 0.7409272757993169423, 1.000000000000000000),
 ( 1.000000000000000000, 0.7386644886093517437, 1.000000000000000000),
 ( 1.000000000000000000, 0.7359402037277118502, 1.000000000000000000),
 ( 1.000000000000000000, 0.7328671738315170048, 1.000000000000000000) ) ) 
 REPRESENTATION_ITEM ( '' )  SURFACE ( )  );
#72092 = CARTESIAN_POINT ( 'NONE',  ( 42.19179521601818550, 484.5286692029256983, -4.078961064719028862 ) ) ;
#72093 = CARTESIAN_POINT ( 'NONE',  ( 69.82668593885752273, -59.99999999999998579, 140.4683949244069368 ) ) ;
#72094 = CARTESIAN_POINT ( 'NONE',  ( -7.199040112754230057E-19, 54.30758622938872549, -7.749999999999999112 ) ) ;
#72095 = EDGE_LOOP ( 'NONE', ( #97827, #82214, #81437, #44234 ) ) ;
#72096 = DIRECTION ( 'NONE',  ( -1.000000000000000000, 0.000000000000000000, 0.000000000000000000 ) ) ;
#72097 = CARTESIAN_POINT ( 'NONE',  ( -8.000000000000000000, -21.03125000409677625, -3.313708498984762496 ) ) ;
#72098 = CONICAL_SURFACE ( 'NONE', #85913, 4.172000000000009479, 0.9599310885968813656 ) ;
#72100 = DIRECTION ( 'NONE',  ( -1.000000000000000000, -0.000000000000000000, -0.000000000000000000 ) ) ;
#72099 = CARTESIAN_POINT ( 'NONE',  ( 34.32456002071940304, -30.00000000000004263, 42.48759634994703305 ) ) ;
#72101 = LINE ( 'NONE', #72628, #7915 ) ;
#72102 = CARTESIAN_POINT ( 'NONE',  ( -5.374793246923815992, -2.224716758540647099, 104.0614974883207111 ) ) ;
#72103 = EDGE_LOOP ( 'NONE', ( #31905, #102505, #46774, #83893, #101098, #63074 ) ) ;
#72104 = EDGE_CURVE ( 'NONE', #21876, #75344, #53393, .T. ) ;
#72105 = CARTESIAN_POINT ( 'NONE',  ( -23.79050601098939310, 306.1176470301992367, 9.215821030969554073 ) ) ;
#72106 = ORIENTED_EDGE ( 'NONE', *, *, #80421, .T. ) ;
#72107 = CARTESIAN_POINT ( 'NONE',  ( 0.000000000000000000, 0.000000000000000000, 0.000000000000000000 ) ) ;
#72108 = CARTESIAN_POINT ( 'NONE',  ( 43.00000000000000000, 450.0000000000002274, 25.20242257375371864 ) ) ;
#72109 = DIRECTION ( 'NONE',  ( 0.000000000000000000, 0.000000000000000000, 1.000000000000000000 ) ) ;
#72110 = ORIENTED_EDGE ( 'NONE', *, *, #3335, .T. ) ;
#72111 = CARTESIAN_POINT ( 'NONE',  ( 4.852941176470595863, -5.000000000000002665, -70.80672828634229177 ) ) ;
#72112 = CARTESIAN_POINT ( 'NONE',  ( 5.000000000000000000, -13.82147230827996331, 10.98112731479300308 ) ) ;
#72113 = CARTESIAN_POINT ( 'NONE',  ( -109.9238538444930526, -59.99999999999752021, 197.0382354099203610 ) ) ;
#72114 = DIRECTION ( 'NONE',  ( -1.000000000000000000, -1.224606353822377258E-16, -0.000000000000000000 ) ) ;
#72115 = CARTESIAN_POINT ( 'NONE',  ( 83.40983118009236819, -59.99999999999992895, 199.1200332089420044 ) ) ;
#72116 = LINE ( 'NONE', #42266, #6366 ) ;
#72117 = FACE_OUTER_BOUND ( 'NONE', #84070, .T. ) ;
#72118 = PRESENTATION_LAYER_ASSIGNMENT (  '', '', ( #97909 ) ) ;
#72120 = CARTESIAN_POINT ( 'NONE',  ( 12.53354992101991883, -49.91574432760546642, 32.26800626715709086 ) ) ;
#72119 = CARTESIAN_POINT ( 'NONE',  ( -106.4002951517535536, -14.21045842199431242, 159.7122570458138284 ) ) ;
#72121 = CARTESIAN_POINT ( 'NONE',  ( 95.03805679281244068, -38.00000000000000000, 107.7969437180587136 ) ) ;
#72122 = SURFACE_STYLE_USAGE ( .BOTH. , #55905 ) ;
#72123 = CARTESIAN_POINT ( 'NONE',  ( -44.27417758264619607, -56.80246321600215964, 47.31014526494450934 ) ) ;
#72124 = CARTESIAN_POINT ( 'NONE',  ( 13.50000000000000355, 7.794228634059934713, -13.00000000000000000 ) ) ;
#72125 = ORIENTED_EDGE ( 'NONE', *, *, #28770, .T. ) ;
#72126 =( NAMED_UNIT ( * ) SI_UNIT ( $, .STERADIAN. ) SOLID_ANGLE_UNIT ( ) );
#72127 = PRESENTATION_LAYER_ASSIGNMENT (  '', '', ( #91086 ) ) ;
#72128 = CARTESIAN_POINT ( 'NONE',  ( -10.00000000000000355, 30.00000000000000000, 4.000000000000000000 ) ) ;
#72129 = CARTESIAN_POINT ( 'NONE',  ( -1.235494359605229464, 15.32027490366484201, 50.72593522979114766 ) ) ;
#72130 = PRESENTATION_STYLE_ASSIGNMENT (( #73167 ) ) ;
#72131 = CARTESIAN_POINT ( 'NONE',  ( 3.389930600490795420, 303.8518027742030085, -9.999999999492535707 ) ) ;
#72132 = DIRECTION ( 'NONE',  ( 0.000000000000000000, -1.000000000000000000, 0.000000000000000000 ) ) ;
#72133 = EDGE_LOOP ( 'NONE', ( #43545, #50468, #88856, #100892 ) ) ;
#72134 = CARTESIAN_POINT ( 'NONE',  ( -9.475162301762221517, -11.83642075861501830, 9.220471602222437113 ) ) ;
#72135 = ORIENTED_EDGE ( 'NONE', *, *, #90324, .F. ) ;
#72136 = CARTESIAN_POINT ( 'NONE',  ( 107.2611508641872859, -29.99999999998129852, 190.9996382533202279 ) ) ;
#72137 = CARTESIAN_POINT ( 'NONE',  ( 6.503370466877179012, 41.93912984867880311, -59.84719185825785104 ) ) ;
#72138 = ADVANCED_FACE ( 'NONE', ( #29985 ), #70574, .T. ) ;
#72139 = CARTESIAN_POINT ( 'NONE',  ( 88.61328692016215314, -29.99999999999999289, 80.34149805594043414 ) ) ;
#72140 = EDGE_CURVE ( 'NONE', #74912, #63111, #79182, .T. ) ;
#72141 = LINE ( 'NONE', #95364, #79366 ) ;
#72142 = ORIENTED_EDGE ( 'NONE', *, *, #59427, .T. ) ;
#72143 = B_SPLINE_CURVE_WITH_KNOTS ( 'NONE', 3,
 ( #55988, #55468, #15018, #80281, #87343, #88928, #70622, #5864, #104031, #94915, #47387, #47910, #21052, #37757, #72209, #70086, #31252, #71140, #53889, #63607, #102990, #103511, #30172, #6392, #29664, #54398, #38789, #86819, #12891, #45817, #96492, #63063, #95962, #78688, #13420, #46344, #79233, #71660, #105110, #104565, #5360, #22087, #54942, #87869, #13954, #79759, #30720, #88402, #89463, #24741, #15554, #7992, #40363, #89982, #396, #40901, #99664, #48966, #106686, #33363, #98595, #50561, #32833, #66775, #32301, #25280, #81338, #17174 ),
 .UNSPECIFIED., .F., .F.,
 ( 4, 2, 2, 2, 2, 2, 2, 2, 2, 2, 2, 2, 2, 2, 2, 2, 2, 2, 2, 2, 2, 2, 2, 2, 2, 2, 2, 2, 2, 2, 2, 2, 2, 4 ),
 ( 0.01355025249921910056, 0.01436585972314286322, 0.01518146694706662414, 0.01681268139491414251, 0.01844389584276166089, 0.02007511029060918273, 0.02333753918630421947, 0.02659996808199925622, 0.02986239697769429297, 0.03312482587338932971, 0.03964968366477939626, 0.05269939924755953631, 0.06574911483033968329, 0.07879883041311983027, 0.09184854599589996338, 0.1179479771614602573, 0.1440474083270205652, 0.1570971239098006844, 0.1701468394925808314, 0.1831965550753610061, 0.1897214128667510658, 0.1962462706581411254, 0.2027711284495312127, 0.2092959862409213001, 0.2125584151366162744, 0.2158208440323112765, 0.2174520584801587497, 0.2182676657040824864, 0.2190832729280062230, 0.2194910765399680774, 0.2198988801519299319, 0.2207144873758536130, 0.2215300945997772664, 0.2223457018237009197 ),
 .UNSPECIFIED. ) ;
#72144 = ORIENTED_EDGE ( 'NONE', *, *, #49584, .F. ) ;
#72145 = ORIENTED_EDGE ( 'NONE', *, *, #13911, .T. ) ;
#72147 = AXIS2_PLACEMENT_3D ( 'NONE', #14465, #32291, #6383 ) ;
#72146 = DIRECTION ( 'NONE',  ( 0.000000000000000000, 1.000000000000000000, 0.000000000000000000 ) ) ;
#72148 = CARTESIAN_POINT ( 'NONE',  ( 31.36650669486618881, 4.898587196589411843E-16, -4.000000000000000888 ) ) ;
#72149 = EDGE_CURVE ( 'NONE', #14152, #2234, #32704, .T. ) ;
#72150 = DIRECTION ( 'NONE',  ( -1.000000000000000000, -1.224606353822377258E-16, -0.000000000000000000 ) ) ;
#72152 = EDGE_LOOP ( 'NONE', ( #88571, #15804, #12455 ) ) ;
#72151 = VECTOR ( 'NONE', #25497, 1000.000000000000000 ) ;
#72153 = CARTESIAN_POINT ( 'NONE',  ( -16.04705908622477750, 4.602417526221017852, 3.432813300977638704 ) ) ;
#72154 = AXIS2_PLACEMENT_3D ( 'NONE', #30984, #12623, #62280 ) ;
#72155 = EDGE_LOOP ( 'NONE', ( #89818, #19718, #99294, #16496, #33618, #64602 ) ) ;
#72156 = DIRECTION ( 'NONE',  ( 1.000000000000000000, 0.000000000000000000, 0.000000000000000000 ) ) ;
#72157 = CARTESIAN_POINT ( 'NONE',  ( 80.09828699751943759, -38.78935091380522238, 193.1656444472805845 ) ) ;
#72158 = CARTESIAN_POINT ( 'NONE',  ( 11.45735263127505021, 9.453390557368402725, 9.374188611738238919 ) ) ;
#72159 = CARTESIAN_POINT ( 'NONE',  ( 86.69934304271014014, -60.14804486455665256, -0.3912972893063921820 ) ) ;
#72160 = CARTESIAN_POINT ( 'NONE',  ( 85.13988909840620067, -38.00000000000004974, 183.5158871499416477 ) ) ;
#72161 = CARTESIAN_POINT ( 'NONE',  ( 36.57269729962153093, 309.7540319447825823, 13.50089482657587503 ) ) ;
#72162 = CARTESIAN_POINT ( 'NONE',  ( 42.36162206505731831, 485.1874691988857649, -2.398526663486076238 ) ) ;
#72163 =( REPRESENTATION_RELATIONSHIP ('NONE','NONE', #69581, #62661 ) REPRESENTATION_RELATIONSHIP_WITH_TRANSFORMATION ( #36825 )SHAPE_REPRESENTATION_RELATIONSHIP( ) );
#72164 = AXIS2_PLACEMENT_3D ( 'NONE', #46383, #41331, #81769 ) ;
#72165 = DIRECTION ( 'NONE',  ( 0.000000000000000000, -1.000000000000000000, 0.000000000000000000 ) ) ;
#72166 = CARTESIAN_POINT ( 'NONE',  ( -38.51502786940058343, 460.0233756673464427, 2.043034587342845043 ) ) ;
#72167 = FACE_OUTER_BOUND ( 'NONE', #26172, .T. ) ;
#72168 = ORIENTED_EDGE ( 'NONE', *, *, #43077, .T. ) ;
#72169 = DIRECTION ( 'NONE',  ( 0.000000000000000000, -1.000000000000000000, 0.000000000000000000 ) ) ;
#72170 = CARTESIAN_POINT ( 'NONE',  ( -35.57320956138945434, 461.3653195830025311, 3.400055647391269087 ) ) ;
#72171 = CARTESIAN_POINT ( 'NONE',  ( -4.036663395287809486, 14.45006652701215977, 4.999999999999999112 ) ) ;
#72172 = ORIENTED_EDGE ( 'NONE', *, *, #31899, .F. ) ;
#72173 = CARTESIAN_POINT ( 'NONE',  ( -35.48605273723305942, 424.7888819862658352, 6.350197726503093776 ) ) ;
#72174 = AXIS2_PLACEMENT_3D ( 'NONE', #50795, #1166, #57827 ) ;
#72175 = CARTESIAN_POINT ( 'NONE',  ( -25.99191122786077557, 305.5540186273516383, 10.54636674004932395 ) ) ;
#72176 = CARTESIAN_POINT ( 'NONE',  ( 0.000000000000000000, 152.0000000000000000, 5.000000000000000000 ) ) ;
#72177 = UNCERTAINTY_MEASURE_WITH_UNIT (LENGTH_MEASURE( 1.000000000000000082E-05 ), #23153, 'distance_accuracy_value', 'NONE');
#72178 = CARTESIAN_POINT ( 'NONE',  ( 8.866506694866188809, 1.474610560812782335E-15, 0.000000000000000000 ) ) ;
#72179 = CARTESIAN_POINT ( 'NONE',  ( 4.898587196589412829E-16, -16.62499999999999289, -8.000000000000000000 ) ) ;
#72180 = CARTESIAN_POINT ( 'NONE',  ( 102.9313392694734688, 1.016364837396684119E-14, 0.000000000000000000 ) ) ;
#72181 = CLOSED_SHELL ( 'NONE', ( #15930, #80288, #86480, #25413, #59080, #74710, #63990, #52429, #84035, #82163, #33406, #19825, #19983, #38645, #64185, #32877, #99983, #28445, #65649, #40506, #28689, #98436, #78853, #50726, #67279, #59846, #637, #72819, #29848, #48707, #59269, #10012, #89573, #42205, #33736, #12436, #100563, #30650, #102283, #51795, #30111, #55430, #74929, #65838, #69432, #19602, #105482, #34362, #53583, #1907, #40448, #63551, #20943, #46250, #98311, #21784 ) ) ;
#72182 = EDGE_CURVE ( 'NONE', #88153, #62246, #101598, .T. ) ;
#72184 = MECHANICAL_DESIGN_GEOMETRIC_PRESENTATION_REPRESENTATION (  '', ( #91146 ), #59679 ) ;
#72183 = PRESENTATION_STYLE_ASSIGNMENT (( #55446 ) ) ;
#72185 = ORIENTED_EDGE ( 'NONE', *, *, #19748, .T. ) ;
#72186 = CARTESIAN_POINT ( 'NONE',  ( 84.13229308240822490, -50.16608149856336496, 187.2769468085622862 ) ) ;
#72187 = EDGE_CURVE ( 'NONE', #10153, #85648, #50001, .T. ) ;
#72188 = AXIS2_PLACEMENT_3D ( 'NONE', #56119, #15156, #57195 ) ;
#72189 = CARTESIAN_POINT ( 'NONE',  ( 0.000000000000000000, 15.00000000000000000, 0.000000000000000000 ) ) ;
#72190 = ORIENTED_EDGE ( 'NONE', *, *, #3101, .F. ) ;
#72191 = CARTESIAN_POINT ( 'NONE',  ( 95.67875834985767369, -57.67165897752772707, 38.73083894233180757 ) ) ;
#72192 = CARTESIAN_POINT ( 'NONE',  ( 36.64823341582350480, 437.5392299810053487, 4.281405873620224511 ) ) ;
#72193 = SURFACE_STYLE_FILL_AREA ( #16072 ) ;
#72194 = CARTESIAN_POINT ( 'NONE',  ( 28.94895647869510569, 13.71030094619077033, 39.84075445247401603 ) ) ;
#72195 = EDGE_CURVE ( 'NONE', #14549, #76811, #56866, .T. ) ;
#72196 = CARTESIAN_POINT ( 'NONE',  ( 29.50183317260396265, 13.72085623994622061, 42.10535821593450123 ) ) ;
#72197 = CARTESIAN_POINT ( 'NONE',  ( 2.094395098902538166, -3.000000000000000000, -8.000000000000000000 ) ) ;
#72198 = DIRECTION ( 'NONE',  ( 0.000000000000000000, 0.000000000000000000, 1.000000000000000000 ) ) ;
#72199 = CIRCLE ( 'NONE', #30884, 6.999999999999992895 ) ;
#72201 = CARTESIAN_POINT ( 'NONE',  ( -13.46865723075405441, 5.375093227679321295, 6.499662672654775264 ) ) ;
#72200 = CARTESIAN_POINT ( 'NONE',  ( 37.49021716374312518, 468.5026615090375230, 18.51838214818229034 ) ) ;
#72202 = CARTESIAN_POINT ( 'NONE',  ( -15.55016539897052397, 44.07927076389781718, -4.778920582525040928 ) ) ;
#72203 = CARTESIAN_POINT ( 'NONE',  ( -28.34313791092428758, 36.34626504971495109, -8.615479580127324510 ) ) ;
#72204 = CARTESIAN_POINT ( 'NONE',  ( -17.01158861293394509, -25.30155750122309044, -30.48162244162692858 ) ) ;
#72205 =( NAMED_UNIT ( * ) SI_UNIT ( $, .STERADIAN. ) SOLID_ANGLE_UNIT ( ) );
#72206 = AXIS2_PLACEMENT_3D ( 'NONE', #25558, #67580, #26099 ) ;
#72207 = STYLED_ITEM ( 'NONE', ( #62749 ), #102828 ) ;
#72208 = EDGE_CURVE ( 'NONE', #58987, #102378, #91908, .T. ) ;
#72209 = CARTESIAN_POINT ( 'NONE',  ( -83.09784762163468486, -38.00000000000002842, -1.930924322092125278 ) ) ;
#72210 = ORIENTED_EDGE ( 'NONE', *, *, #88339, .F. ) ;
#72211 = SURFACE_STYLE_USAGE ( .BOTH. , #64144 ) ;
#72212 = SURFACE_SIDE_STYLE ('',( #39332 ) ) ;
#72213 = CARTESIAN_POINT ( 'NONE',  ( -17.03013798833078241, -17.73699097705837247, -34.10471246031885073 ) ) ;
#72214 = EDGE_CURVE ( 'NONE', #40203, #29177, #29408, .T. ) ;
#72216 = CARTESIAN_POINT ( 'NONE',  ( -31.56605086575277852, -34.58954922973804713, -30.69102488358296199 ) ) ;
#72215 = CARTESIAN_POINT ( 'NONE',  ( 21.04247164025375483, 37.86482112153537116, -10.52123582012688097 ) ) ;
#72217 = ORIENTED_EDGE ( 'NONE', *, *, #34724, .T. ) ;
#72218 = STYLED_ITEM ( 'NONE', ( #9068 ), #45217 ) ;
#72219 = ORIENTED_EDGE ( 'NONE', *, *, #42361, .F. ) ;
#72220 = ADVANCED_FACE ( 'NONE', ( #15892 ), #93041, .T. ) ;
#72221 = CIRCLE ( 'NONE', #89475, 7.025805963803935406 ) ;
#72222 =( NAMED_UNIT ( * ) SI_UNIT ( $, .STERADIAN. ) SOLID_ANGLE_UNIT ( ) );
#72223 = DIRECTION ( 'NONE',  ( 0.000000000000000000, 0.000000000000000000, -1.000000000000000000 ) ) ;
#72224 = CARTESIAN_POINT ( 'NONE',  ( -92.63211006453688867, -59.99999999999997158, -9.950981327657569153 ) ) ;
#72225 = VERTEX_POINT ( 'NONE', #18034 ) ;
#72226 = DIRECTION ( 'NONE',  ( 0.000000000000000000, 0.000000000000000000, 1.000000000000000000 ) ) ;
#72227 = CARTESIAN_POINT ( 'NONE',  ( -7.338578092433039046, 54.31146207452502495, -2.464013259436235614 ) ) ;
#72228 = CARTESIAN_POINT ( 'NONE',  ( 96.88789730132712918, -45.26984529354276532, 194.0225460405672209 ) ) ;
#72229 = FACE_OUTER_BOUND ( 'NONE', #88717, .T. ) ;
#72230 = CARTESIAN_POINT ( 'NONE',  ( -85.23051947703226006, -18.61638337422625966, 157.3767952312193472 ) ) ;
#72231 = EDGE_LOOP ( 'NONE', ( #106716, #53582, #106441, #53257 ) ) ;
#72232 = VERTEX_POINT ( 'NONE', #58486 ) ;
#72233 = ORIENTED_EDGE ( 'NONE', *, *, #58041, .T. ) ;
#72235 =( BOUNDED_SURFACE ( )  B_SPLINE_SURFACE ( 3, 2, ( 
 ( #57915, #41745, #43349 ),
 ( #32625, #28264, #11489 ),
 ( #3425, #77842, #52486 ),
 ( #86494, #85405, #19116 ),
 ( #69752, #68705, #27200 ),
 ( #60616, #77310, #20726 ),
 ( #28806, #76766, #12552 ),
 ( #45490, #54065, #76234 ),
 ( #60090, #3955, #94024 ),
 ( #95101, #20185, #102105 ),
 ( #78357, #61134, #62217 ),
 ( #69236, #53036, #93506 ) ),
 .UNSPECIFIED., .F., .F., .F. ) 
 B_SPLINE_SURFACE_WITH_KNOTS ( ( 4, 2, 2, 2, 2, 4 ),
 ( 3, 3 ),
 ( -2.168404344971008868E-18, 0.001679904595664871237, 0.003359809191329744642, 0.004199761489162181019, 0.005039713786994618264, 0.006719618382659491018 ),
 ( 0.000000000000000000, 1.000000000000000000 ),
 .UNSPECIFIED. ) 
 GEOMETRIC_REPRESENTATION_ITEM ( )  RATIONAL_B_SPLINE_SURFACE ( (
 ( 1.000000000000000000, 0.8014084173415135792, 1.000000000000000000),
 ( 1.000000000000000000, 0.8133474198022304646, 1.000000000000000000),
 ( 1.000000000000000000, 0.8251589633861846629, 1.000000000000000000),
 ( 1.000000000000000000, 0.8478574907170124408, 1.000000000000000000),
 ( 1.000000000000000000, 0.8587488926553007440, 1.000000000000000000),
 ( 1.000000000000000000, 0.8739423948878513038, 1.000000000000000000),
 ( 1.000000000000000000, 0.8787956638559439870, 1.000000000000000000),
 ( 1.000000000000000000, 0.8878757020716585568, 1.000000000000000000),
 ( 1.000000000000000000, 0.8921241670188198025, 1.000000000000000000),
 ( 1.000000000000000000, 0.9038999154880622555, 1.000000000000000000),
 ( 1.000000000000000000, 0.9104653308040103754, 1.000000000000000000),
 ( 1.000000000000000000, 0.9153908114177993216, 1.000000000000000000) ) ) 
 REPRESENTATION_ITEM ( '' )  SURFACE ( )  );
#72234 = CARTESIAN_POINT ( 'NONE',  ( 31.15871529744714863, 428.0462763543694109, 24.54283678189916884 ) ) ;
#72236 = CARTESIAN_POINT ( 'NONE',  ( -5.000000000000000000, -14.30429124282216513, 12.05126107871866026 ) ) ;
#72237 =( LENGTH_UNIT ( ) NAMED_UNIT ( * ) SI_UNIT ( .MILLI., .METRE. ) );
#72238 = ORIENTED_EDGE ( 'NONE', *, *, #70852, .F. ) ;
#72239 = CARTESIAN_POINT ( 'NONE',  ( -32.83963058903137266, 487.9259900561239647, 4.912448545037069181 ) ) ;
#72240 = CARTESIAN_POINT ( 'NONE',  ( -74.02244645645996002, -57.61166141858229395, 187.2311674206319765 ) ) ;
#72241 = FACE_OUTER_BOUND ( 'NONE', #4101, .T. ) ;
#72242 = CIRCLE ( 'NONE', #73918, 4.000000000000001776 ) ;
#72243 = CARTESIAN_POINT ( 'NONE',  ( -65.20309930813586163, 47.99999999999999289, 0.3961530819213011090 ) ) ;
#72244 = CARTESIAN_POINT ( 'NONE',  ( -5.580966921651770022E-13, 25.16821295365027211, 40.75000000000505906 ) ) ;
#72245 = CARTESIAN_POINT ( 'NONE',  ( 0.7835956671373057736, 28.10810970921148311, -38.51249778524339717 ) ) ;
#72246 = CARTESIAN_POINT ( 'NONE',  ( 24.89419722466787022, -30.00000000000004974, -38.80375014483585261 ) ) ;
#72247 = CARTESIAN_POINT ( 'NONE',  ( -54.44990204170284898, -30.00000000000008882, 75.82925260777241760 ) ) ;
#72248 = CARTESIAN_POINT ( 'NONE',  ( -53.51057452807305026, -22.16812215901368432, 50.70531185769669236 ) ) ;
#72249 = VECTOR ( 'NONE', #69231, 1000.000000000000000 ) ;
#72250 = ORIENTED_EDGE ( 'NONE', *, *, #47314, .T. ) ;
#72251 = CARTESIAN_POINT ( 'NONE',  ( 3.787223616631151923, 19.16579769262013500, -5.888204939567934559 ) ) ;
#72252 = VERTEX_POINT ( 'NONE', #98912 ) ;
#72253 = CARTESIAN_POINT ( 'NONE',  ( -102.0339308600683097, -60.20990888865522095, 194.1617984564381629 ) ) ;
#72254 = DIRECTION ( 'NONE',  ( -0.000000000000000000, -0.5617366626182503930, -0.8273160954982743398 ) ) ;
#72255 = VECTOR ( 'NONE', #19228, 1000.000000000000000 ) ;
#72256 = VERTEX_POINT ( 'NONE', #57397 ) ;
#72257 = CARTESIAN_POINT ( 'NONE',  ( -16.83450711267213151, 34.23838129605825742, -24.30698433968598238 ) ) ;
#72258 = CARTESIAN_POINT ( 'NONE',  ( 110.0576603816093950, -38.35596508152210049, 154.9619461380562200 ) ) ;
#72259 = CARTESIAN_POINT ( 'NONE',  ( 5.193195059372482212E-16, -7.895640089090903757, -6.564402953523731377 ) ) ;
#72260 = CYLINDRICAL_SURFACE ( 'NONE', #68067, 4.000000000000000000 ) ;
#72261 = FACE_OUTER_BOUND ( 'NONE', #53484, .T. ) ;
#72262 = CARTESIAN_POINT ( 'NONE',  ( 84.26804285766414182, -30.00000000000000000, 163.4126049098225621 ) ) ;
#72263 = CARTESIAN_POINT ( 'NONE',  ( 13.58964414657211073, 303.5476453198347144, -10.06465184102012955 ) ) ;
#72264 = DIRECTION ( 'NONE',  ( -1.000000000000000000, -0.000000000000000000, -0.000000000000000000 ) ) ;
#72265 = FACE_OUTER_BOUND ( 'NONE', #43713, .T. ) ;
#72266 = ADVANCED_FACE ( 'NONE', ( #82208 ), #46540, .F. ) ;
#72267 = DIRECTION ( 'NONE',  ( 0.000000000000000000, 0.000000000000000000, 1.000000000000000000 ) ) ;
#72268 = VERTEX_POINT ( 'NONE', #16420 ) ;
#72269 = ORIENTED_EDGE ( 'NONE', *, *, #65566, .F. ) ;
#72270 = CARTESIAN_POINT ( 'NONE',  ( 49.29183012222615901, -18.74727630053224914, 42.99191983216383761 ) ) ;
#72271 = CARTESIAN_POINT ( 'NONE',  ( 70.41111111111112564, 6.915964383211875250E-15, 0.000000000000000000 ) ) ;
#72272 = AXIS2_PLACEMENT_3D ( 'NONE', #66083, #74167, #105483 ) ;
#72273 = ADVANCED_FACE ( 'NONE', ( #98399 ), #69716, .T. ) ;
#72274 = DIRECTION ( 'NONE',  ( 0.000000000000000000, 0.000000000000000000, 1.000000000000000000 ) ) ;
#72275 = CARTESIAN_POINT ( 'NONE',  ( -110.3499448355333215, -38.35608688738442140, 183.6271486024410251 ) ) ;
#72276 = ORIENTED_EDGE ( 'NONE', *, *, #57156, .T. ) ;
#72277 = CARTESIAN_POINT ( 'NONE',  ( 90.74655439557324144, -38.34261265473484315, 6.503296633511228997 ) ) ;
#72278 = CARTESIAN_POINT ( 'NONE',  ( 10.94020704007013656, 11.19319730264500024, -9.841999159912100836 ) ) ;
#72279 = DIRECTION ( 'NONE',  ( -1.000000000000000000, -1.224606353822377258E-16, -0.000000000000000000 ) ) ;
#72280 = CARTESIAN_POINT ( 'NONE',  ( -42.69811214730272297, 434.9611672192513652, 18.34625614733208820 ) ) ;
#72281 = CARTESIAN_POINT ( 'NONE',  ( 101.2281462999901152, -37.84858859627455274, 149.3017034182498435 ) ) ;
#72282 = DIRECTION ( 'NONE',  ( -0.8191520442889974607, 0.000000000000000000, -0.5735764363510380548 ) ) ;
#72283 = CIRCLE ( 'NONE', #99606, 3.309500000000001663 ) ;
#72284 = CARTESIAN_POINT ( 'NONE',  ( -36.65515723092381251, 373.6298163844335249, 4.402904589519302192 ) ) ;
#72285 = CARTESIAN_POINT ( 'NONE',  ( 93.22046886666203136, -59.99999999999999289, 202.4896487005214851 ) ) ;
#72286 = CARTESIAN_POINT ( 'NONE',  ( 18.91791044776121211, 45.00000000000000711, 62.18611311450882795 ) ) ;
#72287 = VERTEX_POINT ( 'NONE', #85418 ) ;
#72288 = CARTESIAN_POINT ( 'NONE',  ( 55.90058340703467366, -53.37925634193300795, 68.14343119493420886 ) ) ;
#72289 = CARTESIAN_POINT ( 'NONE',  ( -33.62653946147953121, 300.0647574820262093, -8.836532605440917010 ) ) ;
#72290 = EDGE_CURVE ( 'NONE', #105955, #71682, #43153, .T. ) ;
#72291 = DIRECTION ( 'NONE',  ( -0.5735764363510510444, -0.8191520442889883569, 0.000000000000000000 ) ) ;
#72292 = CARTESIAN_POINT ( 'NONE',  ( -13.50000000000000000, -2.625659737069751198, -12.88678781509933735 ) ) ;
#72293 = ORIENTED_EDGE ( 'NONE', *, *, #91024, .F. ) ;
#72295 = CARTESIAN_POINT ( 'NONE',  ( -9.215420734788356327, -54.00000000000001421, 23.11721482942554928 ) ) ;
#72294 = CARTESIAN_POINT ( 'NONE',  ( -110.3148016707792465, -38.35598278249073445, 183.9770048744294115 ) ) ;
#72296 = DIRECTION ( 'NONE',  ( 0.000000000000000000, 0.000000000000000000, -1.000000000000000000 ) ) ;
#72297 = CARTESIAN_POINT ( 'NONE',  ( 30.86805345995181327, 345.9229254628596095, 18.50907901912128395 ) ) ;
#72298 = DIRECTION ( 'NONE',  ( 0.000000000000000000, 0.000000000000000000, 1.000000000000000000 ) ) ;
#72299 = PRESENTATION_LAYER_ASSIGNMENT (  '', '', ( #8532 ) ) ;
#72300 = CARTESIAN_POINT ( 'NONE',  ( -5.656854249492381470, -32.56249999999999289, 5.656854249492379694 ) ) ;
#72301 = CARTESIAN_POINT ( 'NONE',  ( 6.145467200819017428, -3.000000000000002665, -77.00333157708807619 ) ) ;
#72302 = CIRCLE ( 'NONE', #106782, 4.000000000000007105 ) ;
#72303 = CARTESIAN_POINT ( 'NONE',  ( 7.922281120364393914, -4.573931137438281169, -8.047472243342934206 ) ) ;
#72304 = AXIS2_PLACEMENT_3D ( 'NONE', #6449, #48499, #39385 ) ;
#72305 = ORIENTED_EDGE ( 'NONE', *, *, #88339, .T. ) ;
#72306 = CARTESIAN_POINT ( 'NONE',  ( 83.24093056157693127, -42.97671957674801035, 177.1152172873732695 ) ) ;
#72307 = CARTESIAN_POINT ( 'NONE',  ( 8.619428876659387839, 129.1420429763053903, -0.000000000000000000 ) ) ;
#72308 = B_SPLINE_CURVE_WITH_KNOTS ( 'NONE', 3,
 ( #54744, #104919, #88203, #96305, #4631, #38090, #79565, #46667, #47187, #62872 ),
 .UNSPECIFIED., .F., .F.,
 ( 4, 2, 2, 2, 4 ),
 ( 0.000000000000000000, 0.2500000000000000000, 0.5000000000000000000, 0.7500000000000000000, 1.000000000000000000 ),
 .UNSPECIFIED. ) ;
#72309 = ADVANCED_FACE ( 'NONE', ( #3437 ), #87687, .F. ) ;
#72310 = DIRECTION ( 'NONE',  ( 0.000000000000000000, 1.000000000000000000, 0.000000000000000000 ) ) ;
#72311 = VERTEX_POINT ( 'NONE', #102119 ) ;
#72312 = CARTESIAN_POINT ( 'NONE',  ( -37.46459653829825953, 360.1626999571597594, 2.821112259843927994 ) ) ;
#72313 = CARTESIAN_POINT ( 'NONE',  ( 7.014891834159853623, -4.207085196949424066, -17.12005312236325594 ) ) ;
#72314 = DIRECTION ( 'NONE',  ( -1.000000000000000000, -1.224606353822377258E-16, -0.000000000000000000 ) ) ;
#72315 = CARTESIAN_POINT ( 'NONE',  ( 4.000000000000000000, 4.898587196589412829E-16, -6.838999999999999524 ) ) ;
#72316 = DIRECTION ( 'NONE',  ( 0.000000000000000000, 0.000000000000000000, 1.000000000000000000 ) ) ;
#72317 = CARTESIAN_POINT ( 'NONE',  ( 0.000000000000000000, 0.000000000000000000, -0.7702282920306786629 ) ) ;
#72318 = CONICAL_SURFACE ( 'NONE', #25865, 4.250000000000000000, 0.9599310885968754814 ) ;
#72319 = EDGE_CURVE ( 'NONE', #79502, #70791, #53476, .T. ) ;
#72320 = ORIENTED_EDGE ( 'NONE', *, *, #53366, .T. ) ;
#72321 =( NAMED_UNIT ( * ) PLANE_ANGLE_UNIT ( ) SI_UNIT ( $, .RADIAN. ) );
#72322 = VECTOR ( 'NONE', #105359, 1000.000000000000000 ) ;
#72323 = CARTESIAN_POINT ( 'NONE',  ( 38.81340407398939618, 25.21178748735488284, 12.01518403244543087 ) ) ;
#72324 = DIRECTION ( 'NONE',  ( 0.000000000000000000, 0.000000000000000000, -1.000000000000000000 ) ) ;
#72326 = CARTESIAN_POINT ( 'NONE',  ( -13.53249398123303848, 7.603952788152932740, -8.423294693568777802 ) ) ;
#72325 = DIRECTION ( 'NONE',  ( 0.000000000000000000, -1.000000000000000000, 0.000000000000000000 ) ) ;
#72327 = CIRCLE ( 'NONE', #34491, 3.309500000000007880 ) ;
#72328 = CARTESIAN_POINT ( 'NONE',  ( 7.188101187500000044, -20.65625000204838813, 0.000000000000000000 ) ) ;
#72329 = CARTESIAN_POINT ( 'NONE',  ( -28.58272191126927098, 16.23375075743840412, -41.45992959583551851 ) ) ;
#72330 = DIRECTION ( 'NONE',  ( 0.000000000000000000, -1.000000000000000000, 0.000000000000000000 ) ) ;
#72331 = B_SPLINE_CURVE_WITH_KNOTS ( 'NONE', 3,
 ( #32578, #42223, #143, #41176, #74055, #23969, #663, #90795, #90256, #33629, #83218, #66506, #56811, #15301, #16358, #9313, #98346, #82150 ),
 .UNSPECIFIED., .F., .F.,
 ( 4, 2, 2, 2, 2, 2, 2, 2, 4 ),
 ( 0.01918304055315395856, 0.01998049418066448479, 0.02077794780817501102, 0.02157540143568553379, 0.02237285506319606002, 0.02317030869070658278, 0.02396776231821710901, 0.02476521594572763524, 0.02556266957323816147 ),
 .UNSPECIFIED. ) ;
#72332 = CIRCLE ( 'NONE', #29347, 9.500000000000000000 ) ;
#72333 = ORIENTED_EDGE ( 'NONE', *, *, #61015, .T. ) ;
#72334 = DIRECTION ( 'NONE',  ( -1.000000000000000000, -1.224606353822377258E-16, -0.000000000000000000 ) ) ;
#72335 = CARTESIAN_POINT ( 'NONE',  ( 7.500000000000000000, 1.545478204151520707, -7.491761935628703739 ) ) ;
#72336 = CARTESIAN_POINT ( 'NONE',  ( -9.514962458596817996, 142.5298273669549189, 0.000000000000000000 ) ) ;
#72337 = CARTESIAN_POINT ( 'NONE',  ( -9.432319653624512412, -5.000000000000000888, -70.68463330168729897 ) ) ;
#72338 = EDGE_CURVE ( 'NONE', #56970, #100861, #63356, .T. ) ;
#72339 = CARTESIAN_POINT ( 'NONE',  ( -14.37676598790170956, 2.000025124018793843, 4.258993516771657717 ) ) ;
#72340 = ORIENTED_EDGE ( 'NONE', *, *, #46677, .F. ) ;
#72341 = DIRECTION ( 'NONE',  ( -1.000000000000000000, -1.224606353822377258E-16, -0.000000000000000000 ) ) ;
#72342 = CARTESIAN_POINT ( 'NONE',  ( 0.5805565836007605673, 3.752776749732565253, 6.499999999999997335 ) ) ;
#72343 = ORIENTED_EDGE ( 'NONE', *, *, #83019, .T. ) ;
#72344 = AXIS2_PLACEMENT_3D ( 'NONE', #46590, #4015, #53097 ) ;
#72345 = EDGE_CURVE ( 'NONE', #14213, #29611, #60631, .T. ) ;
#72346 = DIRECTION ( 'NONE',  ( 0.000000000000000000, 0.000000000000000000, 1.000000000000000000 ) ) ;
#72347 = CARTESIAN_POINT ( 'NONE',  ( -2.067305840858484345, -0.1358350450447191882, 102.1177254334556892 ) ) ;
#72348 = FILL_AREA_STYLE_COLOUR ( '', #85544 ) ;
#72349 = CARTESIAN_POINT ( 'NONE',  ( -111.2112538145483143, -59.99999999999999289, 154.2509436529097115 ) ) ;
#72350 = EDGE_CURVE ( 'NONE', #16013, #1287, #6379, .T. ) ;
#72351 = CARTESIAN_POINT ( 'NONE',  ( 29.01988888469873018, 321.8047804620298393, 14.12772110426748284 ) ) ;
#72352 = CARTESIAN_POINT ( 'NONE',  ( -12.53073535838927910, 1.820007232887559612, 14.89064316150549594 ) ) ;
#72353 = CARTESIAN_POINT ( 'NONE',  ( 8.737863884121400915, -4.999999999998638422, -90.03618980231146907 ) ) ;
#72354 = CARTESIAN_POINT ( 'NONE',  ( -85.70070447472639330, -21.88688739919286164, 168.6176033816253153 ) ) ;
#72355 = ORIENTED_EDGE ( 'NONE', *, *, #3372, .T. ) ;
#72356 = CARTESIAN_POINT ( 'NONE',  ( 7.500000000000005329, 9.833333333333344584, -71.71180648257555390 ) ) ;
#72357 = EDGE_CURVE ( 'NONE', #33657, #38940, #89139, .T. ) ;
#72358 = ORIENTED_EDGE ( 'NONE', *, *, #98081, .T. ) ;
#72359 = CARTESIAN_POINT ( 'NONE',  ( 5.500000000000006217, 42.00000000000000000, -62.89165061903125320 ) ) ;
#72360 = DIRECTION ( 'NONE',  ( 1.000000000000000000, -0.000000000000000000, -0.000000000000000000 ) ) ;
#72361 = CARTESIAN_POINT ( 'NONE',  ( -16.10173312979620874, 5.477053992169603980, -4.739458514410732626 ) ) ;
#72362 = CARTESIAN_POINT ( 'NONE',  ( 3.443379947491756354, 27.85683824479126258, -5.000000000000000000 ) ) ;
#72363 = FACE_OUTER_BOUND ( 'NONE', #40307, .T. ) ;
#72364 = CARTESIAN_POINT ( 'NONE',  ( 38.86650669486618881, 4.000000000000003553, 4.898587196589414801E-16 ) ) ;
#72365 = CARTESIAN_POINT ( 'NONE',  ( 89.23375057675741573, -59.99999999999977973, 204.3679297810271862 ) ) ;
#72366 = CONICAL_SURFACE ( 'NONE', #6922, 4.172000000000001485, 0.9599310885968750373 ) ;
#72367 = CARTESIAN_POINT ( 'NONE',  ( -100.7780794135568954, -14.21045842199427156, 117.1455274902871366 ) ) ;
#72368 = CARTESIAN_POINT ( 'NONE',  ( -60.90366851421529759, -56.86960161935190428, 83.15536174215863241 ) ) ;
#72369 = EDGE_LOOP ( 'NONE', ( #56714, #86886, #99567, #94314, #35514, #30106 ) ) ;
#72370 = CARTESIAN_POINT ( 'NONE',  ( 61.55604228310126302, 38.95379169962407673, -16.52177172830128526 ) ) ;
#72371 = CARTESIAN_POINT ( 'NONE',  ( 72.84044669408135064, -60.00000000000491696, 183.1815887110867607 ) ) ;
#72372 = ORIENTED_EDGE ( 'NONE', *, *, #26870, .T. ) ;
#72373 = CARTESIAN_POINT ( 'NONE',  ( 3.030313384945461763, -39.47248979064079322, 30.46354856792267896 ) ) ;
#72374 = CARTESIAN_POINT ( 'NONE',  ( 7.188101187499999156, -19.62500000204838457, 2.977408999572654924 ) ) ;
#72375 = CARTESIAN_POINT ( 'NONE',  ( 32.87491876136141400, 485.1684955304415894, 5.618973769036216481 ) ) ;
#72376 = VERTEX_POINT ( 'NONE', #13096 ) ;
#72377 = CARTESIAN_POINT ( 'NONE',  ( -33.00000000000000000, 450.0000000000002274, 13.20242257375370976 ) ) ;
#72378 = ORIENTED_EDGE ( 'NONE', *, *, #60766, .T. ) ;
#72379 = DIRECTION ( 'NONE',  ( 0.000000000000000000, 1.000000000000000000, 0.000000000000000000 ) ) ;
#72380 = CARTESIAN_POINT ( 'NONE',  ( -7.894787914004607998, -1.231000152045941975E-13, -7.591390474663426424 ) ) ;
#72381 = CARTESIAN_POINT ( 'NONE',  ( -87.16287115447597955, -59.99999999999998579, 201.0813553807005576 ) ) ;
#72382 = CARTESIAN_POINT ( 'NONE',  ( 1.101454001169993813, -14.95253250404446277, -0.8386200322166146304 ) ) ;
#72383 = CARTESIAN_POINT ( 'NONE',  ( -2.977408999572654480, -29.00000000204838813, 7.188101187499999156 ) ) ;
#72384 = AXIS2_PLACEMENT_3D ( 'NONE', #66114, #33776, #8933 ) ;
#72385 = CARTESIAN_POINT ( 'NONE',  ( 6.849999999999999645, 0.000000000000000000, 5.000000000000002665 ) ) ;
#72386 = CARTESIAN_POINT ( 'NONE',  ( -32.78741055188834963, 485.3331003366709524, 5.977022408746728743 ) ) ;
#72387 = CARTESIAN_POINT ( 'NONE',  ( 5.000000000000000000, -54.97504912987177050, 9.868491161016267554 ) ) ;
#72388 = AXIS2_PLACEMENT_3D ( 'NONE', #43364, #35300, #60109 ) ;
#72389 = CARTESIAN_POINT ( 'NONE',  ( 1.308996937483426715, 48.00000000000000000, -95.00000000000000000 ) ) ;
#72390 = CARTESIAN_POINT ( 'NONE',  ( -12.13034742782427777, 41.99999999999999289, -93.82352941176471006 ) ) ;
#72391 = DIRECTION ( 'NONE',  ( -0.000000000000000000, 0.000000000000000000, -1.000000000000000000 ) ) ;
#72392 = ADVANCED_FACE ( 'NONE', ( #12569 ), #39700, .T. ) ;
#72393 = CARTESIAN_POINT ( 'NONE',  ( 29.60041846187245795, 307.3673858255965001, -8.977896531553003712 ) ) ;
#72394 = CARTESIAN_POINT ( 'NONE',  ( -32.43755732417693594, -42.96442599306529075, 34.72761510847016098 ) ) ;
#72395 = ORIENTED_EDGE ( 'NONE', *, *, #36971, .T. ) ;
#72396 = CARTESIAN_POINT ( 'NONE',  ( -14.33580415456969703, 41.99999999999998579, -89.41414988892334748 ) ) ;
#72397 = CARTESIAN_POINT ( 'NONE',  ( 41.90357024077690085, -32.61324066414001521, 38.71707398534343980 ) ) ;
#72398 = CARTESIAN_POINT ( 'NONE',  ( 13.60704923275002010, -1.734723475976807094E-15, -10.45706415777842935 ) ) ;
#72399 = ORIENTED_EDGE ( 'NONE', *, *, #9311, .T. ) ;
#72400 = ADVANCED_FACE ( 'NONE', ( #71342 ), #65478, .T. ) ;
#72401 = EDGE_CURVE ( 'NONE', #13600, #73449, #3505, .T. ) ;
#72402 = CARTESIAN_POINT ( 'NONE',  ( 6.692588830498425345, -3.932766476276031486, 6.892929031562514020 ) ) ;
#72403 = AXIS2_PLACEMENT_3D ( 'NONE', #32639, #49300, #74114 ) ;
#72404 = CARTESIAN_POINT ( 'NONE',  ( -55.77509681992000878, -38.34453011954626334, 83.68376476757157434 ) ) ;
#72405 = ORIENTED_EDGE ( 'NONE', *, *, #1705, .F. ) ;
#72407 = CARTESIAN_POINT ( 'NONE',  ( -24.93816302196866275, 307.4233949143036284, 10.52291764336465008 ) ) ;
#72406 = CARTESIAN_POINT ( 'NONE',  ( 8.749920771053334434, -5.000000000000000000, -16.79831961264161677 ) ) ;
#72408 = DIRECTION ( 'NONE',  ( -0.000000000000000000, -1.000000000000000000, -0.000000000000000000 ) ) ;
#72409 = CARTESIAN_POINT ( 'NONE',  ( 6.162888688655346670, -3.752776749732575468, -6.499999999999999112 ) ) ;
#72410 = DIRECTION ( 'NONE',  ( 0.000000000000000000, 0.000000000000000000, -1.000000000000000000 ) ) ;
#72411 = CARTESIAN_POINT ( 'NONE',  ( 36.36650669486618881, 1.474610560812782335E-15, 0.000000000000000000 ) ) ;
#72412 = CARTESIAN_POINT ( 'NONE',  ( -49.10072971674536291, 12.98664841672704107, -16.25083509557213191 ) ) ;
#72413 = DIRECTION ( 'NONE',  ( -0.000000000000000000, 1.000000000000000000, -0.000000000000000000 ) ) ;
#72414 = PRESENTATION_LAYER_ASSIGNMENT (  '', '', ( #91365 ) ) ;
#72415 = CARTESIAN_POINT ( 'NONE',  ( 94.25213324963540629, -59.99999999999998579, 43.35550940579889101 ) ) ;
#72416 = CARTESIAN_POINT ( 'NONE',  ( 0.000000000000000000, 35.00000000000000000, 0.000000000000000000 ) ) ;
#72417 = DIRECTION ( 'NONE',  ( -1.000000000000000000, -0.000000000000000000, -0.000000000000000000 ) ) ;
#72418 = CARTESIAN_POINT ( 'NONE',  ( 12.61650669486618881, -3.999999999999998224, 0.000000000000000000 ) ) ;
#72419 = ORIENTED_EDGE ( 'NONE', *, *, #57618, .F. ) ;
#72420 = EDGE_CURVE ( 'NONE', #58381, #83030, #36274, .T. ) ;
#72421 = CARTESIAN_POINT ( 'NONE',  ( -89.88336266018133358, -29.99999999998671640, -1.794731794580948003 ) ) ;
#72422 = ORIENTED_EDGE ( 'NONE', *, *, #83284, .F. ) ;
#72423 = FACE_OUTER_BOUND ( 'NONE', #1951, .T. ) ;
#72424 = CARTESIAN_POINT ( 'NONE',  ( -16.02742720722309144, 4.186773460851249240, -2.547561848284168207 ) ) ;
#72425 = CARTESIAN_POINT ( 'NONE',  ( 9.517802784864830556, 9.453294932689157548, 9.300361635023031386E-13 ) ) ;
#72426 = CARTESIAN_POINT ( 'NONE',  ( 2.761899744546835519E-15, 36.79151656018385097, 22.55262289886175964 ) ) ;
#72427 = CARTESIAN_POINT ( 'NONE',  ( 9.797537890442935549, 26.53442202333808098, 2.014215961808872635 ) ) ;
#72428 = CARTESIAN_POINT ( 'NONE',  ( -5.082755093536326818, -27.59375000204838813, 5.082755093536325042 ) ) ;
#72429 = CARTESIAN_POINT ( 'NONE',  ( -18.65899211044941097, 45.00000000000001421, 62.26487979851452081 ) ) ;
#72430 =( NAMED_UNIT ( * ) SI_UNIT ( $, .STERADIAN. ) SOLID_ANGLE_UNIT ( ) );
#72431 = DIRECTION ( 'NONE',  ( -1.000000000000000000, -0.000000000000000000, -0.000000000000000000 ) ) ;
#72432 = ORIENTED_EDGE ( 'NONE', *, *, #96963, .F. ) ;
#72433 = CONICAL_SURFACE ( 'NONE', #24343, 5.000000000000001776, 0.9599310885968803664 ) ;
#72435 = ORIENTED_EDGE ( 'NONE', *, *, #24288, .T. ) ;
#72434 = CARTESIAN_POINT ( 'NONE',  ( -7.491624054469464333, 40.33174201206623621, -59.48414770601905133 ) ) ;
#72436 = CARTESIAN_POINT ( 'NONE',  ( 81.98252987595192565, -32.55966453745716649, 150.9950225902835825 ) ) ;
#72437 = B_SPLINE_CURVE_WITH_KNOTS ( 'NONE', 3,
 ( #66549, #60612, #75700, #99427, #50881, #85401, #91373, #67091, #83785, #77305, #76229, #25606, #68149, #35276 ),
 .UNSPECIFIED., .F., .F.,
 ( 4, 2, 2, 2, 2, 2, 4 ),
 ( 1.532679976604137452E-17, 0.001109001854540035822, 0.002218003709080056032, 0.003327005563620077759, 0.003881506490890071926, 0.004158756954525069660, 0.004436007418160066960 ),
 .UNSPECIFIED. ) ;
#72438 = CARTESIAN_POINT ( 'NONE',  ( -37.72546545933433748, 27.83008492337310358, -10.95617127781036437 ) ) ;
#72439 = VERTEX_POINT ( 'NONE', #14684 ) ;
#72440 = DIRECTION ( 'NONE',  ( -1.000000000000000000, -1.224606353822377258E-16, -0.000000000000000000 ) ) ;
#72441 = CARTESIAN_POINT ( 'NONE',  ( -1.231024308828225999, 16.45180670219713903, -50.25114264119800822 ) ) ;
#72442 = CARTESIAN_POINT ( 'NONE',  ( -1.320432766682874540E-15, -15.03125000204838457, 7.188101187500000044 ) ) ;
#72443 = DIRECTION ( 'NONE',  ( -0.000000000000000000, -1.000000000000000000, -0.000000000000000000 ) ) ;
#72444 = CARTESIAN_POINT ( 'NONE',  ( -29.62390339563712160, -57.68322450639401211, 45.06481242858825453 ) ) ;
#72445 = CARTESIAN_POINT ( 'NONE',  ( 6.562934840145641324, -4.277581483015143071, -6.282640795011896984 ) ) ;
#72446 = ORIENTED_EDGE ( 'NONE', *, *, #51491, .F. ) ;
#72447 = CIRCLE ( 'NONE', #8685, 3.309500000000001663 ) ;
#72448 = DIRECTION ( 'NONE',  ( 0.000000000000000000, 0.000000000000000000, 1.000000000000000000 ) ) ;
#72449 = DIRECTION ( 'NONE',  ( 0.000000000000000000, -1.000000000000000000, 3.755786496842903988E-16 ) ) ;
#72450 = CARTESIAN_POINT ( 'NONE',  ( 35.10078947236149105, 18.64284798592602144, -15.64789144403509091 ) ) ;
#72451 = DIRECTION ( 'NONE',  ( 0.000000000000000000, 0.1742756985702809125, 0.9846968979781752784 ) ) ;
#72452 = ORIENTED_EDGE ( 'NONE', *, *, #102568, .F. ) ;
#72453 = CARTESIAN_POINT ( 'NONE',  ( -3.313708498984765161, -14.65625000409677092, 7.999999999999998224 ) ) ;
#72454 = CARTESIAN_POINT ( 'NONE',  ( -24.30786747476509291, -18.98229748144842688, 31.52624602878413640 ) ) ;
#72455 = CARTESIAN_POINT ( 'NONE',  ( -1.000000000000000000, -26.91905550219100363, -6.087553237119084137 ) ) ;
#72456 = CARTESIAN_POINT ( 'NONE',  ( -3.313708498984726969, -15.96874999999998934, 8.000000000000039080 ) ) ;
#72457 = CARTESIAN_POINT ( 'NONE',  ( 39.28547526272472368, 437.8764796837014046, 22.93021597682914248 ) ) ;
#72458 = APPLICATION_PROTOCOL_DEFINITION ( 'draft international standard', 'automotive_design', 1998, #89333 ) ;
#72459 = CARTESIAN_POINT ( 'NONE',  ( 38.81959903812767720, 27.30122739460367853, 12.35248524812892512 ) ) ;
#72460 = ORIENTED_EDGE ( 'NONE', *, *, #73329, .F. ) ;
#72461 = DIRECTION ( 'NONE',  ( 0.000000000000000000, -1.000000000000000000, 0.000000000000000000 ) ) ;
#72462 = TOROIDAL_SURFACE ( 'NONE', #22532, 4.400000000000000355, 0.4000000000000000222 ) ;
#72463 = SURFACE_STYLE_FILL_AREA ( #9305 ) ;
#72464 = MECHANICAL_DESIGN_GEOMETRIC_PRESENTATION_REPRESENTATION (  '', ( #44922 ), #38100 ) ;
#72465 = CARTESIAN_POINT ( 'NONE',  ( -76.12537862032620239, -38.35598417008156957, -28.58435412235104423 ) ) ;
#72466 = CARTESIAN_POINT ( 'NONE',  ( -59.15011143018023887, -30.00000000000000355, 64.89418600812079774 ) ) ;
#72467 = CARTESIAN_POINT ( 'NONE',  ( 13.07034999569633626, 42.28767565851803312, -92.53123953979158500 ) ) ;
#72468 = EDGE_CURVE ( 'NONE', #94380, #47192, #46023, .T. ) ;
#72469 = ORIENTED_EDGE ( 'NONE', *, *, #50660, .T. ) ;
#72470 = AXIS2_PLACEMENT_3D ( 'NONE', #58680, #33353, #41948 ) ;
#72471 = CARTESIAN_POINT ( 'NONE',  ( 0.7145311798163219708, 4.618802153517003184, -8.000000000000000000 ) ) ;
#72472 = CARTESIAN_POINT ( 'NONE',  ( 101.7590372865866755, -57.63143884806530792, 203.3630881935354182 ) ) ;
#72473 = CIRCLE ( 'NONE', #5349, 18.07003550757956845 ) ;
#72474 = EDGE_CURVE ( 'NONE', #84766, #22594, #63801, .T. ) ;
#72475 = EDGE_CURVE ( 'NONE', #89014, #84193, #80485, .T. ) ;
#72476 = CARTESIAN_POINT ( 'NONE',  ( -16.10155139016692516, 21.86297139503206921, 0.4316986452184163325 ) ) ;
#72477 = CARTESIAN_POINT ( 'NONE',  ( 0.4969600502617456672, -4.995646404165269061, 7.347286611336970807 ) ) ;
#72478 = CARTESIAN_POINT ( 'NONE',  ( -74.80865327367102680, -59.99999999999999289, 179.7763745376072677 ) ) ;
#72479 = PRESENTATION_STYLE_ASSIGNMENT (( #23432 ) ) ;
#72480 = CARTESIAN_POINT ( 'NONE',  ( 28.00203968317441294, 50.00000000000000000, 56.72941417029700517 ) ) ;
#72481 = CARTESIAN_POINT ( 'NONE',  ( -84.23794301257443351, -53.80601704703899912, 189.3816763263162102 ) ) ;
#72482 = ORIENTED_EDGE ( 'NONE', *, *, #81129, .F. ) ;
#72483 = CARTESIAN_POINT ( 'NONE',  ( 27.33006516600399038, 307.9308989645884367, -8.309468075633031248 ) ) ;
#72484 = EDGE_CURVE ( 'NONE', #77528, #90268, #4130, .T. ) ;
#72485 = ORIENTED_EDGE ( 'NONE', *, *, #17490, .T. ) ;
#72486 = CARTESIAN_POINT ( 'NONE',  ( -7.212408192734265810, -12.01517089320369891, -3.465038817813884897 ) ) ;
#72487 = DIRECTION ( 'NONE',  ( -1.000000000000000000, -0.000000000000000000, -0.000000000000000000 ) ) ;
#72488 = CARTESIAN_POINT ( 'NONE',  ( -85.09719550378922293, -60.19746287038491062, -15.90597616068271591 ) ) ;
#72489 = VECTOR ( 'NONE', #76591, 1000.000000000000000 ) ;
#72490 = DIRECTION ( 'NONE',  ( 0.000000000000000000, -1.000000000000000000, 0.000000000000000000 ) ) ;
#72491 = SURFACE_STYLE_FILL_AREA ( #57352 ) ;
#72492 = VERTEX_POINT ( 'NONE', #54083 ) ;
#72493 = CONICAL_SURFACE ( 'NONE', #19200, 4.000000000000001776, 0.9599310885968808105 ) ;
#72494 = CARTESIAN_POINT ( 'NONE',  ( 18.53506029635388686, 50.00000000000000711, 61.21187092669564578 ) ) ;
#72495 = CARTESIAN_POINT ( 'NONE',  ( 13.59379325674309946, 24.77301814849831274, -0.6326043077446807938 ) ) ;
#72496 = CARTESIAN_POINT ( 'NONE',  ( -22.59067934059571314, 27.55769764751302020, 33.04957285560292490 ) ) ;
#72497 = CARTESIAN_POINT ( 'NONE',  ( 15.59999999999999787, 3.309500000000003439, 4.052968581778167743E-16 ) ) ;
#72498 = CARTESIAN_POINT ( 'NONE',  ( 84.06490631893382215, -29.99999999999999645, -21.85721834217820714 ) ) ;
#72499 = AXIS2_PLACEMENT_3D ( 'NONE', #62898, #79593, #23512 ) ;
#72500 = CARTESIAN_POINT ( 'NONE',  ( -73.37834811148371728, -60.32685699175659266, 129.0820052624678169 ) ) ;
#72501 = ORIENTED_EDGE ( 'NONE', *, *, #95117, .F. ) ;
#72502 =( NAMED_UNIT ( * ) PLANE_ANGLE_UNIT ( ) SI_UNIT ( $, .RADIAN. ) );
#72503 = DIRECTION ( 'NONE',  ( 0.000000000000000000, -1.000000000000000000, 0.000000000000000000 ) ) ;
#72504 = CARTESIAN_POINT ( 'NONE',  ( 92.08262379307400636, -57.61612071740184859, 204.3519813252348456 ) ) ;
#72505 = CARTESIAN_POINT ( 'NONE',  ( 0.000000000000000000, 0.000000000000000000, 0.000000000000000000 ) ) ;
#72506 = CARTESIAN_POINT ( 'NONE',  ( 30.76610509901443891, 309.0084209058028932, -8.583914624946309857 ) ) ;
#72507 = LINE ( 'NONE', #47162, #33929 ) ;
#72508 = ORIENTED_EDGE ( 'NONE', *, *, #26494, .F. ) ;
#72509 = CARTESIAN_POINT ( 'NONE',  ( 9.999999999999998224, 16.00000000000000000, -4.582575694955843382 ) ) ;
#72510 = DIRECTION ( 'NONE',  ( -1.000000000000000000, -1.224606353822377258E-16, -0.000000000000000000 ) ) ;
#72512 = CARTESIAN_POINT ( 'NONE',  ( -105.1034263385044198, -52.71031197673006830, 165.8127315669447910 ) ) ;
#72511 = CARTESIAN_POINT ( 'NONE',  ( -4.678819457397884740, 143.9212778189118467, 0.000000000000000000 ) ) ;
#72513 = CARTESIAN_POINT ( 'NONE',  ( 5.082755093536325930, -17.46875000204838457, -5.082755093536325042 ) ) ;
#72514 = CARTESIAN_POINT ( 'NONE',  ( 43.66784424859969960, 484.4037905981119820, 1.818048676808467823 ) ) ;
#72515 = CARTESIAN_POINT ( 'NONE',  ( 6.289692432696789126, -0.6629690750393453236, -6.828989928337168003 ) ) ;
#72516 = CARTESIAN_POINT ( 'NONE',  ( 5.787518022136032947, 41.99999999999999289, -59.87256586542197567 ) ) ;
#72517 = CARTESIAN_POINT ( 'NONE',  ( -7.894706624614592272, -0.7534108004406890879, -7.590222617908723102 ) ) ;
#72518 = FACE_OUTER_BOUND ( 'NONE', #57742, .T. ) ;
#72519 = EDGE_CURVE ( 'NONE', #65856, #104203, #38476, .T. ) ;
#72520 = B_SPLINE_CURVE_WITH_KNOTS ( 'NONE', 3,
 ( #70951, #96827, #29472, #14820, #6737, #38603, #62347, #79567, #4635, #95239, #22957, #105442, #71466, #104366, #63415, #72011 ),
 .UNSPECIFIED., .F., .F.,
 ( 4, 2, 2, 2, 2, 2, 2, 4 ),
 ( 0.003415289155120490843, 0.004063164684144634359, 0.004711040213168779175, 0.006006791271217062737, 0.007302542329265346299, 0.008598293387313628994, 0.01118979550341019785, 0.01378129761950676671 ),
 .UNSPECIFIED. ) ;
#72521 = ORIENTED_EDGE ( 'NONE', *, *, #51014, .T. ) ;
#72522 = CARTESIAN_POINT ( 'NONE',  ( -6.645513941704877858, 41.91298746401114528, -59.84148600730080858 ) ) ;
#72524 = CARTESIAN_POINT ( 'NONE',  ( 32.52394736240458428, -56.84213397606195883, 37.29594050141937345 ) ) ;
#72523 = CARTESIAN_POINT ( 'NONE',  ( -0.5839975711783412793, -70.55108709206167816, 13.00914722619329211 ) ) ;
#72525 = CARTESIAN_POINT ( 'NONE',  ( -23.21751746555244722, 25.25267828308493634, 33.20617127781060418 ) ) ;
#72526 = VERTEX_POINT ( 'NONE', #78905 ) ;
#72527 = EDGE_CURVE ( 'NONE', #102396, #95018, #105124, .T. ) ;
#72528 = EDGE_CURVE ( 'NONE', #4022, #49330, #29863, .T. ) ;
#72529 = ORIENTED_EDGE ( 'NONE', *, *, #7126, .F. ) ;
#72530 = CARTESIAN_POINT ( 'NONE',  ( 1.255263095696489281E-15, 51.26930509877138320, 10.24999999999999822 ) ) ;
#72531 = DIRECTION ( 'NONE',  ( 1.000000000000000000, 1.224606353822377258E-16, 0.000000000000000000 ) ) ;
#72532 = CARTESIAN_POINT ( 'NONE',  ( -8.000000000000000000, -19.53125000409677625, -3.313708498984762496 ) ) ;
#72533 = CARTESIAN_POINT ( 'NONE',  ( 0.000000000000000000, 0.000000000000000000, -3.393184225085859929 ) ) ;
#72534 = LINE ( 'NONE', #81148, #36642 ) ;
#72535 = ORIENTED_EDGE ( 'NONE', *, *, #45008, .T. ) ;
#72536 = CARTESIAN_POINT ( 'NONE',  ( 36.20485447879452323, -59.99999999999999289, -40.16702231068630624 ) ) ;
#72537 = CARTESIAN_POINT ( 'NONE',  ( 67.45855122657930281, -29.99999999999999289, 87.38540783980748472 ) ) ;
#72538 = AXIS2_PLACEMENT_3D ( 'NONE', #58422, #57867, #65973 ) ;
#72540 = DIRECTION ( 'NONE',  ( -1.000000000000000000, -1.224646799147353207E-16, 0.000000000000000000 ) ) ;
#72539 = VECTOR ( 'NONE', #59857, 1000.000000000000000 ) ;
#72541 = CARTESIAN_POINT ( 'NONE',  ( -11.69514296590343427, -5.000000000000000000, -81.87740575804689058 ) ) ;
#72542 = CARTESIAN_POINT ( 'NONE',  ( 48.02835407290504577, 9.771516447483525880, -16.85535821593549954 ) ) ;
#72543 = ORIENTED_EDGE ( 'NONE', *, *, #37396, .F. ) ;
#72544 = AXIS2_PLACEMENT_3D ( 'NONE', #98600, #23692, #41964 ) ;
#72545 = ORIENTED_EDGE ( 'NONE', *, *, #36422, .F. ) ;
#72546 = ORIENTED_EDGE ( 'NONE', *, *, #9014, .T. ) ;
#72547 = CARTESIAN_POINT ( 'NONE',  ( -32.69883954133502613, 464.5926484747980112, 16.74362576150847204 ) ) ;
#72548 = CARTESIAN_POINT ( 'NONE',  ( -33.21102376836597614, 438.9613914113129454, 23.92328486949907074 ) ) ;
#72549 = CARTESIAN_POINT ( 'NONE',  ( 32.97893058398564392, 361.9919399545990473, 22.73043233383004846 ) ) ;
#72551 = STYLED_ITEM ( 'NONE', ( #105537 ), #19597 ) ;
#72550 = CARTESIAN_POINT ( 'NONE',  ( -43.56702065117462297, 370.0667959703745851, 13.88062581363111470 ) ) ;
#72552 = CARTESIAN_POINT ( 'NONE',  ( -2.070413606167707421, -70.53207026027745030, 13.15197026184339713 ) ) ;
#72553 = CARTESIAN_POINT ( 'NONE',  ( -46.00000000000000000, 487.9838442367869220, -0.2095173675535702273 ) ) ;
#72554 = DIRECTION ( 'NONE',  ( -1.000000000000000000, -1.224606353822377258E-16, -0.000000000000000000 ) ) ;
#72555 = EDGE_LOOP ( 'NONE', ( #50605, #101705, #106450, #81867, #345 ) ) ;
#72556 = EDGE_CURVE ( 'NONE', #3450, #8490, #16916, .T. ) ;
#72557 = DIRECTION ( 'NONE',  ( 0.000000000000000000, 0.000000000000000000, 1.000000000000000000 ) ) ;
#72558 = AXIS2_PLACEMENT_3D ( 'NONE', #28048, #53348, #54370 ) ;
#72559 = ORIENTED_EDGE ( 'NONE', *, *, #84660, .T. ) ;
#72560 = DIRECTION ( 'NONE',  ( -1.000000000000000000, -1.224606353822377258E-16, -0.000000000000000000 ) ) ;
#72561 =( NAMED_UNIT ( * ) PLANE_ANGLE_UNIT ( ) SI_UNIT ( $, .RADIAN. ) );
#72562 = SURFACE_SIDE_STYLE ('',( #79595 ) ) ;
#72563 = EDGE_CURVE ( 'NONE', #41040, #38837, #97900, .T. ) ;
#72564 = CARTESIAN_POINT ( 'NONE',  ( -34.63715291467956092, -59.99999999999998579, 39.00976837571851519 ) ) ;
#72565 = CARTESIAN_POINT ( 'NONE',  ( 66.70725985424147098, -29.05557763954682926, 85.69813299201692303 ) ) ;
#72566 = ORIENTED_EDGE ( 'NONE', *, *, #16088, .T. ) ;
#72567 = CARTESIAN_POINT ( 'NONE',  ( 39.63576248123835910, 464.1159270358589879, 18.30995280209005927 ) ) ;
#72568 = DIRECTION ( 'NONE',  ( 0.000000000000000000, 1.000000000000000000, 0.000000000000000000 ) ) ;
#72569 = SURFACE_SIDE_STYLE ('',( #6233 ) ) ;
#72570 = VERTEX_POINT ( 'NONE', #55148 ) ;
#72571 = AXIS2_PLACEMENT_3D ( 'NONE', #687, #8286, #98364 ) ;
#72572 =( NAMED_UNIT ( * ) SI_UNIT ( $, .STERADIAN. ) SOLID_ANGLE_UNIT ( ) );
#72573 = CARTESIAN_POINT ( 'NONE',  ( 47.29386731606080474, 18.29473622528960064, 14.58939859131256256 ) ) ;
#72574 = STYLED_ITEM ( 'NONE', ( #87925 ), #93079 ) ;
#72575 = CARTESIAN_POINT ( 'NONE',  ( 0.000000000000000000, 274.9999999999999432, 0.000000000000000000 ) ) ;
#72576 = VECTOR ( 'NONE', #44223, 1000.000000000000000 ) ;
#72577 = CARTESIAN_POINT ( 'NONE',  ( -8.000000000000000000, -28.53125000409677270, -3.313708498984762496 ) ) ;
#72578 = CARTESIAN_POINT ( 'NONE',  ( -4.175893272573466319, -3.000000000000000000, -7.137815226411295733 ) ) ;
#72579 = CARTESIAN_POINT ( 'NONE',  ( 9.381394091586589212, 247.9865039441838519, 3.465950112474267542 ) ) ;
#72580 = CARTESIAN_POINT ( 'NONE',  ( 86.21108316312455599, -53.80016052557698458, 192.1608066663390844 ) ) ;
#72581 = CARTESIAN_POINT ( 'NONE',  ( 9.948181520647858989, 33.86892802760377919, 1.049088206181486349 ) ) ;
#72582 = CARTESIAN_POINT ( 'NONE',  ( 7.551437640244098581, -6.991275374770918205, -2.648272645923382296 ) ) ;
#72583 = FILL_AREA_STYLE_COLOUR ( '', #33214 ) ;
#72584 = ORIENTED_EDGE ( 'NONE', *, *, #29950, .T. ) ;
#72585 = DIRECTION ( 'NONE',  ( -1.000000000000000000, 0.000000000000000000, 0.000000000000000000 ) ) ;
#72586 = CARTESIAN_POINT ( 'NONE',  ( 17.08697247429566346, -60.00000000000000000, 39.92904733170480824 ) ) ;
#72587 = CARTESIAN_POINT ( 'NONE',  ( -91.20471926501998894, -30.00000000000000000, 190.5760516518613485 ) ) ;
#72589 = ADVANCED_FACE ( 'NONE', ( #64337 ), #99301, .F. ) ;
#72588 = AXIS2_PLACEMENT_3D ( 'NONE', #29481, #62357, #87158 ) ;
#72590 = LINE ( 'NONE', #55848, #89954 ) ;
#72591 = CARTESIAN_POINT ( 'NONE',  ( 52.19818328693233411, -57.67656952867285014, 83.25269862765968298 ) ) ;
#72593 = DIRECTION ( 'NONE',  ( -0.000000000000000000, -1.000000000000000000, -0.000000000000000000 ) ) ;
#72592 = DIRECTION ( 'NONE',  ( -1.000000000000000000, -1.224606353822377258E-16, -0.000000000000000000 ) ) ;
#72594 = EDGE_CURVE ( 'NONE', #57603, #5539, #89659, .T. ) ;
#72595 = ADVANCED_FACE ( 'NONE', ( #49722 ), #3579, .F. ) ;
#72596 = CARTESIAN_POINT ( 'NONE',  ( 0.000000000000000000, 152.0000000000000000, 5.000000000000000000 ) ) ;
#72597 = CARTESIAN_POINT ( 'NONE',  ( -32.16294467543131930, 464.8250491768795882, 14.67690201923579352 ) ) ;
#72598 = CARTESIAN_POINT ( 'NONE',  ( 59.89460441624491693, 4.898587196589294500E-16, -4.000000000000007105 ) ) ;
#72599 =( NAMED_UNIT ( * ) PLANE_ANGLE_UNIT ( ) SI_UNIT ( $, .RADIAN. ) );
#72600 = CARTESIAN_POINT ( 'NONE',  ( -25.22310183047458310, -60.00000000000000000, 41.23078497591944114 ) ) ;
#72601 = CARTESIAN_POINT ( 'NONE',  ( 14.29190075645216673, 6.456385560668102208, 7.561819230143447257 ) ) ;
#72602 = CARTESIAN_POINT ( 'NONE',  ( -86.48546161092085072, -17.02960564313559999, 183.8964038825536704 ) ) ;
#72603 = CIRCLE ( 'NONE', #69173, 13.50000000000000178 ) ;
#72604 = EDGE_LOOP ( 'NONE', ( #58584, #6871, #11100, #58657, #57093 ) ) ;
#72605 = CARTESIAN_POINT ( 'NONE',  ( 17.50000000000000355, 51.30660076970968930, 62.83706383107325166 ) ) ;
#72606 = CARTESIAN_POINT ( 'NONE',  ( 34.12241045381283300, 439.1279507012955037, 24.06036799111038604 ) ) ;
#72607 = CARTESIAN_POINT ( 'NONE',  ( -15.48413422138503037, -29.03194011403549624, 28.89617789578369411 ) ) ;
#72608 = EDGE_CURVE ( 'NONE', #43519, #29837, #25955, .T. ) ;
#72609 = CARTESIAN_POINT ( 'NONE',  ( 16.08349330513380337, 4.000000000000002665, 0.000000000000000000 ) ) ;
#72610 = AXIS2_PLACEMENT_3D ( 'NONE', #91039, #17144, #82924 ) ;
#72612 = CARTESIAN_POINT ( 'NONE',  ( 39.71334445446535000, 460.7040462571919193, 2.103363390004007627 ) ) ;
#72611 = CARTESIAN_POINT ( 'NONE',  ( 15.59999999999999787, 1.533819458162526451E-15, 0.000000000000000000 ) ) ;
#72613 = ORIENTED_EDGE ( 'NONE', *, *, #27391, .F. ) ;
#72614 = CARTESIAN_POINT ( 'NONE',  ( -7.499999907820173561, -3.000141485250358730, -20.99866594742747949 ) ) ;
#72615 = CARTESIAN_POINT ( 'NONE',  ( -7.986539162393899716, 33.97327171057451523, -0.5321833565149886036 ) ) ;
#72616 = STYLED_ITEM ( 'NONE', ( #97715 ), #20124 ) ;
#72617 = CYLINDRICAL_SURFACE ( 'NONE', #38194, 2.000000000000001776 ) ;
#72618 = AXIS2_PLACEMENT_3D ( 'NONE', #10112, #83466, #74829 ) ;
#72620 = CARTESIAN_POINT ( 'NONE',  ( -30.00000000000000000, 0.000000000000000000, 0.000000000000000000 ) ) ;
#72619 = B_SPLINE_CURVE_WITH_KNOTS ( 'NONE', 3,
 ( #83707, #2797, #100430, #25530 ),
 .UNSPECIFIED., .F., .F.,
 ( 4, 4 ),
 ( 0.4999999999999988898, 1.000000000000000000 ),
 .UNSPECIFIED. ) ;
#72621 = CARTESIAN_POINT ( 'NONE',  ( 73.56186416953940466, -60.00000000000000000, 167.8023059681976861 ) ) ;
#72622 = CARTESIAN_POINT ( 'NONE',  ( -1.103649760378013100, 53.60830983912105552, -9.608372721927825211 ) ) ;
#72623 = ORIENTED_EDGE ( 'NONE', *, *, #103836, .F. ) ;
#72624 = CARTESIAN_POINT ( 'NONE',  ( -0.2767341851108402473, -29.99999999999997868, 7.278698476187087429 ) ) ;
#72625 = DIRECTION ( 'NONE',  ( -1.000000000000000000, 0.000000000000000000, 0.000000000000000000 ) ) ;
#72627 = DIRECTION ( 'NONE',  ( -1.000000000000000000, -0.000000000000000000, -0.000000000000000000 ) ) ;
#72626 = CARTESIAN_POINT ( 'NONE',  ( 8.555523463203789092, -60.00000000000005684, 41.98724916707659816 ) ) ;
#72628 = CARTESIAN_POINT ( 'NONE',  ( -4.250000000000000000, 5.204748896376250699E-16, -10.00000000000000000 ) ) ;
#72629 = EDGE_LOOP ( 'NONE', ( #101864, #50957, #3314, #88380 ) ) ;
#72630 = CARTESIAN_POINT ( 'NONE',  ( -28.38881774565038896, 318.1718324713938273, 13.21570572201404303 ) ) ;
#72631 = EDGE_LOOP ( 'NONE', ( #55627, #3150, #73413 ) ) ;
#72632 = CARTESIAN_POINT ( 'NONE',  ( 20.42551034609843086, 304.8951776613778861, 8.946191631382156118 ) ) ;
#72633 = CARTESIAN_POINT ( 'NONE',  ( 3.827754797005777032, 15.98931925350938243, 9.240220675753764823 ) ) ;
#72634 = FACE_BOUND ( 'NONE', #86224, .T. ) ;
#72635 = CARTESIAN_POINT ( 'NONE',  ( -30.00000000000000000, 500.0000000000002274, 0.000000000000000000 ) ) ;
#72636 = ORIENTED_EDGE ( 'NONE', *, *, #80919, .T. ) ;
#72637 = SURFACE_STYLE_FILL_AREA ( #39761 ) ;
#72638 =( NAMED_UNIT ( * ) PLANE_ANGLE_UNIT ( ) SI_UNIT ( $, .RADIAN. ) );
#72640 = CARTESIAN_POINT ( 'NONE',  ( -78.30174078941652738, -60.00000000000486011, 197.9974431830838455 ) ) ;
#72639 = CIRCLE ( 'NONE', #103671, 8.000000000000000000 ) ;
#72641 = CARTESIAN_POINT ( 'NONE',  ( 6.167866516170009028, -1.339763354874886181, -6.500000000000000000 ) ) ;
#72642 = CARTESIAN_POINT ( 'NONE',  ( 75.98234489927602908, -60.00000000000001421, 186.9997704955459596 ) ) ;
#72643 = CARTESIAN_POINT ( 'NONE',  ( 7.036764705882352366, 40.00000000373363207, -71.06385277390853616 ) ) ;
#72644 = CARTESIAN_POINT ( 'NONE',  ( 0.000000000000000000, -2.000000000000000000, 9.500000000000000000 ) ) ;
#72646 = CARTESIAN_POINT ( 'NONE',  ( 13.17625921126869670, -18.58681922276355536, 27.05832475667332915 ) ) ;
#72645 = CARTESIAN_POINT ( 'NONE',  ( -108.8241353627135055, -30.00000000000001421, 157.0475095860343515 ) ) ;
#72648 = CARTESIAN_POINT ( 'NONE',  ( 101.6217879588726447, -38.00000000000002132, 186.1188645697355355 ) ) ;
#72647 = PRODUCT_DEFINITION_CONTEXT ( 'detailed design', #25254, 'design' ) ;
#72649 = CARTESIAN_POINT ( 'NONE',  ( 0.7827249903936659425, 54.19856013892794522, -8.012020349616371107 ) ) ;
#72650 = EDGE_CURVE ( 'NONE', #64937, #17510, #58643, .T. ) ;
#72651 = CARTESIAN_POINT ( 'NONE',  ( -46.35736043082792435, -56.81302380653085748, 50.30497149764946130 ) ) ;
#72652 = CIRCLE ( 'NONE', #26205, 3.000000000000026645 ) ;
#72653 = CARTESIAN_POINT ( 'NONE',  ( -7.980179952708205483E-13, 34.17188553057791722, -29.75000000000694911 ) ) ;
#72654 = ORIENTED_EDGE ( 'NONE', *, *, #98771, .T. ) ;
#72655 = SURFACE_STYLE_USAGE ( .BOTH. , #24147 ) ;
#72656 = CARTESIAN_POINT ( 'NONE',  ( -1.000000000001114220, -70.58759490697448769, 11.03128057732874190 ) ) ;
#72657 = CARTESIAN_POINT ( 'NONE',  ( -2.529110775640357911, -69.31258397332325671, 12.94914962940092629 ) ) ;
#72658 = CARTESIAN_POINT ( 'NONE',  ( 4.503026011213027147, -9.456581377166838109, 3.965236350746918159 ) ) ;
#72659 = FACE_BOUND ( 'NONE', #99608, .T. ) ;
#72660 = VERTEX_POINT ( 'NONE', #600 ) ;
#72661 = CARTESIAN_POINT ( 'NONE',  ( -16.75187969033554936, 37.11970326878314097, -21.80698433968595751 ) ) ;
#72662 = ORIENTED_EDGE ( 'NONE', *, *, #52751, .T. ) ;
#72663 = CARTESIAN_POINT ( 'NONE',  ( 101.9844698653622714, -29.99999999999932143, 198.1683824175306086 ) ) ;
#72664 = CARTESIAN_POINT ( 'NONE',  ( 6.492511067189947305, 41.78432740739263096, -59.03547063838888675 ) ) ;
#72665 = CARTESIAN_POINT ( 'NONE',  ( 93.60111843194438563, -30.00000000000000355, 109.5859247788262820 ) ) ;
#72666 = ADVANCED_FACE ( 'NONE', ( #89665 ), #79167, .T. ) ;
#72667 = CARTESIAN_POINT ( 'NONE',  ( 7.212408192734265810, 102.9848291067962975, -3.465038817813881789 ) ) ;
#72668 = ORIENTED_EDGE ( 'NONE', *, *, #71262, .T. ) ;
#72669 = B_SPLINE_CURVE_WITH_KNOTS ( 'NONE', 3,
 ( #104307, #47660, #23971, #56813 ),
 .UNSPECIFIED., .F., .F.,
 ( 4, 4 ),
 ( 6.871344576781776423E-17, 0.001856568542220787864 ),
 .UNSPECIFIED. ) ;
#72670 = ORIENTED_EDGE ( 'NONE', *, *, #63763, .F. ) ;
#72671 = ORIENTED_EDGE ( 'NONE', *, *, #88027, .T. ) ;
#72672 = CARTESIAN_POINT ( 'NONE',  ( -33.74271564777242816, 484.1802673187708592, 2.058285076122308155 ) ) ;
#72673 = CARTESIAN_POINT ( 'NONE',  ( 22.89018779209756005, 25.33046591275928705, 33.17343505111048074 ) ) ;
#72674 = DIRECTION ( 'NONE',  ( 1.000000000000000000, 1.224606353822377258E-16, 0.000000000000000000 ) ) ;
#72675 = ORIENTED_EDGE ( 'NONE', *, *, #75429, .T. ) ;
#72676 = CARTESIAN_POINT ( 'NONE',  ( 43.21649601278002706, 436.3330504929571703, 19.41248623753888580 ) ) ;
#72677 = ORIENTED_EDGE ( 'NONE', *, *, #25714, .F. ) ;
#72678 = DIRECTION ( 'NONE',  ( 0.000000000000000000, 0.000000000000000000, 1.000000000000000000 ) ) ;
#72679 = CARTESIAN_POINT ( 'NONE',  ( 79.75840094887199427, -38.76322012846202369, 192.5408423534894666 ) ) ;
#72680 = CARTESIAN_POINT ( 'NONE',  ( 11.94036525613893573, 10.81871501779890110, 9.774666796827323978 ) ) ;
#72682 = CARTESIAN_POINT ( 'NONE',  ( 7.000000000000000000, 0.000000000000000000, -11.82492182392400437 ) ) ;
#72681 = B_SPLINE_CURVE_WITH_KNOTS ( 'NONE', 3,
 ( #55884, #73139, #87771, #6828, #48342, #23582, #89882, #62959, #95860, #13853, #46765, #79661, #104464, #38692, #71558, #42386, #67739, #75280, #83912, #74742, #293, #25731, #76343, #90959, #1918, #82314, #75822, #34870, #100625, #1375, #58032, #24643, #49409, #26787 ),
 .UNSPECIFIED., .F., .F.,
 ( 4, 2, 2, 2, 2, 2, 2, 2, 2, 2, 2, 2, 2, 2, 2, 2, 4 ),
 ( 0.000000000000000000, 0.002123632632474287216, 0.004247265264948574433, 0.008494530529897148866, 0.01698906105979429426, 0.02548359158969144139, 0.03397812211958858852, 0.05096718317938292442, 0.06795624423917726031, 0.08494530529897158233, 0.1019343663587659321, 0.1104288968886631278, 0.1189234274185603096, 0.1274179579484575053, 0.1316652232134060962, 0.1337888558458803778, 0.1359124884783546594 ),
 .UNSPECIFIED. ) ;
#72683 = CARTESIAN_POINT ( 'NONE',  ( 38.96347140373135431, 313.4333200668041854, 6.407657066588297035 ) ) ;
#72684 = CARTESIAN_POINT ( 'NONE',  ( 1.625879232102889239E-15, 52.29617335651133914, 13.27631144943088692 ) ) ;
#72685 = ADVANCED_FACE ( 'NONE', ( #19002 ), #91151, .F. ) ;
#72686 = EDGE_CURVE ( 'NONE', #52389, #18709, #54129, .T. ) ;
#72687 = CARTESIAN_POINT ( 'NONE',  ( 64.78349330513380266, -4.000000000000000000, 4.898587196589421703E-16 ) ) ;
#72688 = MECHANICAL_DESIGN_GEOMETRIC_PRESENTATION_REPRESENTATION (  '', ( #36557 ), #100249 ) ;
#72689 = CARTESIAN_POINT ( 'NONE',  ( -40.26058501384667210, 460.2706387420201395, 2.258779328633529371 ) ) ;
#72690 = CIRCLE ( 'NONE', #48572, 4.172000000000001485 ) ;
#72691 = DIRECTION ( 'NONE',  ( 1.000000000000000000, 1.224606353822377258E-16, 0.000000000000000000 ) ) ;
#72692 = DIRECTION ( 'NONE',  ( 1.224646799147349509E-16, 0.000000000000000000, -1.000000000000000000 ) ) ;
#72693 =( NAMED_UNIT ( * ) PLANE_ANGLE_UNIT ( ) SI_UNIT ( $, .RADIAN. ) );
#72694 = EDGE_LOOP ( 'NONE', ( #86346, #22531, #72422, #5134 ) ) ;
#72695 = DIRECTION ( 'NONE',  ( -1.000000000000000000, 0.000000000000000000, 0.000000000000000000 ) ) ;
#72697 = CARTESIAN_POINT ( 'NONE',  ( -28.65514056416654398, 297.4037072407057281, 10.49742630379315322 ) ) ;
#72696 =( LENGTH_UNIT ( ) NAMED_UNIT ( * ) SI_UNIT ( .MILLI., .METRE. ) );
#72698 = CARTESIAN_POINT ( 'NONE',  ( -29.68315524077004852, -1.200000000000000030E-05, -42.10535821593474282 ) ) ;
#72699 = CARTESIAN_POINT ( 'NONE',  ( 105.5353273971932140, 1.030564683017419500E-14, 0.000000000000000000 ) ) ;
#72700 = CARTESIAN_POINT ( 'NONE',  ( 5.656854249492378806, -15.68749999999999289, 5.656854249492381470 ) ) ;
#72701 = CARTESIAN_POINT ( 'NONE',  ( 30.54121840989820669, -32.81349016368368154, 40.87587671059132077 ) ) ;
#72702 = STYLED_ITEM ( 'NONE', ( #59417 ), #20210 ) ;
#72703 =( LENGTH_UNIT ( ) NAMED_UNIT ( * ) SI_UNIT ( .MILLI., .METRE. ) );
#72704 = ORIENTED_EDGE ( 'NONE', *, *, #81, .T. ) ;
#72705 = CARTESIAN_POINT ( 'NONE',  ( 86.01665704136831891, -24.89204632129366246, 179.1268479360217327 ) ) ;
#72706 = SURFACE_SIDE_STYLE ('',( #17152 ) ) ;
#72707 = ORIENTED_EDGE ( 'NONE', *, *, #15874, .F. ) ;
#72708 = CARTESIAN_POINT ( 'NONE',  ( 94.41008270668507407, -57.67099569795677638, -0.2925677098450494840 ) ) ;
#72709 = CARTESIAN_POINT ( 'NONE',  ( 35.72538317320631052, 438.1659592258356497, 3.984952432984858017 ) ) ;
#72710 = DIRECTION ( 'NONE',  ( -1.000000000000000000, 0.000000000000000000, 0.000000000000000000 ) ) ;
#72711 = CARTESIAN_POINT ( 'NONE',  ( 28.61324058441463336, 13.48935699407724265, 40.19649855359969592 ) ) ;
#72712 = CIRCLE ( 'NONE', #81326, 0.5000000000000004441 ) ;
#72713 = CARTESIAN_POINT ( 'NONE',  ( 29.32938745888697696, 18.70033273455120693, 39.65510828929031817 ) ) ;
#72714 = CARTESIAN_POINT ( 'NONE',  ( 0.000000000000000000, -4.999999999999998224, 8.000000000000000000 ) ) ;
#72715 = DIRECTION ( 'NONE',  ( 0.000000000000000000, 0.000000000000000000, 1.000000000000000000 ) ) ;
#72717 = CARTESIAN_POINT ( 'NONE',  ( -13.39394377584697615, 3.642522405528196394, 6.675362191836228476 ) ) ;
#72716 = DIRECTION ( 'NONE',  ( -1.000000000000000000, -1.224606353822377258E-16, -0.000000000000000000 ) ) ;
#72718 = ORIENTED_EDGE ( 'NONE', *, *, #38944, .T. ) ;
#72719 = CARTESIAN_POINT ( 'NONE',  ( 9.675290556392710073, 294.8809879903661226, -10.04271151416038954 ) ) ;
#72720 = CARTESIAN_POINT ( 'NONE',  ( -10.50000000000000711, -5.000000000000000000, -55.73109925765190553 ) ) ;
#72721 = DIRECTION ( 'NONE',  ( 0.000000000000000000, -1.000000000000000000, 0.000000000000000000 ) ) ;
#72722 = CARTESIAN_POINT ( 'NONE',  ( 45.59999999999999432, 3.309500000000003439, 4.052968581778167743E-16 ) ) ;
#72723 =( GEOMETRIC_REPRESENTATION_CONTEXT ( 3 ) GLOBAL_UNCERTAINTY_ASSIGNED_CONTEXT ( ( #18985 ) ) GLOBAL_UNIT_ASSIGNED_CONTEXT ( ( #16984, #63954, #64477 ) ) REPRESENTATION_CONTEXT ( 'NONE', 'WORKASPACE' ) );
#72724 = CARTESIAN_POINT ( 'NONE',  ( 68.00294669520873470, -29.92123893200863094, -21.72257178417913792 ) ) ;
#72725 = ORIENTED_EDGE ( 'NONE', *, *, #78306, .T. ) ;
#72726 =( NAMED_UNIT ( * ) PLANE_ANGLE_UNIT ( ) SI_UNIT ( $, .RADIAN. ) );
#72727 = EDGE_CURVE ( 'NONE', #52295, #80390, #14208, .T. ) ;
#72728 = CARTESIAN_POINT ( 'NONE',  ( -10.67412802623772983, -16.34922207018503570, -34.75766904438820148 ) ) ;
#72729 = EDGE_CURVE ( 'NONE', #34601, #36282, #33375, .T. ) ;
#72731 = CARTESIAN_POINT ( 'NONE',  ( -63.67534439124898427, -60.22833768822253830, -28.64743048599374831 ) ) ;
#72730 = CARTESIAN_POINT ( 'NONE',  ( 40.73953790046563483, -18.92596047533412573, 20.36976895023281742 ) ) ;
#72732 = ORIENTED_EDGE ( 'NONE', *, *, #25340, .T. ) ;
#72733 = ORIENTED_EDGE ( 'NONE', *, *, #34407, .T. ) ;
#72734 = CARTESIAN_POINT ( 'NONE',  ( 0.1061556211655333148, 4.836380039389418961, -4.623144047065555817 ) ) ;
#72735 = DIRECTION ( 'NONE',  ( 0.000000000000000000, -1.000000000000000000, 0.000000000000000000 ) ) ;
#72736 = CARTESIAN_POINT ( 'NONE',  ( -92.46340183990984940, -59.99999999999999289, -0.7256272337619585899 ) ) ;
#72737 = VERTEX_POINT ( 'NONE', #81878 ) ;
#72738 = CARTESIAN_POINT ( 'NONE',  ( -4.852941176470586093, 40.00000000000132871, -70.80672828634229177 ) ) ;
#72739 = CARTESIAN_POINT ( 'NONE',  ( -9.090909090909093493, 16.00000000000000000, 4.165977904505304252 ) ) ;
#72740 = CARTESIAN_POINT ( 'NONE',  ( 95.99736947783486585, -37.71600262711182694, 192.9724029575287716 ) ) ;
#72742 = CARTESIAN_POINT ( 'NONE',  ( -16.64348903516517098, 45.88445698070336221, 4.157797401561652784 ) ) ;
#72741 = CARTESIAN_POINT ( 'NONE',  ( 28.86650669486618881, 4.000000000000003553, 4.898587196589414801E-16 ) ) ;
#72743 = CARTESIAN_POINT ( 'NONE',  ( -82.50772378166941223, -39.49606204731786363, 165.2126353373692496 ) ) ;
#72744 = ORIENTED_EDGE ( 'NONE', *, *, #78643, .T. ) ;
#72745 = ORIENTED_EDGE ( 'NONE', *, *, #85967, .F. ) ;
#72746 = AXIS2_PLACEMENT_3D ( 'NONE', #21563, #29668, #88931 ) ;
#72747 = VERTEX_POINT ( 'NONE', #73255 ) ;
#72748 = CARTESIAN_POINT ( 'NONE',  ( 27.33349330513380693, 4.000000000000003553, 0.000000000000000000 ) ) ;
#72749 = CARTESIAN_POINT ( 'NONE',  ( -5.959251246171386462, -13.44866041637656728, 13.58291813670143888 ) ) ;
#72751 = EDGE_LOOP ( 'NONE', ( #58758, #14631 ) ) ;
#72750 = B_SPLINE_CURVE_WITH_KNOTS ( 'NONE', 3,
 ( #56364, #39695, #73619, #49345, #65548, #71503 ),
 .UNSPECIFIED., .F., .F.,
 ( 4, 2, 4 ),
 ( -4.698498716301074466E-06, 0.0003457374136928007598, 0.0006961733261019026602 ),
 .UNSPECIFIED. ) ;
#72752 = DIRECTION ( 'NONE',  ( -1.000000000000000000, -1.224606353822377258E-16, -0.000000000000000000 ) ) ;
#72753 = CARTESIAN_POINT ( 'NONE',  ( -0.000000000000000000, 7.666536031838887766, -59.53359981990485750 ) ) ;
#72754 = DIRECTION ( 'NONE',  ( -1.000000000000000000, -1.224606353822377258E-16, -0.000000000000000000 ) ) ;
#72755 = CARTESIAN_POINT ( 'NONE',  ( -108.1850948662969216, -57.66112862901258751, 198.7856339303252753 ) ) ;
#72756 = CARTESIAN_POINT ( 'NONE',  ( -5.980543423763064581, -68.97096407501076953, -0.5500789318242859105 ) ) ;
#72757 = CARTESIAN_POINT ( 'NONE',  ( -17.49999999999999645, 2.500000000000000444, 0.000000000000000000 ) ) ;
#72758 = CARTESIAN_POINT ( 'NONE',  ( -28.76346532419124458, 309.5219921958590135, -8.933260212751790164 ) ) ;
#72759 = DIRECTION ( 'NONE',  ( 0.5735764363510466035, -0.8191520442889914655, 1.003171929053524500E-16 ) ) ;
#72760 = VECTOR ( 'NONE', #74117, 1000.000000000000000 ) ;
#72761 = CARTESIAN_POINT ( 'NONE',  ( -59.37491258674359784, -59.99999999999998579, -38.24906085379748788 ) ) ;
#72762 = CARTESIAN_POINT ( 'NONE',  ( -1.425880015568740777, -60.00000000000000711, 42.00000000000002132 ) ) ;
#72763 = EDGE_CURVE ( 'NONE', #89315, #81125, #24231, .T. ) ;
#72764 = CARTESIAN_POINT ( 'NONE',  ( -53.13873901080162909, -46.44135197877653809, 59.08599850147474086 ) ) ;
#72765 = CARTESIAN_POINT ( 'NONE',  ( 43.41290683822506935, 487.0833545439620593, 7.569976829064905210 ) ) ;
#72766 = VERTEX_POINT ( 'NONE', #40376 ) ;
#72767 = CARTESIAN_POINT ( 'NONE',  ( -95.34023284422563904, -37.68404846173547895, 193.0124814966931694 ) ) ;
#72768 = APPLICATION_CONTEXT ( 'automotive_design' ) ;
#72769 = CARTESIAN_POINT ( 'NONE',  ( -7.088826404115056157, 296.1964324881551534, -10.02186216631903370 ) ) ;
#72770 = EDGE_LOOP ( 'NONE', ( #82979, #105531, #12146, #51742, #32505, #26339 ) ) ;
#72771 = CARTESIAN_POINT ( 'NONE',  ( -17.08050361159542874, 34.19939120091158458, -24.26590151447872401 ) ) ;
#72772 = CARTESIAN_POINT ( 'NONE',  ( 91.31681156736948424, -38.36314778512125656, -2.424099829648139082 ) ) ;
#72773 = CARTESIAN_POINT ( 'NONE',  ( 48.99295625602575655, 13.11026251878881688, 16.41069188772014087 ) ) ;
#72774 = CARTESIAN_POINT ( 'NONE',  ( -2.977408999572654480, -11.00000000204838635, 7.188101187499999156 ) ) ;
#72775 = CARTESIAN_POINT ( 'NONE',  ( -13.70970213139414895, 294.5458219564956153, 9.871961192988456091 ) ) ;
#72776 = CARTESIAN_POINT ( 'NONE',  ( 10.11650669486618881, 1.474610560812782335E-15, 0.000000000000000000 ) ) ;
#72777 = CARTESIAN_POINT ( 'NONE',  ( 85.21185514236475456, -29.99999999999999645, 172.2923490395237707 ) ) ;
#72778 = DIRECTION ( 'NONE',  ( -1.000000000000000000, -1.224606353822377258E-16, -0.000000000000000000 ) ) ;
#72779 = CARTESIAN_POINT ( 'NONE',  ( 34.79468063551433232, 490.6633164237547930, 11.75004032468988235 ) ) ;
#72780 = EDGE_CURVE ( 'NONE', #98423, #24472, #19025, .T. ) ;
#72781 = CARTESIAN_POINT ( 'NONE',  ( 54.03872891708841308, -4.000000000000000000, 0.000000000000000000 ) ) ;
#72782 = DIRECTION ( 'NONE',  ( -0.000000000000000000, 0.000000000000000000, 1.000000000000000000 ) ) ;
#72783 = VERTEX_POINT ( 'NONE', #58705 ) ;
#72784 = ORIENTED_EDGE ( 'NONE', *, *, #55028, .T. ) ;
#72785 = CARTESIAN_POINT ( 'NONE',  ( 49.24857862907958150, -22.20931426737695702, 44.01793639162288230 ) ) ;
#72786 = AXIS2_PLACEMENT_3D ( 'NONE', #32669, #31088, #24578 ) ;
#72787 = CARTESIAN_POINT ( 'NONE',  ( 5.898965727403031600, 41.68848182032888872, -58.70906957313534491 ) ) ;
#72788 = DIRECTION ( 'NONE',  ( -8.673617379884035472E-17, -0.000000000000000000, -1.000000000000000000 ) ) ;
#72789 = ORIENTED_EDGE ( 'NONE', *, *, #103652, .T. ) ;
#72790 = CARTESIAN_POINT ( 'NONE',  ( -108.7991622881044123, -38.35665266207558943, 190.7632732821325874 ) ) ;
#72791 = ORIENTED_EDGE ( 'NONE', *, *, #3398, .T. ) ;
#72792 = CARTESIAN_POINT ( 'NONE',  ( 27.72754708733857854, 34.28370776901574857, -9.903118175739001217 ) ) ;
#72793 = CARTESIAN_POINT ( 'NONE',  ( 90.86072268490488568, -38.35173073395984744, 20.62671579895992835 ) ) ;
#72794 = CARTESIAN_POINT ( 'NONE',  ( 10.60908664556402137, 14.26876572314972158, -9.938912124272945903 ) ) ;
#72795 = FACE_OUTER_BOUND ( 'NONE', #80581, .T. ) ;
#72796 = CARTESIAN_POINT ( 'NONE',  ( -42.74438300981208982, 419.2451651247366158, 19.59905343518640919 ) ) ;
#72797 = CARTESIAN_POINT ( 'NONE',  ( 101.8886451212922566, -45.28289133281111134, 144.5137924623328729 ) ) ;
#72798 = CARTESIAN_POINT ( 'NONE',  ( 22.10829536976860510, 28.16405687208418485, 31.35662012625468265 ) ) ;
#72799 = CARTESIAN_POINT ( 'NONE',  ( -34.09307597759925557, 322.8769654760196772, -5.350189533808188180 ) ) ;
#72800 = CARTESIAN_POINT ( 'NONE',  ( 6.326592304916277776, 5.253140224433045624, -4.564380808752273033 ) ) ;
#72801 = CARTESIAN_POINT ( 'NONE',  ( 99.70625480700427090, -60.00000000000000000, 201.9673764616556184 ) ) ;
#72802 = EDGE_CURVE ( 'NONE', #45785, #84766, #57080, .T. ) ;
#72803 = ORIENTED_EDGE ( 'NONE', *, *, #54122, .T. ) ;
#72804 = CARTESIAN_POINT ( 'NONE',  ( 56.19429422314115641, -18.67854215501002813, 54.41800084858584086 ) ) ;
#72805 = ADVANCED_FACE ( 'NONE', ( #17713 ), #50573, .T. ) ;
#72806 = CARTESIAN_POINT ( 'NONE',  ( -29.28112164441576226, 307.0004567166486709, -9.064633347289211329 ) ) ;
#72807 = DIRECTION ( 'NONE',  ( -1.000000000000000000, -0.000000000000000000, -0.000000000000000000 ) ) ;
#72808 = CARTESIAN_POINT ( 'NONE',  ( -7.673189737795076404, -4.999999999999999112, -15.67457516869437129 ) ) ;
#72809 = VERTEX_POINT ( 'NONE', #106157 ) ;
#72811 = CARTESIAN_POINT ( 'NONE',  ( -14.89087697664241183, 23.12189093368899506, -0.5159772465389643736 ) ) ;
#72810 = CARTESIAN_POINT ( 'NONE',  ( -89.24293106356928718, -38.38520225817266152, -17.61820809038416513 ) ) ;
#72812 = CARTESIAN_POINT ( 'NONE',  ( 9.235395886531431551E-16, -3.000000000000000000, -8.000000000000000000 ) ) ;
#72813 = CARTESIAN_POINT ( 'NONE',  ( 25.05494358412147449, 307.4491500886443305, 9.528491992859288828 ) ) ;
#72814 = LINE ( 'NONE', #105721, #9266 ) ;
#72815 = CARTESIAN_POINT ( 'NONE',  ( -5.656854249492379694, -34.43749999999999289, -5.656854249492380582 ) ) ;
#72816 = FACE_OUTER_BOUND ( 'NONE', #7362, .T. ) ;
#72817 = EDGE_CURVE ( 'NONE', #102355, #62903, #15570, .T. ) ;
#72818 = EDGE_CURVE ( 'NONE', #59491, #14702, #16101, .T. ) ;
#72819 = ADVANCED_FACE ( 'NONE', ( #67011, #2786 ), #19562, .T. ) ;
#72820 = DIRECTION ( 'NONE',  ( -1.000000000000000000, -1.224606353822377258E-16, -0.000000000000000000 ) ) ;
#72821 = VERTEX_POINT ( 'NONE', #83699 ) ;
#72822 = CARTESIAN_POINT ( 'NONE',  ( 83.59357190745099331, -39.46543166661771807, 175.2130931883967833 ) ) ;
#72823 = CARTESIAN_POINT ( 'NONE',  ( 1.889203326810533268, -7.108778228558977119, -13.31560817771940108 ) ) ;
#72824 = CARTESIAN_POINT ( 'NONE',  ( 37.24697956223116080, 27.99412332198319220, 10.98691340867259036 ) ) ;
#72825 = ORIENTED_EDGE ( 'NONE', *, *, #105352, .F. ) ;
#72826 = VECTOR ( 'NONE', #61880, 1000.000000000000000 ) ;
#72827 = DIRECTION ( 'NONE',  ( 0.000000000000000000, -1.000000000000000000, 0.000000000000000000 ) ) ;
#72828 = EDGE_CURVE ( 'NONE', #14645, #70408, #42148, .T. ) ;
#72829 = CARTESIAN_POINT ( 'NONE',  ( 6.615712822706482754, -4.357054607612469432, -16.81429077417679707 ) ) ;
#72830 = CARTESIAN_POINT ( 'NONE',  ( 38.82068856954457203, 477.2421094490886162, -1.707083602274671374 ) ) ;
#72831 = CARTESIAN_POINT ( 'NONE',  ( 14.83962450834943780, 1.409789280635078468, 2.191244623890550081 ) ) ;
#72832 = CYLINDRICAL_SURFACE ( 'NONE', #78386, 4.000000000000000000 ) ;
#72833 = ORIENTED_EDGE ( 'NONE', *, *, #48668, .T. ) ;
#72834 = CIRCLE ( 'NONE', #100329, 13.27631144943088515 ) ;
#72835 = LINE ( 'NONE', #6510, #106428 ) ;
#72836 = CARTESIAN_POINT ( 'NONE',  ( 0.1683002306914084256, 26.07813853931758530, 38.24999999999999289 ) ) ;
#72838 = CARTESIAN_POINT ( 'NONE',  ( -10.70840817853610005, 12.38332293683050267, -9.999832067087631060 ) ) ;
#72837 = CARTESIAN_POINT ( 'NONE',  ( 7.251642494156181229, 41.54835750584383192, -68.91429206127320128 ) ) ;
#72839 = CARTESIAN_POINT ( 'NONE',  ( 7.188101187500000044, -11.65625000204838635, 0.000000000000000000 ) ) ;
#72840 = DIRECTION ( 'NONE',  ( 0.000000000000000000, 0.000000000000000000, 1.000000000000000000 ) ) ;
#72841 = ORIENTED_EDGE ( 'NONE', *, *, #36291, .T. ) ;
#72842 = LINE ( 'NONE', #48039, #62963 ) ;
#72843 = CARTESIAN_POINT ( 'NONE',  ( 23.38262301493118756, 25.94998521817065651, 30.71445628890077373 ) ) ;
#72844 = CARTESIAN_POINT ( 'NONE',  ( -9.434261306993260376, 141.8831429913814759, -5.000000000000000888 ) ) ;
#72845 =( BOUNDED_SURFACE ( )  B_SPLINE_SURFACE ( 2, 3, ( 
 ( #68325, #4119, #11658, #27911 ),
 ( #93665, #52652, #61843, #94193 ),
 ( #101219, #85583, #44589, #77478 ) ),
 .UNSPECIFIED., .F., .F., .F. ) 
 B_SPLINE_SURFACE_WITH_KNOTS ( ( 3, 3 ),
 ( 4, 4 ),
 ( 0.000000000000000000, 1.000000000000000000 ),
 ( -0.06873863542433759910, 1.530452813897690353E-17 ),
 .UNSPECIFIED. ) 
 GEOMETRIC_REPRESENTATION_ITEM ( )  RATIONAL_B_SPLINE_SURFACE ( (
 ( 1.000000000000000000, 1.000000000000000000, 1.000000000000000000, 1.000000000000000000),
 ( 1.857142857142858317, 1.857142857142858317, 1.857142857142858317, 1.857142857142858317),
 ( 1.000000000000000000, 1.000000000000000000, 1.000000000000000000, 1.000000000000000000) ) ) 
 REPRESENTATION_ITEM ( '' )  SURFACE ( )  );
#72846 = AXIS2_PLACEMENT_3D ( 'NONE', #104935, #89281, #41245 ) ;
#72847 = DIRECTION ( 'NONE',  ( 0.000000000000000000, -0.07486943176531161981, 0.9971933454386564533 ) ) ;
#72848 = EDGE_CURVE ( 'NONE', #14796, #90464, #75874, .T. ) ;
#72849 = CARTESIAN_POINT ( 'NONE',  ( 30.00000000000000000, 500.0000000000002274, 0.000000000000000000 ) ) ;
#72850 = ORIENTED_EDGE ( 'NONE', *, *, #86111, .F. ) ;
#72851 =( NAMED_UNIT ( * ) PLANE_ANGLE_UNIT ( ) SI_UNIT ( $, .RADIAN. ) );
#72852 = CARTESIAN_POINT ( 'NONE',  ( 61.37206225042174879, 6.856755485862130937E-15, 0.000000000000000000 ) ) ;
#72853 = AXIS2_PLACEMENT_3D ( 'NONE', #4257, #37726, #22051 ) ;
#72854 = ORIENTED_EDGE ( 'NONE', *, *, #51509, .T. ) ;
#72855 = ADVANCED_FACE ( 'NONE', ( #68060 ), #37960, .T. ) ;
#72856 = DIRECTION ( 'NONE',  ( 1.000000000000000000, 0.000000000000000000, 0.000000000000000000 ) ) ;
#72857 = CARTESIAN_POINT ( 'NONE',  ( 36.36650669486618881, 4.898587196589413815E-16, -4.000000000000000888 ) ) ;
#72858 = CARTESIAN_POINT ( 'NONE',  ( 27.61650669486618881, 1.474610560812782335E-15, 0.000000000000000000 ) ) ;
#72859 = UNCERTAINTY_MEASURE_WITH_UNIT (LENGTH_MEASURE( 1.000000000000000082E-05 ), #77263, 'distance_accuracy_value', 'NONE');
#72860 = CARTESIAN_POINT ( 'NONE',  ( -109.0244361759819327, -60.00000000000000000, 136.1499024773399924 ) ) ;
#72861 = B_SPLINE_CURVE_WITH_KNOTS ( 'NONE', 3,
 ( #19618, #84833, #43311, #77807, #84301, #28769, #53529, #52448, #77275, #35244 ),
 .UNSPECIFIED., .F., .F.,
 ( 4, 2, 2, 2, 4 ),
 ( -5.999999997985845112E-08, 0.002353756740120384067, 0.004707573480240747829, 0.009415206960481474485, 0.01883047392096293127 ),
 .UNSPECIFIED. ) ;
#72862 = CARTESIAN_POINT ( 'NONE',  ( 29.49662366984231454, 18.54149253525968533, -39.61409757040036084 ) ) ;
#72863 = CARTESIAN_POINT ( 'NONE',  ( 3.439834737513524090E-06, -25.54951635985603531, 28.14790268624504677 ) ) ;
#72864 = DIRECTION ( 'NONE',  ( -0.8660254037844373753, 0.5000000000000021094, 0.000000000000000000 ) ) ;
#72865 = CARTESIAN_POINT ( 'NONE',  ( -10.92479762610444638, 2.452360385479824600, 14.79862712302001881 ) ) ;
#72867 = CARTESIAN_POINT ( 'NONE',  ( 104.0908829527487711, 1.030564683017419500E-14, 0.000000000000000000 ) ) ;
#72866 = CARTESIAN_POINT ( 'NONE',  ( 9.596002107493083244, -5.000000000000002665, -77.62543935902139935 ) ) ;
#72868 = CARTESIAN_POINT ( 'NONE',  ( -81.16717396890126679, -60.54721624790309420, 184.2208889243687793 ) ) ;
#72869 = ORIENTED_EDGE ( 'NONE', *, *, #91651, .T. ) ;
#72870 = CYLINDRICAL_SURFACE ( 'NONE', #29845, 1.250000000000001110 ) ;
#72871 = VERTEX_POINT ( 'NONE', #1719 ) ;
#72872 = ORIENTED_EDGE ( 'NONE', *, *, #75107, .T. ) ;
#72873 = DIRECTION ( 'NONE',  ( 0.000000000000000000, -1.000000000000000000, 0.000000000000000000 ) ) ;
#72874 = EDGE_CURVE ( 'NONE', #76534, #106390, #60345, .T. ) ;
#72875 = DIRECTION ( 'NONE',  ( -0.000000000000000000, -1.000000000000000000, -0.000000000000000000 ) ) ;
#72876 = FACE_BOUND ( 'NONE', #67658, .T. ) ;
#72877 = CARTESIAN_POINT ( 'NONE',  ( 8.361479372609258220, 30.82354577482384173, -4.999999999999998224 ) ) ;
#72878 = CYLINDRICAL_SURFACE ( 'NONE', #21822, 22.55262289886175964 ) ;
#72879 = DIRECTION ( 'NONE',  ( 0.000000000000000000, -0.3420201433256725987, -0.9396926207859068736 ) ) ;
#72880 = CARTESIAN_POINT ( 'NONE',  ( 106.1778528577414704, -14.21045842199435150, 156.9945530843897075 ) ) ;
#72881 = CARTESIAN_POINT ( 'NONE',  ( -113.3391396720030428, -60.00000000000005684, 187.7090405971777898 ) ) ;
#72882 = EDGE_CURVE ( 'NONE', #65829, #29277, #14561, .T. ) ;
#72883 = CARTESIAN_POINT ( 'NONE',  ( -61.25147057187043487, -39.48936545682737176, 75.54103842554776804 ) ) ;
#72884 = ORIENTED_EDGE ( 'NONE', *, *, #78990, .F. ) ;
#72885 = CARTESIAN_POINT ( 'NONE',  ( -55.40281771843035585, 38.95363459860563182, 31.50562541889846102 ) ) ;
#72886 = CARTESIAN_POINT ( 'NONE',  ( 105.2797116528661974, -60.00000000000249401, 202.0183772298807412 ) ) ;
#72887 = EDGE_LOOP ( 'NONE', ( #62483, #56136, #28424, #65562, #67173 ) ) ;
#72888 = CARTESIAN_POINT ( 'NONE',  ( 13.45079846400083490, -54.26571488717375757, 23.11721482942555284 ) ) ;
#72889 = CARTESIAN_POINT ( 'NONE',  ( 2.977408999572650927, -13.25000000204838280, -7.188101187500000933 ) ) ;
#72890 = DIRECTION ( 'NONE',  ( 0.000000000000000000, 1.000000000000000000, 0.000000000000000000 ) ) ;
#72891 = ORIENTED_EDGE ( 'NONE', *, *, #19814, .F. ) ;
#72892 = CARTESIAN_POINT ( 'NONE',  ( 0.000000000000000000, 0.000000000000000000, 3.469446951953614189E-15 ) ) ;
#72893 = ORIENTED_EDGE ( 'NONE', *, *, #66454, .T. ) ;
#72894 = CARTESIAN_POINT ( 'NONE',  ( 10.61653353389823984, 45.33051817006433026, -15.36625836153913127 ) ) ;
#72895 = B_SPLINE_CURVE_WITH_KNOTS ( 'NONE', 3,
 ( #53478, #93941, #95017, #54503, #70188, #62126 ),
 .UNSPECIFIED., .F., .F.,
 ( 4, 2, 4 ),
 ( 0.000000000000000000, 0.0003491763592121710546, 0.0006983527184243421091 ),
 .UNSPECIFIED. ) ;
#72896 = CIRCLE ( 'NONE', #19545, 0.5000000000000004441 ) ;
#72897 = DIRECTION ( 'NONE',  ( -0.000000000000000000, -1.000000000000000000, -0.000000000000000000 ) ) ;
#72898 = CARTESIAN_POINT ( 'NONE',  ( -83.41754797870378013, -59.99999999999998579, 199.1391409242881139 ) ) ;
#72899 = CARTESIAN_POINT ( 'NONE',  ( 9.287587386881233087, -55.78087779922811507, 30.70844757271691350 ) ) ;
#72900 = CARTESIAN_POINT ( 'NONE',  ( -7.188101187500000044, -26.28125000204838813, -8.802885111219163269E-16 ) ) ;
#72901 = CARTESIAN_POINT ( 'NONE',  ( 37.83758010121639614, 485.6941950553124343, -4.518273513596184898 ) ) ;
#72902 = AXIS2_PLACEMENT_3D ( 'NONE', #27856, #53668, #86070 ) ;
#72903 = CARTESIAN_POINT ( 'NONE',  ( -4.000000000000000000, 18.12212560230942771, -5.744562646538041051 ) ) ;
#72904 = CARTESIAN_POINT ( 'NONE',  ( 0.000000000000000000, 6.123233995736770227E-16, -5.000000000000002665 ) ) ;
#72905 = CARTESIAN_POINT ( 'NONE',  ( -7.211357414135265209, 107.0114653993443596, 3.467230644691329466 ) ) ;
#72906 = EDGE_CURVE ( 'NONE', #60839, #51590, #101665, .T. ) ;
#72907 = CARTESIAN_POINT ( 'NONE',  ( -43.47452733440542261, 362.3092494624403912, 12.84014924004942415 ) ) ;
#72908 = CARTESIAN_POINT ( 'NONE',  ( 21.24454331354147385, 302.9514041099373571, -9.978735210106369991 ) ) ;
#72909 = CARTESIAN_POINT ( 'NONE',  ( -33.46790549732532583, -39.49766074888488276, 34.56548730633365807 ) ) ;
#72910 = FILL_AREA_STYLE ('',( #46534 ) ) ;
#72911 = AXIS2_PLACEMENT_3D ( 'NONE', #8482, #74278, #89937 ) ;
#72912 = CARTESIAN_POINT ( 'NONE',  ( 38.45571508739885758, -46.42947195434589247, 38.95870930491370387 ) ) ;
#72913 = CARTESIAN_POINT ( 'NONE',  ( 10.45706415778036025, -1.734723475976807094E-15, -13.60704923275195455 ) ) ;
#72914 = VERTEX_POINT ( 'NONE', #10863 ) ;
#72915 = DIRECTION ( 'NONE',  ( 1.000000000000000000, 0.000000000000000000, 0.000000000000000000 ) ) ;
#72916 = CARTESIAN_POINT ( 'NONE',  ( -73.93668673393140978, -38.32666573519513520, 159.8187507061171857 ) ) ;
#72917 = EDGE_LOOP ( 'NONE', ( #63335, #96320, #15384, #12416 ) ) ;
#72918 = CARTESIAN_POINT ( 'NONE',  ( 43.74855578046756222, 328.6220886837048170, -1.765109843966993441 ) ) ;
#72919 = DIRECTION ( 'NONE',  ( -1.000000000000000000, 0.000000000000000000, 0.000000000000000000 ) ) ;
#72920 = CARTESIAN_POINT ( 'NONE',  ( 6.692649838135033669, 4.003395468798082391, 6.852343244299697211 ) ) ;
#72921 = CARTESIAN_POINT ( 'NONE',  ( -4.472135954999578722, -65.00000000000000000, -4.000000000000002665 ) ) ;
#72922 = DIRECTION ( 'NONE',  ( 0.000000000000000000, 1.000000000000000000, 0.000000000000000000 ) ) ;
#72923 = CARTESIAN_POINT ( 'NONE',  ( -31.37379325839373934, 432.3256879030839741, 23.18622107664128151 ) ) ;
#72924 = CARTESIAN_POINT ( 'NONE',  ( -5.000000000000001776, -46.28716247248784299, 42.58845726811990318 ) ) ;
#72925 = B_SPLINE_CURVE_WITH_KNOTS ( 'NONE', 3,
 ( #19220, #91469, #18666, #51520, #9455, #75255, #52050, #8932 ),
 .UNSPECIFIED., .F., .F.,
 ( 4, 2, 2, 4 ),
 ( 2.384759638366321710E-15, 0.01120533138725377485, 0.01680799708087945751, 0.02241066277450514191 ),
 .UNSPECIFIED. ) ;
#72926 = CARTESIAN_POINT ( 'NONE',  ( 100.3075067269979428, -59.99999999999999289, 82.82790229349259903 ) ) ;
#72927 = CARTESIAN_POINT ( 'NONE',  ( -6.967015948558341165, -46.95078337943017743, 39.14357484227694783 ) ) ;
#72928 = CIRCLE ( 'NONE', #90198, 4.000000000000001776 ) ;
#72929 = CARTESIAN_POINT ( 'NONE',  ( 14.83349330513380693, -4.000000000000000888, 4.898587196589416773E-16 ) ) ;
#72930 = DIRECTION ( 'NONE',  ( -1.000000000000000000, -1.224606353822377258E-16, -0.000000000000000000 ) ) ;
#72931 = VERTEX_POINT ( 'NONE', #100953 ) ;
#72932 = ADVANCED_FACE ( 'NONE', ( #84780 ), #50790, .T. ) ;
#72933 = STYLED_ITEM ( 'NONE', ( #5085 ), #18881 ) ;
#72934 = CARTESIAN_POINT ( 'NONE',  ( -83.36175203672824807, -30.00000000000000000, 155.5103389558694289 ) ) ;
#72935 = ORIENTED_EDGE ( 'NONE', *, *, #84367, .T. ) ;
#72936 = LINE ( 'NONE', #15778, #40095 ) ;
#72937 = CARTESIAN_POINT ( 'NONE',  ( -16.05785784214673484, 4.775831776474317003, -3.710403933782549846 ) ) ;
#72938 = CARTESIAN_POINT ( 'NONE',  ( 4.086459164111219344, 13.71066660893832712, 5.000000000000000000 ) ) ;
#72939 = DIRECTION ( 'NONE',  ( -1.000000000000000000, -1.224606353822377258E-16, -0.000000000000000000 ) ) ;
#72940 = CARTESIAN_POINT ( 'NONE',  ( 9.999945253488240482, 26.00013686629467458, -0.2662901834230989584 ) ) ;
#72941 = VECTOR ( 'NONE', #56770, 1000.000000000000000 ) ;
#72942 = CARTESIAN_POINT ( 'NONE',  ( 7.188101187500001821, -23.93750000204838457, -2.977408999572650483 ) ) ;
#72943 = CARTESIAN_POINT ( 'NONE',  ( 8.572527594031486009E-16, 0.000000000000000000, 7.000000000000011546 ) ) ;
#72944 =( NAMED_UNIT ( * ) SI_UNIT ( $, .STERADIAN. ) SOLID_ANGLE_UNIT ( ) );
#72946 = EDGE_CURVE ( 'NONE', #58641, #105730, #22480, .T. ) ;
#72945 = CARTESIAN_POINT ( 'NONE',  ( 7.168070102805851995, 40.56150966784696976, -70.87151302692181787 ) ) ;
#72947 = VERTEX_POINT ( 'NONE', #68617 ) ;
#72949 = VERTEX_POINT ( 'NONE', #27652 ) ;
#72948 = CARTESIAN_POINT ( 'NONE',  ( -7.380470314495000572, 40.84001257084522507, -58.87769989985683594 ) ) ;
#72950 = CARTESIAN_POINT ( 'NONE',  ( 79.97290194383445794, -49.90522762054754224, 158.2806676109657928 ) ) ;
#72951 = CARTESIAN_POINT ( 'NONE',  ( 46.00000000000000000, 450.0000000000002274, 13.20242257375370976 ) ) ;
#72952 = CARTESIAN_POINT ( 'NONE',  ( -38.74274399182664297, 27.39031700910832967, -11.77456647869184359 ) ) ;
#72953 = ORIENTED_EDGE ( 'NONE', *, *, #18230, .F. ) ;
#72954 = EDGE_CURVE ( 'NONE', #44189, #55983, #24321, .T. ) ;
#72955 = CARTESIAN_POINT ( 'NONE',  ( -56.15634551241206651, 50.00000000000000000, 28.58296655959290433 ) ) ;
#72956 = CARTESIAN_POINT ( 'NONE',  ( -0.5328921654508612660, 13.17767128240470065, -51.63731992219727118 ) ) ;
#72957 = CARTESIAN_POINT ( 'NONE',  ( 7.188101187499999156, -10.25000000204838813, 2.977408999572654924 ) ) ;
#72958 = DIRECTION ( 'NONE',  ( 0.000000000000000000, 0.000000000000000000, 1.000000000000000000 ) ) ;
#72959 = CARTESIAN_POINT ( 'NONE',  ( -56.21986590610479340, -57.67573674557218766, 94.99882904018191709 ) ) ;
#72960 = CARTESIAN_POINT ( 'NONE',  ( 6.463481858019718196, -4.600809706232204199, -5.711197301637628065 ) ) ;
#72961 = EDGE_LOOP ( 'NONE', ( #33969, #62646, #37993 ) ) ;
#72962 = SHAPE_REPRESENTATION_RELATIONSHIP ( 'NONE' , 'NONE' ,  #58557, #94875 ) ;
#72963 = CARTESIAN_POINT ( 'NONE',  ( 0.000000000000000000, 0.000000000000000000, 0.000000000000000000 ) ) ;
#72964 = CARTESIAN_POINT ( 'NONE',  ( 3.443309072005628746, 124.1408101220383600, 5.000000000000000000 ) ) ;
#72965 = CARTESIAN_POINT ( 'NONE',  ( 7.423110160291532367, 40.85353811916601785, -59.12022462436053161 ) ) ;
#72966 = ORIENTED_EDGE ( 'NONE', *, *, #106484, .F. ) ;
#72967 = CARTESIAN_POINT ( 'NONE',  ( -8.000000000000000000, -10.53125000409677092, -3.313708498984762496 ) ) ;
#72968 = CARTESIAN_POINT ( 'NONE',  ( -14.15215018753299780, -14.92673834348265061, 31.67970770892681287 ) ) ;
#72969 =( NAMED_UNIT ( * ) SI_UNIT ( $, .STERADIAN. ) SOLID_ANGLE_UNIT ( ) );
#72970 = CIRCLE ( 'NONE', #11001, 5.000000000000011546 ) ;
#72971 = DIRECTION ( 'NONE',  ( 0.000000000000000000, 0.000000000000000000, 1.000000000000000000 ) ) ;
#72972 = CARTESIAN_POINT ( 'NONE',  ( 18.09999999999999787, 1.533819458162526451E-15, 0.000000000000000000 ) ) ;
#72973 = CARTESIAN_POINT ( 'NONE',  ( 33.66103144839009786, 439.0639482787724432, 24.00889586765897832 ) ) ;
#72974 = COLOUR_RGB ( '', 0.08235294, 0.09019608, 0.10196078) ;
#72975 = APPLICATION_PROTOCOL_DEFINITION ( 'draft international standard', 'automotive_design', 1998, #17676 ) ;
#72976 = CARTESIAN_POINT ( 'NONE',  ( 48.98943663899292744, 7.951733423214422558, 16.40652009737647887 ) ) ;
#72977 = ORIENTED_EDGE ( 'NONE', *, *, #16901, .F. ) ;
#72978 = DIRECTION ( 'NONE',  ( -0.000000000000000000, -1.000000000000000000, -0.000000000000000000 ) ) ;
#72979 = CARTESIAN_POINT ( 'NONE',  ( 14.55921722940514229, 43.46947890857538255, -90.48438549608371773 ) ) ;
#72980 = FACE_OUTER_BOUND ( 'NONE', #38323, .T. ) ;
#72981 = CARTESIAN_POINT ( 'NONE',  ( -3.778422651548678068, -48.87976032229202872, 103.2432416460067799 ) ) ;
#72982 = EDGE_CURVE ( 'NONE', #93975, #79044, #10389, .T. ) ;
#72983 = EDGE_LOOP ( 'NONE', ( #39831, #14648, #83443, #102146 ) ) ;
#72984 = CARTESIAN_POINT ( 'NONE',  ( -43.51330286016842308, 435.7669547662763989, 8.554287073375030914 ) ) ;
#72985 = CARTESIAN_POINT ( 'NONE',  ( 105.3688122440774464, -57.64581400391074339, 201.4821763970232098 ) ) ;
#72986 = EDGE_CURVE ( 'NONE', #78613, #67620, #9050, .T. ) ;
#72987 = CARTESIAN_POINT ( 'NONE',  ( 36.57468857844234122, 463.9816243198107486, 19.61678995109879864 ) ) ;
#72988 = CARTESIAN_POINT ( 'NONE',  ( -9.797648506390736145, 51.31151531669312504, -2.590383122573969299 ) ) ;
#72989 = CARTESIAN_POINT ( 'NONE',  ( 59.41111111111111143, 6.915964383211875250E-15, 0.000000000000000000 ) ) ;
#72990 = CARTESIAN_POINT ( 'NONE',  ( -73.48687785542945505, -60.00000000000000711, 167.0610275913660416 ) ) ;
#72991 = CARTESIAN_POINT ( 'NONE',  ( -45.48003679188781234, 379.8448106960472614, 7.220331889307936457 ) ) ;
#72992 = CYLINDRICAL_SURFACE ( 'NONE', #71743, 7.499999999992679633 ) ;
#72993 = CARTESIAN_POINT ( 'NONE',  ( -41.58649125062324003, 315.0454808444952732, -5.157136739135766312 ) ) ;
#72994 = CARTESIAN_POINT ( 'NONE',  ( -83.95403480896771953, -53.78288136489426563, 188.7750542527096798 ) ) ;
#72996 = ORIENTED_EDGE ( 'NONE', *, *, #46707, .T. ) ;
#72995 = CIRCLE ( 'NONE', #69566, 65.00000000000000000 ) ;
#72997 = CARTESIAN_POINT ( 'NONE',  ( 29.35909118268796192, 310.5218271128537140, -8.690052357984560771 ) ) ;
#72998 = ORIENTED_EDGE ( 'NONE', *, *, #6457, .T. ) ;
#72999 = FACE_OUTER_BOUND ( 'NONE', #106477, .T. ) ;
#73000 = FILL_AREA_STYLE ('',( #57349 ) ) ;
#73001 = STYLED_ITEM ( 'NONE', ( #44212 ), #1016 ) ;
#73002 = CONICAL_SURFACE ( 'NONE', #71331, 4.172000000000009479, 0.9599310885968813656 ) ;
#73003 = CARTESIAN_POINT ( 'NONE',  ( -83.69066969828963920, -52.72359143521253344, -15.75783544347118159 ) ) ;
#73004 = FACE_OUTER_BOUND ( 'NONE', #68780, .T. ) ;
#73005 = CARTESIAN_POINT ( 'NONE',  ( 13.86650669486618881, 4.000000000000003553, 4.898587196589414801E-16 ) ) ;
#73006 = ORIENTED_EDGE ( 'NONE', *, *, #87722, .T. ) ;
#73007 = CARTESIAN_POINT ( 'NONE',  ( -1.907451454365918675, -0.1079931744079098421, 102.2322703247678248 ) ) ;
#73008 = CARTESIAN_POINT ( 'NONE',  ( 7.063836239582370169, 41.16939439637754816, -58.51215209214867485 ) ) ;
#73009 = CARTESIAN_POINT ( 'NONE',  ( 16.57301948837260497, -3.469446951953614189E-15, -4.453875240779963107 ) ) ;
#73010 = DIRECTION ( 'NONE',  ( -1.000000000000000000, -1.224606353822377258E-16, -0.000000000000000000 ) ) ;
#73011 = CARTESIAN_POINT ( 'NONE',  ( 89.53125762993630588, -30.00000000000007461, -13.19907884436577561 ) ) ;
#73012 = CARTESIAN_POINT ( 'NONE',  ( -79.40447720853664748, -22.14626824436577124, 126.4748337375811786 ) ) ;
#73013 = EDGE_LOOP ( 'NONE', ( #46143, #33374, #57968, #52753, #89257, #15974 ) ) ;
#73014 = CARTESIAN_POINT ( 'NONE',  ( 4.090242245409069888, -14.21045842199428932, 34.36068907045891763 ) ) ;
#73015 = CARTESIAN_POINT ( 'NONE',  ( 7.344133061198929724, 87.44494392680577732, 3.176267128233873027 ) ) ;
#73016 = CARTESIAN_POINT ( 'NONE',  ( 94.65517944311366705, -57.65681286589507692, -9.358892355265044927 ) ) ;
#73017 = DIRECTION ( 'NONE',  ( -0.5735764363510494901, -0.8191520442889894671, 0.000000000000000000 ) ) ;
#73018 = CARTESIAN_POINT ( 'NONE',  ( -30.00000000000000000, 461.8802764867013479, 14.89328939273681662 ) ) ;
#73019 = ORIENTED_EDGE ( 'NONE', *, *, #41160, .F. ) ;
#73020 = B_SPLINE_CURVE_WITH_KNOTS ( 'NONE', 3,
 ( #46920, #15083, #6452, #82885, #104629, #87930 ),
 .UNSPECIFIED., .F., .F.,
 ( 4, 2, 4 ),
 ( 0.006874058789394425426, 0.008773169699889938472, 0.01067228061038545325 ),
 .UNSPECIFIED. ) ;
#73021 = FACE_OUTER_BOUND ( 'NONE', #84181, .T. ) ;
#73022 = CARTESIAN_POINT ( 'NONE',  ( 0.000000000000000000, 0.000000000000000000, 3.469446951953614189E-15 ) ) ;
#73023 = CARTESIAN_POINT ( 'NONE',  ( 32.33349330513379982, 1.593028355512270567E-15, 0.000000000000000000 ) ) ;
#73024 = CARTESIAN_POINT ( 'NONE',  ( 7.188101187500001821, -22.06250000204838813, -2.977408999572650483 ) ) ;
#73025 = CARTESIAN_POINT ( 'NONE',  ( 7.848314987057849024, -4.129027267381569999, -7.493854785173811095 ) ) ;
#73026 = CARTESIAN_POINT ( 'NONE',  ( 9.220915120640585272, 83.95545113567915507, -3.870126578504838655 ) ) ;
#73027 = DIRECTION ( 'NONE',  ( -1.000000000000000000, -0.000000000000000000, -0.000000000000000000 ) ) ;
#73028 = LINE ( 'NONE', #67094, #4923 ) ;
#73029 = CARTESIAN_POINT ( 'NONE',  ( -8.000000000000000000, -13.53125000409676915, -3.313708498984762496 ) ) ;
#73030 = AXIS2_PLACEMENT_3D ( 'NONE', #50247, #91783, #90180 ) ;
#73031 = ORIENTED_EDGE ( 'NONE', *, *, #42489, .T. ) ;
#73032 = DIRECTION ( 'NONE',  ( -1.000000000000000000, -1.224606353822377258E-16, -0.000000000000000000 ) ) ;
#73034 = CARTESIAN_POINT ( 'NONE',  ( 28.08771105297372728, -29.05517447130626962, 30.69056992575482568 ) ) ;
#73033 = CARTESIAN_POINT ( 'NONE',  ( -31.71194513525783165, -14.21045842199430709, 37.70210531190891601 ) ) ;
#73035 = CARTESIAN_POINT ( 'NONE',  ( 23.84378987346994805, 27.93349636785022483, -30.86234801138825645 ) ) ;
#73036 = ORIENTED_EDGE ( 'NONE', *, *, #93374, .F. ) ;
#73037 = AXIS2_PLACEMENT_3D ( 'NONE', #5803, #89399, #103445 ) ;
#73038 = VERTEX_POINT ( 'NONE', #86920 ) ;
#73039 = CARTESIAN_POINT ( 'NONE',  ( 0.4137165646001804142, 52.15082680420621841, 7.817459332776711456 ) ) ;
#73040 = CARTESIAN_POINT ( 'NONE',  ( -16.04053133235774808, 302.5635519178338768, -10.06124968053929436 ) ) ;
#73041 = CIRCLE ( 'NONE', #74740, 5.000000000000010658 ) ;
#73042 = CARTESIAN_POINT ( 'NONE',  ( -5.656854249492379694, -19.62500000409677270, -5.656854249492380582 ) ) ;
#73043 = DIRECTION ( 'NONE',  ( 1.000000000000000000, 1.224606353822377258E-16, 0.000000000000000000 ) ) ;
#73044 = CARTESIAN_POINT ( 'NONE',  ( -7.500000000000000000, 0.7513028741560141555, -0.02472015219302758221 ) ) ;
#73045 = VERTEX_POINT ( 'NONE', #37860 ) ;
#73046 = CARTESIAN_POINT ( 'NONE',  ( 65.38219241326270037, -59.99999999999999289, -34.08627437347746536 ) ) ;
#73047 = CARTESIAN_POINT ( 'NONE',  ( 23.21751746555220564, 25.25267828308493634, -33.20617127781077471 ) ) ;
#73048 = COLOUR_RGB ( '', 0.09019608, 0.27058824, 0.51372549) ;
#73049 = CARTESIAN_POINT ( 'NONE',  ( -85.18896233714281152, -59.99999999999995737, -15.68185129854840554 ) ) ;
#73050 = CARTESIAN_POINT ( 'NONE',  ( 60.14984002819952025, 4.898587196589294500E-16, -4.000000000000007105 ) ) ;
#73051 = CARTESIAN_POINT ( 'NONE',  ( 46.92658635379572729, 13.66002169525850007, -15.01004073971110486 ) ) ;
#73052 = ORIENTED_EDGE ( 'NONE', *, *, #18492, .F. ) ;
#73053 = EDGE_CURVE ( 'NONE', #16354, #103853, #86289, .T. ) ;
#73054 = B_SPLINE_CURVE_WITH_KNOTS ( 'NONE', 3,
 ( #39243, #5788, #105546, #31684, #80198, #64570, #6845, #14391, #39769, #55901, #73157, #96415, #97437, #47303, #89379, #88837, #23062, #6303, #31167, #32209 ),
 .UNSPECIFIED., .F., .F.,
 ( 4, 2, 2, 2, 2, 2, 2, 2, 2, 4 ),
 ( 0.003321483407199190673, 0.003825559474142698705, 0.004077597507614457058, 0.004329635541086214977, 0.004833711608029716070, 0.005337787674973218030, 0.005841863741916719990, 0.006345939808860221951, 0.006850015875803723911, 0.007354091942747225871 ),
 .UNSPECIFIED. ) ;
#73055 = EDGE_LOOP ( 'NONE', ( #12290, #4665, #102019, #34355, #15508 ) ) ;
#73056 = ORIENTED_EDGE ( 'NONE', *, *, #13948, .T. ) ;
#73057 = CARTESIAN_POINT ( 'NONE',  ( -27.99999999999999645, 0.000000000000000000, 0.000000000000000000 ) ) ;
#73058 = CARTESIAN_POINT ( 'NONE',  ( 44.30296249756166560, 485.3595172641092290, 2.292223182636803802 ) ) ;
#73059 = CARTESIAN_POINT ( 'NONE',  ( -37.75731493300575181, 438.6148476127195863, 23.62858942192393386 ) ) ;
#73060 = CARTESIAN_POINT ( 'NONE',  ( 24.83612219788692244, 304.4592009172700386, 10.29129484861557309 ) ) ;
#73061 = CARTESIAN_POINT ( 'NONE',  ( -44.33586564007308795, 336.2641261982522565, -0.002537273210375349999 ) ) ;
#73062 = CARTESIAN_POINT ( 'NONE',  ( -5.789193319501154456, -65.08511655608099034, 14.25240442334545676 ) ) ;
#73063 = CARTESIAN_POINT ( 'NONE',  ( -44.13666298176345038, 485.5987328015601179, 3.573899382266691127 ) ) ;
#73064 = CARTESIAN_POINT ( 'NONE',  ( -2.637755229554568666E-21, 53.39766064372320642, -10.24999999999999822 ) ) ;
#73065 = VERTEX_POINT ( 'NONE', #71759 ) ;
#73066 = CARTESIAN_POINT ( 'NONE',  ( 30.88008372391074730, 8.315965929874641560, 41.22858563418517264 ) ) ;
#73067 = ORIENTED_EDGE ( 'NONE', *, *, #44818, .F. ) ;
#73068 = CARTESIAN_POINT ( 'NONE',  ( -46.00000000000000000, 500.0000000000002274, -5.000000000000001776 ) ) ;
#73069 = CARTESIAN_POINT ( 'NONE',  ( -39.83118896912314000, 485.8577528566776209, -4.999724294280131431 ) ) ;
#73070 = CARTESIAN_POINT ( 'NONE',  ( -72.90163493338778267, -60.00000000000000711, 126.5439322136281675 ) ) ;
#73071 = CARTESIAN_POINT ( 'NONE',  ( 67.99901078833072177, -29.05790011282407193, 89.58219462804794375 ) ) ;
#73072 = AXIS2_PLACEMENT_3D ( 'NONE', #77633, #62522, #3753 ) ;
#73073 = ORIENTED_EDGE ( 'NONE', *, *, #75294, .F. ) ;
#73074 = EDGE_CURVE ( 'NONE', #9279, #50002, #44866, .T. ) ;
#73075 = CARTESIAN_POINT ( 'NONE',  ( -7.439122753854266357, 41.00341855746702180, -68.91429205792265122 ) ) ;
#73076 = CARTESIAN_POINT ( 'NONE',  ( -32.94331731755182346, 463.6330061646623335, 6.942105804440992678 ) ) ;
#73077 = AXIS2_PLACEMENT_3D ( 'NONE', #89825, #24583, #48280 ) ;
#73078 = CARTESIAN_POINT ( 'NONE',  ( -53.00838388237266940, -57.67116150918030115, -39.31046371713402721 ) ) ;
#73079 = PRODUCT_DEFINITION_FORMATION_WITH_SPECIFIED_SOURCE ( 'ANY', '', #101508, .NOT_KNOWN. ) ;
#73080 = VERTEX_POINT ( 'NONE', #104670 ) ;
#73081 =( NAMED_UNIT ( * ) PLANE_ANGLE_UNIT ( ) SI_UNIT ( $, .RADIAN. ) );
#73082 = CARTESIAN_POINT ( 'NONE',  ( 0.000000000000000000, 0.000000000000000000, -2.342872917771300578 ) ) ;
#73083 = CARTESIAN_POINT ( 'NONE',  ( -36.22417390465002285, 491.4095951024455076, 12.30556361669862042 ) ) ;
#73084 = CARTESIAN_POINT ( 'NONE',  ( -8.000000000000001776, -28.34375000409677270, 3.313708498984758943 ) ) ;
#73085 =( NAMED_UNIT ( * ) PLANE_ANGLE_UNIT ( ) SI_UNIT ( $, .RADIAN. ) );
#73086 = CARTESIAN_POINT ( 'NONE',  ( 60.14984002819952025, -4.000000000000000000, 0.000000000000000000 ) ) ;
#73087 = CARTESIAN_POINT ( 'NONE',  ( 9.797936955406312265, 33.46671689770484193, -2.012343231877598448 ) ) ;
#73088 = CARTESIAN_POINT ( 'NONE',  ( 13.50000000000000355, 0.6589394956329810427, -9.910285482875310023E-16 ) ) ;
#73089 = CARTESIAN_POINT ( 'NONE',  ( 18.20175014771579569, 303.6397678898111394, 9.891910565086597273 ) ) ;
#73090 = VERTEX_POINT ( 'NONE', #45395 ) ;
#73091 = CARTESIAN_POINT ( 'NONE',  ( -8.000000000000000000, -10.24999999999999112, -9.797174393178825657E-16 ) ) ;
#73092 = LINE ( 'NONE', #81719, #82393 ) ;
#73093 = CARTESIAN_POINT ( 'NONE',  ( -92.31907403475642582, -30.00000000000000355, 190.9581983028909349 ) ) ;
#73094 = EDGE_CURVE ( 'NONE', #100024, #88304, #84578, .T. ) ;
#73095 = AXIS2_PLACEMENT_3D ( 'NONE', #104248, #72417, #38486 ) ;
#73096 = DIRECTION ( 'NONE',  ( -0.000000000000000000, -0.000000000000000000, -1.000000000000000000 ) ) ;
#73097 = CARTESIAN_POINT ( 'NONE',  ( 53.06187785988736749, -57.67613140857140763, 85.70582740418153378 ) ) ;
#73099 = CARTESIAN_POINT ( 'NONE',  ( -9.306508628549350348, 53.68076281443192954, 1.765973350150533916 ) ) ;
#73098 = CARTESIAN_POINT ( 'NONE',  ( -20.00000000000000000, 12.99999999999999289, 6.999999999999999112 ) ) ;
#73100 = ADVANCED_FACE ( 'NONE', ( #77755 ), #5965, .F. ) ;
#73101 = EDGE_CURVE ( 'NONE', #43534, #66536, #93939, .T. ) ;
#73102 = CARTESIAN_POINT ( 'NONE',  ( -39.16821133293855439, 459.8632445465567571, 1.901232704179571575 ) ) ;
#73103 = B_SPLINE_CURVE_WITH_KNOTS ( 'NONE', 3,
 ( #5073, #88640, #40090, #38006, #55709 ),
 .UNSPECIFIED., .F., .F.,
 ( 4, 1, 4 ),
 ( 0.000000000000000000, 0.003752776749732572234, 0.007505553499465144468 ),
 .UNSPECIFIED. ) ;
#73104 = CARTESIAN_POINT ( 'NONE',  ( 44.00013453485157555, 465.7974093566498937, 11.65569858486426824 ) ) ;
#73105 = AXIS2_PLACEMENT_3D ( 'NONE', #75001, #24900, #49132 ) ;
#73106 = CARTESIAN_POINT ( 'NONE',  ( 29.68315524077034695, -1.200000000000000030E-05, 39.60535821593451544 ) ) ;
#73107 = CARTESIAN_POINT ( 'NONE',  ( -16.64288181053317928, -60.00000000000000000, 39.89607924062331534 ) ) ;
#73108 = MECHANICAL_DESIGN_GEOMETRIC_PRESENTATION_REPRESENTATION (  '', ( #12847 ), #97234 ) ;
#73109 = AXIS2_PLACEMENT_3D ( 'NONE', #89215, #82707, #98358 ) ;
#73110 = STYLED_ITEM ( 'NONE', ( #99431 ), #42019 ) ;
#73111 = DIRECTION ( 'NONE',  ( -1.000000000000000000, -0.000000000000000000, -0.000000000000000000 ) ) ;
#73112 = CARTESIAN_POINT ( 'NONE',  ( 6.400188988269344570, 53.43406968874433716, 7.879101709558080202 ) ) ;
#73113 =( GEOMETRIC_REPRESENTATION_CONTEXT ( 3 ) GLOBAL_UNCERTAINTY_ASSIGNED_CONTEXT ( ( #91893 ) ) GLOBAL_UNIT_ASSIGNED_CONTEXT ( ( #93905, #18440, #19528 ) ) REPRESENTATION_CONTEXT ( 'NONE', 'WORKASPACE' ) );
#73114 = CARTESIAN_POINT ( 'NONE',  ( -86.51221272467716972, -53.78683390949667142, 192.4548174909675708 ) ) ;
#73115 = ORIENTED_EDGE ( 'NONE', *, *, #74349, .F. ) ;
#73116 = CARTESIAN_POINT ( 'NONE',  ( 17.50000000000104805, 48.96861188084124450, 62.56461476143844891 ) ) ;
#73117 = CARTESIAN_POINT ( 'NONE',  ( 11.55908542073290945, -8.827506715863462361, 19.09556135803124377 ) ) ;
#73118 = CARTESIAN_POINT ( 'NONE',  ( -5.972684422919853020, -18.58610353171744123, 26.97790868950432497 ) ) ;
#73119 = MECHANICAL_DESIGN_GEOMETRIC_PRESENTATION_REPRESENTATION (  '', ( #69778 ), #26693 ) ;
#73120 = CARTESIAN_POINT ( 'NONE',  ( 0.000000000000000000, 0.000000000000000000, 0.000000000000000000 ) ) ;
#73121 = EDGE_CURVE ( 'NONE', #51590, #71639, #3867, .T. ) ;
#73122 = DIRECTION ( 'NONE',  ( 0.000000000000000000, -1.000000000000000000, 0.000000000000000000 ) ) ;
#73123 = ORIENTED_EDGE ( 'NONE', *, *, #92736, .T. ) ;
#73124 = ADVANCED_FACE ( 'NONE', ( #95016 ), #98344, .T. ) ;
#73125 = CARTESIAN_POINT ( 'NONE',  ( -7.340594533191627136, -3.410200195908305254, -18.44125947282421407 ) ) ;
#73126 = DIRECTION ( 'NONE',  ( -1.000000000000000000, -1.224606353822377258E-16, -0.000000000000000000 ) ) ;
#73127 = CARTESIAN_POINT ( 'NONE',  ( 29.29475614497689762, 307.0157710316811404, -9.061019955416419691 ) ) ;
#73128 = CARTESIAN_POINT ( 'NONE',  ( 0.000000000000000000, 0.000000000000000000, 0.000000000000000000 ) ) ;
#73129 = ADVANCED_FACE ( 'NONE', ( #79857 ), #38375, .T. ) ;
#73130 = CARTESIAN_POINT ( 'NONE',  ( -7.002990960197232440, -83.94733181616541629, 3.868040364119523566 ) ) ;
#73131 = CARTESIAN_POINT ( 'NONE',  ( 70.25724432519014329, -60.00000000000000000, 142.8801060964537726 ) ) ;
#73132 = CARTESIAN_POINT ( 'NONE',  ( -45.29905483860081716, 480.9466865490944656, -2.171671249451534003 ) ) ;
#73133 = VERTEX_POINT ( 'NONE', #49073 ) ;
#73134 = DIRECTION ( 'NONE',  ( -1.000000000000000000, 0.000000000000000000, 0.000000000000000000 ) ) ;
#73135 = FILL_AREA_STYLE ('',( #55368 ) ) ;
#73137 = CARTESIAN_POINT ( 'NONE',  ( 5.833333333333329485, -4.000000000000003553, 103.8776713793258608 ) ) ;
#73136 = CARTESIAN_POINT ( 'NONE',  ( 40.90273407096766078, -60.00000000000019185, 57.82174102673914007 ) ) ;
#73138 = EDGE_CURVE ( 'NONE', #5546, #33098, #1861, .T. ) ;
#73139 = CARTESIAN_POINT ( 'NONE',  ( 4.560915367935560738, 143.2206717247628944, -4.999999999999999112 ) ) ;
#73140 = CARTESIAN_POINT ( 'NONE',  ( -4.902312018371978830, -3.082176157930676563, 103.3400275729950835 ) ) ;
#73141 = EDGE_LOOP ( 'NONE', ( #106666, #67779, #78627, #53715, #14981 ) ) ;
#73142 = CARTESIAN_POINT ( 'NONE',  ( -24.51502932331456108, 306.8928289099468998, 10.39682823628861108 ) ) ;
#73143 = ORIENTED_EDGE ( 'NONE', *, *, #56773, .T. ) ;
#73145 = FILL_AREA_STYLE_COLOUR ( '', #17303 ) ;
#73144 =( BOUNDED_SURFACE ( )  B_SPLINE_SURFACE ( 3, 2, ( 
 ( #27657, #60530, #3336 ),
 ( #75620, #61052, #11943 ),
 ( #44872, #28709, #61591 ),
 ( #1724, #34675, #94487 ),
 ( #67547, #20642, #59461 ),
 ( #84252, #10349, #70191 ),
 ( #86925, #46962, #37865 ),
 ( #63711, #80388, #5968 ),
 ( #23251, #104674, #71242 ),
 ( #104140, #97109, #95020 ) ),
 .UNSPECIFIED., .F., .F., .T. ) 
 B_SPLINE_SURFACE_WITH_KNOTS ( ( 4, 2, 2, 2, 4 ),
 ( 3, 3 ),
 ( 0.006110147660070369691, 0.007140910106245465863, 0.008171672552420562036, 0.009202434998595659943, 0.01023319744477075612 ),
 ( 0.000000000000000000, 0.8503742053513317911 ),
 .UNSPECIFIED. ) 
 GEOMETRIC_REPRESENTATION_ITEM ( )  RATIONAL_B_SPLINE_SURFACE ( (
 ( 1.000000000000000000, 0.7509311617978130515, 0.9254657543235544903),
 ( 1.000000000000000000, 0.7661071201673247399, 0.9300071839847410260),
 ( 1.000000000000000000, 0.7795789861866246895, 0.9340386613018172302),
 ( 1.000000000000000000, 0.8013757198166023832, 0.9405613684820788301),
 ( 1.000000000000000000, 0.8096851085567824402, 0.9430479662686670483),
 ( 1.000000000000000000, 0.8194567880828296236, 0.9459721568969409189),
 ( 1.000000000000000000, 0.8208804111421099670, 0.9463981783599909603),
 ( 1.000000000000000000, 0.8160668081439683696, 0.9449577000125506387),
 ( 1.000000000000000000, 0.8098474096059313787, 0.9430965351155695675),
 ( 1.000000000000000000, 0.8002676374315798036, 0.9402297730672883880) ) ) 
 REPRESENTATION_ITEM ( '' )  SURFACE ( )  );
#73146 = AXIS2_PLACEMENT_3D ( 'NONE', #67157, #100042, #101111 ) ;
#73147 = CARTESIAN_POINT ( 'NONE',  ( 31.22567349391626124, 439.6199880051409536, 23.21640098373832117 ) ) ;
#73148 =( LENGTH_UNIT ( ) NAMED_UNIT ( * ) SI_UNIT ( .MILLI., .METRE. ) );
#73149 = ORIENTED_EDGE ( 'NONE', *, *, #14992, .T. ) ;
#73150 = PRODUCT_DEFINITION_FORMATION_WITH_SPECIFIED_SOURCE ( 'ANY', '', #79411, .NOT_KNOWN. ) ;
#73151 = CARTESIAN_POINT ( 'NONE',  ( 64.32759900501075379, 49.99999999999999289, -11.06576400629166912 ) ) ;
#73152 = CARTESIAN_POINT ( 'NONE',  ( -9.787739683274441660, 7.346124691387062811, -1.606086870082999107 ) ) ;
#73153 = CARTESIAN_POINT ( 'NONE',  ( -31.10001900035964439, -60.00000000000245848, 46.36770439546862121 ) ) ;
#73154 = CARTESIAN_POINT ( 'NONE',  ( 46.00000000000000000, 438.2642212955902323, 10.59429296198023707 ) ) ;
#73155 = CARTESIAN_POINT ( 'NONE',  ( 52.67981547313412705, -60.00000000000002842, 78.74676858557705827 ) ) ;
#73156 = CARTESIAN_POINT ( 'NONE',  ( 6.683837171061803417, 3.955946848495959234, -6.851900933636991375 ) ) ;
#73157 = CARTESIAN_POINT ( 'NONE',  ( 1.250014052124106323, 25.67358186333530767, -39.34165713028683342 ) ) ;
#73159 = CARTESIAN_POINT ( 'NONE',  ( 18.02386892498230964, -46.43468589485836873, 31.95930805262861440 ) ) ;
#73158 = CARTESIAN_POINT ( 'NONE',  ( -108.8021899934185086, -29.99999999999995026, 184.6878429379334534 ) ) ;
#73160 = DIRECTION ( 'NONE',  ( 0.000000000000000000, 0.000000000000000000, 1.000000000000000000 ) ) ;
#73161 = CARTESIAN_POINT ( 'NONE',  ( 1.008786712439213362, 54.10551997402946256, -8.244280760490370952 ) ) ;
#73162 = CARTESIAN_POINT ( 'NONE',  ( -44.80343625002662833, -42.98650238651817546, 44.34706117140887471 ) ) ;
#73163 = DIRECTION ( 'NONE',  ( -1.000000000000000000, -1.224606353822377258E-16, -0.000000000000000000 ) ) ;
#73164 = ORIENTED_EDGE ( 'NONE', *, *, #101156, .T. ) ;
#73165 = LINE ( 'NONE', #106070, #30191 ) ;
#73166 = CARTESIAN_POINT ( 'NONE',  ( 0.2573354458087839247, 6.889406814520512512, -1.067197363239225760 ) ) ;
#73167 = SURFACE_STYLE_USAGE ( .BOTH. , #33287 ) ;
#73168 = DIRECTION ( 'NONE',  ( -1.000000000000000000, -1.224606353822377258E-16, -0.000000000000000000 ) ) ;
#73169 = DIRECTION ( 'NONE',  ( 0.000000000000000000, 0.000000000000000000, 1.000000000000000000 ) ) ;
#73170 = VERTEX_POINT ( 'NONE', #23248 ) ;
#73171 = CARTESIAN_POINT ( 'NONE',  ( -16.66870162890457863, 37.13814613750710691, -21.80698433968596106 ) ) ;
#73172 = ORIENTED_EDGE ( 'NONE', *, *, #103942, .T. ) ;
#73173 = CARTESIAN_POINT ( 'NONE',  ( 94.54924656135277417, -30.00000000000334310, 199.9234823381102899 ) ) ;
#73174 = CARTESIAN_POINT ( 'NONE',  ( 14.91270732344407257, 41.98564553269472555, -86.62216337287246404 ) ) ;
#73175 = CARTESIAN_POINT ( 'NONE',  ( 5.908324287552553677, 41.91795896428032364, -59.12627191402334148 ) ) ;
#73176 = CARTESIAN_POINT ( 'NONE',  ( -3.659159783247727057E-15, 10.71892156097790583, -14.93965356295127478 ) ) ;
#73177 = CARTESIAN_POINT ( 'NONE',  ( 94.35141610110464683, -30.00000000000000355, 114.0755648428526001 ) ) ;
#73178 = CARTESIAN_POINT ( 'NONE',  ( 7.934883677559675164, 101.1316082206244715, 1.051380792122692753 ) ) ;
#73179 = ORIENTED_EDGE ( 'NONE', *, *, #18259, .T. ) ;
#73180 = EDGE_CURVE ( 'NONE', #55436, #74451, #77647, .T. ) ;
#73181 = CIRCLE ( 'NONE', #88765, 4.000000000000000888 ) ;
#73182 = ORIENTED_EDGE ( 'NONE', *, *, #40207, .F. ) ;
#73183 = ORIENTED_EDGE ( 'NONE', *, *, #44294, .T. ) ;
#73184 = DIRECTION ( 'NONE',  ( 0.000000000000000000, 0.000000000000000000, 1.000000000000000000 ) ) ;
#73185 = CARTESIAN_POINT ( 'NONE',  ( -1.678777966127334764, -5.952373502067780819, -13.77784384362900738 ) ) ;
#73186 = AXIS2_PLACEMENT_3D ( 'NONE', #41374, #82898, #57012 ) ;
#73187 =( LENGTH_UNIT ( ) NAMED_UNIT ( * ) SI_UNIT ( .MILLI., .METRE. ) );
#73188 = EDGE_CURVE ( 'NONE', #93736, #68089, #49614, .T. ) ;
#73189 = ORIENTED_EDGE ( 'NONE', *, *, #46713, .T. ) ;
#73191 = EDGE_CURVE ( 'NONE', #93942, #16556, #93127, .T. ) ;
#73190 = CARTESIAN_POINT ( 'NONE',  ( 42.69811214730273008, 434.9611672192513652, 18.34625614733207755 ) ) ;
#73192 = ORIENTED_EDGE ( 'NONE', *, *, #61290, .T. ) ;
#73193 = CYLINDRICAL_SURFACE ( 'NONE', #75898, 5.000000000000002665 ) ;
#73194 = CARTESIAN_POINT ( 'NONE',  ( 78.85737667306543131, -38.67488751151257276, 190.5950933815901749 ) ) ;
#73195 = CARTESIAN_POINT ( 'NONE',  ( 10.88890915545092142, 9.027303679840910533, 10.01895505698042754 ) ) ;
#73196 = COLOUR_RGB ( '', 0.72549020, 0.75294118, 0.79215686) ;
#73197 = FACE_OUTER_BOUND ( 'NONE', #2876, .T. ) ;
#73198 =( GEOMETRIC_REPRESENTATION_CONTEXT ( 3 ) GLOBAL_UNCERTAINTY_ASSIGNED_CONTEXT ( ( #23482 ) ) GLOBAL_UNIT_ASSIGNED_CONTEXT ( ( #79981, #7154, #72944 ) ) REPRESENTATION_CONTEXT ( 'NONE', 'WORKASPACE' ) );
#73199 = CARTESIAN_POINT ( 'NONE',  ( 38.54753914444563634, 311.7982143856372659, 5.994412429555442401 ) ) ;
#73200 = AXIS2_PLACEMENT_3D ( 'NONE', #68409, #75418, #58168 ) ;
#73201 = CARTESIAN_POINT ( 'NONE',  ( 12.21253585067004543, 1.340359594676612611E-15, 0.000000000000000000 ) ) ;
#73202 = EDGE_CURVE ( 'NONE', #88625, #75902, #7921, .T. ) ;
#73203 = CIRCLE ( 'NONE', #40493, 4.999999999999999112 ) ;
#73204 = EDGE_CURVE ( 'NONE', #94186, #12693, #27717, .T. ) ;
#73205 =( NAMED_UNIT ( * ) PLANE_ANGLE_UNIT ( ) SI_UNIT ( $, .RADIAN. ) );
#73206 = CIRCLE ( 'NONE', #31893, 7.500000000000000888 ) ;
#73207 = ADVANCED_FACE ( 'NONE', ( #106784 ), #98270, .T. ) ;
#73208 = CARTESIAN_POINT ( 'NONE',  ( -40.53119313125447576, 460.3380581626501566, 2.322614769218545039 ) ) ;
#73209 = CARTESIAN_POINT ( 'NONE',  ( -5.000000000093224983, -46.22753318115157128, 103.2791840072271157 ) ) ;
#73210 = DIRECTION ( 'NONE',  ( -1.000000000000000000, 0.000000000000000000, 0.000000000000000000 ) ) ;
#73211 = FACE_OUTER_BOUND ( 'NONE', #66286, .T. ) ;
#73212 = ORIENTED_EDGE ( 'NONE', *, *, #51491, .T. ) ;
#73213 = DIRECTION ( 'NONE',  ( -0.000000000000000000, -0.000000000000000000, 1.000000000000000000 ) ) ;
#73215 = CARTESIAN_POINT ( 'NONE',  ( -30.53534817441637017, 298.8129631075795487, 10.81987346015778328 ) ) ;
#73214 = SURFACE_STYLE_FILL_AREA ( #98037 ) ;
#73216 = CARTESIAN_POINT ( 'NONE',  ( -12.45393346519286837, -3.927217745177864927, -76.72514752459275655 ) ) ;
#73217 = CARTESIAN_POINT ( 'NONE',  ( -5.656854249492379694, -16.43749999999999289, -5.656854249492380582 ) ) ;
#73218 = CARTESIAN_POINT ( 'NONE',  ( 5.128989308823689974, -18.61194742579494132, 35.09291343390540874 ) ) ;
#73219 = CARTESIAN_POINT ( 'NONE',  ( 5.281083960078516881, 298.2116408387686874, 8.506842287730004060 ) ) ;
#73220 = ORIENTED_EDGE ( 'NONE', *, *, #42893, .T. ) ;
#73221 = CARTESIAN_POINT ( 'NONE',  ( 84.67559614028348847, -50.18795068039596430, 188.5560178073191082 ) ) ;
#73222 = DIRECTION ( 'NONE',  ( 0.000000000000000000, 0.000000000000000000, 1.000000000000000000 ) ) ;
#73223 = DIRECTION ( 'NONE',  ( -1.000000000000000000, -1.224606353822377258E-16, -0.000000000000000000 ) ) ;
#73224 = ORIENTED_EDGE ( 'NONE', *, *, #57590, .T. ) ;
#73225 = CARTESIAN_POINT ( 'NONE',  ( 83.08230946783562842, -57.67107110472222331, -28.35002488624179406 ) ) ;
#73226 = FACE_OUTER_BOUND ( 'NONE', #10810, .T. ) ;
#73227 =( NAMED_UNIT ( * ) SI_UNIT ( $, .STERADIAN. ) SOLID_ANGLE_UNIT ( ) );
#73228 = CARTESIAN_POINT ( 'NONE',  ( 104.9555555555555486, 4.172000000000019249, 0.000000000000000000 ) ) ;
#73229 = AXIS2_PLACEMENT_3D ( 'NONE', #61071, #86424, #11963 ) ;
#73230 = CARTESIAN_POINT ( 'NONE',  ( -54.55306156724233091, -38.00000000000002132, 58.68193799101367603 ) ) ;
#73231 = CARTESIAN_POINT ( 'NONE',  ( -4.175893272574851878, -3.000000000000000000, 7.137815226409915503 ) ) ;
#73232 = CARTESIAN_POINT ( 'NONE',  ( 5.500000036871884213, 42.00000000000000000, -68.91429207046176941 ) ) ;
#73234 = CARTESIAN_POINT ( 'NONE',  ( -15.99999999999008438, 4.197692598242061202, 4.745459346044129667 ) ) ;
#73233 =( NAMED_UNIT ( * ) PLANE_ANGLE_UNIT ( ) SI_UNIT ( $, .RADIAN. ) );
#73235 = EDGE_CURVE ( 'NONE', #20907, #32853, #29747, .T. ) ;
#73236 = CARTESIAN_POINT ( 'NONE',  ( 101.2019940638598854, 5.000000000000020428, 0.000000000000000000 ) ) ;
#73237 = CARTESIAN_POINT ( 'NONE',  ( -31.35230430510937794, 438.7809062751878173, 22.96768963798378138 ) ) ;
#73238 = CARTESIAN_POINT ( 'NONE',  ( -9.036570576874968452, -10.37119081301011647, -0.1387913946425914369 ) ) ;
#73239 = CARTESIAN_POINT ( 'NONE',  ( -27.10511071441333542, 36.88665068479732412, -7.556984339679825524 ) ) ;
#73240 = CARTESIAN_POINT ( 'NONE',  ( 9.700350089084272653, 15.75268258782372754, -2.455962139888437701 ) ) ;
#73241 = CARTESIAN_POINT ( 'NONE',  ( 0.000000000000000000, 0.000000000000000000, -55.00000000000000000 ) ) ;
#73242 = CARTESIAN_POINT ( 'NONE',  ( 33.70841932975964994, 485.0774894644218875, 1.934193826885746814 ) ) ;
#73243 = CIRCLE ( 'NONE', #97364, 4.000000000000000000 ) ;
#73244 = ORIENTED_EDGE ( 'NONE', *, *, #2521, .T. ) ;
#73245 = DIRECTION ( 'NONE',  ( 0.5735764363510490460, 0.8191520442889896891, 0.000000000000000000 ) ) ;
#73246 = CARTESIAN_POINT ( 'NONE',  ( 0.000000000000000000, 34.00000000000000711, 0.000000000000000000 ) ) ;
#73247 = CARTESIAN_POINT ( 'NONE',  ( -12.84829414594153718, -16.74545646077213235, -34.56912337068381902 ) ) ;
#73248 = EDGE_CURVE ( 'NONE', #7327, #25681, #12197, .T. ) ;
#73250 = CARTESIAN_POINT ( 'NONE',  ( -64.34419054092482781, -47.40884698333244529, -26.19182566128564105 ) ) ;
#73249 = DIRECTION ( 'NONE',  ( -1.000000000000000000, 0.000000000000000000, 0.000000000000000000 ) ) ;
#73251 = CIRCLE ( 'NONE', #35511, 12.00000000000000711 ) ;
#73252 = EDGE_LOOP ( 'NONE', ( #86989, #84925, #23659, #71377, #8419, #98432 ) ) ;
#73253 = B_SPLINE_CURVE_WITH_KNOTS ( 'NONE', 3,
 ( #6853, #7375, #40288, #65095, #16012, #22554, #81785, #55394, #68296, #41876, #61689, #10046, #58612, #99035, #10571, #74765, #43487, #25201, #84478, #53567, #74242, #26805, #76363, #75845, #844, #1941, #51562, #42953, #59143, #92026, #2476, #33282, #318, #66153 ),
 .UNSPECIFIED., .F., .F.,
 ( 4, 2, 2, 2, 2, 2, 2, 2, 2, 2, 2, 2, 2, 2, 2, 2, 4 ),
 ( 0.4999999999999275579, 0.5312499999999320544, 0.5624999999999366063, 0.5937499999999411582, 0.6249999999999455991, 0.6562499999999501510, 0.6874999999999547029, 0.7187499999999592548, 0.7499999999999638067, 0.7812499999999682476, 0.8124999999999727995, 0.8437499999999773515, 0.8749999999999817923, 0.9062499999999864553, 0.9374999999999908962, 0.9687499999999953371, 1.000000000000000000 ),
 .UNSPECIFIED. ) ;
#73254 = ORIENTED_EDGE ( 'NONE', *, *, #48383, .T. ) ;
#73255 = CARTESIAN_POINT ( 'NONE',  ( 61.11682663846713837, -4.000000000000000888, 4.898587196589422689E-16 ) ) ;
#73256 = CARTESIAN_POINT ( 'NONE',  ( 0.5805565836007616776, 3.752776749732562589, -6.500000000000000888 ) ) ;
#73257 = CARTESIAN_POINT ( 'NONE',  ( 4.852941176470592310, -3.000000000000002665, -70.80672828634229177 ) ) ;
#73258 = CIRCLE ( 'NONE', #6067, 0.9999999999999982236 ) ;
#73259 = CARTESIAN_POINT ( 'NONE',  ( -68.79428259631640685, -60.00000000000000000, -32.96147483378281606 ) ) ;
#73260 = ORIENTED_EDGE ( 'NONE', *, *, #42885, .T. ) ;
#73261 = CARTESIAN_POINT ( 'NONE',  ( 53.28488084350904330, -36.41999201664042118, -27.31396571457552724 ) ) ;
#73262 = AXIS2_PLACEMENT_3D ( 'NONE', #78904, #11501, #76778 ) ;
#73263 = CARTESIAN_POINT ( 'NONE',  ( 32.62207953394533178, 1.482358050883964840E-15, 0.000000000000000000 ) ) ;
#73264 = MECHANICAL_DESIGN_GEOMETRIC_PRESENTATION_REPRESENTATION (  '', ( #97376 ), #100843 ) ;
#73265 = CARTESIAN_POINT ( 'NONE',  ( 95.75131951580081591, -52.82440587276369826, 195.4613675494113068 ) ) ;
#73267 = CARTESIAN_POINT ( 'NONE',  ( -0.009542807171270463462, -57.67120202564520071, -44.61186682692561334 ) ) ;
#73266 = FILL_AREA_STYLE ('',( #40385 ) ) ;
#73268 = EDGE_CURVE ( 'NONE', #78054, #93975, #55565, .T. ) ;
#73269 = CARTESIAN_POINT ( 'NONE',  ( -79.82837926754650937, -56.86146518977977848, 167.4549986377173241 ) ) ;
#73270 = VERTEX_POINT ( 'NONE', #8092 ) ;
#73271 = AXIS2_PLACEMENT_3D ( 'NONE', #11125, #43522, #85589 ) ;
#73272 = ORIENTED_EDGE ( 'NONE', *, *, #58086, .F. ) ;
#73273 = CIRCLE ( 'NONE', #47501, 5.000000000000001776 ) ;
#73274 = EDGE_LOOP ( 'NONE', ( #49232, #41078 ) ) ;
#73275 = CARTESIAN_POINT ( 'NONE',  ( 0.000000000000000000, 0.000000000000000000, -4.814498510800145681 ) ) ;
#73276 = CARTESIAN_POINT ( 'NONE',  ( -4.999999999999960032, -13.06782935463013473, 12.36551185560430710 ) ) ;
#73277 = CARTESIAN_POINT ( 'NONE',  ( -29.68315524077004852, -1.200000000000000030E-05, -40.85535821593474282 ) ) ;
#73278 = ORIENTED_EDGE ( 'NONE', *, *, #44946, .T. ) ;
#73279 = CARTESIAN_POINT ( 'NONE',  ( -4.250000000000000000, 5.204748896376250699E-16, -5.185501489199872083 ) ) ;
#73280 = CARTESIAN_POINT ( 'NONE',  ( -7.499174415388573091E-15, 1.499999999999992450, 61.23540616453487218 ) ) ;
#73281 = CARTESIAN_POINT ( 'NONE',  ( -9.673800154114784888, 15.30085158940939039, -2.563280883359615903 ) ) ;
#73282 = CARTESIAN_POINT ( 'NONE',  ( -93.91996415714238822, -57.61928231945634593, 204.5092364001214946 ) ) ;
#73283 = CARTESIAN_POINT ( 'NONE',  ( 7.188101187500001821, -31.06250000204838813, -2.977408999572650483 ) ) ;
#73284 = CARTESIAN_POINT ( 'NONE',  ( -49.01201108414407059, 47.99999999999999289, 43.00492839360019559 ) ) ;
#73285 = DIRECTION ( 'NONE',  ( 0.5735764363510466035, -0.8191520442889914655, 1.003171929053524500E-16 ) ) ;
#73286 = DIRECTION ( 'NONE',  ( 0.000000000000000000, 0.000000000000000000, 1.000000000000000000 ) ) ;
#73287 = CARTESIAN_POINT ( 'NONE',  ( -72.33650272884364085, -14.21045842199437992, -25.95337777301578797 ) ) ;
#73288 = CARTESIAN_POINT ( 'NONE',  ( 24.83349330513380693, 1.593028355512270962E-15, 0.000000000000000000 ) ) ;
#73289 = CARTESIAN_POINT ( 'NONE',  ( -51.76998541488613625, -42.97695565422467467, 55.08012004277745888 ) ) ;
#73290 = CARTESIAN_POINT ( 'NONE',  ( -18.99999999999999289, -4.000000000000000000, -2.500000000000000000 ) ) ;
#73291 = PRODUCT_DEFINITION ( 'UNKNOWN', '', #100734, #52092 ) ;
#73292 = ORIENTED_EDGE ( 'NONE', *, *, #47294, .T. ) ;
#73293 = CARTESIAN_POINT ( 'NONE',  ( -98.35819475468484541, -37.73781679060022043, 192.3236476725261923 ) ) ;
#73294 = CARTESIAN_POINT ( 'NONE',  ( -0.1688158579390501568, 51.27205306785339900, 10.24139233105815272 ) ) ;
#73295 = VERTEX_POINT ( 'NONE', #24839 ) ;
#73296 = CARTESIAN_POINT ( 'NONE',  ( -17.85751735367976067, 43.17548293752579980, 5.717193597672930672 ) ) ;
#73297 = B_SPLINE_CURVE_WITH_KNOTS ( 'NONE', 3,
 ( #45157, #11155, #3085, #86685, #38147, #36031, #53758, #68905, #95823, #44084, #19852, #101778, #71003, #29527, #27945, #86161, #29017, #37087 ),
 .UNSPECIFIED., .F., .F.,
 ( 4, 2, 2, 2, 2, 2, 2, 2, 4 ),
 ( 8.901954559210201327E-16, 0.0005478302971557816618, 0.001095660594310672977, 0.001643490891465564400, 0.002191321188620456040, 0.002739151485775347464, 0.003286981782930238887, 0.003834812080085130311, 0.004382642377240021300 ),
 .UNSPECIFIED. ) ;
#73298 = CARTESIAN_POINT ( 'NONE',  ( 91.46124806493796200, -38.38747635837011529, -7.532907868879641811 ) ) ;
#73299 = DIRECTION ( 'NONE',  ( -1.000000000000000000, -1.224606353822377258E-16, -0.000000000000000000 ) ) ;
#73300 = CARTESIAN_POINT ( 'NONE',  ( 2.977408999572651815, -10.81250000204838457, 7.188101187500000933 ) ) ;
#73301 = CARTESIAN_POINT ( 'NONE',  ( -9.614507834009854648, 294.6546879296599855, 9.895101348594113944 ) ) ;
#73302 = COLOUR_RGB ( '', 0.40784314, 0.44705882, 0.49803922) ;
#73303 = CYLINDRICAL_SURFACE ( 'NONE', #84405, 14.00000000000000000 ) ;
#73305 = CARTESIAN_POINT ( 'NONE',  ( 84.64623062946745335, -29.99999999999999645, 166.9594626320265718 ) ) ;
#73304 = UNCERTAINTY_MEASURE_WITH_UNIT (LENGTH_MEASURE( 1.000000000000000082E-05 ), #7352, 'distance_accuracy_value', 'NONE');
#73306 = LINE ( 'NONE', #65237, #94082 ) ;
#73307 = CARTESIAN_POINT ( 'NONE',  ( -34.85314843810904506, 481.9552851365352808, 14.52865862526927643 ) ) ;
#73308 = CARTESIAN_POINT ( 'NONE',  ( -6.815830331203682313, 0.6610623347507927905, -6.171384342982605631 ) ) ;
#73309 = EDGE_LOOP ( 'NONE', ( #90217, #2351, #54851, #97265, #19568, #11727 ) ) ;
#73310 = ORIENTED_EDGE ( 'NONE', *, *, #106544, .T. ) ;
#73311 = CARTESIAN_POINT ( 'NONE',  ( 49.48743286625204973, -29.12953531296649246, 46.55428020132097799 ) ) ;
#73312 = CARTESIAN_POINT ( 'NONE',  ( -6.144719067894300224, 301.8764984594092198, -10.02047959687495826 ) ) ;
#73313 = CARTESIAN_POINT ( 'NONE',  ( 9.307407628962446111, 51.55202669552782169, 1.766814834372365306 ) ) ;
#73314 = EDGE_CURVE ( 'NONE', #31200, #66609, #22553, .T. ) ;
#73315 = ORIENTED_EDGE ( 'NONE', *, *, #57313, .T. ) ;
#73316 = CARTESIAN_POINT ( 'NONE',  ( -99.05629584364598372, -38.35566002928235463, 82.90449515628614563 ) ) ;
#73317 = ORIENTED_EDGE ( 'NONE', *, *, #86312, .T. ) ;
#73318 = CARTESIAN_POINT ( 'NONE',  ( 28.04563069813499254, 34.20672709930742883, -9.634527181935203188 ) ) ;
#73319 = CARTESIAN_POINT ( 'NONE',  ( 91.74760752124998930, -38.35367829061644329, 32.25783006298658506 ) ) ;
#73320 = CARTESIAN_POINT ( 'NONE',  ( 11.23686421050524586, 17.72294612705177030, -8.838715948563953262 ) ) ;
#73321 = FACE_OUTER_BOUND ( 'NONE', #28433, .T. ) ;
#73322 = CARTESIAN_POINT ( 'NONE',  ( 105.8789942812274347, -60.15140141051522704, 158.7628738880897004 ) ) ;
#73323 = DIRECTION ( 'NONE',  ( 0.000000000000000000, -1.000000000000000000, 0.000000000000000000 ) ) ;
#73324 = CARTESIAN_POINT ( 'NONE',  ( 22.43989698835544999, 28.20716416251315906, 30.97385700653301299 ) ) ;
#73325 = CARTESIAN_POINT ( 'NONE',  ( -30.98269412877740336, 314.5905989724842584, -6.678017073065344533 ) ) ;
#73326 = CARTESIAN_POINT ( 'NONE',  ( 1.000000000000000000, -69.59657292934913642, 12.76848391599222765 ) ) ;
#73327 = CARTESIAN_POINT ( 'NONE',  ( 76.37025012973165872, -60.00000000000000000, 188.4228991859059477 ) ) ;
#73328 = MECHANICAL_DESIGN_GEOMETRIC_PRESENTATION_REPRESENTATION (  '', ( #4436 ), #78505 ) ;
#73329 = EDGE_CURVE ( 'NONE', #22473, #54377, #14579, .T. ) ;
#73330 = CARTESIAN_POINT ( 'NONE',  ( 17.89029056138539531, 45.00000000000001421, 62.64214772316259427 ) ) ;
#73331 = ORIENTED_EDGE ( 'NONE', *, *, #36551, .T. ) ;
#73332 = CARTESIAN_POINT ( 'NONE',  ( 56.18747785061527367, -29.08556120447800097, 58.61083588748905271 ) ) ;
#73333 = EDGE_CURVE ( 'NONE', #57232, #56205, #41358, .T. ) ;
#73334 = CARTESIAN_POINT ( 'NONE',  ( -25.42905077590008744, 295.6753621798500262, -9.823388355175115549 ) ) ;
#73335 = CYLINDRICAL_SURFACE ( 'NONE', #1430, 5.000000000000002665 ) ;
#73336 = CARTESIAN_POINT ( 'NONE',  ( -9.500000000000000000, -5.000000000000000000, -20.99851272547259384 ) ) ;
#73337 = ORIENTED_EDGE ( 'NONE', *, *, #42951, .T. ) ;
#73339 = CARTESIAN_POINT ( 'NONE',  ( 0.000000000000000000, 0.000000000000000000, 0.000000000000000000 ) ) ;
#73338 = CARTESIAN_POINT ( 'NONE',  ( -78.82921310057996322, -29.99999999998994937, 186.5840926925319536 ) ) ;
#73340 = CARTESIAN_POINT ( 'NONE',  ( 6.990291106834063406, -3.000000000000000444, -4.028951842967194885 ) ) ;
#73341 = CARTESIAN_POINT ( 'NONE',  ( 29.36238239445474107, 323.3665426074553579, 13.50881304725993282 ) ) ;
#73342 = CARTESIAN_POINT ( 'NONE',  ( -1.000000000000000444, -54.00000000000000711, 44.97220075561143204 ) ) ;
#73343 = CARTESIAN_POINT ( 'NONE',  ( -5.656854249492381470, -31.06249999999999645, 5.656854249492379694 ) ) ;
#73344 = DIRECTION ( 'NONE',  ( 0.000000000000000000, 0.000000000000000000, 1.000000000000000000 ) ) ;
#73345 = AXIS2_PLACEMENT_3D ( 'NONE', #46934, #23224, #30251 ) ;
#73346 = EDGE_CURVE ( 'NONE', #15372, #16354, #60421, .T. ) ;
#73347 = CARTESIAN_POINT ( 'NONE',  ( 65.02775738911797987, 48.00000000000000711, -4.794983377755723808 ) ) ;
#73348 = ORIENTED_EDGE ( 'NONE', *, *, #52278, .T. ) ;
#73349 = CARTESIAN_POINT ( 'NONE',  ( 85.29287252500783723, -25.40231041538968526, 170.0305094119342471 ) ) ;
#73350 = CARTESIAN_POINT ( 'NONE',  ( 19.29515645702225868, 5.000000000000002665, 0.000000000000000000 ) ) ;
#73351 = CARTESIAN_POINT ( 'NONE',  ( 25.53945892759312031, 6.123233995736770227E-16, -5.000000000000002665 ) ) ;
#73352 = ORIENTED_EDGE ( 'NONE', *, *, #106466, .T. ) ;
#73353 = FACE_BOUND ( 'NONE', #44570, .T. ) ;
#73354 = CARTESIAN_POINT ( 'NONE',  ( 7.092880029127421437, -4.030086327928861678, -17.38322132479146376 ) ) ;
#73355 = CARTESIAN_POINT ( 'NONE',  ( 26.78474689927651653, 34.86756896202341238, -7.587912695338806301 ) ) ;
#73356 = DIRECTION ( 'NONE',  ( -1.000000000000000000, -0.000000000000000000, -0.000000000000000000 ) ) ;
#73357 = DIRECTION ( 'NONE',  ( -0.000000000000000000, 1.000000000000000000, -0.000000000000000000 ) ) ;
#73358 = AXIS2_PLACEMENT_3D ( 'NONE', #81342, #95967, #97014 ) ;
#73359 = DIRECTION ( 'NONE',  ( 0.000000000000000000, -1.000000000000000000, 0.000000000000000000 ) ) ;
#73360 =( NAMED_UNIT ( * ) SI_UNIT ( $, .STERADIAN. ) SOLID_ANGLE_UNIT ( ) );
#73361 = CIRCLE ( 'NONE', #47505, 4.172000000000009479 ) ;
#73362 = CARTESIAN_POINT ( 'NONE',  ( 6.499999999999999112, 2.723353699433560315, -5.896365680526115760 ) ) ;
#73363 = CARTESIAN_POINT ( 'NONE',  ( 0.7841136692415845433, 25.26116217180792489, 40.48719991889687719 ) ) ;
#73365 = CARTESIAN_POINT ( 'NONE',  ( -11.76332149636490598, 11.37125156745868004, -9.882589870049462988 ) ) ;
#73364 = CARTESIAN_POINT ( 'NONE',  ( -26.01198988472668105, -29.73227193545200109, 38.65812357631961049 ) ) ;
#73366 = EDGE_CURVE ( 'NONE', #37125, #18823, #80717, .T. ) ;
#73367 = CARTESIAN_POINT ( 'NONE',  ( 7.188101187500000044, -14.65625000204838457, 0.000000000000000000 ) ) ;
#73368 = CARTESIAN_POINT ( 'NONE',  ( -60.62677696757947388, 40.83906611472935566, 24.18439664997239191 ) ) ;
#73369 = LINE ( 'NONE', #22221, #34580 ) ;
#73370 = ORIENTED_EDGE ( 'NONE', *, *, #33450, .F. ) ;
#73371 = CARTESIAN_POINT ( 'NONE',  ( -17.49999999999997868, 49.46308821774191955, 63.99046601235075826 ) ) ;
#73372 = DIRECTION ( 'NONE',  ( -1.000000000000000000, 0.000000000000000000, 0.000000000000000000 ) ) ;
#73373 = AXIS2_PLACEMENT_3D ( 'NONE', #22803, #23325, #30900 ) ;
#73374 = CARTESIAN_POINT ( 'NONE',  ( -7.860352320337314680, 85.38611325940999563, -4.999999999992382982 ) ) ;
#73375 = EDGE_CURVE ( 'NONE', #65067, #55144, #39776, .T. ) ;
#73376 = CARTESIAN_POINT ( 'NONE',  ( 44.78945892759311675, 5.000000000000015099, 6.123233995736782060E-16 ) ) ;
#73377 = EDGE_CURVE ( 'NONE', #59035, #68982, #27274, .T. ) ;
#73378 = DIRECTION ( 'NONE',  ( 0.000000000000000000, -1.000000000000000000, 0.000000000000000000 ) ) ;
#73379 = VERTEX_POINT ( 'NONE', #42586 ) ;
#73380 = CARTESIAN_POINT ( 'NONE',  ( -5.093082057083965886, -87.44446206421569912, -3.176439207277721000 ) ) ;
#73381 =( NAMED_UNIT ( * ) PLANE_ANGLE_UNIT ( ) SI_UNIT ( $, .RADIAN. ) );
#73382 = VERTEX_POINT ( 'NONE', #60399 ) ;
#73383 =( LENGTH_UNIT ( ) NAMED_UNIT ( * ) SI_UNIT ( .MILLI., .METRE. ) );
#73384 = FACE_OUTER_BOUND ( 'NONE', #90481, .T. ) ;
#73385 = CARTESIAN_POINT ( 'NONE',  ( -33.29153341846981817, 40.67237416681741990, -61.88034040721849749 ) ) ;
#73386 = CARTESIAN_POINT ( 'NONE',  ( -109.0325503311019446, -60.00000000000000000, 136.2077695858294817 ) ) ;
#73387 = DIRECTION ( 'NONE',  ( 0.000000000000000000, 0.000000000000000000, 1.000000000000000000 ) ) ;
#73388 = CARTESIAN_POINT ( 'NONE',  ( 0.000000000000000000, 304.8518027762758038, -10.00000000000000355 ) ) ;
#73389 = CARTESIAN_POINT ( 'NONE',  ( 23.09999999999999432, 1.533819458162526451E-15, 0.000000000000000000 ) ) ;
#73390 = CARTESIAN_POINT ( 'NONE',  ( 0.000000000000000000, 0.000000000000000000, -5.703399999999999359 ) ) ;
#73392 = CARTESIAN_POINT ( 'NONE',  ( -15.12883458092753841, 3.606451457941037830, -4.265946247306469097 ) ) ;
#73391 = CARTESIAN_POINT ( 'NONE',  ( 6.145467200816499442, -5.000000000008177459, -92.99666842292330671 ) ) ;
#73393 = EDGE_CURVE ( 'NONE', #24576, #79056, #82797, .T. ) ;
#73394 = CARTESIAN_POINT ( 'NONE',  ( -86.20327847884676942, -18.29549290550911778, 168.7810058706911889 ) ) ;
#73395 = STYLED_ITEM ( 'NONE', ( #41916 ), #65971 ) ;
#73396 = ORIENTED_EDGE ( 'NONE', *, *, #32651, .F. ) ;
#73397 = CARTESIAN_POINT ( 'NONE',  ( 4.852941176470593199, 44.25000000000000000, -70.80672828634229177 ) ) ;
#73398 = ORIENTED_EDGE ( 'NONE', *, *, #53562, .T. ) ;
#73399 = ORIENTED_EDGE ( 'NONE', *, *, #19889, .T. ) ;
#73400 = FACE_OUTER_BOUND ( 'NONE', #89762, .T. ) ;
#73401 = EDGE_CURVE ( 'NONE', #48389, #27209, #58707, .T. ) ;
#73403 = FACE_OUTER_BOUND ( 'NONE', #29199, .T. ) ;
#73402 = VECTOR ( 'NONE', #31753, 1000.000000000000000 ) ;
#73404 = DIRECTION ( 'NONE',  ( -1.000000000000000000, -1.224606353822377258E-16, -0.000000000000000000 ) ) ;
#73405 = FACE_OUTER_BOUND ( 'NONE', #85995, .T. ) ;
#73406 = CIRCLE ( 'NONE', #59670, 4.000000000000000888 ) ;
#73407 = CARTESIAN_POINT ( 'NONE',  ( 30.00000000000000000, 462.0143252985375852, 13.78012569455009029 ) ) ;
#73408 = FACE_OUTER_BOUND ( 'NONE', #40142, .T. ) ;
#73409 = DIRECTION ( 'NONE',  ( 0.000000000000000000, 1.000000000000000000, 0.000000000000000000 ) ) ;
#73410 = CARTESIAN_POINT ( 'NONE',  ( 114.3489886862215883, -60.00000000000002842, 164.2602920347584359 ) ) ;
#73411 = CARTESIAN_POINT ( 'NONE',  ( -106.7878682580589071, -14.21045842199432663, 165.8353880188381027 ) ) ;
#73412 = CARTESIAN_POINT ( 'NONE',  ( -64.43939551583753200, -22.10274715365727261, 75.67409506763341653 ) ) ;
#73413 = ORIENTED_EDGE ( 'NONE', *, *, #53165, .T. ) ;
#73414 = AXIS2_PLACEMENT_3D ( 'NONE', #29343, #39533, #72410 ) ;
#73415 = CARTESIAN_POINT ( 'NONE',  ( 14.51107877698349569, 38.95396704606918803, 62.06021138805395765 ) ) ;
#73416 = CARTESIAN_POINT ( 'NONE',  ( 112.9852162270515379, -60.00000000000000000, 189.2447496387153478 ) ) ;
#73417 =( GEOMETRIC_REPRESENTATION_CONTEXT ( 3 ) GLOBAL_UNCERTAINTY_ASSIGNED_CONTEXT ( ( #63408 ) ) GLOBAL_UNIT_ASSIGNED_CONTEXT ( ( #32657, #80630, #33180 ) ) REPRESENTATION_CONTEXT ( 'NONE', 'WORKASPACE' ) );
#73419 = EDGE_LOOP ( 'NONE', ( #64819, #39785, #48994, #55804, #13932, #23369, #52073 ) ) ;
#73418 = AXIS2_PLACEMENT_3D ( 'NONE', #32827, #9043, #9571 ) ;
#73420 = CARTESIAN_POINT ( 'NONE',  ( 2.066515801291814188E-05, -35.99156565065722191, 29.88824423471190883 ) ) ;
#73422 = PRESENTATION_LAYER_ASSIGNMENT (  '', '', ( #104463 ) ) ;
#73421 = CARTESIAN_POINT ( 'NONE',  ( -7.188101187500000044, -11.28125000204838457, -8.802885111219163269E-16 ) ) ;
#73423 = SURFACE_STYLE_FILL_AREA ( #9225 ) ;
#73424 = ORIENTED_EDGE ( 'NONE', *, *, #7874, .T. ) ;
#73425 = DIRECTION ( 'NONE',  ( 1.000000000000000000, 0.000000000000000000, 0.000000000000000000 ) ) ;
#73426 = ORIENTED_EDGE ( 'NONE', *, *, #21549, .F. ) ;
#73427 = CARTESIAN_POINT ( 'NONE',  ( -3.809068165403739048, -5.306386968807679239, -1.794524002052960067E-14 ) ) ;
#73428 = EDGE_CURVE ( 'NONE', #63624, #96955, #96593, .T. ) ;
#73429 = CARTESIAN_POINT ( 'NONE',  ( 37.33349330513379982, 1.593028355512270962E-15, 0.000000000000000000 ) ) ;
#73431 = CIRCLE ( 'NONE', #97523, 5.000000000000010658 ) ;
#73430 = CARTESIAN_POINT ( 'NONE',  ( -107.3076241182627228, -59.99999999999998579, 196.6869121037917978 ) ) ;
#73432 = CARTESIAN_POINT ( 'NONE',  ( -3.438773559902674304, -0.8293899918508151892, 103.7823003339716053 ) ) ;
#73433 = CARTESIAN_POINT ( 'NONE',  ( 7.188101187500001821, -28.43750000204839168, -2.977408999572650483 ) ) ;
#73434 = CARTESIAN_POINT ( 'NONE',  ( 1.224646799147353454E-15, -4.000000000000003553, 17.00000000000000000 ) ) ;
#73435 = STYLED_ITEM ( 'NONE', ( #25020 ), #15243 ) ;
#73436 = DIRECTION ( 'NONE',  ( -0.000000000000000000, -1.000000000000000000, -0.000000000000000000 ) ) ;
#73437 = DIRECTION ( 'NONE',  ( 0.000000000000000000, -1.000000000000000000, 0.000000000000000000 ) ) ;
#73438 = FACE_OUTER_BOUND ( 'NONE', #68204, .T. ) ;
#73439 = CARTESIAN_POINT ( 'NONE',  ( 12.00269904674914656, -6.870077166404533031, 19.79010987306656588 ) ) ;
#73440 = SURFACE_STYLE_FILL_AREA ( #1678 ) ;
#73441 = CARTESIAN_POINT ( 'NONE',  ( 106.4540643960806818, -59.99999999999999289, 175.2089101670526645 ) ) ;
#73442 = CARTESIAN_POINT ( 'NONE',  ( -32.69629451572926371, -25.62164330307078686, 31.60428463432279145 ) ) ;
#73443 = CARTESIAN_POINT ( 'NONE',  ( -1.276674890335059320, -50.00000000000000000, 101.3108517956396639 ) ) ;
#73444 = CARTESIAN_POINT ( 'NONE',  ( 41.83556152829600450, -56.79490171586785863, 44.35057537570739328 ) ) ;
#73445 = CYLINDRICAL_SURFACE ( 'NONE', #19749, 5.000000000000000888 ) ;
#73446 = ORIENTED_EDGE ( 'NONE', *, *, #104818, .T. ) ;
#73447 = CARTESIAN_POINT ( 'NONE',  ( 44.32955949053914679, 435.2565657989975421, 11.97827722465379097 ) ) ;
#73448 = CARTESIAN_POINT ( 'NONE',  ( -84.03771973047440724, -38.76031024263880909, 197.8063387002864886 ) ) ;
#73449 = VERTEX_POINT ( 'NONE', #51198 ) ;
#73451 = CARTESIAN_POINT ( 'NONE',  ( -30.87955015324946828, 351.7733141111877444, 20.67482462247657082 ) ) ;
#73450 = CARTESIAN_POINT ( 'NONE',  ( 2.499999999999999556, -11.82938852550672593, 20.68569722764979701 ) ) ;
#73452 = CARTESIAN_POINT ( 'NONE',  ( -11.08827160299917480, 19.49528337425789104, -8.747723196539737955 ) ) ;
#73453 = CARTESIAN_POINT ( 'NONE',  ( -32.88333705524295425, 439.7317646416726689, 24.13381181826147781 ) ) ;
#73454 = CARTESIAN_POINT ( 'NONE',  ( 6.449804269883611774, -2.701269212710093459, 6.840189325177291835 ) ) ;
#73455 = CARTESIAN_POINT ( 'NONE',  ( 0.000000000000000000, -15.00000000000000000, -9.000000000000000000 ) ) ;
#73456 = LINE ( 'NONE', #8734, #77319 ) ;
#73457 = CARTESIAN_POINT ( 'NONE',  ( -30.50035377180213558, 337.4047871495883442, 16.76239630436412043 ) ) ;
#73458 = FACE_OUTER_BOUND ( 'NONE', #7819, .T. ) ;
#73459 = AXIS2_PLACEMENT_3D ( 'NONE', #21438, #86701, #102864 ) ;
#73460 = CARTESIAN_POINT ( 'NONE',  ( 97.79592197825088817, -59.99999999999998579, 67.65900241341216770 ) ) ;
#73461 = CARTESIAN_POINT ( 'NONE',  ( -3.258466594083123002, -53.34205889910419529, 40.61703279866434002 ) ) ;
#73462 =( GEOMETRIC_REPRESENTATION_CONTEXT ( 3 ) GLOBAL_UNCERTAINTY_ASSIGNED_CONTEXT ( ( #70400 ) ) GLOBAL_UNIT_ASSIGNED_CONTEXT ( ( #16557, #852, #65641 ) ) REPRESENTATION_CONTEXT ( 'NONE', 'WORKASPACE' ) );
#73463 = CARTESIAN_POINT ( 'NONE',  ( -38.89974112662849137, 460.7404230935934493, 2.234279992752822963 ) ) ;
#73464 = ORIENTED_EDGE ( 'NONE', *, *, #43829, .F. ) ;
#73465 = EDGE_CURVE ( 'NONE', #76534, #28165, #26036, .T. ) ;
#73466 = CARTESIAN_POINT ( 'NONE',  ( -95.68750834249433979, -29.99999999999991473, 191.3192462275344781 ) ) ;
#73467 = EDGE_LOOP ( 'NONE', ( #24685, #85364, #106088, #64929 ) ) ;
#73468 = CARTESIAN_POINT ( 'NONE',  ( -9.960763185286923616, -57.87158879323015270, 26.07764662560745705 ) ) ;
#73469 = CARTESIAN_POINT ( 'NONE',  ( -16.02187926457684597, 4.033883445135416856, 2.088897399371232311 ) ) ;
#73470 = CARTESIAN_POINT ( 'NONE',  ( 32.10815921214906865, 435.9979227416979484, 24.01722067222687684 ) ) ;
#73471 = CARTESIAN_POINT ( 'NONE',  ( -22.89193641261722689, 27.46073252125954411, -33.16577871831040625 ) ) ;
#73472 = CARTESIAN_POINT ( 'NONE',  ( 7.188101187499999156, -24.12500000204838457, 2.977408999572654924 ) ) ;
#73474 = EDGE_CURVE ( 'NONE', #74667, #77225, #48369, .T. ) ;
#73473 = CARTESIAN_POINT ( 'NONE',  ( -3.454253436624930451, -0.8414180287960395521, 103.7259032015043232 ) ) ;
#73475 = CARTESIAN_POINT ( 'NONE',  ( 6.733158597025957093, 41.46658730117229652, -70.54360491111089004 ) ) ;
#73476 = ORIENTED_EDGE ( 'NONE', *, *, #11221, .T. ) ;
#73478 = ORIENTED_EDGE ( 'NONE', *, *, #1825, .T. ) ;
#73477 = CARTESIAN_POINT ( 'NONE',  ( 2.000000000000000888, 4.000000000000000000, 0.000000000000000000 ) ) ;
#73479 = CARTESIAN_POINT ( 'NONE',  ( 82.15109098281409672, -25.62403950325144208, 144.0112107024839077 ) ) ;
#73480 = CARTESIAN_POINT ( 'NONE',  ( -16.66584972143294863, 38.95383793067399125, 62.01418705518651819 ) ) ;
#73481 = AXIS2_PLACEMENT_3D ( 'NONE', #28853, #96200, #20233 ) ;
#73482 = CARTESIAN_POINT ( 'NONE',  ( -37.88389991164935111, 27.77159677234703494, -10.98672745669020401 ) ) ;
#73483 = ORIENTED_EDGE ( 'NONE', *, *, #36108, .F. ) ;
#73484 = CARTESIAN_POINT ( 'NONE',  ( -56.71108403266729425, 50.00000000000000711, 27.46636503440964105 ) ) ;
#73485 = CARTESIAN_POINT ( 'NONE',  ( 6.944371705245973025, -85.53899691424548735, -3.972324460300566962 ) ) ;
#73486 = CARTESIAN_POINT ( 'NONE',  ( -7.188101187500002709, -15.31250000204838813, 2.977408999572647819 ) ) ;
#73487 = CARTESIAN_POINT ( 'NONE',  ( 7.618844049274132502, 26.82764101070540264, 2.450177051822847840 ) ) ;
#73488 = CARTESIAN_POINT ( 'NONE',  ( 21.19369299071200174, -60.00000000000002132, -35.98201359092684015 ) ) ;
#73489 =( BOUNDED_CURVE ( )  B_SPLINE_CURVE ( 2, ( #58247, #499, #84126, #41534, #24847 ),
 .UNSPECIFIED., .F., .F. ) 
 B_SPLINE_CURVE_WITH_KNOTS ( ( 3, 2, 3 ),
 ( 0.000000000000000000, 0.9999561054434824570, 1.000000000000000000 ),
 .UNSPECIFIED. ) 
 CURVE ( )  GEOMETRIC_REPRESENTATION_ITEM ( )  RATIONAL_B_SPLINE_CURVE ( ( 1.000000000000000000, 1.857142857142858317, 1.000000000000000000, 1.000000000000000000, 1.000000000000000000 ) ) 
 REPRESENTATION_ITEM ( '' )  );
#73490 = CARTESIAN_POINT ( 'NONE',  ( -14.02841258157142690, -57.67128452586098319, 41.71853563109401364 ) ) ;
#73491 = EDGE_CURVE ( 'NONE', #71083, #35336, #19436, .T. ) ;
#73492 = ORIENTED_EDGE ( 'NONE', *, *, #476, .T. ) ;
#73493 = VECTOR ( 'NONE', #2156, 1000.000000000000000 ) ;
#73494 = DIRECTION ( 'NONE',  ( -3.469446951953614189E-16, 1.000000000000000000, -0.000000000000000000 ) ) ;
#73495 = CARTESIAN_POINT ( 'NONE',  ( 29.83349330513380337, 4.000000000000003553, 0.000000000000000000 ) ) ;
#73496 = CARTESIAN_POINT ( 'NONE',  ( -4.999999999999998224, 5.773502691896257311, -7.063244554130002406 ) ) ;
#73497 = EDGE_CURVE ( 'NONE', #9794, #25439, #10738, .T. ) ;
#73498 = ORIENTED_EDGE ( 'NONE', *, *, #81848, .T. ) ;
#73499 = CARTESIAN_POINT ( 'NONE',  ( -7.188101187500000044, -28.90625000204838813, -8.802885111219163269E-16 ) ) ;
#73500 = CARTESIAN_POINT ( 'NONE',  ( 26.50624775675402134, -30.07146743491984253, 38.85830190916826155 ) ) ;
#73501 = VECTOR ( 'NONE', #101790, 999.9999999999998863 ) ;
#73502 = CARTESIAN_POINT ( 'NONE',  ( -39.83282735953067544, 489.3954873304602415, 11.44298468960946025 ) ) ;
#73503 = DIRECTION ( 'NONE',  ( 1.000000000000000000, 0.000000000000000000, -0.000000000000000000 ) ) ;
#73504 = ADVANCED_FACE ( 'NONE', ( #44198 ), #103506, .T. ) ;
#73505 = CARTESIAN_POINT ( 'NONE',  ( 32.99999999999999289, 439.7597899781498541, 24.16317522621305613 ) ) ;
#73506 = SHAPE_DEFINITION_REPRESENTATION ( #68139, #38413 ) ;
#73507 = CARTESIAN_POINT ( 'NONE',  ( 48.15203510316958813, 9.493368196138895598, 16.85535821593427386 ) ) ;
#73508 = ORIENTED_EDGE ( 'NONE', *, *, #49072, .T. ) ;
#73509 = FACE_OUTER_BOUND ( 'NONE', #72961, .T. ) ;
#73510 = CARTESIAN_POINT ( 'NONE',  ( 13.44497361249347556, 42.85008855513920878, -92.01621721121948383 ) ) ;
#73511 = CARTESIAN_POINT ( 'NONE',  ( 8.560863513991206375, -22.26022726792948347, -38.54397950491892288 ) ) ;
#73512 = DIRECTION ( 'NONE',  ( 0.000000000000000000, -1.000000000000000000, 0.000000000000000000 ) ) ;
#73513 = EDGE_CURVE ( 'NONE', #49616, #71082, #91437, .T. ) ;
#73514 = DIRECTION ( 'NONE',  ( -1.000000000000000000, -0.000000000000000000, -0.000000000000000000 ) ) ;
#73515 = ORIENTED_EDGE ( 'NONE', *, *, #89345, .T. ) ;
#73516 = CARTESIAN_POINT ( 'NONE',  ( -26.47069814182328784, 36.83824913210050767, -9.930511453896439633 ) ) ;
#73517 = CARTESIAN_POINT ( 'NONE',  ( 111.7166322225655932, -57.67144568547145411, 141.1164683676901461 ) ) ;
#73518 = CARTESIAN_POINT ( 'NONE',  ( 37.22405814379364841, 463.3230035706885701, 20.09439497145411124 ) ) ;
#73519 = CARTESIAN_POINT ( 'NONE',  ( -9.306959991822290945, 51.55220751856156625, -1.766502984829542600 ) ) ;
#73520 = CARTESIAN_POINT ( 'NONE',  ( 73.50474219086036953, -59.99999999999997158, -24.84696050693406022 ) ) ;
#73521 = DIRECTION ( 'NONE',  ( 0.000000000000000000, 0.000000000000000000, -1.000000000000000000 ) ) ;
#73522 = CARTESIAN_POINT ( 'NONE',  ( -73.36883549988228026, -59.99999999999997868, 165.9088962234452254 ) ) ;
#73523 = CARTESIAN_POINT ( 'NONE',  ( -35.76379064120181539, 307.0162303970107587, 12.81051142610679960 ) ) ;
#73524 = EDGE_CURVE ( 'NONE', #32665, #85099, #87846, .T. ) ;
#73525 = CARTESIAN_POINT ( 'NONE',  ( -27.18908553330205180, 296.5274986157688772, 10.30015177545897842 ) ) ;
#73526 = AXIS2_PLACEMENT_3D ( 'NONE', #5133, #23462, #21875 ) ;
#73527 = CARTESIAN_POINT ( 'NONE',  ( -86.05794333201590973, -24.85278311144536190, 179.6146324082043861 ) ) ;
#73528 = VERTEX_POINT ( 'NONE', #71117 ) ;
#73529 = CARTESIAN_POINT ( 'NONE',  ( 30.20825430514037535, 310.0052099631511737, -8.578664711180536528 ) ) ;
#73530 = AXIS2_PLACEMENT_3D ( 'NONE', #30123, #39276, #46292 ) ;
#73531 = ORIENTED_EDGE ( 'NONE', *, *, #56973, .F. ) ;
#73532 = CARTESIAN_POINT ( 'NONE',  ( 37.56673239365841255, 27.88554838446202311, -10.95617127781092037 ) ) ;
#73533 = EDGE_CURVE ( 'NONE', #57508, #91175, #29556, .T. ) ;
#73534 = CARTESIAN_POINT ( 'NONE',  ( -4.919733272805030921, -1.562181361514374478, 104.2477112191710944 ) ) ;
#73535 = CARTESIAN_POINT ( 'NONE',  ( -84.43672636148829724, -45.26723741285099578, -8.687404643540368454 ) ) ;
#73536 = CARTESIAN_POINT ( 'NONE',  ( 21.08349330513380693, 1.593028355512270962E-15, 0.000000000000000000 ) ) ;
#73537 = CARTESIAN_POINT ( 'NONE',  ( 42.69811214730273718, 434.9611672192513652, 18.34625614733210242 ) ) ;
#73538 = VERTEX_POINT ( 'NONE', #3745 ) ;
#73539 = CARTESIAN_POINT ( 'NONE',  ( -33.49978038584191609, 465.4670364589441647, 16.54746596769432543 ) ) ;
#73540 = CARTESIAN_POINT ( 'NONE',  ( 10.29549899077097486, 16.65270026559913319, -9.997496007081116076 ) ) ;
#73541 = EDGE_CURVE ( 'NONE', #18205, #91522, #38176, .T. ) ;
#73542 = CARTESIAN_POINT ( 'NONE',  ( -10.45706415777859455, -1.734723475976807094E-15, 13.60704923275178935 ) ) ;
#73543 = CARTESIAN_POINT ( 'NONE',  ( -35.65219468668893654, 436.9652430364855036, 4.678245027582931925 ) ) ;
#73544 = CARTESIAN_POINT ( 'NONE',  ( 2.726837646490497757, -14.21045842199434794, -37.36840973699905533 ) ) ;
#73545 = CARTESIAN_POINT ( 'NONE',  ( -77.58900850978491803, -32.55426609391764714, 126.5529035919531538 ) ) ;
#73546 = ORIENTED_EDGE ( 'NONE', *, *, #6680, .F. ) ;
#73547 = CARTESIAN_POINT ( 'NONE',  ( 32.49824730387988581, -59.99999999999999289, 47.28149596916139075 ) ) ;
#73548 = CARTESIAN_POINT ( 'NONE',  ( 7.213352437320216914, 87.01836473007681150, -3.463014597543481621 ) ) ;
#73549 = CARTESIAN_POINT ( 'NONE',  ( 109.2379923685197127, -57.67120357111281947, 124.0924491272076011 ) ) ;
#73550 = ORIENTED_EDGE ( 'NONE', *, *, #104411, .F. ) ;
#73551 = CARTESIAN_POINT ( 'NONE',  ( 27.10511071441204578, 34.75829513984540142, 7.556984339685363317 ) ) ;
#73552 = AXIS2_PLACEMENT_3D ( 'NONE', #14471, #61619, #44897 ) ;
#73553 = CARTESIAN_POINT ( 'NONE',  ( 45.11650669486618881, 1.474610560812782335E-15, 0.000000000000000000 ) ) ;
#73554 = ORIENTED_EDGE ( 'NONE', *, *, #55616, .T. ) ;
#73555 = VECTOR ( 'NONE', #81839, 1000.000000000000000 ) ;
#73556 = DIRECTION ( 'NONE',  ( -1.000000000000000000, -1.224606353822377258E-16, -0.000000000000000000 ) ) ;
#73557 = EDGE_CURVE ( 'NONE', #68982, #13191, #104005, .T. ) ;
#73558 = CARTESIAN_POINT ( 'NONE',  ( -12.50000000000000711, 18.64303733123573537, -36.27143273323382999 ) ) ;
#73559 = DIRECTION ( 'NONE',  ( -1.000000000000000000, 0.000000000000000000, 0.000000000000000000 ) ) ;
#73560 = CARTESIAN_POINT ( 'NONE',  ( 2.977408999572650927, -17.37500000204838457, -7.188101187500001821 ) ) ;
#73561 = FACE_OUTER_BOUND ( 'NONE', #44743, .T. ) ;
#73562 = CARTESIAN_POINT ( 'NONE',  ( 9.645512969475857901, 81.98896849324276559, -2.645801731561386205 ) ) ;
#73563 = LINE ( 'NONE', #16952, #43386 ) ;
#73564 = DIRECTION ( 'NONE',  ( 0.000000000000000000, 0.000000000000000000, -1.000000000000000000 ) ) ;
#73565 = DIRECTION ( 'NONE',  ( -1.000000000000000000, -1.224606353822377258E-16, -0.000000000000000000 ) ) ;
#73566 = ORIENTED_EDGE ( 'NONE', *, *, #45819, .F. ) ;
#73567 = CARTESIAN_POINT ( 'NONE',  ( -7.442703362271647194, 40.98154495329247737, -69.28862671947442209 ) ) ;
#73568 = CIRCLE ( 'NONE', #20383, 4.000000000000007105 ) ;
#73570 = CARTESIAN_POINT ( 'NONE',  ( 30.23427007269342681, -36.01284674722493406, 32.58737572666365878 ) ) ;
#73569 = CARTESIAN_POINT ( 'NONE',  ( -0.2923334656586880076, -70.53271932724192084, 13.00000000000000000 ) ) ;
#73571 = CARTESIAN_POINT ( 'NONE',  ( 26.86604693904285668, 307.4841669554380701, -8.413536135732222476 ) ) ;
#73572 = ORIENTED_EDGE ( 'NONE', *, *, #17507, .F. ) ;
#73573 = ORIENTED_EDGE ( 'NONE', *, *, #38615, .F. ) ;
#73574 = AXIS2_PLACEMENT_3D ( 'NONE', #45387, #36791, #78268 ) ;
#73576 = CARTESIAN_POINT ( 'NONE',  ( 11.84999999999999787, 1.533819458162526451E-15, 0.000000000000000000 ) ) ;
#73575 = DIRECTION ( 'NONE',  ( -1.000000000000000000, -1.224606353822377258E-16, -0.000000000000000000 ) ) ;
#73577 = VECTOR ( 'NONE', #70368, 1000.000000000000000 ) ;
#73578 = FACE_OUTER_BOUND ( 'NONE', #39023, .T. ) ;
#73579 = DIRECTION ( 'NONE',  ( -1.000000000000000000, -0.000000000000000000, -0.000000000000000000 ) ) ;
#73580 = AXIS2_PLACEMENT_3D ( 'NONE', #48063, #21324, #54160 ) ;
#73581 = DIRECTION ( 'NONE',  ( -0.000000000000000000, -1.000000000000000000, -0.000000000000000000 ) ) ;
#73582 = CARTESIAN_POINT ( 'NONE',  ( 1.218732506510818103, 45.85998149243336286, 17.17911318258725117 ) ) ;
#73583 = CARTESIAN_POINT ( 'NONE',  ( -36.27064846733345860, 463.5381974806653602, 19.67843218035488562 ) ) ;
#73584 = ORIENTED_EDGE ( 'NONE', *, *, #28804, .F. ) ;
#73585 = CARTESIAN_POINT ( 'NONE',  ( 9.708955930194042239, -60.00000000000000711, -42.43033358671466004 ) ) ;
#73586 = CARTESIAN_POINT ( 'NONE',  ( -11.07233799575505628, 45.30046846812411587, -15.14426123305350558 ) ) ;
#73587 = PRESENTATION_LAYER_ASSIGNMENT (  '', '', ( #13301 ) ) ;
#73588 = CARTESIAN_POINT ( 'NONE',  ( 6.683837171061803417, -3.955946848495962787, 6.851900933636989599 ) ) ;
#73589 = CIRCLE ( 'NONE', #46059, 5.000000000000001776 ) ;
#73590 = FACE_OUTER_BOUND ( 'NONE', #564, .T. ) ;
#73591 = ORIENTED_EDGE ( 'NONE', *, *, #13029, .T. ) ;
#73592 = ADVANCED_FACE ( 'NONE', ( #94350 ), #17446, .F. ) ;
#73593 = CARTESIAN_POINT ( 'NONE',  ( -3.400000000000000355, 4.163799117101001052E-16, -8.000000000000000000 ) ) ;
#73594 = ORIENTED_EDGE ( 'NONE', *, *, #102333, .F. ) ;
#73595 = ORIENTED_EDGE ( 'NONE', *, *, #103079, .F. ) ;
#73596 = DIRECTION ( 'NONE',  ( 0.000000000000000000, 0.6935263888316357539, -0.7204312236391137159 ) ) ;
#73597 = CARTESIAN_POINT ( 'NONE',  ( -43.74985542820371620, 435.5770091380364306, 16.96136490515579354 ) ) ;
#73598 = CARTESIAN_POINT ( 'NONE',  ( -40.91188376428177520, 436.7570986683169281, 21.64372942866937422 ) ) ;
#73599 = CARTESIAN_POINT ( 'NONE',  ( 32.54109659871799920, 344.3893346267446987, 19.67009027976686042 ) ) ;
#73600 = CARTESIAN_POINT ( 'NONE',  ( -36.78952342955899724, 340.7883647611195670, -0.8934509747473148300 ) ) ;
#73601 = CARTESIAN_POINT ( 'NONE',  ( -4.259638269668483801, -69.00982656590272768, 13.66265674538449204 ) ) ;
#73602 = CARTESIAN_POINT ( 'NONE',  ( -43.89153851290792829, 485.1215805105567824, -0.3742518171758901224 ) ) ;
#73604 = EDGE_CURVE ( 'NONE', #53057, #72256, #89817, .T. ) ;
#73603 = CARTESIAN_POINT ( 'NONE',  ( 12.50000000000000533, 41.05801042994118433, -71.24449801089164680 ) ) ;
#73605 = ORIENTED_EDGE ( 'NONE', *, *, #78564, .F. ) ;
#73606 = CARTESIAN_POINT ( 'NONE',  ( 30.48935137155323716, 7.748232456196025630, 41.81352479775706854 ) ) ;
#73607 = VERTEX_POINT ( 'NONE', #46839 ) ;
#73608 = AXIS2_PLACEMENT_3D ( 'NONE', #96181, #103205, #28286 ) ;
#73609 = CARTESIAN_POINT ( 'NONE',  ( 9.734943007948952953, 51.35523771563250506, -2.348059683008551612 ) ) ;
#73610 = DIRECTION ( 'NONE',  ( 1.000000000000000000, 0.000000000000000000, 0.000000000000000000 ) ) ;
#73611 = B_SPLINE_CURVE_WITH_KNOTS ( 'NONE', 3,
 ( #73896, #56097, #65283, #49079 ),
 .UNSPECIFIED., .F., .F.,
 ( 4, 4 ),
 ( 0.000000000000000000, 1.000000000000000000 ),
 .UNSPECIFIED. ) ;
#73612 = CARTESIAN_POINT ( 'NONE',  ( -42.44423885992037526, -60.00000000000002842, 45.81425615931330952 ) ) ;
#73613 = CARTESIAN_POINT ( 'NONE',  ( 66.61458672392836888, -49.90900424519782064, 96.76507275318283519 ) ) ;
#73614 = B_SPLINE_CURVE_WITH_KNOTS ( 'NONE', 3,
 ( #73336, #73879, #106774, #33999, #98157, #81959, #32924, #66326, #57684, #42048, #16178, #8615, #91678, #82512, #24311, #90607, #9664, #65799, #99209, #98676, #50643, #49605, #74932, #72808, #58782, #64738, #41517, #17794, #74403, #105715, #49064, #97614, #16716, #25373, #7539, #56627, #58229, #48535, #81426, #40456 ),
 .UNSPECIFIED., .F., .F.,
 ( 4, 1, 1, 1, 1, 1, 1, 2, 2, 1, 1, 1, 1, 1, 2, 2, 1, 1, 1, 1, 1, 1, 2, 2, 1, 1, 1, 2, 2, 4 ),
 ( 0.000000000000000000, 0.1250000000000340283, 0.1875000000000504874, 0.2187500000000587308, 0.2343750000000622558, 0.2421875000000639766, 0.2460937500000649203, 0.2480468750000653366, 0.2500000000000657252, 0.3750000000000667799, 0.4375000000000666689, 0.4687500000000665024, 0.4843750000000663913, 0.4921875000000663913, 0.4960937500000657252, 0.5000000000000650591, 0.6250000000000497380, 0.6875000000000424105, 0.7187500000000386358, 0.7343750000000368594, 0.7421875000000359712, 0.7460937500000354161, 0.7480468750000351941, 0.7500000000000349720, 0.8125000000000258682, 0.8437500000000213163, 0.8593750000000189848, 0.8671875000000177636, 0.8750000000000165423, 1.000000000000000000 ),
 .UNSPECIFIED. ) ;
#73615 = VERTEX_POINT ( 'NONE', #60920 ) ;
#73616 = CARTESIAN_POINT ( 'NONE',  ( 62.01418705508225315, 38.95383793066456946, 16.66584972136411480 ) ) ;
#73617 = AXIS2_PLACEMENT_3D ( 'NONE', #63297, #28846, #54107 ) ;
#73618 = CARTESIAN_POINT ( 'NONE',  ( 7.188101187499999156, -29.75000000204838813, 2.977408999572654924 ) ) ;
#73619 = CARTESIAN_POINT ( 'NONE',  ( 6.575918192882435065, -3.850883087735915922, -6.669925161966313354 ) ) ;
#73620 = EDGE_CURVE ( 'NONE', #77744, #32226, #70870, .T. ) ;
#73621 = VERTEX_POINT ( 'NONE', #22061 ) ;
#73622 = CARTESIAN_POINT ( 'NONE',  ( 48.02835407290544367, 14.94086294439726892, 16.85535821593427386 ) ) ;
#73623 = PRESENTATION_LAYER_ASSIGNMENT (  '', '', ( #1230 ) ) ;
#73624 = CARTESIAN_POINT ( 'NONE',  ( -35.46673095357269290, 491.6344107835661816, 12.45081314981167786 ) ) ;
#73625 = DIRECTION ( 'NONE',  ( 0.8191520442889975717, 1.003171929053531773E-16, -0.5735764363510378328 ) ) ;
#73626 = CARTESIAN_POINT ( 'NONE',  ( -8.000000000000000000, -24.03125000409677270, -3.313708498984762496 ) ) ;
#73627 = CARTESIAN_POINT ( 'NONE',  ( -8.922269033015549411, -5.000000000000000000, -5.219866590717671784 ) ) ;
#73628 = DIRECTION ( 'NONE',  ( -1.000000000000000000, -0.000000000000000000, -0.000000000000000000 ) ) ;
#73629 = AXIS2_PLACEMENT_3D ( 'NONE', #69314, #51511, #52040 ) ;
#73630 = FACE_OUTER_BOUND ( 'NONE', #101835, .T. ) ;
#73631 = AXIS2_PLACEMENT_3D ( 'NONE', #76957, #92074, #12216 ) ;
#73632 = CARTESIAN_POINT ( 'NONE',  ( -5.920512269712092213, 4.608878292434047452, 5.000000000000000888 ) ) ;
#73633 = DIRECTION ( 'NONE',  ( -1.000000000000000000, -1.224606353822377258E-16, -0.000000000000000000 ) ) ;
#73634 = CARTESIAN_POINT ( 'NONE',  ( -3.827754797006719834, 15.98931925350938243, -9.240220675753395341 ) ) ;
#73635 = EDGE_LOOP ( 'NONE', ( #81745, #59289, #59081, #33637, #39477, #42310 ) ) ;
#73636 = PRESENTATION_STYLE_ASSIGNMENT (( #97382 ) ) ;
#73637 = CARTESIAN_POINT ( 'NONE',  ( 0.000000000000000000, 12.00000000000000000, 0.000000000000000000 ) ) ;
#73638 = CARTESIAN_POINT ( 'NONE',  ( -5.000000000000000000, -57.08340687971455196, 10.85455823726397284 ) ) ;
#73639 = CARTESIAN_POINT ( 'NONE',  ( -97.74289867503729567, -29.99999999999999645, 190.7460677368483459 ) ) ;
#73640 = ADVANCED_FACE ( 'NONE', ( #79209 ), #69015, .T. ) ;
#73641 = STYLED_ITEM ( 'NONE', ( #30475 ), #26496 ) ;
#73642 = CARTESIAN_POINT ( 'NONE',  ( -41.31945219041483597, 484.8187774037884878, -3.609221751577367243 ) ) ;
#73643 = VECTOR ( 'NONE', #30754, 1000.000000000000000 ) ;
#73644 = CARTESIAN_POINT ( 'NONE',  ( 59.91412286587753755, -57.67713599549763615, 107.0922378007342672 ) ) ;
#73646 = CARTESIAN_POINT ( 'NONE',  ( -9.466035365373274502, 7.112811939922738524, 2.503306211807451831 ) ) ;
#73645 = CARTESIAN_POINT ( 'NONE',  ( 7.999999999999998224, -15.78125000409677092, 3.313708498984766049 ) ) ;
#73647 = CARTESIAN_POINT ( 'NONE',  ( 10.51353532556417214, -22.75354294893093865, -38.54225802751280838 ) ) ;
#73648 = CARTESIAN_POINT ( 'NONE',  ( -4.237512335919120849E-14, 43.17555810750860701, 18.75000000000000355 ) ) ;
#73649 =( LENGTH_UNIT ( ) NAMED_UNIT ( * ) SI_UNIT ( .MILLI., .METRE. ) );
#73650 = CARTESIAN_POINT ( 'NONE',  ( -12.63134323606425191, -60.00000000000000000, 39.70362636174434101 ) ) ;
#73651 = PRESENTATION_LAYER_ASSIGNMENT (  '', '', ( #68525 ) ) ;
#73652 = CIRCLE ( 'NONE', #6438, 4.172000000000001485 ) ;
#73653 = CONICAL_SURFACE ( 'NONE', #46125, 3.309500000000001663, 0.9599310885968770357 ) ;
#73654 = B_SPLINE_CURVE_WITH_KNOTS ( 'NONE', 3,
 ( #28618, #94390, #61499, #29162, #72734, #80294, #56548, #73256 ),
 .UNSPECIFIED., .F., .F.,
 ( 4, 2, 2, 4 ),
 ( 0.003797433802554452380, 0.004743183970586247432, 0.005688934138618043784, 0.007580434474681633887 ),
 .UNSPECIFIED. ) ;
#73655 = CARTESIAN_POINT ( 'NONE',  ( 12.00983892818876697, 17.07531081145824103, 9.138738903015008574 ) ) ;
#73656 = CARTESIAN_POINT ( 'NONE',  ( 36.19631612776407792, 463.3208255589806299, 20.09850791239177070 ) ) ;
#73657 = CARTESIAN_POINT ( 'NONE',  ( -86.30857863919766260, -53.80050282809293094, 192.2617187078320171 ) ) ;
#73658 = ORIENTED_EDGE ( 'NONE', *, *, #38225, .F. ) ;
#73659 = CARTESIAN_POINT ( 'NONE',  ( 17.49999999999850431, 50.00907933620509027, 60.12834585265864007 ) ) ;
#73660 = CARTESIAN_POINT ( 'NONE',  ( 11.20469880689023334, -9.947014048322465385, 18.60075416151417471 ) ) ;
#73661 = CARTESIAN_POINT ( 'NONE',  ( -8.254083131201605639, -49.92098614289960068, 32.20337770899964625 ) ) ;
#73662 = PRESENTATION_STYLE_ASSIGNMENT (( #45304 ) ) ;
#73663 = PRESENTATION_LAYER_ASSIGNMENT (  '', '', ( #82294 ) ) ;
#73665 = CARTESIAN_POINT ( 'NONE',  ( -8.559508646656370345, 53.68473964988125857, 4.031152949374564365 ) ) ;
#73664 = FACE_OUTER_BOUND ( 'NONE', #101086, .T. ) ;
#73666 = EDGE_CURVE ( 'NONE', #93357, #88074, #24390, .T. ) ;
#73667 = VERTEX_POINT ( 'NONE', #63036 ) ;
#73668 = COLOUR_RGB ( '', 0.31764706, 0.68627451, 0.89019608) ;
#73669 = CARTESIAN_POINT ( 'NONE',  ( -6.731961105522484168, -4.334285474471498034, -16.87634736350372222 ) ) ;
#73670 = CARTESIAN_POINT ( 'NONE',  ( 16.11128504972181119, 35.08385997426073288, 21.97063235475975063 ) ) ;
#73671 = CARTESIAN_POINT ( 'NONE',  ( 31.42582775662773642, 298.3612856942310145, -9.227187029712617061 ) ) ;
#73672 = CARTESIAN_POINT ( 'NONE',  ( 18.09999999999999787, 1.533819458162526451E-15, 0.000000000000000000 ) ) ;
#73673 = EDGE_CURVE ( 'NONE', #38219, #59944, #8795, .T. ) ;
#73674 = CARTESIAN_POINT ( 'NONE',  ( -7.619135598915496743, -81.82694632215323338, 2.449260492474795825 ) ) ;
#73675 = FACE_OUTER_BOUND ( 'NONE', #67971, .T. ) ;
#73676 = VECTOR ( 'NONE', #35282, 1000.000000000000000 ) ;
#73677 = CARTESIAN_POINT ( 'NONE',  ( 108.8020855619825653, -30.00000000000001066, 184.6883589252716433 ) ) ;
#73678 = CARTESIAN_POINT ( 'NONE',  ( -21.23684446602553777, 304.9566545053270943, -9.977713076987676288 ) ) ;
#73679 = VERTEX_POINT ( 'NONE', #78662 ) ;
#73680 = CARTESIAN_POINT ( 'NONE',  ( -7.869731216972585486, -29.99999999999999645, 0.3816394668114562738 ) ) ;
#73681 = CARTESIAN_POINT ( 'NONE',  ( -9.176803346051528365, 250.5294715579742899, 3.973598758023538124 ) ) ;
#73682 = CARTESIAN_POINT ( 'NONE',  ( 13.37207953394533355, 3.851859888774471706E-31, 5.000000000000001776 ) ) ;
#73683 = FACE_OUTER_BOUND ( 'NONE', #16031, .T. ) ;
#73685 = CONICAL_SURFACE ( 'NONE', #59948, 15.00000000000000178, 0.7292773806962717931 ) ;
#73684 = DIRECTION ( 'NONE',  ( 0.000000000000000000, 0.000000000000000000, 1.000000000000000000 ) ) ;
#73686 = CYLINDRICAL_SURFACE ( 'NONE', #25239, 61.50000000000000000 ) ;
#73687 = VERTEX_POINT ( 'NONE', #95938 ) ;
#73688 = EDGE_CURVE ( 'NONE', #103417, #53703, #48440, .T. ) ;
#73689 = CARTESIAN_POINT ( 'NONE',  ( -23.27911350275410030, 305.7949572072080286, 9.142907481312498419 ) ) ;
#73690 = ORIENTED_EDGE ( 'NONE', *, *, #78838, .T. ) ;
#73691 = CARTESIAN_POINT ( 'NONE',  ( -8.000000000000000000, 0.000000000000000000, -1.875285714285714445 ) ) ;
#73692 = FACE_OUTER_BOUND ( 'NONE', #69039, .T. ) ;
#73693 = CARTESIAN_POINT ( 'NONE',  ( 9.721734870800576189, 46.20860777233757233, 13.03934063175024605 ) ) ;
#73694 = ORIENTED_EDGE ( 'NONE', *, *, #8243, .F. ) ;
#73695 = CARTESIAN_POINT ( 'NONE',  ( 62.59524157948160905, 49.99999999997998401, 18.50207713769105311 ) ) ;
#73696 = CARTESIAN_POINT ( 'NONE',  ( 5.000000000000160760, -12.34932486159375031, 8.854147762509146702 ) ) ;
#73697 = CARTESIAN_POINT ( 'NONE',  ( -55.85648761906974613, -60.00000000001953282, 95.11638450465373751 ) ) ;
#73699 = DIRECTION ( 'NONE',  ( 0.000000000000000000, -1.000000000000000000, 0.000000000000000000 ) ) ;
#73698 = AXIS2_PLACEMENT_3D ( 'NONE', #75104, #10378, #57863 ) ;
#73700 = CARTESIAN_POINT ( 'NONE',  ( 93.94670038468932205, -60.00000000000001421, 41.20803089316482470 ) ) ;
#73702 = CARTESIAN_POINT ( 'NONE',  ( 16.01724265899924049, -60.35821680913219467, 34.15402070262287282 ) ) ;
#73701 = CARTESIAN_POINT ( 'NONE',  ( -109.5916892278405470, -30.00000000000001776, 172.2591039824585550 ) ) ;
#73704 = CARTESIAN_POINT ( 'NONE',  ( 87.09402098694862104, -38.00000000000002132, 60.21609768695862641 ) ) ;
#73703 = UNCERTAINTY_MEASURE_WITH_UNIT (LENGTH_MEASURE( 1.000000000000000082E-05 ), #40480, 'distance_accuracy_value', 'NONE');
#73705 = AXIS2_PLACEMENT_3D ( 'NONE', #10060, #16562, #65646 ) ;
#73706 = CARTESIAN_POINT ( 'NONE',  ( -46.15598990074098396, -18.78241605370739009, 39.24116979527025251 ) ) ;
#73707 = CARTESIAN_POINT ( 'NONE',  ( -0.7862528207961816396, 34.26448653555612367, -29.48533061255973564 ) ) ;
#73708 = ORIENTED_EDGE ( 'NONE', *, *, #99432, .F. ) ;
#73709 = DIRECTION ( 'NONE',  ( 0.9921085174016663899, 0.1089071661330606455, -0.06212824529900790038 ) ) ;
#73710 = CARTESIAN_POINT ( 'NONE',  ( 5.964242399901847236, -13.95070288504633638, 13.91433285878922632 ) ) ;
#73711 = CIRCLE ( 'NONE', #29050, 4.000000000000001776 ) ;
#73712 = DIRECTION ( 'NONE',  ( -1.000000000000000000, -1.224606353822377258E-16, -0.000000000000000000 ) ) ;
#73713 = CARTESIAN_POINT ( 'NONE',  ( 19.34999999999999787, 3.309500000000003439, 4.052968581778167743E-16 ) ) ;
#73714 = CARTESIAN_POINT ( 'NONE',  ( 35.69739812508499455, 430.4862580793411553, 4.964222856391316441 ) ) ;
#73715 = EDGE_LOOP ( 'NONE', ( #38694, #55291, #70877, #71705 ) ) ;
#73716 = CARTESIAN_POINT ( 'NONE',  ( 5.833333333391548692, -46.26205164321707741, 103.8776713793676834 ) ) ;
#73717 = ORIENTED_EDGE ( 'NONE', *, *, #66560, .F. ) ;
#73718 = CARTESIAN_POINT ( 'NONE',  ( 78.24277327743527621, -29.99999999990264499, 183.8761278456963453 ) ) ;
#73719 = CARTESIAN_POINT ( 'NONE',  ( 15.51400478511171244, 41.97981636269011574, -85.80391510450277792 ) ) ;
#73720 = CARTESIAN_POINT ( 'NONE',  ( 23.38236582681999920, 25.21829724408700812, -33.20617127781077471 ) ) ;
#73721 = CARTESIAN_POINT ( 'NONE',  ( 4.852941176470595863, 39.99999999999999289, -70.80672828634229177 ) ) ;
#73722 = CARTESIAN_POINT ( 'NONE',  ( 100.5432165947128453, -30.00000000000000711, 159.7633814667663330 ) ) ;
#73723 = CARTESIAN_POINT ( 'NONE',  ( -30.00000000000000000, 500.0000000000002274, 0.000000000000000000 ) ) ;
#73724 = ORIENTED_EDGE ( 'NONE', *, *, #2506, .T. ) ;
#73725 = EDGE_CURVE ( 'NONE', #72821, #12582, #69114, .T. ) ;
#73726 = EDGE_LOOP ( 'NONE', ( #44277, #77806, #92663, #49833, #41790 ) ) ;
#73727 = ORIENTED_EDGE ( 'NONE', *, *, #6369, .F. ) ;
#73728 = CIRCLE ( 'NONE', #8282, 0.5000000000000004441 ) ;
#73729 = CARTESIAN_POINT ( 'NONE',  ( 0.7145311798163210826, 4.618802153517001408, -8.000000000000000000 ) ) ;
#73730 = CARTESIAN_POINT ( 'NONE',  ( -5.911961378333534967, -11.74849339892130295, -9.342346711816039928 ) ) ;
#73731 = COLOUR_RGB ( '', 0.40784314, 0.44705882, 0.49803922) ;
#73732 = PRESENTATION_LAYER_ASSIGNMENT (  '', '', ( #104769 ) ) ;
#73733 = CARTESIAN_POINT ( 'NONE',  ( -39.43334695255446576, 464.6962277817929134, 18.31103035469426388 ) ) ;
#73734 = EDGE_CURVE ( 'NONE', #63037, #16979, #58089, .T. ) ;
#73735 = EDGE_CURVE ( 'NONE', #95748, #112, #86795, .T. ) ;
#73736 = EDGE_LOOP ( 'NONE', ( #23318, #90455, #86435, #66939, #50911, #59118 ) ) ;
#73737 = CARTESIAN_POINT ( 'NONE',  ( 9.699189539447123920, 108.1769222824671175, -2.444343703917212007 ) ) ;
#73738 = ORIENTED_EDGE ( 'NONE', *, *, #43432, .F. ) ;
#73739 = DIRECTION ( 'NONE',  ( 0.000000000000000000, -1.000000000000000000, 0.000000000000000000 ) ) ;
#73740 = CARTESIAN_POINT ( 'NONE',  ( 81.30285530623764600, -38.84117475569783551, 195.0272007915274060 ) ) ;
#73741 = DIRECTION ( 'NONE',  ( 0.000000000000000000, 0.000000000000000000, -1.000000000000000000 ) ) ;
#73742 = CARTESIAN_POINT ( 'NONE',  ( 28.87552933249129339, 311.5367771203828511, 12.02311567741501364 ) ) ;
#73743 = AXIS2_PLACEMENT_3D ( 'NONE', #39437, #12469, #105217 ) ;
#73744 = CARTESIAN_POINT ( 'NONE',  ( 41.46910480218706851, 484.7338956289814860, -3.418960549715459596 ) ) ;
#73745 = ADVANCED_FACE ( 'NONE', ( #77624 ), #79739, .T. ) ;
#73746 = DIRECTION ( 'NONE',  ( -0.000000000000000000, -1.000000000000000000, -0.000000000000000000 ) ) ;
#73747 = CARTESIAN_POINT ( 'NONE',  ( -41.54789589616743939, 460.8787123354538835, 2.862784844401427886 ) ) ;
#73748 = LINE ( 'NONE', #74804, #47143 ) ;
#73749 = CARTESIAN_POINT ( 'NONE',  ( 0.000000000000000000, 0.000000000000000000, 0.000000000000000000 ) ) ;
#73750 = EDGE_CURVE ( 'NONE', #54099, #17876, #99132, .T. ) ;
#73751 = DIRECTION ( 'NONE',  ( -0.8191520442889884679, 1.003171929053520679E-16, 0.5735764363510508224 ) ) ;
#73752 = ORIENTED_EDGE ( 'NONE', *, *, #74125, .T. ) ;
#73753 = CONICAL_SURFACE ( 'NONE', #8310, 7.000000000000000000, 0.9599310885968753704 ) ;
#73754 = CARTESIAN_POINT ( 'NONE',  ( 2.691782409370788276, -49.46317646816598312, 103.4277688390371281 ) ) ;
#73755 = CARTESIAN_POINT ( 'NONE',  ( 5.430163322397451253, 41.93410894844108583, -59.17461580565397128 ) ) ;
#73756 = DIRECTION ( 'NONE',  ( -1.000000000000000000, -1.224606353822377258E-16, -0.000000000000000000 ) ) ;
#73757 = CYLINDRICAL_SURFACE ( 'NONE', #19725, 5.000000000000002665 ) ;
#73758 = CARTESIAN_POINT ( 'NONE',  ( -3.313708498984760720, -10.53124999999999112, -8.000000000000000000 ) ) ;
#73759 = DIRECTION ( 'NONE',  ( -1.000000000000000000, -0.000000000000000000, -0.000000000000000000 ) ) ;
#73760 = ADVANCED_FACE ( 'NONE', ( #32810, #23657 ), #6365, .T. ) ;
#73761 = CARTESIAN_POINT ( 'NONE',  ( -8.000113193197769590, 100.9997736135413788, -0.2613481123984672250 ) ) ;
#73762 = CONICAL_SURFACE ( 'NONE', #56508, 4.000000000000001776, 0.9599310885968808105 ) ;
#73763 = EDGE_LOOP ( 'NONE', ( #17789, #49259, #9908, #9601, #16961 ) ) ;
#73764 = CARTESIAN_POINT ( 'NONE',  ( 86.32898320831061767, -21.03587308976179671, 180.4856531993580973 ) ) ;
#73765 = B_SPLINE_CURVE_WITH_KNOTS ( 'NONE', 3,
 ( #34072, #8689, #35130, #100356, #66945, #74479, #91750, #91231, #59392, #50212 ),
 .UNSPECIFIED., .F., .F.,
 ( 4, 2, 2, 2, 4 ),
 ( 0.000000000000000000, 0.001268689343002603895, 0.002537378686005207790, 0.003806068029007811902, 0.005074757372010415581 ),
 .UNSPECIFIED. ) ;
#73766 = FACE_OUTER_BOUND ( 'NONE', #80328, .T. ) ;
#73767 = ORIENTED_EDGE ( 'NONE', *, *, #72078, .F. ) ;
#73768 = CARTESIAN_POINT ( 'NONE',  ( 92.45459292580818556, -57.65848211217247865, -18.44663115571118439 ) ) ;
#73769 = CARTESIAN_POINT ( 'NONE',  ( -4.250000000000000000, 5.204748896376250699E-16, -6.235812796514431433 ) ) ;
#73770 = DIRECTION ( 'NONE',  ( 0.000000000000000000, 0.000000000000000000, -1.000000000000000000 ) ) ;
#73771 = FILL_AREA_STYLE_COLOUR ( '', #13132 ) ;
#73772 = CARTESIAN_POINT ( 'NONE',  ( -81.53069149982411545, -30.00000000000001421, -8.902666450183531310 ) ) ;
#73773 = AXIS2_PLACEMENT_3D ( 'NONE', #94925, #43691, #44236 ) ;
#73774 = CARTESIAN_POINT ( 'NONE',  ( -81.88346289758811736, -38.00000000000000000, 157.3757661605745284 ) ) ;
#73775 = CARTESIAN_POINT ( 'NONE',  ( 8.000000000000000000, -3.000000000000000000, -2.094395098902536834 ) ) ;
#73776 = DIRECTION ( 'NONE',  ( 0.000000000000000000, -1.000000000000000000, 0.000000000000000000 ) ) ;
#73778 = CARTESIAN_POINT ( 'NONE',  ( 89.64643850830432825, 5.000000000000020428, 0.000000000000000000 ) ) ;
#73777 = DIRECTION ( 'NONE',  ( 0.000000000000000000, 0.000000000000000000, -1.000000000000000000 ) ) ;
#73779 = DIRECTION ( 'NONE',  ( -0.000000000000000000, -0.000000000000000000, -1.000000000000000000 ) ) ;
#73780 = CARTESIAN_POINT ( 'NONE',  ( -28.43341640144473814, 17.76796145515719516, 40.78017990900028877 ) ) ;
#73781 = CARTESIAN_POINT ( 'NONE',  ( -12.50000000000000711, -4.999999999999999112, -79.51734232575269345 ) ) ;
#73782 = DIRECTION ( 'NONE',  ( 0.000000000000000000, 0.000000000000000000, -1.000000000000000000 ) ) ;
#73783 = CARTESIAN_POINT ( 'NONE',  ( -21.97265383647320292, 25.82522707506753790, 32.15451870283014557 ) ) ;
#73784 = FILL_AREA_STYLE ('',( #16085 ) ) ;
#73785 = CIRCLE ( 'NONE', #87595, 4.000000000000001776 ) ;
#73786 = CARTESIAN_POINT ( 'NONE',  ( -4.981862520314373377, 6.112127992515964325E-16, -0.01270000000000090501 ) ) ;
#73787 = AXIS2_PLACEMENT_3D ( 'NONE', #29917, #97797, #7192 ) ;
#73788 = EDGE_LOOP ( 'NONE', ( #80291, #13213, #9902, #22653 ) ) ;
#73789 = DIRECTION ( 'NONE',  ( 0.000000000000000000, 0.000000000000000000, 1.000000000000000000 ) ) ;
#73790 = DIRECTION ( 'NONE',  ( 0.000000000000000000, 0.000000000000000000, -1.000000000000000000 ) ) ;
#73791 = CARTESIAN_POINT ( 'NONE',  ( 32.85155332502863956, 463.8111683108725174, 7.359358840565810134 ) ) ;
#73792 = CARTESIAN_POINT ( 'NONE',  ( -33.00000000000000000, 434.0826380246136296, 11.57835738278528659 ) ) ;
#73793 =( BOUNDED_SURFACE ( )  B_SPLINE_SURFACE ( 3, 2, ( 
 ( #37752, #103504, #22628 ),
 ( #55981, #46337, #72200 ),
 ( #96484, #97002, #21554 ),
 ( #38784, #30711, #105104 ),
 ( #71651, #4816, #21045 ),
 ( #88392, #5352, #6385 ) ),
 .UNSPECIFIED., .F., .F., .F. ) 
 B_SPLINE_SURFACE_WITH_KNOTS ( ( 4, 2, 4 ),
 ( 3, 3 ),
 ( 0.06198440071626125369, 0.07559254306859702899, 0.08920068542093280428 ),
 ( 0.000000000000000000, 0.6299191188712893741 ),
 .UNSPECIFIED. ) 
 GEOMETRIC_REPRESENTATION_ITEM ( )  RATIONAL_B_SPLINE_SURFACE ( (
 ( 1.000000000000000000, 0.8155006202972323592, 0.8634406139837984551),
 ( 1.000000000000000000, 0.8155004682860759191, 0.8634405014709529702),
 ( 1.000000000000000000, 0.8155003797931379417, 0.8634404359718641508),
 ( 1.000000000000000000, 0.8155004189615391308, 0.8634404649628169004),
 ( 1.000000000000000000, 0.8155005447095090565, 0.8634405580366559807),
 ( 1.000000000000000000, 0.8155006922796284030, 0.8634406672624155288) ) ) 
 REPRESENTATION_ITEM ( '' )  SURFACE ( )  );
#73795 = CARTESIAN_POINT ( 'NONE',  ( -62.72865154022586154, -21.76998117876125960, -22.22417429766882080 ) ) ;
#73794 = CARTESIAN_POINT ( 'NONE',  ( -4.463429423125060858, 13.01149508916975428, -0.1387913946425749778 ) ) ;
#73796 = EDGE_CURVE ( 'NONE', #76618, #20011, #65682, .T. ) ;
#73797 = EDGE_LOOP ( 'NONE', ( #27035, #2118, #101567, #99985 ) ) ;
#73798 = CIRCLE ( 'NONE', #1422, 4.172000000000009479 ) ;
#73799 = ORIENTED_EDGE ( 'NONE', *, *, #16880, .F. ) ;
#73800 = CARTESIAN_POINT ( 'NONE',  ( -25.89634907308706246, 35.00173212496974884, 9.164867755282383399 ) ) ;
#73801 = CONICAL_SURFACE ( 'NONE', #48010, 3.309500000000001663, 0.9599310885968770357 ) ;
#73802 = EDGE_CURVE ( 'NONE', #89178, #57603, #46694, .T. ) ;
#73803 = ADVANCED_FACE ( 'NONE', ( #31228 ), #64116, .F. ) ;
#73804 = CARTESIAN_POINT ( 'NONE',  ( -5.656854249492381470, -29.56249999999999645, 5.656854249492379694 ) ) ;
#73805 = SURFACE_SIDE_STYLE ('',( #57605 ) ) ;
#73806 = CARTESIAN_POINT ( 'NONE',  ( -66.14779852596444698, -60.00000000000000000, -33.84381125176143001 ) ) ;
#73807 = ORIENTED_EDGE ( 'NONE', *, *, #34598, .F. ) ;
#73808 = CARTESIAN_POINT ( 'NONE',  ( 56.93684650526180491, -37.03532724266435849, -26.56149101784519928 ) ) ;
#73809 = CARTESIAN_POINT ( 'NONE',  ( -2.256328376251533818, 294.8363286739503337, -9.758570717811821282 ) ) ;
#73810 = VECTOR ( 'NONE', #1586, 1000.000000000000000 ) ;
#73811 = CARTESIAN_POINT ( 'NONE',  ( 94.99852919210989910, -37.71004738711080506, 193.0139001793616558 ) ) ;
#73813 = CARTESIAN_POINT ( 'NONE',  ( -46.86248696599245989, 13.70470512780033978, 15.14813956650301385 ) ) ;
#73812 = DIRECTION ( 'NONE',  ( -0.000000000000000000, 1.000000000000000000, 0.000000000000000000 ) ) ;
#73814 = ADVANCED_FACE ( 'NONE', ( #100695 ), #92076, .T. ) ;
#73815 = ORIENTED_EDGE ( 'NONE', *, *, #47989, .T. ) ;
#73816 = EDGE_CURVE ( 'NONE', #101881, #28693, #82875, .T. ) ;
#73817 = ORIENTED_EDGE ( 'NONE', *, *, #46985, .F. ) ;
#73818 = ORIENTED_EDGE ( 'NONE', *, *, #86503, .T. ) ;
#73819 = CARTESIAN_POINT ( 'NONE',  ( 32.16579691290905174, 416.1863149338369681, 25.51939566887129018 ) ) ;
#73820 = CARTESIAN_POINT ( 'NONE',  ( -5.000000000000039080, -12.81882114893590341, 11.98449427369159004 ) ) ;
#73821 = CARTESIAN_POINT ( 'NONE',  ( 10.28624191511809371, -1.200000000000000030E-05, -14.15779740156171584 ) ) ;
#73822 = EDGE_LOOP ( 'NONE', ( #32788, #104449, #16945, #73244, #7867 ) ) ;
#73823 = CARTESIAN_POINT ( 'NONE',  ( 15.42941528477435398, 46.21391461311947779, -5.098611828030635174 ) ) ;
#73824 = CARTESIAN_POINT ( 'NONE',  ( -88.26372640434641426, 34.25047185182970111, 44.13186320217319292 ) ) ;
#73825 = VECTOR ( 'NONE', #1074, 1000.000000000000000 ) ;
#73826 = LINE ( 'NONE', #32869, #59902 ) ;
#73827 = CARTESIAN_POINT ( 'NONE',  ( -39.01690548088378563, -57.69424739071683916, 54.12508632231112671 ) ) ;
#73828 = CARTESIAN_POINT ( 'NONE',  ( 2.977408999572650927, -29.37500000204838457, -7.188101187500001821 ) ) ;
#73829 = CARTESIAN_POINT ( 'NONE',  ( -29.68315524076957246, 18.29184282782463455, 39.60535821593508388 ) ) ;
#73830 = AXIS2_PLACEMENT_3D ( 'NONE', #39842, #30709, #55980 ) ;
#73831 = CARTESIAN_POINT ( 'NONE',  ( 1.130019378125521223, 27.54905683648467729, -40.04036428441008155 ) ) ;
#73832 = CARTESIAN_POINT ( 'NONE',  ( 25.62974135805828979, -60.00000000000002132, -43.76006462505735328 ) ) ;
#73833 = CARTESIAN_POINT ( 'NONE',  ( -35.98784834194372451, -29.99999999999998934, 43.73664282352994803 ) ) ;
#73834 = AXIS2_PLACEMENT_3D ( 'NONE', #58904, #18453, #69123 ) ;
#73835 = CARTESIAN_POINT ( 'NONE',  ( -51.81172722203650949, -56.84363277413236659, 60.27128131545431700 ) ) ;
#73836 = AXIS2_PLACEMENT_3D ( 'NONE', #61752, #20795, #95169 ) ;
#73837 = CARTESIAN_POINT ( 'NONE',  ( 0.5361540264281685619, 21.82547874031371649, -6.984343682103323125 ) ) ;
#73838 = ORIENTED_EDGE ( 'NONE', *, *, #78132, .F. ) ;
#73839 = CARTESIAN_POINT ( 'NONE',  ( -100.1592349301962628, -52.75790702199028459, 194.0880419080440618 ) ) ;
#73840 = CARTESIAN_POINT ( 'NONE',  ( -1.338640380347093206, 297.3185856424206008, -10.00123718159664321 ) ) ;
#73841 = VECTOR ( 'NONE', #30, 1000.000000000000000 ) ;
#73842 = CARTESIAN_POINT ( 'NONE',  ( 11.47368253460178700, 2.275697256493656617, 14.82749015516199087 ) ) ;
#73843 = ORIENTED_EDGE ( 'NONE', *, *, #101333, .T. ) ;
#73844 = CARTESIAN_POINT ( 'NONE',  ( 0.000000000000000000, 0.000000000000000000, 5.000000000000002665 ) ) ;
#73845 = CARTESIAN_POINT ( 'NONE',  ( 74.44968402934742358, -38.32904790398288952, 164.3025046429760323 ) ) ;
#73846 = CARTESIAN_POINT ( 'NONE',  ( 36.08349330513379982, 1.593028355512270962E-15, 0.000000000000000000 ) ) ;
#73847 = CARTESIAN_POINT ( 'NONE',  ( -6.309776332879510896, 51.28523556860736221, -8.023844445462220420 ) ) ;
#73848 = CARTESIAN_POINT ( 'NONE',  ( -12.23762156676873758, 302.5837270733004516, 9.880035066194738036 ) ) ;
#73849 = DIRECTION ( 'NONE',  ( 0.000000000000000000, 1.000000000000000000, 0.000000000000000000 ) ) ;
#73850 = CARTESIAN_POINT ( 'NONE',  ( 84.64943319986461745, -30.00000000000001066, 166.9899077754115808 ) ) ;
#73851 = CARTESIAN_POINT ( 'NONE',  ( -10.92836421268331293, 43.17363766063942165, -15.24329784724702996 ) ) ;
#73852 = CARTESIAN_POINT ( 'NONE',  ( -28.94979900162252662, 13.71034195483037443, 39.84012157007414601 ) ) ;
#73853 = FACE_OUTER_BOUND ( 'NONE', #14564, .T. ) ;
#73854 = CIRCLE ( 'NONE', #1545, 5.000000000000010658 ) ;
#73855 = VERTEX_POINT ( 'NONE', #10622 ) ;
#73856 = ORIENTED_EDGE ( 'NONE', *, *, #96705, .T. ) ;
#73857 = CARTESIAN_POINT ( 'NONE',  ( 48.95189267709701397, -60.28532577491037614, 55.82551791209952796 ) ) ;
#73858 = CARTESIAN_POINT ( 'NONE',  ( 6.542885630808934927, 41.77241054322398384, -59.03854290128418825 ) ) ;
#73859 = CARTESIAN_POINT ( 'NONE',  ( 36.31383080563109189, 28.20116312085306731, -12.06289833560200009 ) ) ;
#73860 = ADVANCED_FACE ( 'NONE', ( #9024 ), #50022, .T. ) ;
#73861 = ORIENTED_EDGE ( 'NONE', *, *, #37039, .T. ) ;
#73862 = CARTESIAN_POINT ( 'NONE',  ( -92.64563826212697961, -38.35495884179172066, 40.48894988335383260 ) ) ;
#73863 = VERTEX_POINT ( 'NONE', #59201 ) ;
#73864 = CARTESIAN_POINT ( 'NONE',  ( 35.90484354297773706, 1.340359594676612611E-15, 0.000000000000000000 ) ) ;
#73865 = CARTESIAN_POINT ( 'NONE',  ( 97.20990545091203217, -38.35580220330457024, 71.88490386968666712 ) ) ;
#73866 = CARTESIAN_POINT ( 'NONE',  ( 11.80490210714441801, 16.44756287846985288, -9.391209061505895406 ) ) ;
#73867 = CARTESIAN_POINT ( 'NONE',  ( 103.1286089144194733, -52.71713921426092497, 144.4394181523613554 ) ) ;
#73868 = CARTESIAN_POINT ( 'NONE',  ( 95.42421628608209971, 1.030564683017419500E-14, 0.000000000000000000 ) ) ;
#73869 = CARTESIAN_POINT ( 'NONE',  ( 21.99817791066577044, 28.09376123749147069, 31.66916887880059761 ) ) ;
#73870 = CARTESIAN_POINT ( 'NONE',  ( -35.30859608300242058, 361.7926923559893453, 3.555634394399922904 ) ) ;
#73871 = CARTESIAN_POINT ( 'NONE',  ( 6.683837171061802529, 3.955946848495958346, -6.851900933636989599 ) ) ;
#73872 = B_SPLINE_CURVE_WITH_KNOTS ( 'NONE', 3,
 ( #28787, #62709, #77828, #3937, #87516, #71311, #13597, #38445, #36349, #104204, #44398, #12011, #94559, #30349, #63241, #85390, #11470, #77295, #94006, #3406, #69219, #102086, #20167, #16259, #31425, #15194, #90154, #64300, #56708, #47559, #7620, #55115, #72888, #40016 ),
 .UNSPECIFIED., .F., .F.,
 ( 4, 2, 2, 2, 2, 2, 2, 2, 2, 2, 2, 2, 2, 2, 2, 2, 4 ),
 ( 0.01257177810263095975, 0.01335728547384937119, 0.01414279284506778263, 0.01492830021628619580, 0.01571380758750460724, 0.01649931495872301868, 0.01728482232994143011, 0.01807032970115984155, 0.01885583707237825299, 0.01964134444359666443, 0.02042685181481507933, 0.02121235918603348730, 0.02199786655725190221, 0.02278337392847031018, 0.02356888129968872508, 0.02435438867090713652, 0.02513989604212554796 ),
 .UNSPECIFIED. ) ;
#73873 = CARTESIAN_POINT ( 'NONE',  ( 76.72974224477856353, -59.99999999999997868, 189.6511138508473095 ) ) ;
#73874 = FACE_OUTER_BOUND ( 'NONE', #85986, .T. ) ;
#73875 = ORIENTED_EDGE ( 'NONE', *, *, #52200, .F. ) ;
#73876 = CARTESIAN_POINT ( 'NONE',  ( 60.16448956355160504, -18.65125552583483071, 63.02594496277924918 ) ) ;
#73877 = CARTESIAN_POINT ( 'NONE',  ( -23.71817961469832525, 303.5093770010555545, -9.858623782581350525 ) ) ;
#73878 = LINE ( 'NONE', #7018, #63684 ) ;
#73879 = CARTESIAN_POINT ( 'NONE',  ( -9.499963314427418482, -5.000000000000000000, -20.52065077656356351 ) ) ;
#73881 = CARTESIAN_POINT ( 'NONE',  ( -4.278209688530829169, 54.28328794773042176, 6.542503565097912421 ) ) ;
#73880 = CARTESIAN_POINT ( 'NONE',  ( -57.17200305705274133, -29.99999999999333866, 83.43905756859183498 ) ) ;
#73882 = CARTESIAN_POINT ( 'NONE',  ( -39.95193705026029818, 335.6054456153876799, 19.72964827771248864 ) ) ;
#73883 = CARTESIAN_POINT ( 'NONE',  ( -37.56673239365863282, 25.75719283951018568, -10.95617127781023648 ) ) ;
#73884 = CARTESIAN_POINT ( 'NONE',  ( -3.400000000000000355, 4.163799117101001052E-16, -2.716724522925831220 ) ) ;
#73885 = CARTESIAN_POINT ( 'NONE',  ( -8.000000000000000000, -32.84375000000000000, -3.313708498984762496 ) ) ;
#73886 = DIRECTION ( 'NONE',  ( 0.000000000000000000, 0.000000000000000000, -1.000000000000000000 ) ) ;
#73887 = PRESENTATION_LAYER_ASSIGNMENT (  '', '', ( #5070 ) ) ;
#73888 = AXIS2_PLACEMENT_3D ( 'NONE', #77124, #69577, #3239 ) ;
#73889 = CARTESIAN_POINT ( 'NONE',  ( 52.56483885390523625, 48.00000000000000000, -38.23529411764706509 ) ) ;
#73890 = ORIENTED_EDGE ( 'NONE', *, *, #55096, .T. ) ;
#73891 = CARTESIAN_POINT ( 'NONE',  ( 83.11751895291531866, -42.97626541852498860, 176.1565397990591464 ) ) ;
#73892 = EDGE_CURVE ( 'NONE', #53703, #55070, #92610, .T. ) ;
#73893 = FACE_OUTER_BOUND ( 'NONE', #103328, .T. ) ;
#73894 = CARTESIAN_POINT ( 'NONE',  ( 33.74271564777244237, 484.1802673187708592, 2.058285076122321922 ) ) ;
#73895 = EDGE_LOOP ( 'NONE', ( #59711, #106002, #547, #72745 ) ) ;
#73896 = CARTESIAN_POINT ( 'NONE',  ( 12.49955057316562090, -4.332870170068738425, -12.71907580248059233 ) ) ;
#73897 = CARTESIAN_POINT ( 'NONE',  ( 7.101747359470889975, -4.047770588429576044, -17.37629258577385727 ) ) ;
#73898 = CARTESIAN_POINT ( 'NONE',  ( -43.53427904077744159, 41.44002608692422029, -50.65026129109237019 ) ) ;
#73899 = FILL_AREA_STYLE ('',( #81983 ) ) ;
#73900 = TOROIDAL_SURFACE ( 'NONE', #39519, 8.000000000000000000, 1.000000000000000000 ) ;
#73901 = CARTESIAN_POINT ( 'NONE',  ( 6.499999999998793854, -1.392325603687970981, -6.058577540041909515 ) ) ;
#73902 = PRESENTATION_STYLE_ASSIGNMENT (( #81452 ) ) ;
#73905 = CIRCLE ( 'NONE', #27466, 4.000000000000001776 ) ;
#73904 = CARTESIAN_POINT ( 'NONE',  ( -13.51713435554249720, 20.10123978775306242, -7.061460334258709004 ) ) ;
#73903 = CARTESIAN_POINT ( 'NONE',  ( -12.27450249641863245, -21.25525156901051815, 35.59543369205189123 ) ) ;
#73906 = ADVANCED_FACE ( 'NONE', ( #82394 ), #45019, .F. ) ;
#73907 = CARTESIAN_POINT ( 'NONE',  ( 5.082755093536325930, -15.96875000204838635, -5.082755093536325042 ) ) ;
#73908 = CARTESIAN_POINT ( 'NONE',  ( 17.59729583105167094, 294.5991521133998390, -2.053319976387710799 ) ) ;
#73909 = CARTESIAN_POINT ( 'NONE',  ( 4.460876563139990481, -1.165516444892326087, 104.3906876480053398 ) ) ;
#73910 = ORIENTED_EDGE ( 'NONE', *, *, #36375, .F. ) ;
#73911 = CARTESIAN_POINT ( 'NONE',  ( -17.49999999999842260, 50.02580020273055084, 60.61389435658627889 ) ) ;
#73912 = CARTESIAN_POINT ( 'NONE',  ( 23.30083868525793278, 25.23530067567654811, 33.20617127781017786 ) ) ;
#73913 = CARTESIAN_POINT ( 'NONE',  ( -9.061861678394784292, 137.7616487646406256, -5.000000000000000888 ) ) ;
#73914 = DIRECTION ( 'NONE',  ( -1.000000000000000000, 2.498001805406602216E-14, 0.000000000000000000 ) ) ;
#73916 = CARTESIAN_POINT ( 'NONE',  ( 72.23675078389933901, -60.22819274490537822, -25.48594946497165026 ) ) ;
#73915 = CARTESIAN_POINT ( 'NONE',  ( 97.73333333333333428, 1.023464760207051730E-14, 0.000000000000000000 ) ) ;
#73917 = VERTEX_POINT ( 'NONE', #84537 ) ;
#73918 = AXIS2_PLACEMENT_3D ( 'NONE', #75220, #75767, #9414 ) ;
#73919 = CARTESIAN_POINT ( 'NONE',  ( 12.60424787139770153, 18.50010450913565307, -8.389313221795688946 ) ) ;
#73920 = CARTESIAN_POINT ( 'NONE',  ( -4.880198815736334517, 52.15761557286078443, 6.097275048993607172 ) ) ;
#73921 = EDGE_LOOP ( 'NONE', ( #32600, #7585, #1203, #54889, #74978 ) ) ;
#73922 = EDGE_CURVE ( 'NONE', #48619, #102355, #75358, .T. ) ;
#73923 = EDGE_CURVE ( 'NONE', #104224, #46568, #105272, .T. ) ;
#73924 = CARTESIAN_POINT ( 'NONE',  ( 100.6222222222222200, 4.172000000000019249, 0.000000000000000000 ) ) ;
#73925 = AXIS2_PLACEMENT_3D ( 'NONE', #54723, #14268, #87658 ) ;
#73926 = CARTESIAN_POINT ( 'NONE',  ( -31.96306626099171311, 40.83985558186470399, -63.64673710329628165 ) ) ;
#73927 = CARTESIAN_POINT ( 'NONE',  ( -103.7172116487474938, -60.00000000000002132, 102.7823711783175469 ) ) ;
#73928 = CARTESIAN_POINT ( 'NONE',  ( 0.000000000000000000, -100.0000000000000000, 0.000000000000000000 ) ) ;
#73929 = CARTESIAN_POINT ( 'NONE',  ( -12.08334041755991706, 304.5866437775407007, -10.05636128505472726 ) ) ;
#73930 = CARTESIAN_POINT ( 'NONE',  ( 25.95507789760542039, 309.1386286255022924, 10.94030088463808070 ) ) ;
#73931 = DIRECTION ( 'NONE',  ( 0.000000000000000000, -1.000000000000000000, 0.000000000000000000 ) ) ;
#73933 = CARTESIAN_POINT ( 'NONE',  ( -7.126148247341459019, 41.12758119229484066, -58.55282700859728351 ) ) ;
#73932 = CARTESIAN_POINT ( 'NONE',  ( 5.036189802310023111, -5.000000000000002665, -76.26213611588336505 ) ) ;
#73934 = VECTOR ( 'NONE', #92651, 1000.000000000000227 ) ;
#73935 = CARTESIAN_POINT ( 'NONE',  ( -86.07252144299347663, -18.39191110879000490, 166.6798528094340952 ) ) ;
#73936 = ORIENTED_EDGE ( 'NONE', *, *, #63991, .F. ) ;
#73937 = SURFACE_STYLE_FILL_AREA ( #97679 ) ;
#73938 = EDGE_CURVE ( 'NONE', #77629, #3065, #35480, .T. ) ;
#73939 = ORIENTED_EDGE ( 'NONE', *, *, #91432, .F. ) ;
#73940 = VERTEX_POINT ( 'NONE', #43010 ) ;
#73941 = CARTESIAN_POINT ( 'NONE',  ( 86.75754961941542831, -5.000000000000000888, 6.123233995736779101E-16 ) ) ;
#73942 = DIRECTION ( 'NONE',  ( 0.000000000000000000, 0.000000000000000000, 1.000000000000000000 ) ) ;
#73943 = ORIENTED_EDGE ( 'NONE', *, *, #71469, .F. ) ;
#73944 = FACE_OUTER_BOUND ( 'NONE', #54731, .T. ) ;
#73945 = FACE_OUTER_BOUND ( 'NONE', #72555, .T. ) ;
#73946 = DIRECTION ( 'NONE',  ( 0.5735764363510442720, -0.8191520442889930198, 1.003171929053526349E-16 ) ) ;
#73947 = CARTESIAN_POINT ( 'NONE',  ( -7.999885325681426629, -61.00022934870061420, 0.2682325777720057647 ) ) ;
#73948 = CARTESIAN_POINT ( 'NONE',  ( 3.836994546500236414, 17.95060345994707518, -5.000000000000000000 ) ) ;
#73949 = CARTESIAN_POINT ( 'NONE',  ( 11.20323936960019928, -5.000000000000000000, -78.29850497474416215 ) ) ;
#73950 = CARTESIAN_POINT ( 'NONE',  ( 73.33904886068935980, -1.232595164407830946E-29, 4.000000000000007105 ) ) ;
#73951 = PRESENTATION_LAYER_ASSIGNMENT (  '', '', ( #60224 ) ) ;
#73952 = CARTESIAN_POINT ( 'NONE',  ( 109.5313825839763382, -30.00000000000004619, 176.4140126643321196 ) ) ;
#73953 = CARTESIAN_POINT ( 'NONE',  ( -114.3490076612200568, -60.00000000000000000, 164.2604626692111367 ) ) ;
#73954 = CARTESIAN_POINT ( 'NONE',  ( -61.66793082946371385, -32.53820867738551215, 73.28858974252342762 ) ) ;
#73955 = ORIENTED_EDGE ( 'NONE', *, *, #91027, .T. ) ;
#73956 = CARTESIAN_POINT ( 'NONE',  ( 28.09999999999999787, 1.533819458162526451E-15, 0.000000000000000000 ) ) ;
#73957 = CARTESIAN_POINT ( 'NONE',  ( 94.71960157893720123, -59.99999999999998579, 0.7631219686126513579 ) ) ;
#73958 = VERTEX_POINT ( 'NONE', #82927 ) ;
#73959 = CARTESIAN_POINT ( 'NONE',  ( 2.640755779914924649E-05, -39.47262781682785970, 30.46842126240701631 ) ) ;
#73960 =( GEOMETRIC_REPRESENTATION_CONTEXT ( 3 ) GLOBAL_UNCERTAINTY_ASSIGNED_CONTEXT ( ( #4601 ) ) GLOBAL_UNIT_ASSIGNED_CONTEXT ( ( #46399, #103049, #62591 ) ) REPRESENTATION_CONTEXT ( 'NONE', 'WORKASPACE' ) );
#73961 = CARTESIAN_POINT ( 'NONE',  ( -2.977408999572650039, -13.06250000204838280, -7.188101187500000933 ) ) ;
#73962 = CARTESIAN_POINT ( 'NONE',  ( 9.833493305133805151, 1.593028355512270962E-15, 0.000000000000000000 ) ) ;
#73963 = ORIENTED_EDGE ( 'NONE', *, *, #48926, .F. ) ;
#73964 = CARTESIAN_POINT ( 'NONE',  ( 6.817771574508174837, -30.00000000000000000, 2.289596480420060143 ) ) ;
#73965 = VERTEX_POINT ( 'NONE', #67815 ) ;
#73966 = LINE ( 'NONE', #48620, #71770 ) ;
#73967 = CARTESIAN_POINT ( 'NONE',  ( -108.2395898723600851, -60.00000000000000000, 130.5556691422416975 ) ) ;
#73968 = CARTESIAN_POINT ( 'NONE',  ( 7.188101187500001821, -20.93750000204838457, -2.977408999572650483 ) ) ;
#73969 = CARTESIAN_POINT ( 'NONE',  ( 44.25156094338286294, 463.6569123591601738, 7.442995203284897165 ) ) ;
#73970 = CARTESIAN_POINT ( 'NONE',  ( 17.77044000761073050, 43.17862937570248505, -5.955230444982646532 ) ) ;
#73971 = CARTESIAN_POINT ( 'NONE',  ( -5.934175881463731095, 53.39571318504778219, -8.365722538783465723 ) ) ;
#73972 = CARTESIAN_POINT ( 'NONE',  ( 5.000000000000000888, -15.67194501421787756, -10.31047629133739818 ) ) ;
#73973 = CARTESIAN_POINT ( 'NONE',  ( -30.00000000000000355, 461.8163627757389236, 11.11111419090868857 ) ) ;
#73974 = FACE_OUTER_BOUND ( 'NONE', #10933, .T. ) ;
#73975 = DIRECTION ( 'NONE',  ( 0.000000000000000000, -1.000000000000000000, 0.000000000000000000 ) ) ;
#73976 = CARTESIAN_POINT ( 'NONE',  ( 106.3740829544859565, -59.99999999999997868, 177.4779890160187961 ) ) ;
#73977 = CARTESIAN_POINT ( 'NONE',  ( -31.99426222591429081, -29.08333287831730019, 31.97858915124429657 ) ) ;
#73978 = PRESENTATION_LAYER_ASSIGNMENT (  '', '', ( #36157 ) ) ;
#73979 = B_SPLINE_CURVE_WITH_KNOTS ( 'NONE', 3,
 ( #37854, #62120, #78789, #4922 ),
 .UNSPECIFIED., .F., .F.,
 ( 4, 4 ),
 ( 0.0007508562874606444218, 0.02095882498916069175 ),
 .UNSPECIFIED. ) ;
#73980 = DIRECTION ( 'NONE',  ( 0.000000000000000000, 0.000000000000000000, -1.000000000000000000 ) ) ;
#73981 = CARTESIAN_POINT ( 'NONE',  ( 39.39460558282306835, -22.22791209051591466, 34.40903791641994047 ) ) ;
#73982 = DIRECTION ( 'NONE',  ( 0.000000000000000000, -1.000000000000000000, 0.000000000000000000 ) ) ;
#73983 = EDGE_LOOP ( 'NONE', ( #5299, #83061, #90541, #79724 ) ) ;
#73984 = CARTESIAN_POINT ( 'NONE',  ( -7.986452802927059835, 88.97309757691886034, 0.5332468218996367915 ) ) ;
#73985 = CONICAL_SURFACE ( 'NONE', #75679, 4.000000000000001776, 0.9599310885968774798 ) ;
#73986 = EDGE_CURVE ( 'NONE', #57259, #40695, #20952, .T. ) ;
#73987 = CARTESIAN_POINT ( 'NONE',  ( -77.04287001588842543, -38.46292279798635860, 184.5679294465321050 ) ) ;
#73988 = EDGE_LOOP ( 'NONE', ( #44723, #2380, #103185, #32592 ) ) ;
#73990 = CARTESIAN_POINT ( 'NONE',  ( -42.52018344096930491, 435.0260445553154796, 8.239822296475871610 ) ) ;
#73989 = DIRECTION ( 'NONE',  ( -1.000000000000000000, 0.000000000000000000, 0.000000000000000000 ) ) ;
#73991 = CARTESIAN_POINT ( 'NONE',  ( -11.79034953273680664, 6.758388275560107239, 9.087657628957359179 ) ) ;
#73992 = DIRECTION ( 'NONE',  ( 0.000000000000000000, -1.000000000000000000, 0.000000000000000000 ) ) ;
#73993 = CARTESIAN_POINT ( 'NONE',  ( -43.35041983548516953, 465.4837887082163093, 10.07799631915044358 ) ) ;
#73994 = CARTESIAN_POINT ( 'NONE',  ( 6.701893401236465486, 41.44328394225253476, -70.59544911815949320 ) ) ;
#73995 = CARTESIAN_POINT ( 'NONE',  ( 43.58349330513380693, 4.000000000000003553, 0.000000000000000000 ) ) ;
#73996 = CARTESIAN_POINT ( 'NONE',  ( 4.472135954999577834, -85.27329903512642773, -4.000000000000002665 ) ) ;
#73997 = DIRECTION ( 'NONE',  ( -1.000000000000000000, -1.224606353822377258E-16, -0.000000000000000000 ) ) ;
#73998 = CARTESIAN_POINT ( 'NONE',  ( 103.6056036519425021, -60.00000000000000000, 102.1281063761447996 ) ) ;
#73999 = CARTESIAN_POINT ( 'NONE',  ( -5.167237685039475892, -51.69260020507286413, 40.01460860130989516 ) ) ;
#74000 = CARTESIAN_POINT ( 'NONE',  ( -6.928203230275506996, -65.26930929695539874, -4.000000000000002665 ) ) ;
#74001 = ADVANCED_FACE ( 'NONE', ( #26340 ), #25663, .T. ) ;
#74002 = EDGE_LOOP ( 'NONE', ( #39920, #26646, #66453, #43688, #21168 ) ) ;
#74003 = EDGE_CURVE ( 'NONE', #66339, #70791, #10098, .T. ) ;
#74004 = CARTESIAN_POINT ( 'NONE',  ( -87.13860669537896797, -30.00000000000003908, 184.2824706449898144 ) ) ;
#74005 = VERTEX_POINT ( 'NONE', #91568 ) ;
#74006 = CIRCLE ( 'NONE', #84341, 15.00000000000000711 ) ;
#74007 = CARTESIAN_POINT ( 'NONE',  ( -9.204646778667628482, -55.29777711479709978, 30.90975160907398234 ) ) ;
#74008 = CARTESIAN_POINT ( 'NONE',  ( 43.00000000000000711, 461.4080316921935605, 3.462976341553827719 ) ) ;
#74009 = CARTESIAN_POINT ( 'NONE',  ( 9.439578325719789831, 141.9252321839973092, 8.673617380357923939E-16 ) ) ;
#74010 = DIRECTION ( 'NONE',  ( -0.000000000000000000, -1.000000000000000000, -0.000000000000000000 ) ) ;
#74011 = CARTESIAN_POINT ( 'NONE',  ( 9.948561005166128624, 26.13009726251801723, -1.045755304005140607 ) ) ;
#74012 = CARTESIAN_POINT ( 'NONE',  ( 2.977408999572651815, -25.81250000204838813, 7.188101187500000933 ) ) ;
#74013 = DIRECTION ( 'NONE',  ( -0.000000000000000000, -1.000000000000000000, -0.000000000000000000 ) ) ;
#74014 = CARTESIAN_POINT ( 'NONE',  ( 6.856834870136921722, 41.38254192504039963, -70.56142689300520487 ) ) ;
#74015 = ORIENTED_EDGE ( 'NONE', *, *, #54674, .F. ) ;
#74016 = CIRCLE ( 'NONE', #3432, 60.00000000000000000 ) ;
#74017 = CIRCLE ( 'NONE', #77505, 4.000000000000007105 ) ;
#74019 = ORIENTED_EDGE ( 'NONE', *, *, #30380, .F. ) ;
#74018 = LINE ( 'NONE', #56765, #2962 ) ;
#74020 = CARTESIAN_POINT ( 'NONE',  ( 82.52664522055025031, -32.55557495989385330, 155.0942886860429155 ) ) ;
#74021 = EDGE_CURVE ( 'NONE', #38361, #98861, #94987, .T. ) ;
#74022 = VECTOR ( 'NONE', #37720, 1000.000000000000000 ) ;
#74023 =( NAMED_UNIT ( * ) PLANE_ANGLE_UNIT ( ) SI_UNIT ( $, .RADIAN. ) );
#74024 = CARTESIAN_POINT ( 'NONE',  ( 9.797372177749755551, 88.46509494847563815, 2.014953862275842944 ) ) ;
#74025 = ORIENTED_EDGE ( 'NONE', *, *, #25686, .T. ) ;
#74026 = FILL_AREA_STYLE_COLOUR ( '', #8296 ) ;
#74027 = CARTESIAN_POINT ( 'NONE',  ( 12.79230769230769305, 4.172000000000003261, 0.000000000000000000 ) ) ;
#74028 = CARTESIAN_POINT ( 'NONE',  ( -7.188101187500000933, -11.00000000204838635, -2.977408999572651371 ) ) ;
#74029 = CYLINDRICAL_SURFACE ( 'NONE', #89858, 33.82893434829263413 ) ;
#74030 = CARTESIAN_POINT ( 'NONE',  ( 66.17605003987134182, -60.00000000000000000, -27.79200239227810698 ) ) ;
#74031 = CARTESIAN_POINT ( 'NONE',  ( -33.07276483573667747, 438.9325140356154975, 23.89537236861306013 ) ) ;
#74032 = ADVANCED_FACE ( 'NONE', ( #49490 ), #371, .F. ) ;
#74033 = DIRECTION ( 'NONE',  ( -1.000000000000000000, -1.224606353822377258E-16, -0.000000000000000000 ) ) ;
#74034 = EDGE_LOOP ( 'NONE', ( #32679, #22764, #59522, #89703 ) ) ;
#74035 = CARTESIAN_POINT ( 'NONE',  ( 4.474623633717270010, 142.5192855048741762, 5.000000000000000888 ) ) ;
#74036 = VECTOR ( 'NONE', #59482, 1000.000000000000000 ) ;
#74037 = CARTESIAN_POINT ( 'NONE',  ( 7.416285617647480066, 41.02764994231083762, -59.17152657697691609 ) ) ;
#74038 = FACE_OUTER_BOUND ( 'NONE', #78780, .T. ) ;
#74039 = CARTESIAN_POINT ( 'NONE',  ( -5.082755093536326818, -33.21875000204838813, 5.082755093536325042 ) ) ;
#74040 = CARTESIAN_POINT ( 'NONE',  ( 38.04269904239736633, -36.98679888056368981, 47.30367013139319710 ) ) ;
#74041 = CARTESIAN_POINT ( 'NONE',  ( -39.73996485276600055, 490.7364375727938750, 11.79908848420498302 ) ) ;
#74042 = CARTESIAN_POINT ( 'NONE',  ( 0.5219667817988785652, -7.204195837485550591, -0.5602453477493567480 ) ) ;
#74043 = LINE ( 'NONE', #97787, #52859 ) ;
#74044 = PRODUCT_CONTEXT ( 'NONE', #10721, 'mechanical' ) ;
#74045 = CARTESIAN_POINT ( 'NONE',  ( 48.80467726777884252, 9.660151405757227749, 14.61811727277425987 ) ) ;
#74046 = CARTESIAN_POINT ( 'NONE',  ( -36.59842210978563060, 438.2481675559515111, 3.880703544898892687 ) ) ;
#74047 = DIRECTION ( 'NONE',  ( -1.000000000000000000, -0.000000000000000000, -0.000000000000000000 ) ) ;
#74048 = SURFACE_STYLE_FILL_AREA ( #25004 ) ;
#74049 = CARTESIAN_POINT ( 'NONE',  ( 14.33580413386840213, 42.00000000000000000, -89.41414995614803729 ) ) ;
#74050 = AXIS2_PLACEMENT_3D ( 'NONE', #46266, #61940, #70543 ) ;
#74051 = EDGE_LOOP ( 'NONE', ( #16036, #65659, #3894, #101344 ) ) ;
#74052 = CARTESIAN_POINT ( 'NONE',  ( 114.0943401353945603, -57.67137920739276780, 166.6188124564318116 ) ) ;
#74053 = MECHANICAL_DESIGN_GEOMETRIC_PRESENTATION_REPRESENTATION (  '', ( #25849 ), #25933 ) ;
#74054 = CARTESIAN_POINT ( 'NONE',  ( 35.35823899438943840, 463.7178658455732148, 19.28807933140813446 ) ) ;
#74055 = CARTESIAN_POINT ( 'NONE',  ( 1.314337315968152620, 14.06570418733889483, 6.879968599000877205 ) ) ;
#74056 = DIRECTION ( 'NONE',  ( 0.000000000000000000, 0.000000000000000000, 1.000000000000000000 ) ) ;
#74057 = CARTESIAN_POINT ( 'NONE',  ( 36.44116660230073990, 26.07456738169941701, 11.65597035723753372 ) ) ;
#74058 = CARTESIAN_POINT ( 'NONE',  ( -76.89441695137394106, -59.99999999999999289, 190.1397586532095545 ) ) ;
#74059 = CARTESIAN_POINT ( 'NONE',  ( 1.381740507186689448E-16, 7.550813340387661832, -6.286444963328676749 ) ) ;
#74060 = CARTESIAN_POINT ( 'NONE',  ( -40.17205142263708240, 310.2804317922712016, -6.358608209523628929 ) ) ;
#74061 = CARTESIAN_POINT ( 'NONE',  ( -84.82604425270216097, -46.57314820510289621, 187.1285925919904116 ) ) ;
#74062 = ORIENTED_EDGE ( 'NONE', *, *, #68911, .F. ) ;
#74063 = CARTESIAN_POINT ( 'NONE',  ( 20.96800765626202789, 304.9222235596747623, -9.985031600492462189 ) ) ;
#74064 = VECTOR ( 'NONE', #81412, 1000.000000000000114 ) ;
#74065 = EDGE_CURVE ( 'NONE', #31075, #24250, #55362, .T. ) ;
#74066 = AXIS2_PLACEMENT_3D ( 'NONE', #19134, #43888, #2883 ) ;
#74067 = VERTEX_POINT ( 'NONE', #85064 ) ;
#74068 = CARTESIAN_POINT ( 'NONE',  ( -7.045965687440315151, -11.30392463786035684, 3.790395326974319801 ) ) ;
#74069 = ADVANCED_FACE ( 'NONE', ( #19841 ), #41600, .T. ) ;
#74070 = CARTESIAN_POINT ( 'NONE',  ( -6.195804093982627769, 41.59435685013754380, -70.65487364512668478 ) ) ;
#74071 = CARTESIAN_POINT ( 'NONE',  ( -85.75027484506800590, -52.74039826046678314, -7.195638168032203907 ) ) ;
#74072 = CIRCLE ( 'NONE', #65469, 7.000000000000011546 ) ;
#74073 = CARTESIAN_POINT ( 'NONE',  ( -43.43869229197127169, 464.9661605157749591, 13.42065392471462815 ) ) ;
#74074 = CARTESIAN_POINT ( 'NONE',  ( 43.02621584241283870, 434.6128289108255558, 16.97888786058996402 ) ) ;
#74075 = ORIENTED_EDGE ( 'NONE', *, *, #73922, .T. ) ;
#74076 = DIRECTION ( 'NONE',  ( 0.000000000000000000, 0.000000000000000000, -1.000000000000000000 ) ) ;
#74077 = EDGE_CURVE ( 'NONE', #85895, #3882, #85608, .T. ) ;
#74078 = CARTESIAN_POINT ( 'NONE',  ( 6.464976090918999496, 41.32133059754584536, -58.37832579531859523 ) ) ;
#74079 = CARTESIAN_POINT ( 'NONE',  ( -4.453875240779026079, -1.734723475976807094E-15, 16.57301948836938621 ) ) ;
#74080 = CARTESIAN_POINT ( 'NONE',  ( -36.22735294587202759, 437.9860357368660289, 4.211724321152335193 ) ) ;
#74081 = AXIS2_PLACEMENT_3D ( 'NONE', #102013, #18471, #61048 ) ;
#74082 = CARTESIAN_POINT ( 'NONE',  ( -2.851760031137707596, -60.00000000000000000, -45.00000000000002132 ) ) ;
#74083 = CARTESIAN_POINT ( 'NONE',  ( -77.85220176464979147, -42.96760201762617015, 136.7854011922409256 ) ) ;
#74084 = VERTEX_POINT ( 'NONE', #94767 ) ;
#74085 = CARTESIAN_POINT ( 'NONE',  ( 76.30472591814422856, -30.00000000000007105, 168.5677193688796649 ) ) ;
#74086 = CARTESIAN_POINT ( 'NONE',  ( 16.36650669486618881, 4.000000000000003553, 4.898587196589414801E-16 ) ) ;
#74087 = CARTESIAN_POINT ( 'NONE',  ( 106.5469097212175171, -57.67120316527606150, 107.4300699905816714 ) ) ;
#74088 = VERTEX_POINT ( 'NONE', #38140 ) ;
#74089 = CARTESIAN_POINT ( 'NONE',  ( 28.18166793234509981, 34.32241243842408807, 8.150798923637601945 ) ) ;
#74090 = CIRCLE ( 'NONE', #27656, 4.000000000000001776 ) ;
#74091 = DIRECTION ( 'NONE',  ( 0.000000000000000000, -1.000000000000000000, 0.000000000000000000 ) ) ;
#74092 = ORIENTED_EDGE ( 'NONE', *, *, #43450, .T. ) ;
#74093 = CARTESIAN_POINT ( 'NONE',  ( 3.173243715879570548, 15.40382952331938782, -6.241576743951559259 ) ) ;
#74094 = DIRECTION ( 'NONE',  ( -1.000000000000000000, -0.000000000000000000, -0.000000000000000000 ) ) ;
#74095 = CARTESIAN_POINT ( 'NONE',  ( -1.320432766682874540E-15, -21.03125000204838457, 7.188101187500000044 ) ) ;
#74096 = CARTESIAN_POINT ( 'NONE',  ( 2.558993250141107456, -7.638875775591494666, -7.593821156097297020 ) ) ;
#74097 = DIRECTION ( 'NONE',  ( -0.5735764363510497121, 0.8191520442889892450, 1.003171929053521665E-16 ) ) ;
#74098 = CARTESIAN_POINT ( 'NONE',  ( -7.922798540899431252, 4.627424769998830456, -8.057412477672047046 ) ) ;
#74099 = CARTESIAN_POINT ( 'NONE',  ( 14.85284876471456350, 1.482358050883964840E-15, 0.000000000000000000 ) ) ;
#74100 = ORIENTED_EDGE ( 'NONE', *, *, #78457, .F. ) ;
#74101 = CARTESIAN_POINT ( 'NONE',  ( -7.321076910647204450, 40.29402652806530227, -70.66289162821402670 ) ) ;
#74103 = CARTESIAN_POINT ( 'NONE',  ( 28.71054976466791331, -42.95721924763428490, 33.31278848725109043 ) ) ;
#74102 = CARTESIAN_POINT ( 'NONE',  ( -3.883877898720302202, -48.93467900693696038, 104.5781496044265282 ) ) ;
#74104 = CIRCLE ( 'NONE', #27670, 7.000000000000000000 ) ;
#74105 = CARTESIAN_POINT ( 'NONE',  ( -4.959638304640701101, 51.41909874265953562, -8.497456494351391498 ) ) ;
#74106 = ORIENTED_EDGE ( 'NONE', *, *, #86587, .T. ) ;
#74107 = CARTESIAN_POINT ( 'NONE',  ( -0.1552019576139205825, 18.85513881606577158, 49.25764478663058554 ) ) ;
#74108 = EDGE_CURVE ( 'NONE', #21702, #105760, #95055, .T. ) ;
#74109 = UNCERTAINTY_MEASURE_WITH_UNIT (LENGTH_MEASURE( 1.000000000000000082E-05 ), #35582, 'distance_accuracy_value', 'NONE');
#74110 = EDGE_LOOP ( 'NONE', ( #81903, #102783, #13897, #92769 ) ) ;
#74112 = CARTESIAN_POINT ( 'NONE',  ( 36.69990213913942512, 461.9654235716706694, 3.159576000644405358 ) ) ;
#74111 = CARTESIAN_POINT ( 'NONE',  ( 0.1317522424410006998, 1.959574484677833794, 7.999999999999998224 ) ) ;
#74113 = CARTESIAN_POINT ( 'NONE',  ( 0.000000000000000000, 0.000000000000000000, 0.000000000000000000 ) ) ;
#74114 = DIRECTION ( 'NONE',  ( 0.000000000000000000, 1.000000000000000000, 0.000000000000000000 ) ) ;
#74115 = FACE_OUTER_BOUND ( 'NONE', #87084, .T. ) ;
#74116 = CARTESIAN_POINT ( 'NONE',  ( 32.33349330513380693, -4.000000000000000000, 4.898587196589415787E-16 ) ) ;
#74117 = DIRECTION ( 'NONE',  ( 0.000000000000000000, 0.000000000000000000, 1.000000000000000000 ) ) ;
#74118 = ORIENTED_EDGE ( 'NONE', *, *, #10077, .F. ) ;
#74119 = CARTESIAN_POINT ( 'NONE',  ( 91.72933629761578800, -60.00000000000000000, -14.91791294062407758 ) ) ;
#74120 = CARTESIAN_POINT ( 'NONE',  ( -9.076853247125740154, 45.89842957983099581, 14.51167170299874520 ) ) ;
#74121 = CARTESIAN_POINT ( 'NONE',  ( 30.00000000000155964, 464.1855333580207343, 13.92840612649013110 ) ) ;
#74122 =( LENGTH_UNIT ( ) NAMED_UNIT ( * ) SI_UNIT ( .MILLI., .METRE. ) );
#74123 =( BOUNDED_CURVE ( )  B_SPLINE_CURVE ( 2, ( #75823, #58590, #1919 ),
 .UNSPECIFIED., .F., .F. ) 
 B_SPLINE_CURVE_WITH_KNOTS ( ( 3, 3 ),
 ( 0.000000000000000000, 1.000000000000000000 ),
 .UNSPECIFIED. ) 
 CURVE ( )  GEOMETRIC_REPRESENTATION_ITEM ( )  RATIONAL_B_SPLINE_CURVE ( ( 1.000000000000000000, 1.857142857142858317, 1.000000000000000000 ) ) 
 REPRESENTATION_ITEM ( '' )  );
#74124 = CARTESIAN_POINT ( 'NONE',  ( -17.49999999999999645, 2.500000000000000444, 25.00000000000000000 ) ) ;
#74125 = EDGE_CURVE ( 'NONE', #60867, #63010, #104306, .T. ) ;
#74126 = ORIENTED_EDGE ( 'NONE', *, *, #62711, .T. ) ;
#74127 = ADVANCED_FACE ( 'NONE', ( #87194 ), #31323, .T. ) ;
#74128 = AXIS2_PLACEMENT_3D ( 'NONE', #43485, #19265, #67756 ) ;
#74129 = DIRECTION ( 'NONE',  ( -1.000000000000000000, -1.224606353822377258E-16, -0.000000000000000000 ) ) ;
#74130 = ORIENTED_EDGE ( 'NONE', *, *, #20778, .F. ) ;
#74131 = ORIENTED_EDGE ( 'NONE', *, *, #38130, .F. ) ;
#74132 = CARTESIAN_POINT ( 'NONE',  ( 0.9999999999999940048, 0.000000000000000000, 101.0455488498966758 ) ) ;
#74133 = CARTESIAN_POINT ( 'NONE',  ( -37.56673239365971284, 27.88554838446211548, -10.95617127780556466 ) ) ;
#74134 = CARTESIAN_POINT ( 'NONE',  ( 19.96162532426522773, 302.8116070918645164, 9.928455558879880627 ) ) ;
#74135 = CARTESIAN_POINT ( 'NONE',  ( 85.70657369333201814, -52.73561151911660971, -4.539914901182836360 ) ) ;
#74136 = CARTESIAN_POINT ( 'NONE',  ( -37.00818793297098352, 345.1386355367852730, 0.03061739860943737609 ) ) ;
#74137 = CARTESIAN_POINT ( 'NONE',  ( -4.568199989557032659, -65.71137023209668371, 13.11834388973587728 ) ) ;
#74138 = DIRECTION ( 'NONE',  ( -0.000000000000000000, -0.000000000000000000, -1.000000000000000000 ) ) ;
#74139 = ORIENTED_EDGE ( 'NONE', *, *, #6506, .T. ) ;
#74140 = CARTESIAN_POINT ( 'NONE',  ( -9.184438934625386963, 44.03862627902407922, 13.56153005510785725 ) ) ;
#74141 = ORIENTED_EDGE ( 'NONE', *, *, #9619, .F. ) ;
#74142 = CARTESIAN_POINT ( 'NONE',  ( 11.84999999999999787, -3.309499999999999886, 4.475777889183790779E-16 ) ) ;
#74143 = DIRECTION ( 'NONE',  ( 0.000000000000000000, 1.000000000000000000, 0.000000000000000000 ) ) ;
#74144 = CARTESIAN_POINT ( 'NONE',  ( 39.99565418590076860, 463.9333411592453444, 18.76875386499541776 ) ) ;
#74145 = AXIS2_PLACEMENT_3D ( 'NONE', #63075, #46358, #103527 ) ;
#74147 = ORIENTED_EDGE ( 'NONE', *, *, #31336, .F. ) ;
#74146 = CARTESIAN_POINT ( 'NONE',  ( -49.24092377949861543, -59.99999999999996447, 56.22341034505959811 ) ) ;
#74148 = CARTESIAN_POINT ( 'NONE',  ( 63.81336088806118312, -53.38611597571917855, 89.97107311934965423 ) ) ;
#74149 = EDGE_CURVE ( 'NONE', #84262, #87039, #20386, .T. ) ;
#74150 = VERTEX_POINT ( 'NONE', #46199 ) ;
#74151 = SURFACE_STYLE_FILL_AREA ( #91428 ) ;
#74152 = DIRECTION ( 'NONE',  ( -1.000000000000000000, -1.224606353822377258E-16, -0.000000000000000000 ) ) ;
#74153 = CARTESIAN_POINT ( 'NONE',  ( -77.41886385744251697, -57.67119865640713527, -31.55546021046578531 ) ) ;
#74154 = ADVANCED_FACE ( 'NONE', ( #4147 ), #17433, .F. ) ;
#74155 = ORIENTED_EDGE ( 'NONE', *, *, #47662, .T. ) ;
#74156 = SURFACE_SIDE_STYLE ('',( #81703 ) ) ;
#74157 = CARTESIAN_POINT ( 'NONE',  ( 10.28624191511840458, 43.99263840937192782, 12.90779740156148847 ) ) ;
#74158 = EDGE_CURVE ( 'NONE', #84731, #38550, #44616, .T. ) ;
#74159 = CARTESIAN_POINT ( 'NONE',  ( -35.43142158410745424, 491.1302584546127150, 12.10548931029582853 ) ) ;
#74160 = MECHANICAL_DESIGN_GEOMETRIC_PRESENTATION_REPRESENTATION (  '', ( #79332 ), #75940 ) ;
#74161 = B_SPLINE_CURVE_WITH_KNOTS ( 'NONE', 3,
 ( #29509, #37603, #47223, #38128, #69932, #21404, #102832, #86137, #54241, #45140 ),
 .UNSPECIFIED., .F., .F.,
 ( 4, 2, 2, 2, 4 ),
 ( 0.000000000000000000, 0.001637141140915473027, 0.003274282281830946054, 0.004911423422746419298, 0.006548564563661892109 ),
 .UNSPECIFIED. ) ;
#74162 = CARTESIAN_POINT ( 'NONE',  ( 7.042157147547021781E-15, 43.34115912517999902, -57.50357696970298349 ) ) ;
#74163 = CARTESIAN_POINT ( 'NONE',  ( 4.898587196589412829E-16, -21.31250000409676915, -8.000000000000000000 ) ) ;
#74164 = ADVANCED_FACE ( 'NONE', ( #53229 ), #51109, .T. ) ;
#74165 = CARTESIAN_POINT ( 'NONE',  ( -7.137815226409941260, -3.000000000000000000, 4.175893272574811910 ) ) ;
#74166 = DIRECTION ( 'NONE',  ( -1.000000000000000000, -1.224606353822377258E-16, -0.000000000000000000 ) ) ;
#74167 = DIRECTION ( 'NONE',  ( -1.000000000000000000, -0.000000000000000000, -0.000000000000000000 ) ) ;
#74168 = CARTESIAN_POINT ( 'NONE',  ( -5.899761283606826723, 4.638522211504596093, 5.000000000000000000 ) ) ;
#74169 = DIRECTION ( 'NONE',  ( -0.5735764363510459374, -0.8191520442889919096, 0.000000000000000000 ) ) ;
#74170 = CARTESIAN_POINT ( 'NONE',  ( -0.7768758660234609259, 15.00000000000000000, -9.999999999999998224 ) ) ;
#74171 = EDGE_LOOP ( 'NONE', ( #72135, #60209, #106377, #48258, #89127, #70525 ) ) ;
#74172 = PRESENTATION_STYLE_ASSIGNMENT (( #37086 ) ) ;
#74173 = CARTESIAN_POINT ( 'NONE',  ( 42.33349330513380693, 1.593028355512270567E-15, 0.000000000000000000 ) ) ;
#74174 = CARTESIAN_POINT ( 'NONE',  ( 4.289501753560038821, -60.00000000000000000, 39.63072196994962582 ) ) ;
#74175 = CARTESIAN_POINT ( 'NONE',  ( -94.42958044472295853, -29.99999999999999645, 191.3151220890198374 ) ) ;
#74176 = CARTESIAN_POINT ( 'NONE',  ( 34.83349330513380693, -4.000000000000000000, 4.898587196589415787E-16 ) ) ;
#74177 = CARTESIAN_POINT ( 'NONE',  ( 70.41099422567990018, -57.68249184797887352, 157.3713819725495853 ) ) ;
#74179 = CARTESIAN_POINT ( 'NONE',  ( -8.559508646656370345, 53.68473964988125857, 4.031152949374564365 ) ) ;
#74178 = CARTESIAN_POINT ( 'NONE',  ( -0.1694831974862292256, 26.07487419649228855, -38.25868201985088035 ) ) ;
#74180 = CARTESIAN_POINT ( 'NONE',  ( 14.50404474426535906, -23.92104523642918679, -38.53261106116733714 ) ) ;
#74181 = AXIS2_PLACEMENT_3D ( 'NONE', #6883, #5821, #72678 ) ;
#74182 = CARTESIAN_POINT ( 'NONE',  ( 5.007715329123895321E-16, -7.505553499465175804, -6.064240316920414209 ) ) ;
#74183 = DIRECTION ( 'NONE',  ( -1.000000000000000000, -1.224606353822377258E-16, -0.000000000000000000 ) ) ;
#74184 = CARTESIAN_POINT ( 'NONE',  ( -12.69242650814801365, -59.99999999999999289, 39.70541446682850761 ) ) ;
#74185 =( REPRESENTATION_RELATIONSHIP ('NONE','NONE', #69581, #22667 ) REPRESENTATION_RELATIONSHIP_WITH_TRANSFORMATION ( #42211 )SHAPE_REPRESENTATION_RELATIONSHIP( ) );
#74186 = CARTESIAN_POINT ( 'NONE',  ( -0.2996719224662260928, -70.51541691410464807, 12.99134206341307163 ) ) ;
#74187 = CARTESIAN_POINT ( 'NONE',  ( 0.8408997231841593978, 45.41398511527192738, -18.42850300921338658 ) ) ;
#74188 = CARTESIAN_POINT ( 'NONE',  ( -85.88719281955947338, -61.05569566503563550, 194.2292230513385505 ) ) ;
#74189 = VERTEX_POINT ( 'NONE', #74689 ) ;
#74190 = CARTESIAN_POINT ( 'NONE',  ( 19.42937650476797629, 49.96296734528399242, 60.82359239913252225 ) ) ;
#74191 = CARTESIAN_POINT ( 'NONE',  ( 29.77292113577873423, 13.34857726707554448, 42.10535821593450834 ) ) ;
#74192 = CARTESIAN_POINT ( 'NONE',  ( -9.185217898028438910, -35.99447867802918921, 29.89084909448629190 ) ) ;
#74193 = CARTESIAN_POINT ( 'NONE',  ( 16.00000000000008882, 2.437231117875652053, -5.694551215225447827 ) ) ;
#74194 = CARTESIAN_POINT ( 'NONE',  ( 3.959695725110176756, -69.40440198710396658, 13.56584679134417293 ) ) ;
#74195 = EDGE_CURVE ( 'NONE', #42925, #31421, #7175, .T. ) ;
#74196 = EDGE_LOOP ( 'NONE', ( #52605, #32844, #31017, #4705, #24744, #68840 ) ) ;
#74197 = AXIS2_PLACEMENT_3D ( 'NONE', #93772, #75982, #44160 ) ;
#74198 = DIRECTION ( 'NONE',  ( -0.000000000000000000, -0.000000000000000000, 1.000000000000000000 ) ) ;
#74199 = B_SPLINE_CURVE_WITH_KNOTS ( 'NONE', 3,
 ( #93205, #52201, #83504, #74867, #67345, #34478, #67865, #9606 ),
 .UNSPECIFIED., .F., .F.,
 ( 4, 2, 2, 4 ),
 ( 0.02179091314793462145, 0.02376333058066962614, 0.02573574801340463430, 0.02968058287887464369 ),
 .UNSPECIFIED. ) ;
#74200 = CARTESIAN_POINT ( 'NONE',  ( -7.014891834166682827, -4.207085196961300788, -17.12005312235260845 ) ) ;
#74201 = CARTESIAN_POINT ( 'NONE',  ( -6.943926999490791729, 30.53300992626148158, -3.973092371898545139 ) ) ;
#74202 = CARTESIAN_POINT ( 'NONE',  ( 26.64323232996463631, 304.7933454163547253, -9.574263947122538809 ) ) ;
#74203 = EDGE_CURVE ( 'NONE', #106458, #58764, #89874, .T. ) ;
#74204 = DIRECTION ( 'NONE',  ( 0.000000000000000000, 1.000000000000000000, 0.000000000000000000 ) ) ;
#74205 = CARTESIAN_POINT ( 'NONE',  ( -6.944031699373470090, -84.46539345443872548, 3.972913591453824278 ) ) ;
#74206 = DIRECTION ( 'NONE',  ( -1.000000000000000000, -1.224606353822377258E-16, -0.000000000000000000 ) ) ;
#74207 = CARTESIAN_POINT ( 'NONE',  ( 106.1778528577414704, -14.21045842199435150, 156.9945530843897075 ) ) ;
#74208 = CARTESIAN_POINT ( 'NONE',  ( -35.44563196690202744, 355.0508310518326311, 1.542887188894044526 ) ) ;
#74209 = ORIENTED_EDGE ( 'NONE', *, *, #58751, .T. ) ;
#74210 = CARTESIAN_POINT ( 'NONE',  ( 44.11331465659122131, 485.7406967462466696, 4.043683577888340430 ) ) ;
#74211 = CARTESIAN_POINT ( 'NONE',  ( -9.165151389911699198, 249.9999999999999432, 4.000000000000002665 ) ) ;
#74212 = DIRECTION ( 'NONE',  ( 0.000000000000000000, 1.000000000000000000, 0.000000000000000000 ) ) ;
#74213 = CARTESIAN_POINT ( 'NONE',  ( -1.306442393143578240, -8.377108146505396036, -7.792327460285862983 ) ) ;
#74214 = CARTESIAN_POINT ( 'NONE',  ( -42.31104777394613592, 465.8656652864358421, 14.28483731023798065 ) ) ;
#74215 = DIRECTION ( 'NONE',  ( 1.000000000000000000, 0.000000000000000000, 0.000000000000000000 ) ) ;
#74216 = VERTEX_POINT ( 'NONE', #57438 ) ;
#74217 = UNCERTAINTY_MEASURE_WITH_UNIT (LENGTH_MEASURE( 1.000000000000000082E-05 ), #106532, 'distance_accuracy_value', 'NONE');
#74218 = AXIS2_PLACEMENT_3D ( 'NONE', #91333, #49787, #17448 ) ;
#74219 = CIRCLE ( 'NONE', #82855, 5.000000000000011546 ) ;
#74220 = CARTESIAN_POINT ( 'NONE',  ( 32.04230769230768772, 1.411358822780289120E-15, 0.000000000000000000 ) ) ;
#74221 = ORIENTED_EDGE ( 'NONE', *, *, #50537, .F. ) ;
#74222 = CARTESIAN_POINT ( 'NONE',  ( 0.000000000000000000, 0.000000000000000000, -6.499999999999999112 ) ) ;
#74223 = AXIS2_PLACEMENT_3D ( 'NONE', #32116, #87699, #30008 ) ;
#74224 = CARTESIAN_POINT ( 'NONE',  ( 9.960122430517651893, 45.46309208840076366, 15.36726729605906527 ) ) ;
#74225 = ORIENTED_EDGE ( 'NONE', *, *, #83053, .F. ) ;
#74226 = EDGE_CURVE ( 'NONE', #104720, #70219, #21028, .T. ) ;
#74227 = CARTESIAN_POINT ( 'NONE',  ( 11.91432047182400211, 48.00000000000000000, 64.17585289259234571 ) ) ;
#74228 = CARTESIAN_POINT ( 'NONE',  ( 5.000000000000039968, -12.89614509141023291, 12.11365041472630644 ) ) ;
#74229 = CARTESIAN_POINT ( 'NONE',  ( -72.13545514535530856, -59.99999999997070432, 177.2956874472480990 ) ) ;
#74230 = AXIS2_PLACEMENT_3D ( 'NONE', #16096, #48977, #24750 ) ;
#74231 = DIRECTION ( 'NONE',  ( -0.000000000000000000, 0.000000000000000000, -1.000000000000000000 ) ) ;
#74232 = VERTEX_POINT ( 'NONE', #83324 ) ;
#74233 = CARTESIAN_POINT ( 'NONE',  ( 110.6907876672333657, -60.00000000000001421, 188.6866862957170667 ) ) ;
#74234 = TOROIDAL_SURFACE ( 'NONE', #7029, 12.00000000000000000, 2.000000000000000000 ) ;
#74236 = CARTESIAN_POINT ( 'NONE',  ( 19.48570689116957411, -60.35677515645173941, 34.43380376002015453 ) ) ;
#74235 = CARTESIAN_POINT ( 'NONE',  ( -109.5128114756446109, -29.99999999999999289, 168.1048973186342437 ) ) ;
#74237 = CARTESIAN_POINT ( 'NONE',  ( 38.26404824536036386, 461.1055978787671847, 2.389911169387158196 ) ) ;
#74238 = CARTESIAN_POINT ( 'NONE',  ( 0.4147425415936616955, 54.27900644350521020, -7.817881304308153645 ) ) ;
#74239 = CARTESIAN_POINT ( 'NONE',  ( -43.56207904828443844, -60.25507094030576383, 47.28631016918702556 ) ) ;
#74240 = PRESENTATION_LAYER_ASSIGNMENT (  '', '', ( #103585 ) ) ;
#74241 = EDGE_CURVE ( 'NONE', #31918, #82092, #96690, .T. ) ;
#74242 = CARTESIAN_POINT ( 'NONE',  ( -38.12216208879733870, 18.64284798593187631, -4.860317469385954325 ) ) ;
#74243 = EDGE_LOOP ( 'NONE', ( #88950, #100219, #81353, #57964 ) ) ;
#74244 = DIRECTION ( 'NONE',  ( -0.000000000000000000, -1.000000000000000000, -0.000000000000000000 ) ) ;
#74245 = CARTESIAN_POINT ( 'NONE',  ( 16.14595037822613932, 20.23371447307438586, 4.922994507617745263 ) ) ;
#74246 = CARTESIAN_POINT ( 'NONE',  ( 40.95420997525301487, 387.0967036739339164, 27.26945002580065136 ) ) ;
#74247 = FILL_AREA_STYLE ('',( #66158 ) ) ;
#74248 = CARTESIAN_POINT ( 'NONE',  ( -5.656854249492381470, -28.25000000409677270, 5.656854249492379694 ) ) ;
#74249 = CARTESIAN_POINT ( 'NONE',  ( -38.51502786940007184, 460.0233756673457606, 2.043034587342192676 ) ) ;
#74250 = ORIENTED_EDGE ( 'NONE', *, *, #97134, .T. ) ;
#74251 = CARTESIAN_POINT ( 'NONE',  ( 4.928386788250681327, -48.42812442315226207, 104.2441249819462712 ) ) ;
#74252 = ORIENTED_EDGE ( 'NONE', *, *, #19350, .F. ) ;
#74253 = CARTESIAN_POINT ( 'NONE',  ( 48.93247286101075844, -30.00000000006591350, 62.56579767259364644 ) ) ;
#74254 = CARTESIAN_POINT ( 'NONE',  ( 47.90305809253377589, 10.05329658600983400, 16.85535821593427386 ) ) ;
#74255 = DIRECTION ( 'NONE',  ( 0.000000000000000000, -1.000000000000000000, 0.000000000000000000 ) ) ;
#74256 = CARTESIAN_POINT ( 'NONE',  ( -3.400000000000000355, 4.163799117101001052E-16, -8.000000000000000000 ) ) ;
#74257 = CARTESIAN_POINT ( 'NONE',  ( 90.42596699330265153, -30.00000000000000000, 90.98457831099128157 ) ) ;
#74258 = CARTESIAN_POINT ( 'NONE',  ( 6.943926999490790841, 104.4669900737385291, -3.973092371898547803 ) ) ;
#74259 = EDGE_CURVE ( 'NONE', #8093, #58207, #772, .T. ) ;
#74260 = ORIENTED_EDGE ( 'NONE', *, *, #78370, .F. ) ;
#74261 = EDGE_CURVE ( 'NONE', #46619, #1725, #82542, .T. ) ;
#74262 = EDGE_LOOP ( 'NONE', ( #100085, #1920 ) ) ;
#74263 = ORIENTED_EDGE ( 'NONE', *, *, #23247, .T. ) ;
#74264 = CARTESIAN_POINT ( 'NONE',  ( 54.52222222222221859, 6.915964383211875250E-15, 0.000000000000000000 ) ) ;
#74265 = CARTESIAN_POINT ( 'NONE',  ( -4.277293724315427426, -9.465728641413040378, -11.68612602563391079 ) ) ;
#74266 = AXIS2_PLACEMENT_3D ( 'NONE', #72511, #37540, #47166 ) ;
#74267 = CARTESIAN_POINT ( 'NONE',  ( -41.59749957395938225, 465.5821881718248392, 15.80727685357802947 ) ) ;
#74268 = CARTESIAN_POINT ( 'NONE',  ( -31.42024686275397727, 416.1372461024106428, 24.31832120901086469 ) ) ;
#74269 = DIRECTION ( 'NONE',  ( -1.000000000000000000, -1.224606353822377258E-16, -0.000000000000000000 ) ) ;
#74270 = ORIENTED_EDGE ( 'NONE', *, *, #35028, .F. ) ;
#74271 = CARTESIAN_POINT ( 'NONE',  ( 9.989690267985800176, 108.9744441659491088, -0.5238310916885804414 ) ) ;
#74272 = AXIS2_PLACEMENT_3D ( 'NONE', #55817, #39685, #55304 ) ;
#74273 = VERTEX_POINT ( 'NONE', #100570 ) ;
#74274 = DIRECTION ( 'NONE',  ( 0.000000000000000000, 0.000000000000000000, 1.000000000000000000 ) ) ;
#74275 = CARTESIAN_POINT ( 'NONE',  ( 78.81272654805164279, -38.66995965544662539, 190.4856035335980664 ) ) ;
#74276 = DIRECTION ( 'NONE',  ( 0.000000000000000000, 0.000000000000000000, 1.000000000000000000 ) ) ;
#74277 = CARTESIAN_POINT ( 'NONE',  ( 24.72051274681640010, 304.3800740200679797, 10.27342727648563603 ) ) ;
#74278 = DIRECTION ( 'NONE',  ( -0.000000000000000000, -1.000000000000000000, -0.000000000000000000 ) ) ;
#74279 = CARTESIAN_POINT ( 'NONE',  ( 14.29190075645216851, 12.99999999999999289, 0.000000000000000000 ) ) ;
#74280 = CARTESIAN_POINT ( 'NONE',  ( -28.35805569942980497, 34.17680034679604262, -8.950141237612221801 ) ) ;
#74281 = CARTESIAN_POINT ( 'NONE',  ( 59.89460441624491693, 6.975173280561618775E-15, 0.000000000000000000 ) ) ;
#74282 = EDGE_CURVE ( 'NONE', #80083, #95018, #99499, .T. ) ;
#74283 = FILL_AREA_STYLE_COLOUR ( '', #69507 ) ;
#74284 = ORIENTED_EDGE ( 'NONE', *, *, #92312, .T. ) ;
#74286 = CARTESIAN_POINT ( 'NONE',  ( -22.02746468779565348, 303.1977850725832582, 10.01134046771178099 ) ) ;
#74285 = LINE ( 'NONE', #40332, #95150 ) ;
#74287 =( NAMED_UNIT ( * ) SI_UNIT ( $, .STERADIAN. ) SOLID_ANGLE_UNIT ( ) );
#74288 = UNCERTAINTY_MEASURE_WITH_UNIT (LENGTH_MEASURE( 1.000000000000000082E-05 ), #25168, 'distance_accuracy_value', 'NONE');
#74289 = DIRECTION ( 'NONE',  ( 0.000000000000000000, 0.000000000000000000, 1.000000000000000000 ) ) ;
#74290 = DIRECTION ( 'NONE',  ( -1.000000000000000000, -0.000000000000000000, -0.000000000000000000 ) ) ;
#74291 = CARTESIAN_POINT ( 'NONE',  ( 60.14984002819952025, 6.856755485862130937E-15, 0.000000000000000000 ) ) ;
#74292 = SHAPE_REPRESENTATION ( 'hex nut high strength_din_Hexagon Nut DIN 6915 - M16 - S', ( #10728 ), #83338 ) ;
#74293 = EDGE_CURVE ( 'NONE', #4337, #2494, #9968, .T. ) ;
#74294 = CARTESIAN_POINT ( 'NONE',  ( 8.577352724654989657, 295.3685542829744008, 5.149687988174879827 ) ) ;
#74295 = CARTESIAN_POINT ( 'NONE',  ( 85.74559076837111604, -39.25363284317074175, 186.2120581904971175 ) ) ;
#74296 = CARTESIAN_POINT ( 'NONE',  ( 0.000000000000000000, 0.000000000000000000, 5.000000000000000000 ) ) ;
#74297 = DIRECTION ( 'NONE',  ( -1.000000000000000000, -0.000000000000000000, -0.000000000000000000 ) ) ;
#74298 = EDGE_LOOP ( 'NONE', ( #28106, #86923, #83943, #103651 ) ) ;
#74299 = CARTESIAN_POINT ( 'NONE',  ( 91.47088685542546216, -57.66242603154207558, -20.20556468422682883 ) ) ;
#74300 = EDGE_CURVE ( 'NONE', #32770, #2944, #84719, .T. ) ;
#74301 = CYLINDRICAL_SURFACE ( 'NONE', #67694, 15.00000000000000000 ) ;
#74302 = DIRECTION ( 'NONE',  ( -1.000000000000000000, -0.000000000000000000, -0.000000000000000000 ) ) ;
#74303 = CARTESIAN_POINT ( 'NONE',  ( 0.000000000000000000, 79.50000000000000000, 0.000000000000000000 ) ) ;
#74304 = COLOUR_RGB ( '', 0.66274510, 0.83137255, 0.94901961) ;
#74305 = CARTESIAN_POINT ( 'NONE',  ( -81.41118343893772646, -30.00000000000000000, -9.978428732768641396 ) ) ;
#74306 = CARTESIAN_POINT ( 'NONE',  ( 28.43253669899775815, 17.35855320307317129, 40.99008157358971971 ) ) ;
#74307 = CIRCLE ( 'NONE', #58790, 5.000000000000001776 ) ;
#74308 = CARTESIAN_POINT ( 'NONE',  ( 0.000000000000000000, 6.123233995736767268E-16, -5.000000000000000888 ) ) ;
#74309 = DIRECTION ( 'NONE',  ( -0.000000000000000000, 0.000000000000000000, -1.000000000000000000 ) ) ;
#74311 = SURFACE_STYLE_USAGE ( .BOTH. , #9569 ) ;
#74310 = CARTESIAN_POINT ( 'NONE',  ( 0.000000000000000000, 0.000000000000000000, 60.00000000000000000 ) ) ;
#74312 = AXIS2_PLACEMENT_3D ( 'NONE', #45149, #12749, #28451 ) ;
#74313 = CARTESIAN_POINT ( 'NONE',  ( -17.49999999999997513, 49.62432460127385525, 63.94669766439164960 ) ) ;
#74314 = CARTESIAN_POINT ( 'NONE',  ( -28.58254312158966570, 16.23466659877849949, 41.45958612840279045 ) ) ;
#74315 = CARTESIAN_POINT ( 'NONE',  ( -12.50000000000000711, -4.999999999999999112, -78.42624373368740009 ) ) ;
#74316 = FACE_OUTER_BOUND ( 'NONE', #93284, .T. ) ;
#74317 = CARTESIAN_POINT ( 'NONE',  ( -68.37927364716395573, -37.97112778231701213, -23.07505795230966683 ) ) ;
#74318 = CARTESIAN_POINT ( 'NONE',  ( 104.0908829527487711, 6.123233995736568081E-16, -5.000000000000011546 ) ) ;
#74319 = CARTESIAN_POINT ( 'NONE',  ( 5.000000000000000000, -15.93202192939576634, -5.930487099830193287 ) ) ;
#74320 = ORIENTED_EDGE ( 'NONE', *, *, #32460, .T. ) ;
#74321 = CARTESIAN_POINT ( 'NONE',  ( 47.33349330513379982, -4.000000000000000000, 4.898587196589415787E-16 ) ) ;
#74322 =( NAMED_UNIT ( * ) PLANE_ANGLE_UNIT ( ) SI_UNIT ( $, .RADIAN. ) );
#74323 = CARTESIAN_POINT ( 'NONE',  ( 0.5336329302387069484, 21.82583525534633395, 6.984546992747041827 ) ) ;
#74324 = CARTESIAN_POINT ( 'NONE',  ( -38.96813603250004832, -24.55621239451162907, -30.50670703037211950 ) ) ;
#74326 = CARTESIAN_POINT ( 'NONE',  ( -70.42419927718661654, -34.58954792057054561, -21.61483060261837252 ) ) ;
#74325 = CARTESIAN_POINT ( 'NONE',  ( 42.61650669486618881, 4.000000000000003553, 4.898587196589414801E-16 ) ) ;
#74327 = EDGE_CURVE ( 'NONE', #26769, #48423, #67156, .T. ) ;
#74328 = ORIENTED_EDGE ( 'NONE', *, *, #11277, .T. ) ;
#74329 = CIRCLE ( 'NONE', #41627, 5.000000000000001776 ) ;
#74330 =( NAMED_UNIT ( * ) SI_UNIT ( $, .STERADIAN. ) SOLID_ANGLE_UNIT ( ) );
#74331 = VERTEX_POINT ( 'NONE', #90901 ) ;
#74332 = CARTESIAN_POINT ( 'NONE',  ( -26.48318267654033420, 34.96074735818669410, 7.710518002484812783 ) ) ;
#74333 = STYLED_ITEM ( 'NONE', ( #82058 ), #92949 ) ;
#74334 = ADVANCED_FACE ( 'NONE', ( #59067 ), #26733, .T. ) ;
#74335 = CARTESIAN_POINT ( 'NONE',  ( 6.999999999999999112, 0.000000000000000000, 0.000000000000000000 ) ) ;
#74336 = CARTESIAN_POINT ( 'NONE',  ( -26.53069809822883585, -60.00000000000000711, -41.28480351003638305 ) ) ;
#74337 = EDGE_LOOP ( 'NONE', ( #104497, #36346, #52306, #59034 ) ) ;
#74338 = CARTESIAN_POINT ( 'NONE',  ( 31.08825020654288096, -30.41363042624472257, -30.04296242939974704 ) ) ;
#74339 = CARTESIAN_POINT ( 'NONE',  ( -8.232252328884545278, 294.6936158193711321, -5.684270446938944232 ) ) ;
#74340 = CARTESIAN_POINT ( 'NONE',  ( 99.23206058371319216, -37.81684522924224012, 191.6622011877896057 ) ) ;
#74341 = CARTESIAN_POINT ( 'NONE',  ( -17.26536970378605318, 45.41327343741740918, 6.504208684746012104 ) ) ;
#74342 = VERTEX_POINT ( 'NONE', #65555 ) ;
#74343 = ORIENTED_EDGE ( 'NONE', *, *, #85309, .T. ) ;
#74344 = ORIENTED_EDGE ( 'NONE', *, *, #23528, .T. ) ;
#74345 = CARTESIAN_POINT ( 'NONE',  ( 31.22166362330205658, 392.4804080715629766, 25.19617774411732469 ) ) ;
#74346 = CARTESIAN_POINT ( 'NONE',  ( -6.105464488525263356, -12.30761336974420317, 12.19688296868001842 ) ) ;
#74347 = CARTESIAN_POINT ( 'NONE',  ( 0.000000000000000000, 0.000000000000000000, -0.01270000000000090501 ) ) ;
#74348 = EDGE_LOOP ( 'NONE', ( #10879, #40373, #4372, #13901 ) ) ;
#74349 = EDGE_CURVE ( 'NONE', #96401, #1420, #92477, .T. ) ;
#74350 = CARTESIAN_POINT ( 'NONE',  ( -7.069742149889167493, 41.66287055432060527, -69.58314084294492829 ) ) ;
#74351 = CYLINDRICAL_SURFACE ( 'NONE', #75499, 4.000000000000001776 ) ;
#74352 = CARTESIAN_POINT ( 'NONE',  ( -18.14395573440383203, -57.67158919250769600, 41.98617601139094546 ) ) ;
#74353 = CARTESIAN_POINT ( 'NONE',  ( -5.082755093536325042, -32.09375000204838813, -5.082755093536325930 ) ) ;
#74354 = CARTESIAN_POINT ( 'NONE',  ( -30.87964800539037569, 13.48323453669521044, 41.23000148635482276 ) ) ;
#74355 = DIRECTION ( 'NONE',  ( 0.000000000000000000, -1.000000000000000000, 0.000000000000000000 ) ) ;
#74356 = DIRECTION ( 'NONE',  ( 0.000000000000000000, 0.000000000000000000, 1.000000000000000000 ) ) ;
#74357 = CARTESIAN_POINT ( 'NONE',  ( 49.63358250961842799, -60.00000000000001421, -40.41868810089377462 ) ) ;
#74358 = CARTESIAN_POINT ( 'NONE',  ( -34.32536616635837845, -30.00000000000003553, 42.48815186199111338 ) ) ;
#74359 = CARTESIAN_POINT ( 'NONE',  ( -51.90208491409480018, -18.71866842149948695, 46.78754088036709646 ) ) ;
#74360 = CARTESIAN_POINT ( 'NONE',  ( 0.000000000000000000, 0.5000000000000000000, 0.000000000000000000 ) ) ;
#74361 = ORIENTED_EDGE ( 'NONE', *, *, #12747, .F. ) ;
#74362 = CARTESIAN_POINT ( 'NONE',  ( -98.06883061208564811, -45.24973764535013032, 193.7416408753538235 ) ) ;
#74363 = CARTESIAN_POINT ( 'NONE',  ( -1.050160786985519401, 296.8373249700017595, -10.00076906402484056 ) ) ;
#74364 = CARTESIAN_POINT ( 'NONE',  ( 12.39857089150704006, -3.847148675972121179, 20.49778519109818475 ) ) ;
#74365 = EDGE_LOOP ( 'NONE', ( #105607, #29474, #95926, #29402, #85940, #16981 ) ) ;
#74367 = B_SPLINE_CURVE_WITH_KNOTS ( 'NONE', 3,
 ( #92388, #68122, #101018, #74608, #18534, #58982, #53414, #25588 ),
 .UNSPECIFIED., .F., .F.,
 ( 4, 2, 2, 4 ),
 ( -1.045097417706059526E-05, 0.0004743348448042788079, 0.0007167277542949298044, 0.0009591206637855809094 ),
 .UNSPECIFIED. ) ;
#74366 = CARTESIAN_POINT ( 'NONE',  ( -17.99616949565368174, 34.41190775537305768, -22.85621917946001247 ) ) ;
#74368 = CARTESIAN_POINT ( 'NONE',  ( 98.38089941204171396, -38.47856758464003946, 200.9301062742698605 ) ) ;
#74369 = CARTESIAN_POINT ( 'NONE',  ( -6.139120788623333130E-13, -7.790635086498917339, -6.526184258131205951 ) ) ;
#74370 = CARTESIAN_POINT ( 'NONE',  ( 6.123233995736763324E-16, 48.00000000000000000, -75.00000000000001421 ) ) ;
#74371 = CIRCLE ( 'NONE', #19327, 5.000000000000001776 ) ;
#74372 = CARTESIAN_POINT ( 'NONE',  ( -17.24530556510137913, 294.5883485050384252, 1.881388368280897394 ) ) ;
#74373 = CARTESIAN_POINT ( 'NONE',  ( 88.20421627925426833, 42.00000000000000000, 23.70422451874904013 ) ) ;
#74374 = CARTESIAN_POINT ( 'NONE',  ( 85.56723171479005430, -30.00000000000000355, 175.4130121643509597 ) ) ;
#74375 = CARTESIAN_POINT ( 'NONE',  ( 8.559508646656405872, 51.55638410492942825, 4.031152949374444461 ) ) ;
#74376 = CARTESIAN_POINT ( 'NONE',  ( -37.52432843440377042, 473.0043530063420576, 17.54905768162751656 ) ) ;
#74377 = LINE ( 'NONE', #66839, #48409 ) ;
#74378 = ORIENTED_EDGE ( 'NONE', *, *, #74423, .F. ) ;
#74379 = ORIENTED_EDGE ( 'NONE', *, *, #103147, .T. ) ;
#74380 = CARTESIAN_POINT ( 'NONE',  ( 53.02351809876299882, -36.03604319102321085, 54.92990362263699211 ) ) ;
#74381 = CARTESIAN_POINT ( 'NONE',  ( 24.83349330513380337, 1.593028355512270567E-15, 0.000000000000000000 ) ) ;
#74382 = PRESENTATION_LAYER_ASSIGNMENT (  '', '', ( #72616 ) ) ;
#74383 = CARTESIAN_POINT ( 'NONE',  ( 36.32007205877684441, 28.16029012736642656, -12.39624372369306293 ) ) ;
#74384 = CIRCLE ( 'NONE', #55445, 8.000000000000014211 ) ;
#74385 = ORIENTED_EDGE ( 'NONE', *, *, #21019, .T. ) ;
#74386 = CARTESIAN_POINT ( 'NONE',  ( -107.8813328617326874, -38.35631905857745494, 136.9743310841232642 ) ) ;
#74387 = ORIENTED_EDGE ( 'NONE', *, *, #69607, .F. ) ;
#74388 = FILL_AREA_STYLE_COLOUR ( '', #19128 ) ;
#74389 = CARTESIAN_POINT ( 'NONE',  ( 91.67123410567980102, -38.35356722036148369, 31.46187313383635242 ) ) ;
#74390 = CARTESIAN_POINT ( 'NONE',  ( 13.77302195033687937, 22.96143443510463200, -1.023475060063897768 ) ) ;
#74391 = CARTESIAN_POINT ( 'NONE',  ( 87.75812269781596342, -52.71627564034628222, 47.57411664421275788 ) ) ;
#74392 = FACE_OUTER_BOUND ( 'NONE', #397, .T. ) ;
#74393 = CARTESIAN_POINT ( 'NONE',  ( -5.075566108724573589, -4.332661967060489339, -17.09624963492156624 ) ) ;
#74394 = CARTESIAN_POINT ( 'NONE',  ( -31.63428818830020006, 313.0192821382818806, -7.834016845888556624 ) ) ;
#74395 = FACE_OUTER_BOUND ( 'NONE', #103876, .T. ) ;
#74396 = CARTESIAN_POINT ( 'NONE',  ( 77.13274333098043201, -60.00000000000001421, 190.8571566051506636 ) ) ;
#74397 = CARTESIAN_POINT ( 'NONE',  ( -43.99245308601258841, 435.4957624057696535, 9.973844990784979103 ) ) ;
#74398 = ORIENTED_EDGE ( 'NONE', *, *, #93967, .T. ) ;
#74399 = CARTESIAN_POINT ( 'NONE',  ( 61.80202793844345877, -53.38729615061397737, 84.00710957604638907 ) ) ;
#74400 = CARTESIAN_POINT ( 'NONE',  ( -24.02662587718601728, 303.6064254585912181, -9.837495461294045285 ) ) ;
#74401 = CARTESIAN_POINT ( 'NONE',  ( 9.667921046838758414, -50.82596344167677671, 29.56517872135010094 ) ) ;
#74402 = EDGE_CURVE ( 'NONE', #23078, #45089, #7830, .T. ) ;
#74403 = CARTESIAN_POINT ( 'NONE',  ( -7.454085080097326177, -5.000000000000000000, -15.56508920776378702 ) ) ;
#74404 = B_SPLINE_CURVE_WITH_KNOTS ( 'NONE', 3,
 ( #99538, #276, #15975, #1361 ),
 .UNSPECIFIED., .F., .F.,
 ( 4, 4 ),
 ( 0.000000000000000000, 0.001739938677309369732 ),
 .UNSPECIFIED. ) ;
#74405 = EDGE_CURVE ( 'NONE', #100497, #34913, #19268, .T. ) ;
#74407 = CARTESIAN_POINT ( 'NONE',  ( -35.40631554953355931, 484.3223335191826777, -1.491095299259842077 ) ) ;
#74406 = CARTESIAN_POINT ( 'NONE',  ( -53.29442438667957305, -30.00000000005343992, 72.87987713644304222 ) ) ;
#74408 = CARTESIAN_POINT ( 'NONE',  ( -39.77306975198764860, 332.5681192115835643, 19.05727885500202845 ) ) ;
#74409 = CARTESIAN_POINT ( 'NONE',  ( -6.250000000000000888, -5.051814855409237026, -7.198902722707430257 ) ) ;
#74410 = DIRECTION ( 'NONE',  ( 0.000000000000000000, 0.000000000000000000, -1.000000000000000000 ) ) ;
#74411 = CARTESIAN_POINT ( 'NONE',  ( -8.000000000000000000, -28.24999999999999645, -9.797174393178825657E-16 ) ) ;
#74412 = CIRCLE ( 'NONE', #100211, 3.309500000000001663 ) ;
#74413 = SURFACE_STYLE_FILL_AREA ( #65274 ) ;
#74414 = EDGE_CURVE ( 'NONE', #57113, #67441, #98444, .T. ) ;
#74415 = AXIS2_PLACEMENT_3D ( 'NONE', #22378, #39072, #46096 ) ;
#74416 = DIRECTION ( 'NONE',  ( -1.000000000000000000, -1.224606353822377258E-16, -0.000000000000000000 ) ) ;
#74417 = VERTEX_POINT ( 'NONE', #27270 ) ;
#74418 = CARTESIAN_POINT ( 'NONE',  ( 82.57840738188596674, -53.59987598830502975, 184.4164446621147704 ) ) ;
#74419 = CARTESIAN_POINT ( 'NONE',  ( 43.49684453862397504, 485.4584183652858655, 3.971660685822626213 ) ) ;
#74420 = DIRECTION ( 'NONE',  ( -1.000000000000000000, -1.224606353822377258E-16, -0.000000000000000000 ) ) ;
#74421 = VERTEX_POINT ( 'NONE', #60155 ) ;
#74422 = CARTESIAN_POINT ( 'NONE',  ( 5.299999999999999822, -3.752776749732578132, -6.500000000000000888 ) ) ;
#74423 = EDGE_CURVE ( 'NONE', #77653, #104941, #38254, .T. ) ;
#74424 = CARTESIAN_POINT ( 'NONE',  ( 9.499999896953584155, -5.000000000000023093, -20.99851281918370205 ) ) ;
#74425 = FACE_OUTER_BOUND ( 'NONE', #17647, .T. ) ;
#74426 = CARTESIAN_POINT ( 'NONE',  ( -5.000000000000000888, -50.00000000000000000, 40.07669683062201926 ) ) ;
#74427 = CARTESIAN_POINT ( 'NONE',  ( -38.53974113589808326, 42.10961629870702438, -57.51661569422308418 ) ) ;
#74428 = CARTESIAN_POINT ( 'NONE',  ( -12.39352808926492067, -3.234829339351946054, 20.63804935124764484 ) ) ;
#74429 =( BOUNDED_SURFACE ( )  B_SPLINE_SURFACE ( 3, 3, ( 
 ( #25197, #100112, #18157, #26278 ),
 ( #92022, #43484, #24660, #57513 ),
 ( #83930, #16540, #66151, #69886 ),
 ( #21363, #4090, #86626, #68292 ),
 ( #86092, #29466, #28944, #11627 ),
 ( #53693, #52619, #87142, #77445 ),
 ( #20860, #12689, #95232, #85547 ),
 ( #37018, #61818, #62337, #4624 ),
 ( #3014, #68837, #93635, #19786 ),
 ( #101186, #37554, #102244, #35966 ),
 ( #2473, #45094, #3559, #60747 ),
 ( #54203, #45621, #61269, #78493 ),
 ( #19264, #44013, #76902, #85003 ),
 ( #13219, #36497, #76360, #94712 ),
 ( #101715, #35420, #69365, #27347 ),
 ( #77973, #103319, #60225, #12163 ),
 ( #93093, #52093, #11087, #27882 ),
 ( #70422, #44557, #28396, #94159 ) ),
 .UNSPECIFIED., .F., .F., .T. ) 
 B_SPLINE_SURFACE_WITH_KNOTS ( ( 4, 2, 2, 2, 2, 2, 2, 2, 4 ),
 ( 4, 4 ),
 ( 0.000000000000000000, 0.06249999999999997224, 0.1249999999999999445, 0.2500000000000000000, 0.3750000000000000555, 0.5000000000000000000, 0.7500000000000000000, 0.8750000000000000000, 1.000000000000000000 ),
 ( 0.000000000000000000, 1.000000000000000000 ),
 .UNSPECIFIED. ) 
 GEOMETRIC_REPRESENTATION_ITEM ( )  RATIONAL_B_SPLINE_SURFACE ( (
 ( 1.000000000000000000, 0.3333333333333334259, 0.3333333333333334259, 1.000000000000000000),
 ( 1.000000000000000000, 0.3333333333333334259, 0.3333333333333334259, 1.000000000000000000),
 ( 1.000000000000000000, 0.3333333333333334259, 0.3333333333333334259, 1.000000000000000000),
 ( 1.000000000000000000, 0.3333333333333334259, 0.3333333333333334259, 1.000000000000000000),
 ( 1.000000000000000000, 0.3333333333333334259, 0.3333333333333334259, 1.000000000000000000),
 ( 1.000000000000000000, 0.3333333333333334259, 0.3333333333333334259, 1.000000000000000000),
 ( 1.000000000000000000, 0.3333333333333334259, 0.3333333333333334259, 1.000000000000000000),
 ( 1.000000000000000000, 0.3333333333333334259, 0.3333333333333334259, 1.000000000000000000),
 ( 1.000000000000000000, 0.3333333333333334259, 0.3333333333333334259, 1.000000000000000000),
 ( 1.000000000000000000, 0.3333333333333334259, 0.3333333333333334259, 1.000000000000000000),
 ( 1.000000000000000000, 0.3333333333333334259, 0.3333333333333334259, 1.000000000000000000),
 ( 1.000000000000000000, 0.3333333333333334259, 0.3333333333333334259, 1.000000000000000000),
 ( 1.000000000000000000, 0.3333333333333334259, 0.3333333333333334259, 1.000000000000000000),
 ( 1.000000000000000000, 0.3333333333333334259, 0.3333333333333334259, 1.000000000000000000),
 ( 1.000000000000000000, 0.3333333333333334259, 0.3333333333333334259, 1.000000000000000000),
 ( 1.000000000000000000, 0.3333333333333334259, 0.3333333333333334259, 1.000000000000000000),
 ( 1.000000000000000000, 0.3333333333333334259, 0.3333333333333334259, 1.000000000000000000),
 ( 1.000000000000000000, 0.3333333333333334259, 0.3333333333333334259, 1.000000000000000000) ) ) 
 REPRESENTATION_ITEM ( '' )  SURFACE ( )  );
#74430 = CARTESIAN_POINT ( 'NONE',  ( 50.66975656709965392, -60.00000000000000000, 73.49217170142772204 ) ) ;
#74431 = CARTESIAN_POINT ( 'NONE',  ( 7.619753052866894194, 108.1745150280717382, -2.447276542590450354 ) ) ;
#74432 = CARTESIAN_POINT ( 'NONE',  ( 24.24390522887371802, -18.95292958071728151, 31.52331660755031706 ) ) ;
#74434 = CARTESIAN_POINT ( 'NONE',  ( -13.59263768938421713, 24.77097348052605597, -0.6145898399614796448 ) ) ;
#74433 = CARTESIAN_POINT ( 'NONE',  ( -12.95257293317843228, -21.59228805338226920, 35.67007454052365034 ) ) ;
#74435 = CARTESIAN_POINT ( 'NONE',  ( 7.188101187500001821, -13.06250000204838280, -2.977408999572650483 ) ) ;
#74436 = CARTESIAN_POINT ( 'NONE',  ( 24.41215030396864449, 295.4555635972245682, -1.870474547456364878 ) ) ;
#74437 = CARTESIAN_POINT ( 'NONE',  ( 0.000000000000000000, 0.000000000000000000, 0.000000000000000000 ) ) ;
#74438 = ORIENTED_EDGE ( 'NONE', *, *, #2495, .T. ) ;
#74439 = VECTOR ( 'NONE', #48556, 1000.000000000000000 ) ;
#74440 = CARTESIAN_POINT ( 'NONE',  ( -17.49999999999739941, 49.76444793454294313, 62.19248936617950818 ) ) ;
#74441 = DIRECTION ( 'NONE',  ( -1.000000000000000000, -0.000000000000000000, -0.000000000000000000 ) ) ;
#74442 = CIRCLE ( 'NONE', #91648, 9.000000000000000000 ) ;
#74443 = FACE_OUTER_BOUND ( 'NONE', #87160, .T. ) ;
#74445 = CARTESIAN_POINT ( 'NONE',  ( 25.26525204496489252, -34.58978890963047093, -31.37000190431579583 ) ) ;
#74444 = CARTESIAN_POINT ( 'NONE',  ( 4.298171162025412606, 53.80428045674285187, 8.058306618997294279 ) ) ;
#74446 = EDGE_CURVE ( 'NONE', #18270, #48268, #91584, .T. ) ;
#74447 = ORIENTED_EDGE ( 'NONE', *, *, #51284, .F. ) ;
#74448 = CARTESIAN_POINT ( 'NONE',  ( 13.63566925393123164, 20.28444567501044915, -6.862276106173472279 ) ) ;
#74449 = DIRECTION ( 'NONE',  ( 0.000000000000000000, 1.000000000000000000, 0.000000000000000000 ) ) ;
#74451 = VERTEX_POINT ( 'NONE', #84932 ) ;
#74450 = VECTOR ( 'NONE', #77716, 1000.000000000000000 ) ;
#74452 = EDGE_CURVE ( 'NONE', #49798, #22652, #100489, .T. ) ;
#74453 =( NAMED_UNIT ( * ) PLANE_ANGLE_UNIT ( ) SI_UNIT ( $, .RADIAN. ) );
#74454 = EDGE_CURVE ( 'NONE', #34973, #18508, #105358, .T. ) ;
#74455 = CARTESIAN_POINT ( 'NONE',  ( 0.000000000000000000, 0.000000000000000000, 4.000000000000000888 ) ) ;
#74456 = CARTESIAN_POINT ( 'NONE',  ( -23.01262813884551761, 41.68868216767802437, -75.63873355076052007 ) ) ;
#74457 = CARTESIAN_POINT ( 'NONE',  ( -100.8708696091340897, -60.00000000000001421, 86.14267496683164893 ) ) ;
#74458 = CARTESIAN_POINT ( 'NONE',  ( -31.96671797320371766, 484.9925651024506692, 5.143045411170144909 ) ) ;
#74459 = CARTESIAN_POINT ( 'NONE',  ( 6.601567268551443490, -5.319966374295975520, -7.792327460285858542 ) ) ;
#74460 = CARTESIAN_POINT ( 'NONE',  ( 35.76320840016588676, 388.4727839510825333, 5.610592865731860002 ) ) ;
#74461 = DIRECTION ( 'NONE',  ( 0.000000000000000000, 0.000000000000000000, 1.000000000000000000 ) ) ;
#74463 = CARTESIAN_POINT ( 'NONE',  ( -2.500000000000001332, 0.000000000000000000, 8.900000000000000355 ) ) ;
#74462 = CARTESIAN_POINT ( 'NONE',  ( -7.374560640984191728, -5.000000000000002665, -75.40399789251388540 ) ) ;
#74464 = CARTESIAN_POINT ( 'NONE',  ( -80.98092848404644428, -56.94632824160903795, 178.5830683470894655 ) ) ;
#74465 = VERTEX_POINT ( 'NONE', #55196 ) ;
#74466 = VERTEX_POINT ( 'NONE', #14735 ) ;
#74467 = ORIENTED_EDGE ( 'NONE', *, *, #5337, .F. ) ;
#74468 = LINE ( 'NONE', #25988, #33744 ) ;
#74469 = TOROIDAL_SURFACE ( 'NONE', #79639, 13.00000000000000000, 2.000000000000000000 ) ;
#74470 = FACE_OUTER_BOUND ( 'NONE', #65485, .T. ) ;
#74471 = VERTEX_POINT ( 'NONE', #47634 ) ;
#74472 = EDGE_CURVE ( 'NONE', #43607, #36441, #80535, .T. ) ;
#74473 = STYLED_ITEM ( 'NONE', ( #14325 ), #31828 ) ;
#74474 = DIRECTION ( 'NONE',  ( -0.000000000000000000, -0.000000000000000000, 1.000000000000000000 ) ) ;
#74475 = SURFACE_STYLE_FILL_AREA ( #25994 ) ;
#74476 = CARTESIAN_POINT ( 'NONE',  ( 98.31310517497099966, 6.123233995736568081E-16, -5.000000000000011546 ) ) ;
#74477 = CARTESIAN_POINT ( 'NONE',  ( 95.42421628608209971, 1.030564683017419500E-14, 0.000000000000000000 ) ) ;
#74478 = CONICAL_SURFACE ( 'NONE', #3837, 7.000000000000000000, 0.9599310885968753704 ) ;
#74479 = CARTESIAN_POINT ( 'NONE',  ( 43.63014793319424456, 464.1804522840816389, 6.475900273557109621 ) ) ;
#74480 = CARTESIAN_POINT ( 'NONE',  ( 37.96538461538461462, 1.411358822780289120E-15, 0.000000000000000000 ) ) ;
#74481 = CARTESIAN_POINT ( 'NONE',  ( -43.86555507693260836, 486.1044689237326679, 5.341991804863218007 ) ) ;
#74482 = CARTESIAN_POINT ( 'NONE',  ( 114.5768552918926986, -59.99999999999997868, 170.6725192690976485 ) ) ;
#74483 = EDGE_CURVE ( 'NONE', #102392, #61647, #32319, .T. ) ;
#74484 = CARTESIAN_POINT ( 'NONE',  ( -108.4361608695136994, -30.00000000000004974, 186.7333242197273080 ) ) ;
#74485 = CARTESIAN_POINT ( 'NONE',  ( -63.73445214523361102, -22.10497644405380768, 73.75391651273872640 ) ) ;
#74486 = EDGE_LOOP ( 'NONE', ( #83526, #72435, #25213, #71926 ) ) ;
#74487 = CARTESIAN_POINT ( 'NONE',  ( 11.63000494888384395, 38.95405869521447784, 62.66525763215405220 ) ) ;
#74488 = CARTESIAN_POINT ( 'NONE',  ( 114.6102123966894055, -60.00000000000000000, 174.7595319735745818 ) ) ;
#74489 = ORIENTED_EDGE ( 'NONE', *, *, #84212, .F. ) ;
#74490 = CARTESIAN_POINT ( 'NONE',  ( 5.993569525592590708, -22.06720269990192307, 27.55800827838890399 ) ) ;
#74491 = CARTESIAN_POINT ( 'NONE',  ( -103.7138855257204995, -60.15497775133528791, 139.5353567617456463 ) ) ;
#74492 = CARTESIAN_POINT ( 'NONE',  ( 7.188101187500000044, -15.03125000204838457, 0.000000000000000000 ) ) ;
#74493 = EDGE_CURVE ( 'NONE', #88353, #93333, #45802, .T. ) ;
#74494 = CARTESIAN_POINT ( 'NONE',  ( -4.205882352941162416, -5.000000000000000000, -72.69916451482997388 ) ) ;
#74495 = ORIENTED_EDGE ( 'NONE', *, *, #31661, .F. ) ;
#74496 = CARTESIAN_POINT ( 'NONE',  ( -10.36871714652622245, 45.36883139708662327, 15.40779740156165367 ) ) ;
#74497 = ORIENTED_EDGE ( 'NONE', *, *, #1070, .F. ) ;
#74498 = CARTESIAN_POINT ( 'NONE',  ( 0.000000000000000000, 1.999999999999998224, 0.000000000000000000 ) ) ;
#74499 = CARTESIAN_POINT ( 'NONE',  ( -55.39551486789333978, -59.99999999999998579, 86.38772855768377212 ) ) ;
#74500 = CARTESIAN_POINT ( 'NONE',  ( 9.226882652173665988, -54.53219447884240623, 23.14412647329060491 ) ) ;
#74501 = CARTESIAN_POINT ( 'NONE',  ( -2.977408999572654480, -18.50000000204838457, 7.188101187499999156 ) ) ;
#74502 = CARTESIAN_POINT ( 'NONE',  ( -7.000000000000000000, 8.572527594031471218E-16, -13.00000000000000000 ) ) ;
#74503 = FACE_OUTER_BOUND ( 'NONE', #10725, .T. ) ;
#74504 = CARTESIAN_POINT ( 'NONE',  ( 23.86650669486618881, 1.474610560812782335E-15, 0.000000000000000000 ) ) ;
#74505 = DIRECTION ( 'NONE',  ( 1.000000000000000000, -0.000000000000000000, -0.000000000000000000 ) ) ;
#74506 = LINE ( 'NONE', #58332, #2010 ) ;
#74507 = CARTESIAN_POINT ( 'NONE',  ( 8.238185353303229874, -12.24652543886333511, 8.668425773002917722 ) ) ;
#74508 = CARTESIAN_POINT ( 'NONE',  ( -35.38683386460204616, 303.0231846730247867, -0.1303635103169306364 ) ) ;
#74509 = DIRECTION ( 'NONE',  ( 0.000000000000000000, 0.8267102254928009319, -0.5626279437298172814 ) ) ;
#74510 = B_SPLINE_CURVE_WITH_KNOTS ( 'NONE', 3,
 ( #44028, #36511, #85018, #28960, #94178, #76920, #68852, #20344, #53190, #94727, #73, #46160, #87684, #54752, #55281, #70956, #79572, #13235, #14291, #82079, #96313, #79048, #87155, #98275, #73452, #62354, #37571, #45632, #95244, #57800, #106350, #38096, #62878, #29477, #21376, #5167, #32512, #40570, #47195, #54214, #103847, #29992, #95769, #21905, #13764, #63421, #38609, #41109, #65384, #24433, #33044, #46673, #5685, #80095, #57265, #71472, #104372, #22441, #16290, #30523, #88210, #7653, #4640, #70436, #90188, #12703, #49175, #8198, #73991, #65910, #98790, #24947, #78507, #103331, #17911, #82628 ),
 .UNSPECIFIED., .F., .F.,
 ( 4, 2, 2, 2, 2, 2, 2, 2, 2, 2, 2, 2, 2, 2, 2, 2, 2, 2, 2, 2, 2, 2, 2, 2, 2, 2, 2, 2, 2, 2, 2, 2, 2, 2, 2, 2, 2, 4 ),
 ( 0.02393199801744600591, 0.02587788593328142414, 0.02782377384911684237, 0.02976966176495226060, 0.03171554968078767883, 0.03366143759662310053, 0.03560732551245852223, 0.03755321342829394393, 0.03852615738621165825, 0.03949910134412936563, 0.04144498925996478733, 0.04339087717580021597, 0.04436382113371792335, 0.04533676509163563073, 0.04728265300747104549, 0.04825559696538875981, 0.04922854092330646719, 0.05117442883914188889, 0.05312031675497731753, 0.05506620467081274617, 0.05603914862873046049, 0.05701209258664816787, 0.05895798050248358957, 0.06090386841831902515, 0.06187681237623673253, 0.06284975633415444685, 0.06479564424998987548, 0.06674153216582529025, 0.06868742008166071888, 0.07063330799749614752, 0.07257919591333157616, 0.07452508382916700480, 0.07647097174500241956, 0.07841685966083784820, 0.08036274757667327684, 0.08230863549250871936, 0.08425452340834414799, 0.08620041132417957663 ),
 .UNSPECIFIED. ) ;
#74511 = CARTESIAN_POINT ( 'NONE',  ( -32.86356798609371310, -39.49558199937673919, 34.28045917445315638 ) ) ;
#74512 = CARTESIAN_POINT ( 'NONE',  ( -3.363582653045684712, -48.78526580464421869, 104.5994639297834681 ) ) ;
#74513 = CARTESIAN_POINT ( 'NONE',  ( 43.56271327712536845, -60.24810023598861619, 47.28533951050904705 ) ) ;
#74514 = SURFACE_STYLE_USAGE ( .BOTH. , #98267 ) ;
#74515 = ORIENTED_EDGE ( 'NONE', *, *, #6512, .T. ) ;
#74516 = CARTESIAN_POINT ( 'NONE',  ( 43.99245308600651327, 435.4957624057694261, 9.973844990776925101 ) ) ;
#74517 = CARTESIAN_POINT ( 'NONE',  ( -76.01953405358801774, -38.37905128380688069, 178.5008278763145313 ) ) ;
#74518 = ORIENTED_EDGE ( 'NONE', *, *, #49103, .F. ) ;
#74520 = CARTESIAN_POINT ( 'NONE',  ( 40.77380256327629837, 468.8478597483947965, 21.13608272249925690 ) ) ;
#74519 = FACE_OUTER_BOUND ( 'NONE', #70601, .T. ) ;
#74521 = CARTESIAN_POINT ( 'NONE',  ( 80.33268691154432872, -59.99999999999999289, 177.7134108711020133 ) ) ;
#74522 = DIRECTION ( 'NONE',  ( 0.000000000000000000, 0.000000000000000000, -1.000000000000000000 ) ) ;
#74523 = CARTESIAN_POINT ( 'NONE',  ( 6.352644769543715597, 2.685840869108905071, 6.499999999999998224 ) ) ;
#74524 = LINE ( 'NONE', #68037, #67016 ) ;
#74525 = FACE_OUTER_BOUND ( 'NONE', #42649, .T. ) ;
#74527 = CARTESIAN_POINT ( 'NONE',  ( 6.000208918519490453, -89.00031337789968688, -0.2646532170642273973 ) ) ;
#74526 = AXIS2_PLACEMENT_3D ( 'NONE', #19385, #83000, #68424 ) ;
#74528 = CARTESIAN_POINT ( 'NONE',  ( 16.64348903516499334, 45.60392139269944067, 6.657797401562596917 ) ) ;
#74529 = CARTESIAN_POINT ( 'NONE',  ( 111.0024401811853210, -60.00000000000000000, 152.1606877285774715 ) ) ;
#74531 = CARTESIAN_POINT ( 'NONE',  ( -3.053636405311067836, -53.45138136750625790, 40.66466748881163795 ) ) ;
#74530 = CIRCLE ( 'NONE', #90088, 4.000000000000000888 ) ;
#74532 = MECHANICAL_DESIGN_GEOMETRIC_PRESENTATION_REPRESENTATION (  '', ( #5631 ), #79698 ) ;
#74533 = CARTESIAN_POINT ( 'NONE',  ( -38.85838710091159953, 485.2519636814003547, -4.251885899892715592 ) ) ;
#74534 = ORIENTED_EDGE ( 'NONE', *, *, #48102, .F. ) ;
#74535 = ADVANCED_FACE ( 'NONE', ( #4812 ), #60566, .T. ) ;
#74536 = CARTESIAN_POINT ( 'NONE',  ( -98.19961658146921479, -29.99999999999990763, 190.3012536825193308 ) ) ;
#74537 = ORIENTED_EDGE ( 'NONE', *, *, #8335, .T. ) ;
#74538 = CARTESIAN_POINT ( 'NONE',  ( 26.49205890517669104, 36.83376193817070288, -9.907811712491993106 ) ) ;
#74539 = CARTESIAN_POINT ( 'NONE',  ( -15.85122647056015488, 4.114663126770048862, 4.288211754903009876 ) ) ;
#74540 = FILL_AREA_STYLE_COLOUR ( '', #48346 ) ;
#74541 = CARTESIAN_POINT ( 'NONE',  ( 9.989435848181784650, 26.02619707471574273, -0.5278651953176120015 ) ) ;
#74542 = AXIS2_PLACEMENT_3D ( 'NONE', #84762, #68040, #94462 ) ;
#74543 = CARTESIAN_POINT ( 'NONE',  ( 7.188101187499999156, -16.62500000204838457, 2.977408999572654924 ) ) ;
#74544 =( NAMED_UNIT ( * ) PLANE_ANGLE_UNIT ( ) SI_UNIT ( $, .RADIAN. ) );
#74545 = CARTESIAN_POINT ( 'NONE',  ( 16.75187969033515145, 37.11970326878314808, -21.80698433968624528 ) ) ;
#74546 = EDGE_CURVE ( 'NONE', #59135, #64268, #58863, .T. ) ;
#74547 = ADVANCED_FACE ( 'NONE', ( #22076 ), #87859, .T. ) ;
#74548 = B_SPLINE_CURVE_WITH_KNOTS ( 'NONE', 3,
 ( #79422, #64320, #37951, #15214, #81003, #79944, #89646, #23337, #103703, #105295, #72907, #63260, #22815, #14142, #64838, #105817, #46010, #5017, #13614, #5537, #71854, #29850, #88586, #62727, #6054, #38462, #104222, #30369, #96151, #22284, #55133, #16276, #74508, #25479, #57253, #15748, #32498, #98779, #34102, #83143, #16823, #24931, #24414, #57783, #585, #9240, #98261, #65368 ),
 .UNSPECIFIED., .F., .F.,
 ( 4, 2, 2, 2, 2, 2, 2, 2, 2, 2, 2, 2, 2, 2, 2, 2, 2, 2, 2, 2, 2, 2, 2, 4 ),
 ( 0.0007293822660806825427, 0.01952279057336408011, 0.03831619888064748125, 0.05710960718793087892, 0.06650631134157250490, 0.07590301549521411006, 0.08529971964885574298, 0.09469642380249734814, 0.1040931279561389672, 0.1134898321097805723, 0.1181881841866014582, 0.1228865362634223579, 0.1252357123018327245, 0.1275848883402430911, 0.1322832404170639631, 0.1334578284362692435, 0.1346324164554744685, 0.1369815924938849461, 0.1393307685322954514, 0.1405053565515007596, 0.1416799445707060401, 0.1440291206091167397, 0.1463782966475274394, 0.1510766487243488110 ),
 .UNSPECIFIED. ) ;
#74549 = ORIENTED_EDGE ( 'NONE', *, *, #24497, .F. ) ;
#74550 = CARTESIAN_POINT ( 'NONE',  ( 81.95403812627554885, -46.45362839144696920, 171.2155095704361543 ) ) ;
#74551 = SURFACE_SIDE_STYLE ('',( #66467 ) ) ;
#74552 = VERTEX_POINT ( 'NONE', #85750 ) ;
#74553 = CARTESIAN_POINT ( 'NONE',  ( -58.66291549205074318, 49.99999999999999289, -23.00456702330189174 ) ) ;
#74554 = EDGE_CURVE ( 'NONE', #72232, #45904, #70892, .T. ) ;
#74556 = EDGE_CURVE ( 'NONE', #46369, #49037, #16834, .T. ) ;
#74555 = CARTESIAN_POINT ( 'NONE',  ( -47.01788285976065396, 17.61616053603705723, 16.34433538609877345 ) ) ;
#74557 = CARTESIAN_POINT ( 'NONE',  ( 38.18871050945294598, 27.40971527590679102, -13.30253190289822918 ) ) ;
#74558 = CARTESIAN_POINT ( 'NONE',  ( 0.000000000000000000, 0.000000000000000000, -4.999999999999999112 ) ) ;
#74559 = CARTESIAN_POINT ( 'NONE',  ( 11.74185064025517100, -59.99999999999997868, -36.59818147136398636 ) ) ;
#74561 = CARTESIAN_POINT ( 'NONE',  ( -30.39986296867173365, 318.3104204385729190, 13.73210969081261013 ) ) ;
#74560 = AXIS2_PLACEMENT_3D ( 'NONE', #74836, #41421, #8517 ) ;
#74562 = B_SPLINE_CURVE_WITH_KNOTS ( 'NONE', 3,
 ( #49676, #75002, #10281, #82582, #25996, #83633, #42653, #1096, #34071, #1646, #43193, #34607, #67476, #76077, #27586, #45332, #36741, #70124 ),
 .UNSPECIFIED., .F., .F.,
 ( 4, 2, 2, 2, 2, 2, 2, 2, 4 ),
 ( 0.01279395524623341308, 0.01359259090959848149, 0.01439122657296354989, 0.01518986223632861829, 0.01598849789969368496, 0.01678713356305875509, 0.01758576922642382523, 0.01838440488978889190, 0.01918304055315395856 ),
 .UNSPECIFIED. ) ;
#74563 = DIRECTION ( 'NONE',  ( 1.000000000000000000, -0.000000000000000000, -0.000000000000000000 ) ) ;
#74564 = ORIENTED_EDGE ( 'NONE', *, *, #23670, .F. ) ;
#74565 = COLOUR_RGB ( '', 0.72549020, 0.75294118, 0.79215686) ;
#74566 = CARTESIAN_POINT ( 'NONE',  ( -1.128087032575124216, 302.6811185911183770, 9.936167251361171182 ) ) ;
#74567 = LINE ( 'NONE', #96741, #65104 ) ;
#74568 = CARTESIAN_POINT ( 'NONE',  ( 85.99101760945637807, -57.43956396353277682, 193.1180272415432739 ) ) ;
#74569 = DIRECTION ( 'NONE',  ( -0.000000000000000000, 1.000000000000000000, -0.000000000000000000 ) ) ;
#74570 = CARTESIAN_POINT ( 'NONE',  ( -5.082755093536326818, -31.71875000204838457, 5.082755093536325042 ) ) ;
#74571 = DIRECTION ( 'NONE',  ( -0.000000000000000000, -1.000000000000000000, -0.000000000000000000 ) ) ;
#74572 = LINE ( 'NONE', #100981, #51705 ) ;
#74573 = CARTESIAN_POINT ( 'NONE',  ( 36.49542067541441526, 439.4713014004300362, 23.89653312818885311 ) ) ;
#74574 = CONTEXT_DEPENDENT_SHAPE_REPRESENTATION ( #90748, #54399 ) ;
#74575 = CARTESIAN_POINT ( 'NONE',  ( -9.380871178326124493, 32.01116379798327216, 3.467392232194196566 ) ) ;
#74576 = VERTEX_POINT ( 'NONE', #76432 ) ;
#74577 = CARTESIAN_POINT ( 'NONE',  ( 0.7821289637610407963, 43.98379635595578208, 16.51122116237588244 ) ) ;
#74578 = CARTESIAN_POINT ( 'NONE',  ( 0.000000000000000000, 4.898587196589412829E-16, -4.000000000000000000 ) ) ;
#74579 = CARTESIAN_POINT ( 'NONE',  ( 31.36650669486618881, 4.000000000000003553, 4.898587196589414801E-16 ) ) ;
#74580 =( NAMED_UNIT ( * ) PLANE_ANGLE_UNIT ( ) SI_UNIT ( $, .RADIAN. ) );
#74581 = EDGE_LOOP ( 'NONE', ( #36092, #1848, #68286, #89455 ) ) ;
#74582 = DIRECTION ( 'NONE',  ( 0.000000000000000000, 1.000000000000000000, 0.000000000000000000 ) ) ;
#74583 = FACE_OUTER_BOUND ( 'NONE', #27886, .T. ) ;
#74584 = CARTESIAN_POINT ( 'NONE',  ( 106.9239920550738958, -57.67118183550353905, 109.9283693084385760 ) ) ;
#74585 = EDGE_CURVE ( 'NONE', #29666, #35363, #33005, .T. ) ;
#74586 = CARTESIAN_POINT ( 'NONE',  ( 35.72584807339057988, 463.6218724463090552, 19.50045127627888775 ) ) ;
#74587 = LINE ( 'NONE', #48188, #56967 ) ;
#74588 = DIRECTION ( 'NONE',  ( 1.000000000000000000, 1.224606353822377258E-16, 0.000000000000000000 ) ) ;
#74589 = CARTESIAN_POINT ( 'NONE',  ( 13.69035610859369889, 302.5483965847918739, 9.872518234831204609 ) ) ;
#74590 = CARTESIAN_POINT ( 'NONE',  ( -84.26043389055706712, -60.00000000000001421, 199.6846189265752116 ) ) ;
#74591 = CONICAL_SURFACE ( 'NONE', #47108, 3.309500000000001663, 0.9599310885968770357 ) ;
#74592 = DIRECTION ( 'NONE',  ( 0.000000000000000000, -1.000000000000000000, 0.000000000000000000 ) ) ;
#74593 = CARTESIAN_POINT ( 'NONE',  ( -40.88293604215247967, 432.5779639752643675, 26.56799667982232549 ) ) ;
#74594 = CARTESIAN_POINT ( 'NONE',  ( -83.31161619671260610, -53.71026484535321543, 187.1193032696220655 ) ) ;
#74595 = STYLED_ITEM ( 'NONE', ( #55861 ), #84035 ) ;
#74596 = VERTEX_POINT ( 'NONE', #50550 ) ;
#74597 = CARTESIAN_POINT ( 'NONE',  ( 26.45606761501369064, 305.8501895426643387, -9.560627638420045926 ) ) ;
#74598 = CONICAL_SURFACE ( 'NONE', #57345, 5.000000000000010658, 0.9599310885968697082 ) ;
#74599 = ORIENTED_EDGE ( 'NONE', *, *, #67679, .F. ) ;
#74600 = CARTESIAN_POINT ( 'NONE',  ( -23.21751746555280249, 25.98869614573808207, -30.70617127781034839 ) ) ;
#74601 = CARTESIAN_POINT ( 'NONE',  ( -84.32710418608468217, -45.26462801463393504, -10.05937244304523759 ) ) ;
#74602 = CARTESIAN_POINT ( 'NONE',  ( -4.337283319711771057, -10.96666117361756321, -10.25672613774104391 ) ) ;
#74603 = CARTESIAN_POINT ( 'NONE',  ( 5.420470438621123321, 41.88321586334136981, -59.04137885805280916 ) ) ;
#74604 = AXIS2_PLACEMENT_3D ( 'NONE', #49595, #474, #8605 ) ;
#74605 = CARTESIAN_POINT ( 'NONE',  ( 17.33349330513380693, 1.593028355512270962E-15, 0.000000000000000000 ) ) ;
#74606 = CARTESIAN_POINT ( 'NONE',  ( -3.202923538441288187, -1.002156644461976498, 104.2983658136044909 ) ) ;
#74607 = CARTESIAN_POINT ( 'NONE',  ( 11.89626370526795185, 6.535353899124712207, -8.953647278333551895 ) ) ;
#74608 = CARTESIAN_POINT ( 'NONE',  ( 3.375204959346052025, -0.8899440043431781078, 104.1122719450857375 ) ) ;
#74609 = DIRECTION ( 'NONE',  ( -1.000000000000000000, 0.000000000000000000, 0.000000000000000000 ) ) ;
#74610 = CARTESIAN_POINT ( 'NONE',  ( -40.75117554026711275, -14.21045842199432663, -34.22202116092960011 ) ) ;
#74611 = CARTESIAN_POINT ( 'NONE',  ( -75.17510521376654253, -49.90938227346595113, 129.2199156371341360 ) ) ;
#74612 = ORIENTED_EDGE ( 'NONE', *, *, #47518, .T. ) ;
#74613 = CARTESIAN_POINT ( 'NONE',  ( 57.26188992556405566, -30.00000000000000355, 83.64747613098029433 ) ) ;
#74614 = CARTESIAN_POINT ( 'NONE',  ( 7.046357527897575856, 86.30615650601002642, -3.789683693877207826 ) ) ;
#74615 = CARTESIAN_POINT ( 'NONE',  ( 94.74039510923110186, -57.67204590878498749, 29.85737974855511112 ) ) ;
#74616 = ORIENTED_EDGE ( 'NONE', *, *, #75268, .F. ) ;
#74617 = LINE ( 'NONE', #99415, #9683 ) ;
#74618 = ADVANCED_FACE ( 'NONE', ( #92624 ), #25267, .F. ) ;
#74619 = FACE_BOUND ( 'NONE', #50863, .T. ) ;
#74620 = VERTEX_POINT ( 'NONE', #34958 ) ;
#74621 = DIRECTION ( 'NONE',  ( 0.000000000000000000, -1.000000000000000000, 0.000000000000000000 ) ) ;
#74622 = CIRCLE ( 'NONE', #33553, 8.000000000000000000 ) ;
#74623 = DIRECTION ( 'NONE',  ( 0.000000000000000000, 0.000000000000000000, 1.000000000000000000 ) ) ;
#74624 = DIRECTION ( 'NONE',  ( -0.000000000000000000, -1.000000000000000000, -0.000000000000000000 ) ) ;
#74625 = CARTESIAN_POINT ( 'NONE',  ( 5.082755093536324154, -10.34375000204838457, 5.082755093536326818 ) ) ;
#74626 = CARTESIAN_POINT ( 'NONE',  ( 6.486836893982499852, -4.915077010914404632, -7.231838333420563814 ) ) ;
#74627 = AXIS2_PLACEMENT_3D ( 'NONE', #59038, #58504, #42842 ) ;
#74628 = DIRECTION ( 'NONE',  ( -3.469446951953611033E-15, 0.000000000000000000, 1.000000000000000000 ) ) ;
#74629 = CARTESIAN_POINT ( 'NONE',  ( -7.908228835406298174, 3.123118350875301985, -7.776694659840482693 ) ) ;
#74630 = CARTESIAN_POINT ( 'NONE',  ( 8.841337832402281549, 48.00000000000000711, -97.17444126923535919 ) ) ;
#74631 =( GEOMETRIC_REPRESENTATION_CONTEXT ( 3 ) GLOBAL_UNCERTAINTY_ASSIGNED_CONTEXT ( ( #48886 ) ) GLOBAL_UNIT_ASSIGNED_CONTEXT ( ( #114, #24987, #36814 ) ) REPRESENTATION_CONTEXT ( 'NONE', 'WORKASPACE' ) );
#74632 = AXIS2_PLACEMENT_3D ( 'NONE', #97792, #23956, #88652 ) ;
#74633 = ORIENTED_EDGE ( 'NONE', *, *, #93351, .T. ) ;
#74634 = CARTESIAN_POINT ( 'NONE',  ( -7.176538178872569951, 40.00000000006200196, -70.93639620227449427 ) ) ;
#74635 = AXIS2_PLACEMENT_3D ( 'NONE', #10729, #52258, #18333 ) ;
#74637 = CARTESIAN_POINT ( 'NONE',  ( 30.11862666518024767, -46.43205139143292826, 34.40975861721332762 ) ) ;
#74636 = DIRECTION ( 'NONE',  ( -1.000000000000000000, -1.224606353822377258E-16, -0.000000000000000000 ) ) ;
#74638 = CARTESIAN_POINT ( 'NONE',  ( 33.54694104246176778, 327.2920069512696273, -3.491838498529484802 ) ) ;
#74639 = ORIENTED_EDGE ( 'NONE', *, *, #91450, .T. ) ;
#74640 = LINE ( 'NONE', #83275, #102966 ) ;
#74641 = ORIENTED_EDGE ( 'NONE', *, *, #64124, .T. ) ;
#74642 = DIRECTION ( 'NONE',  ( 1.000000000000000000, -0.000000000000000000, -0.000000000000000000 ) ) ;
#74643 = CARTESIAN_POINT ( 'NONE',  ( 18.75165323930665906, 302.6701165016055484, -10.03850434714902740 ) ) ;
#74644 = CARTESIAN_POINT ( 'NONE',  ( -17.59839952628324511, 294.5991929880352700, -2.053311126443894352 ) ) ;
#74645 = CARTESIAN_POINT ( 'NONE',  ( 0.3334994693927795795, 45.31831760051831282, 18.70763632781319075 ) ) ;
#74646 = CARTESIAN_POINT ( 'NONE',  ( -36.98821436528694306, 463.5274861635123216, 19.70078135306431477 ) ) ;
#74647 = VERTEX_POINT ( 'NONE', #85075 ) ;
#74648 = CARTESIAN_POINT ( 'NONE',  ( 92.56322867397322796, -59.99999999999999289, -10.69608963466881235 ) ) ;
#74649 = CARTESIAN_POINT ( 'NONE',  ( -9.646320399536650214, 46.21287003049852871, 13.08069908581821572 ) ) ;
#74650 = FILL_AREA_STYLE_COLOUR ( '', #84116 ) ;
#74651 = DIRECTION ( 'NONE',  ( 0.000000000000000000, -1.000000000000000000, 0.000000000000000000 ) ) ;
#74652 = CARTESIAN_POINT ( 'NONE',  ( -46.96293930799764382, 18.79139706470984805, -14.94845605815084255 ) ) ;
#74653 = VERTEX_POINT ( 'NONE', #75911 ) ;
#74654 = DIRECTION ( 'NONE',  ( 0.9090909090909091717, -7.226819671346018786E-16, 0.4165977904505309137 ) ) ;
#74655 = ORIENTED_EDGE ( 'NONE', *, *, #37418, .T. ) ;
#74656 = ORIENTED_EDGE ( 'NONE', *, *, #25695, .F. ) ;
#74657 = CARTESIAN_POINT ( 'NONE',  ( 34.16642289233210050, 463.8422268500519863, 18.98106911353328385 ) ) ;
#74658 = FACE_OUTER_BOUND ( 'NONE', #44169, .T. ) ;
#74659 = CARTESIAN_POINT ( 'NONE',  ( 0.06682554136337834350, 4.993536075455418555, -4.350941807883112133 ) ) ;
#74660 = DIRECTION ( 'NONE',  ( -1.000000000000000000, -1.224606353822377258E-16, -0.000000000000000000 ) ) ;
#74661 = CARTESIAN_POINT ( 'NONE',  ( 82.81677989675817741, -37.85377912558440983, 1.740399077028625063 ) ) ;
#74662 = CARTESIAN_POINT ( 'NONE',  ( -39.28789537393542020, 311.9693088241641021, 2.089465571748127637 ) ) ;
#74663 = CARTESIAN_POINT ( 'NONE',  ( -4.999999999999801048, -61.23402596802289111, 12.68529909296846370 ) ) ;
#74664 = ORIENTED_EDGE ( 'NONE', *, *, #86255, .T. ) ;
#74665 = FACE_OUTER_BOUND ( 'NONE', #19883, .T. ) ;
#74666 = EDGE_CURVE ( 'NONE', #11758, #33126, #26188, .T. ) ;
#74667 = VERTEX_POINT ( 'NONE', #17162 ) ;
#74668 = DIRECTION ( 'NONE',  ( -0.000000000000000000, -1.000000000000000000, -0.000000000000000000 ) ) ;
#74669 = CARTESIAN_POINT ( 'NONE',  ( -81.02582043684626001, -38.83538064993233263, 194.6489687308902887 ) ) ;
#74670 = LINE ( 'NONE', #753, #62769 ) ;
#74671 = AXIS2_PLACEMENT_3D ( 'NONE', #43820, #76713, #12504 ) ;
#74673 = ORIENTED_EDGE ( 'NONE', *, *, #77233, .F. ) ;
#74672 = CARTESIAN_POINT ( 'NONE',  ( -31.86600978156343444, -60.00000000000000000, 37.52812459344517748 ) ) ;
#74674 = CARTESIAN_POINT ( 'NONE',  ( 63.36932946075098272, -60.33828791889990129, 92.29599462647620101 ) ) ;
#74675 = VECTOR ( 'NONE', #46363, 999.9999999999998863 ) ;
#74676 = EDGE_LOOP ( 'NONE', ( #37576, #57662, #53694, #91875 ) ) ;
#74677 = CARTESIAN_POINT ( 'NONE',  ( 54.43501200703078524, 38.95383793069735390, -33.39731814189929082 ) ) ;
#74678 = ADVANCED_FACE ( 'NONE', ( #67825 ), #67564, .T. ) ;
#74679 = AXIS2_PLACEMENT_3D ( 'NONE', #61249, #45070, #77952 ) ;
#74680 = CARTESIAN_POINT ( 'NONE',  ( 5.082755093536324154, -26.84375000204838813, 5.082755093536326818 ) ) ;
#74681 = ADVANCED_FACE ( 'NONE', ( #10632 ), #17688, .T. ) ;
#74682 = CARTESIAN_POINT ( 'NONE',  ( -113.9602498558271719, -57.67115345197749576, 163.9892394128282262 ) ) ;
#74683 = VERTEX_POINT ( 'NONE', #66765 ) ;
#74684 = CARTESIAN_POINT ( 'NONE',  ( 19.50000000000000000, 12.99999999999999467, -7.500000000000000000 ) ) ;
#74685 = CARTESIAN_POINT ( 'NONE',  ( 101.8543654623573929, -37.84848643670019896, 184.8799554269737371 ) ) ;
#74686 = CARTESIAN_POINT ( 'NONE',  ( -37.83989825151990516, 491.6297408768480750, 12.44743998624971759 ) ) ;
#74687 = CARTESIAN_POINT ( 'NONE',  ( 0.000000000000000000, 0.000000000000000000, 22.55262289886175964 ) ) ;
#74688 = CARTESIAN_POINT ( 'NONE',  ( -3.313708498984760720, -24.21875000409677625, -8.000000000000000000 ) ) ;
#74689 = CARTESIAN_POINT ( 'NONE',  ( 8.000000000000000000, 9.797174393178825657E-16, -5.575057142857143155 ) ) ;
#74690 = CARTESIAN_POINT ( 'NONE',  ( 9.482945380845317018, 247.5566694122106242, 3.177595346755247796 ) ) ;
#74691 = EDGE_CURVE ( 'NONE', #89611, #17242, #101265, .T. ) ;
#74692 = CARTESIAN_POINT ( 'NONE',  ( 0.000000000000000000, 0.000000000000000000, -3.764187203485586330 ) ) ;
#74693 = CARTESIAN_POINT ( 'NONE',  ( 9.537291425704607306, 32.64404377332772356, 3.012810007365997578 ) ) ;
#74694 = CARTESIAN_POINT ( 'NONE',  ( -19.07845090537422550, 294.6331628770684574, 9.890526070132905190 ) ) ;
#74696 = AXIS2_PLACEMENT_3D ( 'NONE', #83319, #8894, #16460 ) ;
#74695 = FILL_AREA_STYLE_COLOUR ( '', #55829 ) ;
#74697 = CARTESIAN_POINT ( 'NONE',  ( -3.409011323176792896, 15.24615751665884744, -9.403185743875123848 ) ) ;
#74698 = VERTEX_POINT ( 'NONE', #26875 ) ;
#74699 = CARTESIAN_POINT ( 'NONE',  ( -7.000000000000000000, 8.572527594031471218E-16, -6.275264681066861527 ) ) ;
#74700 = DIRECTION ( 'NONE',  ( 0.000000000000000000, 0.000000000000000000, 1.000000000000000000 ) ) ;
#74701 = VECTOR ( 'NONE', #49344, 999.9999999999998863 ) ;
#74702 = CARTESIAN_POINT ( 'NONE',  ( -94.11789465525937715, -29.99999999999999289, 191.2872302807874689 ) ) ;
#74703 = MECHANICAL_DESIGN_GEOMETRIC_PRESENTATION_REPRESENTATION (  '', ( #104041 ), #47228 ) ;
#74704 = ORIENTED_EDGE ( 'NONE', *, *, #43376, .T. ) ;
#74705 = AXIS2_PLACEMENT_3D ( 'NONE', #93415, #28179, #4395 ) ;
#74706 = CARTESIAN_POINT ( 'NONE',  ( 38.81316105428458485, 25.21210130169110641, -12.01306034898426844 ) ) ;
#74707 = CARTESIAN_POINT ( 'NONE',  ( 62.06629429558737598, -57.67807194442349328, 114.8863211712005210 ) ) ;
#74709 = DIRECTION ( 'NONE',  ( 1.871721906610600077E-16, 0.000000000000000000, -1.000000000000000000 ) ) ;
#74708 = CARTESIAN_POINT ( 'NONE',  ( -0.7769499151835902451, 25.97800031865995862, -38.51735009866241910 ) ) ;
#74710 = ADVANCED_FACE ( 'NONE', ( #34434 ), #22765, .T. ) ;
#74711 = CARTESIAN_POINT ( 'NONE',  ( 23.88087707229235335, -27.28680826393994607, -38.40335539918089580 ) ) ;
#74712 = CARTESIAN_POINT ( 'NONE',  ( -0.08530053327169842547, 43.17555810750862122, 18.75000000000000000 ) ) ;
#74713 = DIRECTION ( 'NONE',  ( 0.000000000000000000, 0.000000000000000000, 1.000000000000000000 ) ) ;
#74714 = CARTESIAN_POINT ( 'NONE',  ( -29.24377091299251674, -60.00000000000000000, 42.67557265589431381 ) ) ;
#74715 = FACE_OUTER_BOUND ( 'NONE', #61627, .T. ) ;
#74716 = CARTESIAN_POINT ( 'NONE',  ( 5.456272071277679991, 53.44287117986112889, 8.531152949374478212 ) ) ;
#74717 = CARTESIAN_POINT ( 'NONE',  ( -87.17749325152986728, -39.07517086902483072, 189.3868324704938573 ) ) ;
#74718 = ORIENTED_EDGE ( 'NONE', *, *, #59344, .T. ) ;
#74719 = CARTESIAN_POINT ( 'NONE',  ( 8.515745267470094859, -14.14492484005115891, 15.87637050603546385 ) ) ;
#74720 = CARTESIAN_POINT ( 'NONE',  ( -7.006332439432221726, -22.06780448926463123, 27.55795484604703560 ) ) ;
#74721 = CARTESIAN_POINT ( 'NONE',  ( -6.542885568110277106, 41.77240995323538897, -59.03854211387476880 ) ) ;
#74722 = FACE_OUTER_BOUND ( 'NONE', #79468, .T. ) ;
#74723 = B_SPLINE_SURFACE_WITH_KNOTS ( 'NONE', 1, 3, ( 
 ( #43745, #93371, #36762, #61550, #94443, #52358, #50749, #83654, #9768, #75578, #2743, #35698, #1674, #34633, #97455, #80744, #48898, #32767, #86361, #30641, #53439, #65639, #32222, #105041, #88855, #56996, #31182, #65102 ),
 ( #96427, #24152, #71588, #81793, #106617, #105558, #23611, #63529, #89911, #81270, #22562, #16019, #56463, #96942, #31697, #97999, #55400, #7918, #64584, #40296, #89394, #40821, #15488, #73714, #48376, #20602, #12425, #39784 ) ),
 .UNSPECIFIED., .F., .F., .F.,
 ( 2, 2 ),
 ( 4, 2, 2, 2, 2, 2, 2, 2, 2, 2, 2, 2, 2, 4 ),
 ( 0.000000000000000000, 1.000000000000000000 ),
 ( 0.08901491201581737678, 0.1032490540155679704, 0.1174831960153185778, 0.1317173380150691853, 0.1459514800148197788, 0.1744197640143299588, 0.2028880480138401388, 0.2598246160128514504, 0.3167611840118632616, 0.4306343200098861623, 0.5445074560079088410, 0.6583805920059359051, 0.7722537280039543095, 1.000000000000000000 ),
 .UNSPECIFIED. ) ;
#74725 = EDGE_CURVE ( 'NONE', #39998, #28086, #43551, .T. ) ;
#74724 = CARTESIAN_POINT ( 'NONE',  ( 3.851852197295787317, -68.60299753987145266, 13.53085478509467166 ) ) ;
#74726 = VERTEX_POINT ( 'NONE', #102853 ) ;
#74728 =( NAMED_UNIT ( * ) SI_UNIT ( $, .STERADIAN. ) SOLID_ANGLE_UNIT ( ) );
#74727 = AXIS2_PLACEMENT_3D ( 'NONE', #88052, #72897, #48092 ) ;
#74729 = CARTESIAN_POINT ( 'NONE',  ( 0.000000000000000000, 0.000000000000000000, 5.000000000000002665 ) ) ;
#74730 = CARTESIAN_POINT ( 'NONE',  ( -7.800703710507059796, 33.58595692657940646, 1.791736796405271281 ) ) ;
#74731 = CARTESIAN_POINT ( 'NONE',  ( 28.36261055972402190, 306.0659664076646891, -9.283380716933603338 ) ) ;
#74732 = CARTESIAN_POINT ( 'NONE',  ( 0.000000000000000000, 0.000000000000000000, -13.00000000000000000 ) ) ;
#74733 = CARTESIAN_POINT ( 'NONE',  ( -6.928203230275508773, -84.73520732746429474, 4.000000000000000888 ) ) ;
#74734 = LINE ( 'NONE', #25723, #66895 ) ;
#74735 = CARTESIAN_POINT ( 'NONE',  ( 103.8765618273974951, -14.21045842199444209, 137.3601107225250360 ) ) ;
#74736 = VERTEX_POINT ( 'NONE', #36565 ) ;
#74737 = CARTESIAN_POINT ( 'NONE',  ( 35.11650669486618170, 4.000000000000003553, 4.898587196589414801E-16 ) ) ;
#74738 = DIRECTION ( 'NONE',  ( -1.000000000000000000, -0.000000000000000000, -0.000000000000000000 ) ) ;
#74739 = FILL_AREA_STYLE ('',( #65603 ) ) ;
#74740 = AXIS2_PLACEMENT_3D ( 'NONE', #54830, #89347, #103920 ) ;
#74741 = CARTESIAN_POINT ( 'NONE',  ( -36.41079454256560410, 485.4442866794553879, -3.629012552424295102 ) ) ;
#74742 = CARTESIAN_POINT ( 'NONE',  ( 2.955787000303736534, 53.34311400849869500, -5.000000000000000888 ) ) ;
#74743 = EDGE_CURVE ( 'NONE', #29175, #29666, #68212, .T. ) ;
#74744 = CARTESIAN_POINT ( 'NONE',  ( 43.10371592040115019, 462.6168321841718125, 4.970041475426357991 ) ) ;
#74745 = ORIENTED_EDGE ( 'NONE', *, *, #1355, .F. ) ;
#74746 = B_SPLINE_CURVE_WITH_KNOTS ( 'NONE', 3,
 ( #70711, #29753, #104659, #87963, #86910, #47476, #23238, #12980, #103602, #105199, #7019, #56076, #71229, #30811, #21656, #62627, #96584, #14044, #45908, #80373, #89018, #55556, #14570, #38365, #88492, #22718, #96053, #6486, #15114, #95515, #54492, #104125, #39417, #87437 ),
 .UNSPECIFIED., .F., .F.,
 ( 4, 2, 2, 2, 2, 2, 2, 2, 2, 2, 2, 2, 2, 2, 2, 2, 4 ),
 ( 0.01272238763756220956, 0.01351613129786392691, 0.01430987495816564425, 0.01510361861846736334, 0.01589736227876908242, 0.01669110593907079804, 0.01748484959937251712, 0.01827859325967423620, 0.01907233691997595182, 0.01986608058027766743, 0.02065982424057938652, 0.02145356790088110560, 0.02224731156118282122, 0.02304105522148454030, 0.02383479888178625938, 0.02462854254208797500, 0.02542228620238969408 ),
 .UNSPECIFIED. ) ;
#74747 = CIRCLE ( 'NONE', #12771, 0.9999999999999991118 ) ;
#74748 = DIRECTION ( 'NONE',  ( 0.000000000000000000, -1.000000000000000000, 0.000000000000000000 ) ) ;
#74749 = ORIENTED_EDGE ( 'NONE', *, *, #106198, .T. ) ;
#74750 = FACE_OUTER_BOUND ( 'NONE', #99506, .T. ) ;
#74752 = ADVANCED_FACE ( 'NONE', ( #53242 ), #17595, .T. ) ;
#74751 = CARTESIAN_POINT ( 'NONE',  ( 31.00808149270786274, 439.2166318629403463, 22.50860008698266057 ) ) ;
#74753 = CARTESIAN_POINT ( 'NONE',  ( 9.648094638230904962, 46.21279293231379626, 13.07965317076976319 ) ) ;
#74754 = CARTESIAN_POINT ( 'NONE',  ( 65.26738680890606759, 48.00000000000000000, 0.8120011905328435864 ) ) ;
#74755 = CARTESIAN_POINT ( 'NONE',  ( 5.000000000000039968, -14.06131484383594099, 13.29904837184988509 ) ) ;
#74756 = FACE_OUTER_BOUND ( 'NONE', #85232, .T. ) ;
#74757 = ORIENTED_EDGE ( 'NONE', *, *, #94422, .T. ) ;
#74758 = CARTESIAN_POINT ( 'NONE',  ( 102.0894480219289591, -59.99999999999998579, 201.1080374328564915 ) ) ;
#74760 = CARTESIAN_POINT ( 'NONE',  ( 13.42259877889314801, -35.99176036207357754, 29.96878892533495886 ) ) ;
#74759 = CARTESIAN_POINT ( 'NONE',  ( -100.5643661290868209, -60.00000000000009237, 204.3458358344470582 ) ) ;
#74762 = DIRECTION ( 'NONE',  ( 0.000000000000000000, 0.000000000000000000, 1.000000000000000000 ) ) ;
#74761 = PRODUCT_DEFINITION_CONTEXT ( 'detailed design', #50704, 'design' ) ;
#74763 = CARTESIAN_POINT ( 'NONE',  ( 74.56127108291157413, 6.975173280561618775E-15, 0.000000000000000000 ) ) ;
#74764 = CARTESIAN_POINT ( 'NONE',  ( -40.33367101206530947, -42.97933796220600300, 39.77954886268002355 ) ) ;
#74765 = CARTESIAN_POINT ( 'NONE',  ( -36.90124019533217137, 18.64284798593122616, 10.73407659158960747 ) ) ;
#74766 = ORIENTED_EDGE ( 'NONE', *, *, #5143, .T. ) ;
#74767 = CARTESIAN_POINT ( 'NONE',  ( -21.88880945939638778, -4.285714285714296246, 12.64023069600373717 ) ) ;
#74768 = CARTESIAN_POINT ( 'NONE',  ( 7.800296835061319989, 54.21723526805532600, 1.774124769967747595 ) ) ;
#74769 = CARTESIAN_POINT ( 'NONE',  ( 31.21759734847655210, 387.2566916973277671, 24.99345285570965913 ) ) ;
#74770 = FACE_OUTER_BOUND ( 'NONE', #70565, .T. ) ;
#74771 = CARTESIAN_POINT ( 'NONE',  ( 6.463344223170841119, 7.245769408789096033, 1.129975644293424120 ) ) ;
#74772 = CARTESIAN_POINT ( 'NONE',  ( -30.00000000000000355, 487.5660443506044999, 6.762394459359180487 ) ) ;
#74773 = ORIENTED_EDGE ( 'NONE', *, *, #99200, .F. ) ;
#74774 = DIRECTION ( 'NONE',  ( 0.000000000000000000, -1.000000000000000000, 0.000000000000000000 ) ) ;
#74775 = CARTESIAN_POINT ( 'NONE',  ( -4.000000000000002665, 0.000000000000000000, -7.974599999999995248 ) ) ;
#74776 = VERTEX_POINT ( 'NONE', #103382 ) ;
#74777 = CARTESIAN_POINT ( 'NONE',  ( 71.80342808059910453, -30.00000000000000000, -19.71766482350837535 ) ) ;
#74778 = DIRECTION ( 'NONE',  ( -0.000000000000000000, -1.000000000000000000, -0.000000000000000000 ) ) ;
#74780 = EDGE_CURVE ( 'NONE', #29420, #96657, #74384, .T. ) ;
#74779 = CIRCLE ( 'NONE', #28324, 3.309500000000007880 ) ;
#74781 = CARTESIAN_POINT ( 'NONE',  ( 24.46392420078501218, 25.31575836906371890, -32.08127962606481987 ) ) ;
#74782 = FACE_OUTER_BOUND ( 'NONE', #28307, .T. ) ;
#74783 = CARTESIAN_POINT ( 'NONE',  ( 82.12584806139965110, -30.00000000000000000, 35.18806641379789824 ) ) ;
#74784 = CIRCLE ( 'NONE', #7634, 8.000000000000000000 ) ;
#74785 = CARTESIAN_POINT ( 'NONE',  ( 7.801339272325196639, 101.4126852804029966, -1.788609912539668834 ) ) ;
#74786 = ORIENTED_EDGE ( 'NONE', *, *, #48465, .F. ) ;
#74787 = AXIS2_PLACEMENT_3D ( 'NONE', #30162, #24072, #17022 ) ;
#74788 = EDGE_LOOP ( 'NONE', ( #20665, #4426, #53214, #6040 ) ) ;
#74789 = ORIENTED_EDGE ( 'NONE', *, *, #67199, .F. ) ;
#74790 = CARTESIAN_POINT ( 'NONE',  ( 82.70911704725124025, -2.002967142162725287E-29, 5.000000000000011546 ) ) ;
#74791 = CARTESIAN_POINT ( 'NONE',  ( -6.642722259512091831, 41.46658730094534917, -70.60825968550385312 ) ) ;
#74792 = CARTESIAN_POINT ( 'NONE',  ( -38.06223451516787293, 464.2386140055725718, 19.21930428800968471 ) ) ;
#74793 = CARTESIAN_POINT ( 'NONE',  ( -31.36907691194473813, 433.8632848466868381, 23.03436070161451710 ) ) ;
#74794 = VERTEX_POINT ( 'NONE', #79621 ) ;
#74795 = CARTESIAN_POINT ( 'NONE',  ( 9.646083234704169840, 108.0129060902347646, -2.643797197754291783 ) ) ;
#74796 = ORIENTED_EDGE ( 'NONE', *, *, #70621, .F. ) ;
#74797 = DIRECTION ( 'NONE',  ( 0.000000000000000000, -1.000000000000000000, 0.000000000000000000 ) ) ;
#74798 = CARTESIAN_POINT ( 'NONE',  ( 76.76261672097879796, -38.43742884780580482, 183.2131921944575765 ) ) ;
#74799 = CARTESIAN_POINT ( 'NONE',  ( 5.819846122303830249, 4.937269551422627245, -4.448398286273205215 ) ) ;
#74800 = CARTESIAN_POINT ( 'NONE',  ( 33.01607209031806178, 301.6304077285213907, 11.48551711194975766 ) ) ;
#74801 = DIRECTION ( 'NONE',  ( 0.000000000000000000, 1.000000000000000000, 0.000000000000000000 ) ) ;
#74802 = B_SPLINE_CURVE_WITH_KNOTS ( 'NONE', 3,
 ( #20738, #94033, #44426, #68717, #101600, #36898, #61145, #77322 ),
 .UNSPECIFIED., .F., .F.,
 ( 4, 2, 2, 4 ),
 ( 0.000000000000000000, 0.5000000000000000000, 0.7500000000000000000, 1.000000000000000000 ),
 .UNSPECIFIED. ) ;
#74803 = CARTESIAN_POINT ( 'NONE',  ( -41.50820411079211425, 461.5963371455321180, 2.703439750996433855 ) ) ;
#74804 = CARTESIAN_POINT ( 'NONE',  ( 0.000000000000000000, 0.000000000000000000, -7.000000000000011546 ) ) ;
#74805 = EDGE_CURVE ( 'NONE', #89689, #234, #106783, .T. ) ;
#74806 = CYLINDRICAL_SURFACE ( 'NONE', #51397, 4.000000000000000000 ) ;
#74807 = CARTESIAN_POINT ( 'NONE',  ( -4.921335115252323256, 6.865562341691512138, 5.000000000000000000 ) ) ;
#74808 = EDGE_LOOP ( 'NONE', ( #41631, #38773, #106618 ) ) ;
#74809 = CARTESIAN_POINT ( 'NONE',  ( -24.97007374329429652, 295.7209793996028111, 10.12394817307690786 ) ) ;
#74810 = DIRECTION ( 'NONE',  ( 0.000000000000000000, 0.000000000000000000, 1.000000000000000000 ) ) ;
#74811 = DIRECTION ( 'NONE',  ( 0.000000000000000000, -1.000000000000000000, 0.000000000000000000 ) ) ;
#74812 = CARTESIAN_POINT ( 'NONE',  ( 0.000000000000000000, 0.000000000000000000, 0.000000000000000000 ) ) ;
#74813 = CARTESIAN_POINT ( 'NONE',  ( 33.67444716837015761, 489.3309112354451713, 10.55021651976789521 ) ) ;
#74814 = EDGE_CURVE ( 'NONE', #80953, #100791, #8944, .T. ) ;
#74815 = CARTESIAN_POINT ( 'NONE',  ( 4.395101463923444918, 299.0276004806994479, 8.996626958117586170 ) ) ;
#74816 = AXIS2_PLACEMENT_3D ( 'NONE', #81176, #14848, #64490 ) ;
#74817 = CIRCLE ( 'NONE', #42099, 6.499999999999999112 ) ;
#74818 = DIRECTION ( 'NONE',  ( -1.000000000000000000, -1.224606353822377258E-16, -0.000000000000000000 ) ) ;
#74819 = APPLICATION_CONTEXT ( 'automotive_design' ) ;
#74820 = CARTESIAN_POINT ( 'NONE',  ( 84.39583363381976255, -57.44525944421299357, 191.2968279531777398 ) ) ;
#74821 = DIRECTION ( 'NONE',  ( 0.000000000000000000, -1.000000000000000000, 0.000000000000000000 ) ) ;
#74822 = ORIENTED_EDGE ( 'NONE', *, *, #13536, .F. ) ;
#74823 = AXIS2_PLACEMENT_3D ( 'NONE', #91781, #32501, #73980 ) ;
#74824 = CARTESIAN_POINT ( 'NONE',  ( 91.48089852627707330, -57.66238869088599728, -20.18956347066234258 ) ) ;
#74825 = CARTESIAN_POINT ( 'NONE',  ( 0.000000000000000000, -30.00000000000000000, 0.000000000000000000 ) ) ;
#74826 = CARTESIAN_POINT ( 'NONE',  ( 16.12458315221519811, 34.43091553126765803, -24.15015252360366205 ) ) ;
#74827 = DIRECTION ( 'NONE',  ( 0.000000000000000000, 0.000000000000000000, -1.000000000000000000 ) ) ;
#74828 = CARTESIAN_POINT ( 'NONE',  ( -80.99455166116037219, -30.00000000000000711, 4.108193232890078761 ) ) ;
#74829 = DIRECTION ( 'NONE',  ( 0.000000000000000000, -0.5000000000000009992, -0.8660254037844380415 ) ) ;
#74830 = CARTESIAN_POINT ( 'NONE',  ( 21.96335563855636863, 28.05277650238786080, -31.83030418064933897 ) ) ;
#74831 = CYLINDRICAL_SURFACE ( 'NONE', #89409, 7.000000000000006217 ) ;
#74833 = CARTESIAN_POINT ( 'NONE',  ( -18.99999999999999289, 5.000000000000000888, -1.500000000000001332 ) ) ;
#74832 = CARTESIAN_POINT ( 'NONE',  ( 0.4033376246892471650, 4.059728990630802947, 5.968343123267131567 ) ) ;
#74834 = EDGE_CURVE ( 'NONE', #61960, #79974, #5187, .T. ) ;
#74835 = CARTESIAN_POINT ( 'NONE',  ( -17.49999999999997158, 48.72924342453988089, 64.08323380050735807 ) ) ;
#74836 = CARTESIAN_POINT ( 'NONE',  ( 10.11650669486618881, 1.474610560812782335E-15, 0.000000000000000000 ) ) ;
#74837 = CARTESIAN_POINT ( 'NONE',  ( -12.49999999999999822, -4.999999999999999112, -34.12705337364893410 ) ) ;
#74838 = DIRECTION ( 'NONE',  ( 0.000000000000000000, 0.000000000000000000, -1.000000000000000000 ) ) ;
#74839 = CARTESIAN_POINT ( 'NONE',  ( -23.05266710533800278, 25.28705973898638959, 33.20617127781060418 ) ) ;
#74840 = DIRECTION ( 'NONE',  ( 0.000000000000000000, 1.000000000000000000, 0.000000000000000000 ) ) ;
#74841 = CARTESIAN_POINT ( 'NONE',  ( 71.80342808059909032, -30.00000000000000000, -19.71766482350836469 ) ) ;
#74842 = TOROIDAL_SURFACE ( 'NONE', #33539, 5.999999999999996447, 4.000000000000000000 ) ;
#74843 = ORIENTED_EDGE ( 'NONE', *, *, #94998, .F. ) ;
#74844 = FACE_OUTER_BOUND ( 'NONE', #44740, .T. ) ;
#74845 = CARTESIAN_POINT ( 'NONE',  ( 1.054315034361395842, 21.72038501719248060, 6.925105097140866306 ) ) ;
#74846 = CARTESIAN_POINT ( 'NONE',  ( -52.81788617984520329, -28.08527092621403298, -27.21337244879998707 ) ) ;
#74847 = CIRCLE ( 'NONE', #28412, 4.000000000000001776 ) ;
#74850 = ADVANCED_FACE ( 'NONE', ( #5739 ), #62407, .T. ) ;
#74849 = FACE_OUTER_BOUND ( 'NONE', #46036, .T. ) ;
#74848 = CARTESIAN_POINT ( 'NONE',  ( 39.34999999999999432, 1.533819458162526451E-15, 0.000000000000000000 ) ) ;
#74851 = ORIENTED_EDGE ( 'NONE', *, *, #29868, .F. ) ;
#74852 = ORIENTED_EDGE ( 'NONE', *, *, #80100, .F. ) ;
#74853 = DIRECTION ( 'NONE',  ( -0.000000000000000000, -1.000000000000000000, -0.000000000000000000 ) ) ;
#74854 = CARTESIAN_POINT ( 'NONE',  ( 39.83456023769738863, 489.3941229067897325, 11.44194699760926603 ) ) ;
#74855 = CARTESIAN_POINT ( 'NONE',  ( -19.50000000000000000, 12.99999999999999289, 0.000000000000000000 ) ) ;
#74856 = CARTESIAN_POINT ( 'NONE',  ( -18.14215405046660834, -60.00000000000000000, -41.96107740640177042 ) ) ;
#74857 = ORIENTED_EDGE ( 'NONE', *, *, #91013, .F. ) ;
#74858 = CARTESIAN_POINT ( 'NONE',  ( 15.35683281173218973, 2.987586243233406602, 2.780571802877160881 ) ) ;
#74859 = CARTESIAN_POINT ( 'NONE',  ( 101.7724625413487018, -52.72604442183713758, 192.4186900641388434 ) ) ;
#74861 = CARTESIAN_POINT ( 'NONE',  ( -0.01431428620034891179, -57.67120202577072519, -44.61186648040676772 ) ) ;
#74860 = DIRECTION ( 'NONE',  ( 0.000000000000000000, 0.000000000000000000, 1.000000000000000000 ) ) ;
#74862 = VERTEX_POINT ( 'NONE', #52691 ) ;
#74863 = VERTEX_POINT ( 'NONE', #4693 ) ;
#74864 = ORIENTED_EDGE ( 'NONE', *, *, #35218, .T. ) ;
#74865 = CARTESIAN_POINT ( 'NONE',  ( 31.22086979617878910, 398.3983149021029249, 25.40418687235769113 ) ) ;
#74866 = ADVANCED_FACE ( 'NONE', ( #101783 ), #44629, .T. ) ;
#74867 = CARTESIAN_POINT ( 'NONE',  ( -13.50000000000000178, 2.646256834279085979, -12.86070865178833600 ) ) ;
#74868 = CARTESIAN_POINT ( 'NONE',  ( 16.64348903516499334, 45.60392139269944067, 6.657797401562596917 ) ) ;
#74869 = ORIENTED_EDGE ( 'NONE', *, *, #12261, .T. ) ;
#74870 = CONICAL_SURFACE ( 'NONE', #76576, 3.309500000000007880, 0.9599310885968770357 ) ;
#74871 = DIRECTION ( 'NONE',  ( 1.000000000000000000, 1.224606353822377258E-16, 0.000000000000000000 ) ) ;
#74872 = CARTESIAN_POINT ( 'NONE',  ( 6.326445470157509909, 5.253846677262518305, 4.563138989068574958 ) ) ;
#74873 = CARTESIAN_POINT ( 'NONE',  ( 43.52075891743746894, 484.7805561108181109, 4.063293749111048569 ) ) ;
#74874 = CARTESIAN_POINT ( 'NONE',  ( 1.494050070974696619E-08, -60.00000000000000711, -44.99999999996101252 ) ) ;
#74875 = CARTESIAN_POINT ( 'NONE',  ( 5.082755093536325930, -33.96875000204838813, -5.082755093536325042 ) ) ;
#74876 = CARTESIAN_POINT ( 'NONE',  ( -30.04234920459634495, 13.07620473719203602, 42.05403970751757470 ) ) ;
#74877 = FACE_BOUND ( 'NONE', #59163, .T. ) ;
#74878 = CARTESIAN_POINT ( 'NONE',  ( -6.828042834505471781, 41.63841151066672808, -58.95291702778770571 ) ) ;
#74879 = CARTESIAN_POINT ( 'NONE',  ( -86.74711523299461646, -14.21045842199446518, 20.03206905870895227 ) ) ;
#74880 = EDGE_CURVE ( 'NONE', #35260, #105857, #62402, .T. ) ;
#74881 = CARTESIAN_POINT ( 'NONE',  ( 13.09999999999999787, -3.309499999999999886, 0.000000000000000000 ) ) ;
#74882 = CARTESIAN_POINT ( 'NONE',  ( -50.52096995421375425, -49.90828412712392748, 55.20216876667482353 ) ) ;
#74883 = DIRECTION ( 'NONE',  ( 1.000000000000000000, 1.224606353822377258E-16, 0.000000000000000000 ) ) ;
#74884 = ORIENTED_EDGE ( 'NONE', *, *, #59223, .T. ) ;
#74885 = CIRCLE ( 'NONE', #42182, 5.000000000000000000 ) ;
#74886 = CARTESIAN_POINT ( 'NONE',  ( 35.68327731609498699, 437.0250969216240264, 4.635559385101182706 ) ) ;
#74887 = VECTOR ( 'NONE', #44549, 1000.000000000000227 ) ;
#74888 = CARTESIAN_POINT ( 'NONE',  ( -2.469322996728156472, 298.9266300818543414, -10.00398374146220171 ) ) ;
#74889 = CARTESIAN_POINT ( 'NONE',  ( 0.000000000000000000, 43.50000000000000711, 0.000000000000000000 ) ) ;
#74890 = EDGE_LOOP ( 'NONE', ( #98010, #99556, #14282, #25797 ) ) ;
#74891 = CARTESIAN_POINT ( 'NONE',  ( 4.472135954999577834, 249.7292277993263383, 4.000000000000005329 ) ) ;
#74892 = CONICAL_SURFACE ( 'NONE', #21592, 4.172000000000009479, 0.9599310885968813656 ) ;
#74893 = CARTESIAN_POINT ( 'NONE',  ( 101.8192011966949337, -38.44775644747127075, 199.7746753136944449 ) ) ;
#74894 = CARTESIAN_POINT ( 'NONE',  ( 48.49215721461877848, 15.66554462475086495, 14.43870166537688249 ) ) ;
#74895 = DIRECTION ( 'NONE',  ( -1.000000000000000000, -1.224606353822377258E-16, -0.000000000000000000 ) ) ;
#74896 = EDGE_CURVE ( 'NONE', #93010, #84586, #37091, .T. ) ;
#74897 = CARTESIAN_POINT ( 'NONE',  ( -17.64534493868312026, 294.6036102501091705, 9.884244339924812550 ) ) ;
#74898 = CIRCLE ( 'NONE', #30138, 0.9999999999999997780 ) ;
#74899 = CARTESIAN_POINT ( 'NONE',  ( -88.20421627925426833, 42.00000000000000000, -23.70422451879017345 ) ) ;
#74900 = CARTESIAN_POINT ( 'NONE',  ( 91.51571527023273234, -30.00000000000001066, 190.6995551984874737 ) ) ;
#74901 = CARTESIAN_POINT ( 'NONE',  ( 37.67950550371620722, 491.6872717898539236, 12.48612654750107964 ) ) ;
#74902 = CARTESIAN_POINT ( 'NONE',  ( -28.56401049668894032, 13.37477103922272192, 40.29034081819133917 ) ) ;
#74903 = CARTESIAN_POINT ( 'NONE',  ( -10.00000000000000000, 0.000000000000000000, 10.00000000000000000 ) ) ;
#74904 = B_SPLINE_CURVE_WITH_KNOTS ( 'NONE', 3,
 ( #62820, #95713, #56130, #66926, #91731, #59372, #1075, #24883 ),
 .UNSPECIFIED., .F., .F.,
 ( 4, 2, 2, 4 ),
 ( 4.429863980152083197E-29, 0.01011967574619566934, 0.01517951361929350575, 0.02023935149239133868 ),
 .UNSPECIFIED. ) ;
#74905 = VERTEX_POINT ( 'NONE', #87208 ) ;
#74906 = ORIENTED_EDGE ( 'NONE', *, *, #65291, .F. ) ;
#74907 = CARTESIAN_POINT ( 'NONE',  ( 52.40231891019367083, -53.37153954349100360, 60.21125311485567977 ) ) ;
#74908 = CARTESIAN_POINT ( 'NONE',  ( 6.784953749580444615, 41.67963532863181797, -59.00226812211813154 ) ) ;
#74909 = CARTESIAN_POINT ( 'NONE',  ( 37.40778227969215664, 27.94108768513336472, -10.95617127781084399 ) ) ;
#74910 = ORIENTED_EDGE ( 'NONE', *, *, #67614, .F. ) ;
#74911 = CARTESIAN_POINT ( 'NONE',  ( -99.53716699256776224, -38.35579409513464100, 85.73697495571477134 ) ) ;
#74912 = VERTEX_POINT ( 'NONE', #20927 ) ;
#74913 = CARTESIAN_POINT ( 'NONE',  ( 15.79261075262969527, 4.810720122700525181, 5.431533035173099044 ) ) ;
#74914 = CARTESIAN_POINT ( 'NONE',  ( 98.49355459790156431, -38.35583652005738742, 79.56885252902853267 ) ) ;
#74915 = CARTESIAN_POINT ( 'NONE',  ( 14.42176108926845757, 21.45314454056250142, -5.349682917995179032 ) ) ;
#74916 = CARTESIAN_POINT ( 'NONE',  ( 91.54334141914280565, -37.84851935321219685, 87.62289096787682752 ) ) ;
#74917 = CARTESIAN_POINT ( 'NONE',  ( -31.48659109300052350, 438.9656692063605306, 23.23080034282737927 ) ) ;
#74918 = CARTESIAN_POINT ( 'NONE',  ( -0.3365330672310704596, 46.20030378422329420, -16.28442818836915862 ) ) ;
#74919 = CARTESIAN_POINT ( 'NONE',  ( -31.19706370536868434, 315.2691834397311368, -6.507072380722979332 ) ) ;
#74920 = CARTESIAN_POINT ( 'NONE',  ( 4.363347285238665663, -66.51195625152190871, 13.14303842901982122 ) ) ;
#74921 =( BOUNDED_SURFACE ( )  B_SPLINE_SURFACE ( 3, 2, ( 
 ( #22975, #56886, #31081 ),
 ( #6215, #96847, #73063 ),
 ( #15380, #72032, #89813 ),
 ( #47209, #14840, #97890 ),
 ( #13777, #81167, #80636 ),
 ( #23506, #63960, #40185 ),
 ( #56350, #15913, #96327 ),
 ( #72553, #22454, #73602 ),
 ( #48791, #62893, #14305 ),
 ( #80111, #104386, #30536 ) ),
 .UNSPECIFIED., .F., .F., .F. ) 
 B_SPLINE_SURFACE_WITH_KNOTS ( ( 4, 2, 2, 2, 4 ),
 ( 3, 3 ),
 ( 0.007162312563335121278, 0.008169815727932031035, 0.009177318892528939925, 0.01018482205712584882, 0.01119232522172275771 ),
 ( 0.000000000000000000, 0.8513194332817035637 ),
 .UNSPECIFIED. ) 
 GEOMETRIC_REPRESENTATION_ITEM ( )  RATIONAL_B_SPLINE_SURFACE ( (
 ( 1.000000000000000000, 0.7967391679699951101, 0.9395581286042928859),
 ( 1.000000000000000000, 0.8061132416517035049, 0.9423456137792036724),
 ( 1.000000000000000000, 0.8123079594501175782, 0.9441876820850600982),
 ( 1.000000000000000000, 0.8173936710915957748, 0.9456999750631016610),
 ( 1.000000000000000000, 0.8162642092137375460, 0.9453641169989284165),
 ( 1.000000000000000000, 0.8072284251113268638, 0.9426772259967470813),
 ( 1.000000000000000000, 0.7993563690608861405, 0.9403363824871115995),
 ( 1.000000000000000000, 0.7784392998177147582, 0.9341164590687904834),
 ( 1.000000000000000000, 0.7654114976929390357, 0.9302424970627795053),
 ( 1.000000000000000000, 0.7506543109476874198, 0.9258542832858760452) ) ) 
 REPRESENTATION_ITEM ( '' )  SURFACE ( )  );
#74922 = CARTESIAN_POINT ( 'NONE',  ( 73.95865299267170201, -59.99999999999999289, 171.8011999975828417 ) ) ;
#74923 = CARTESIAN_POINT ( 'NONE',  ( -2.500000000000001332, -15.46059980043578541, 23.70577374505222679 ) ) ;
#74924 = CIRCLE ( 'NONE', #21548, 0.5000000000000004441 ) ;
#74925 = DIRECTION ( 'NONE',  ( 1.000000000000000000, 1.224606353822377258E-16, 0.000000000000000000 ) ) ;
#74926 = ORIENTED_EDGE ( 'NONE', *, *, #91001, .T. ) ;
#74927 = CARTESIAN_POINT ( 'NONE',  ( 62.44672187089501847, -42.95944451888637161, 80.58943253863333211 ) ) ;
#74928 = CARTESIAN_POINT ( 'NONE',  ( -29.06849802192348875, 297.2210473627602028, -1.482792297568717776 ) ) ;
#74929 = ADVANCED_FACE ( 'NONE', ( #53761 ), #31394, .T. ) ;
#74930 = CARTESIAN_POINT ( 'NONE',  ( 16.08349330513380337, -4.000000000000000000, 4.898587196589415787E-16 ) ) ;
#74931 = AXIS2_PLACEMENT_3D ( 'NONE', #87150, #79042, #37564 ) ;
#74932 = CARTESIAN_POINT ( 'NONE',  ( -7.890153520192944470, -5.000000000000000000, -15.80729722286742067 ) ) ;
#74934 = CARTESIAN_POINT ( 'NONE',  ( -4.151304510089519617, 54.24136489722235410, 6.759182313523147911 ) ) ;
#74933 = CARTESIAN_POINT ( 'NONE',  ( -75.43382409620862461, -30.00000000032916958, 160.3244271219596726 ) ) ;
#74935 = CARTESIAN_POINT ( 'NONE',  ( -31.72164027590077140, 329.7834567237236456, 16.51415323402584434 ) ) ;
#74936 = LINE ( 'NONE', #42580, #72539 ) ;
#74937 = FILL_AREA_STYLE_COLOUR ( '', #97194 ) ;
#74938 = CARTESIAN_POINT ( 'NONE',  ( 8.000000000000000000, -25.90624999999999645, -3.313708498984761608 ) ) ;
#74939 = CARTESIAN_POINT ( 'NONE',  ( -7.996668422906619611, -3.000000000000002665, -78.85453279917568636 ) ) ;
#74940 = EDGE_CURVE ( 'NONE', #66555, #19188, #26250, .T. ) ;
#74941 = B_SPLINE_CURVE_WITH_KNOTS ( 'NONE', 3,
 ( #77179, #58882, #43219, #11354, #76102, #18433 ),
 .UNSPECIFIED., .F., .F.,
 ( 4, 2, 4 ),
 ( 2.322283588913139083E-15, 0.01115492851740942232, 0.02230985703481652010 ),
 .UNSPECIFIED. ) ;
#74942 = CARTESIAN_POINT ( 'NONE',  ( -9.500000000000003553, -5.000000000000000000, -68.91429205785459544 ) ) ;
#74943 = ORIENTED_EDGE ( 'NONE', *, *, #87460, .T. ) ;
#74944 = CARTESIAN_POINT ( 'NONE',  ( 83.96313902567902687, -39.44727629013741677, 178.0741200447442054 ) ) ;
#74945 = CARTESIAN_POINT ( 'NONE',  ( 1.000000000000000222, -5.000000000000000000, -14.14213562373095101 ) ) ;
#74946 = AXIS2_PLACEMENT_3D ( 'NONE', #44626, #62399, #70485 ) ;
#74947 = DIRECTION ( 'NONE',  ( 0.5735764363510468256, 0.8191520442889913545, 0.000000000000000000 ) ) ;
#74948 = EDGE_LOOP ( 'NONE', ( #23540, #47472, #92240, #89744 ) ) ;
#74949 = DIRECTION ( 'NONE',  ( -1.000000000000000000, -0.000000000000000000, -0.000000000000000000 ) ) ;
#74950 = CARTESIAN_POINT ( 'NONE',  ( 42.80559098686211428, 434.8801202229377623, 8.726134940903639503 ) ) ;
#74951 = CARTESIAN_POINT ( 'NONE',  ( 0.000000000000000000, 15.00000000000000000, 0.000000000000000000 ) ) ;
#74952 = CARTESIAN_POINT ( 'NONE',  ( -2.751706330279349633, -3.000000000000002665, -100.0000000000000000 ) ) ;
#74953 = CARTESIAN_POINT ( 'NONE',  ( -13.94654863431429348, -23.74387561856928031, -38.53487845396338685 ) ) ;
#74954 = CARTESIAN_POINT ( 'NONE',  ( -12.24137076217897757, -2.657276045107078932, 20.68757701188024356 ) ) ;
#74955 = CONICAL_SURFACE ( 'NONE', #11200, 3.309500000000001663, 0.9599310885968770357 ) ;
#74956 = CARTESIAN_POINT ( 'NONE',  ( 53.11837506377438700, -60.00000000000000711, 79.96834070773113012 ) ) ;
#74957 = DIRECTION ( 'NONE',  ( -1.000000000000000000, -1.224606353822377258E-16, -0.000000000000000000 ) ) ;
#74958 = CARTESIAN_POINT ( 'NONE',  ( 9.531068631029500082, -13.65597988659789763, 31.91744325619306366 ) ) ;
#74960 = CARTESIAN_POINT ( 'NONE',  ( -13.02750095097563587, 21.68772054867059751, -4.979202728191992833 ) ) ;
#74959 = CARTESIAN_POINT ( 'NONE',  ( -16.64300274584347861, -23.63378944864288300, 36.18542074223226734 ) ) ;
#74961 = CARTESIAN_POINT ( 'NONE',  ( -1.469576158976823947E-15, -15.87499999999999289, 8.000000000000000000 ) ) ;
#74962 = CARTESIAN_POINT ( 'NONE',  ( -5.082755093536326818, -10.71875000204838457, 5.082755093536325042 ) ) ;
#74963 = FILL_AREA_STYLE ('',( #35088 ) ) ;
#74964 = CONICAL_SURFACE ( 'NONE', #26845, 4.172000000000009479, 0.9599310885968813656 ) ;
#74965 = STYLED_ITEM ( 'NONE', ( #42112 ), #56276 ) ;
#74966 = DIRECTION ( 'NONE',  ( -1.000000000000000000, -1.224606353822377258E-16, -0.000000000000000000 ) ) ;
#74967 = AXIS2_PLACEMENT_3D ( 'NONE', #69326, #53655, #28351 ) ;
#74968 = EDGE_LOOP ( 'NONE', ( #102002, #53589, #89991, #51585 ) ) ;
#74969 = CONICAL_SURFACE ( 'NONE', #23363, 4.000000000000007105, 0.9599310885968835860 ) ;
#74970 = CARTESIAN_POINT ( 'NONE',  ( -19.13866731017106204, 49.71730248559588006, 61.67331676225234105 ) ) ;
#74971 = CARTESIAN_POINT ( 'NONE',  ( -15.94126187130347816, -2.914874698625427030, 14.71615789485484527 ) ) ;
#74972 = STYLED_ITEM ( 'NONE', ( #104683 ), #13822 ) ;
#74973 = CARTESIAN_POINT ( 'NONE',  ( 37.29743189577540363, 437.4067884073982100, 4.451016994670380811 ) ) ;
#74975 = CARTESIAN_POINT ( 'NONE',  ( 38.30684875469531647, -47.40885643735987998, -31.93458248487312545 ) ) ;
#74974 = DIRECTION ( 'NONE',  ( -0.5735764363510497121, 0.8191520442889892450, 1.003171929053521665E-16 ) ) ;
#74976 = EDGE_LOOP ( 'NONE', ( #67123, #88450, #37559, #71092, #26931 ) ) ;
#74977 = CYLINDRICAL_SURFACE ( 'NONE', #61917, 9.500000000000000000 ) ;
#74978 = ORIENTED_EDGE ( 'NONE', *, *, #27606, .F. ) ;
#74979 = PRESENTATION_STYLE_ASSIGNMENT (( #83091 ) ) ;
#74980 = CARTESIAN_POINT ( 'NONE',  ( 20.00100000000000477, 12.99999999999999289, 0.000000000000000000 ) ) ;
#74981 = CARTESIAN_POINT ( 'NONE',  ( -24.58887437406745491, 41.57629742064543166, -73.51403340649437723 ) ) ;
#74982 = CARTESIAN_POINT ( 'NONE',  ( -102.3610540385565173, -59.99999999999999289, 94.85075420443190808 ) ) ;
#74983 = CYLINDRICAL_SURFACE ( 'NONE', #89321, 10.00000000000000178 ) ;
#74984 = CARTESIAN_POINT ( 'NONE',  ( 0.000000000000000000, -0.5000000000000000000, 8.000000000000000000 ) ) ;
#74985 = CARTESIAN_POINT ( 'NONE',  ( 0.000000000000000000, -0.5000000000000000000, 0.000000000000000000 ) ) ;
#74986 = CARTESIAN_POINT ( 'NONE',  ( 41.70256300459691090, 461.0340457114389778, 3.032228049028132588 ) ) ;
#74988 = CARTESIAN_POINT ( 'NONE',  ( 19.83349330513379982, -4.000000000000000888, 4.898587196589416773E-16 ) ) ;
#74987 = CARTESIAN_POINT ( 'NONE',  ( 9.999999999999994671, -3.000000000000002665, -86.30899693747679180 ) ) ;
#74989 = CARTESIAN_POINT ( 'NONE',  ( -80.94085204086121621, -60.50534541559768797, 182.8664948990503660 ) ) ;
#74990 = VERTEX_POINT ( 'NONE', #88265 ) ;
#74991 = ORIENTED_EDGE ( 'NONE', *, *, #15864, .F. ) ;
#74992 =( GEOMETRIC_REPRESENTATION_CONTEXT ( 3 ) GLOBAL_UNCERTAINTY_ASSIGNED_CONTEXT ( ( #27616 ) ) GLOBAL_UNIT_ASSIGNED_CONTEXT ( ( #65958, #7706, #72969 ) ) REPRESENTATION_CONTEXT ( 'NONE', 'WORKASPACE' ) );
#74993 = VERTEX_POINT ( 'NONE', #65567 ) ;
#74994 = CYLINDRICAL_SURFACE ( 'NONE', #61313, 4.000000000000002665 ) ;
#74995 = EDGE_CURVE ( 'NONE', #94269, #45028, #1318, .T. ) ;
#74996 = CARTESIAN_POINT ( 'NONE',  ( 42.19180677453719142, 462.2931784592651638, 3.389262873192005809 ) ) ;
#74997 = ORIENTED_EDGE ( 'NONE', *, *, #57883, .F. ) ;
#74998 = DIRECTION ( 'NONE',  ( 1.000000000000000000, 0.000000000000000000, 0.000000000000000000 ) ) ;
#74999 = EDGE_CURVE ( 'NONE', #86218, #96995, #15417, .T. ) ;
#75000 = DIRECTION ( 'NONE',  ( 0.000000000000000000, -1.000000000000000000, 0.000000000000000000 ) ) ;
#75001 = CARTESIAN_POINT ( 'NONE',  ( -13.00000000000003730, 249.9999999999999432, 0.000000000000000000 ) ) ;
#75002 = CARTESIAN_POINT ( 'NONE',  ( -4.000000000000000888, 17.58270891865066687, 5.744562646538041939 ) ) ;
#75003 = CARTESIAN_POINT ( 'NONE',  ( -1.221109131435400341, 53.71017309888716085, 9.311974234608470624 ) ) ;
#75004 = CARTESIAN_POINT ( 'NONE',  ( -13.49954484221011519, -52.22483108233568316, 30.71121296612578888 ) ) ;
#75005 = CARTESIAN_POINT ( 'NONE',  ( 43.74985542820358830, 435.5770091380369422, 16.96136490515564788 ) ) ;
#75006 = CARTESIAN_POINT ( 'NONE',  ( 108.4360931436784767, -30.00000000000001066, 186.7338794867829677 ) ) ;
#75007 = EDGE_CURVE ( 'NONE', #48472, #95649, #31635, .T. ) ;
#75008 = CARTESIAN_POINT ( 'NONE',  ( -114.5769593907454862, -59.99999999999998579, 170.6727965893586827 ) ) ;
#75009 = CARTESIAN_POINT ( 'NONE',  ( -59.01117578513747475, -39.49325923892655510, 69.67093582982462863 ) ) ;
#75010 = ORIENTED_EDGE ( 'NONE', *, *, #6744, .F. ) ;
#75011 = DIRECTION ( 'NONE',  ( 1.000000000000000000, 0.000000000000000000, -0.000000000000000000 ) ) ;
#75012 = CARTESIAN_POINT ( 'NONE',  ( 106.9295305114262931, -59.99999999999999289, 107.3648086918558420 ) ) ;
#75013 = ORIENTED_EDGE ( 'NONE', *, *, #18641, .F. ) ;
#75014 = CARTESIAN_POINT ( 'NONE',  ( 3.963954421596001421, -18.58606326360312266, 26.98072944107077831 ) ) ;
#75015 = CARTESIAN_POINT ( 'NONE',  ( -101.5623509475985173, -45.26550195618241901, 142.1330721071399239 ) ) ;
#75016 = CARTESIAN_POINT ( 'NONE',  ( 5.082755093536325930, -13.34375000204838457, -5.082755093536325042 ) ) ;
#75017 = DIRECTION ( 'NONE',  ( 0.000000000000000000, 0.000000000000000000, 1.000000000000000000 ) ) ;
#75018 = ORIENTED_EDGE ( 'NONE', *, *, #45041, .T. ) ;
#75019 = DIRECTION ( 'NONE',  ( 1.871721906610600077E-16, 0.000000000000000000, -1.000000000000000000 ) ) ;
#75020 = CIRCLE ( 'NONE', #88822, 4.000000000000001776 ) ;
#75021 = CARTESIAN_POINT ( 'NONE',  ( -26.66627763802065232, -60.00000000000002842, 41.62965253161740264 ) ) ;
#75022 = CARTESIAN_POINT ( 'NONE',  ( 9.300615953693611715, -55.29760853177170077, 23.32435243128603730 ) ) ;
#75023 = CARTESIAN_POINT ( 'NONE',  ( -1.320432766682874540E-15, -18.40625000204838457, 7.188101187500000044 ) ) ;
#75024 = ADVANCED_FACE ( 'NONE', ( #98454 ), #24545, .F. ) ;
#75025 = CARTESIAN_POINT ( 'NONE',  ( -37.85084083633361018, 437.2249973798734004, 3.569182825063079711 ) ) ;
#75026 = CARTESIAN_POINT ( 'NONE',  ( 0.000000000000000000, -78.00000000000000000, 27.00000000000000000 ) ) ;
#75027 = CARTESIAN_POINT ( 'NONE',  ( 7.002619243997878939, -83.94992681986181537, -3.868708944012999584 ) ) ;
#75028 = CARTESIAN_POINT ( 'NONE',  ( 0.000000000000000000, 0.000000000000000000, 5.000000000000000888 ) ) ;
#75029 = CARTESIAN_POINT ( 'NONE',  ( -30.00000000000000355, 461.8665156241398222, 11.40533150091695447 ) ) ;
#75030 = SURFACE_SIDE_STYLE ('',( #43746 ) ) ;
#75031 = CARTESIAN_POINT ( 'NONE',  ( 8.542937654374686218, 1.046208125374535811E-15, -6.800000000000000711 ) ) ;
#75032 = CARTESIAN_POINT ( 'NONE',  ( 88.95618763265999007, -60.00000000000002842, 47.35786141365969115 ) ) ;
#75033 = CARTESIAN_POINT ( 'NONE',  ( -30.11868724977495759, -46.43670190743181792, 34.41063938579866033 ) ) ;
#75034 = CARTESIAN_POINT ( 'NONE',  ( -3.499286860954911482, -49.14195911236761560, 104.2445795335841723 ) ) ;
#75035 = CARTESIAN_POINT ( 'NONE',  ( 44.95488294866025569, -53.34550232067736886, 47.31495729669310180 ) ) ;
#75036 = DIRECTION ( 'NONE',  ( 0.2107607412267715197, 0.000000000000000000, 0.9775376770015271610 ) ) ;
#75037 = VERTEX_POINT ( 'NONE', #7313 ) ;
#75038 = CARTESIAN_POINT ( 'NONE',  ( 43.62838954006687686, 434.9736691849527688, 14.34345830637867891 ) ) ;
#75039 = CARTESIAN_POINT ( 'NONE',  ( -80.51573996916087594, -38.81441202086065090, 193.8693134589343572 ) ) ;
#75040 = VERTEX_POINT ( 'NONE', #106547 ) ;
#75042 = CARTESIAN_POINT ( 'NONE',  ( 37.04388863813380794, 311.3287000699716032, 13.89786840526617517 ) ) ;
#75041 = CARTESIAN_POINT ( 'NONE',  ( 0.000000000000000000, 300.0000000000000000, 0.000000000000000000 ) ) ;
#75043 = CARTESIAN_POINT ( 'NONE',  ( 52.76369956428789720, -60.00000000000002132, 63.53480520484748695 ) ) ;
#75044 = DIRECTION ( 'NONE',  ( 0.000000000000000000, 0.000000000000000000, 1.000000000000000000 ) ) ;
#75045 = CARTESIAN_POINT ( 'NONE',  ( 6.291779652043022253, -1.386462189980468773, 6.829130021847237053 ) ) ;
#75046 = VECTOR ( 'NONE', #36776, 1000.000000000000000 ) ;
#75047 = AXIS2_PLACEMENT_3D ( 'NONE', #64043, #23054, #56974 ) ;
#75048 = CARTESIAN_POINT ( 'NONE',  ( 6.757705285491359071, 41.35007050631321590, -70.67351639401239538 ) ) ;
#75049 = DIRECTION ( 'NONE',  ( 0.000000000000000000, -1.000000000000000000, 0.000000000000000000 ) ) ;
#75050 = CARTESIAN_POINT ( 'NONE',  ( 5.858824175751784047, -88.78579060872363016, -1.318356988357131998 ) ) ;
#75051 = DIRECTION ( 'NONE',  ( 0.000000000000000000, -1.000000000000000000, 0.000000000000000000 ) ) ;
#75052 = CARTESIAN_POINT ( 'NONE',  ( 110.2341470348194719, -60.00000000000000000, 145.3203655816352580 ) ) ;
#75053 = CARTESIAN_POINT ( 'NONE',  ( -6.835395722631245619, -47.88907770483961457, 39.21814578782241512 ) ) ;
#75054 = CIRCLE ( 'NONE', #25131, 4.000000000000001776 ) ;
#75055 = CIRCLE ( 'NONE', #35466, 4.000000000000001776 ) ;
#75056 =( BOUNDED_SURFACE ( )  B_SPLINE_SURFACE ( 3, 2, ( 
 ( #35205, #61061, #68077 ),
 ( #3348, #36811, #100968 ),
 ( #2802, #69157, #102028 ),
 ( #93955, #27665, #35750 ),
 ( #69674, #51878, #60539 ),
 ( #102574, #61602, #92340 ),
 ( #19041, #84796, #68632 ),
 ( #73842, #75439, #99718 ),
 ( #33412, #43084, #100244 ),
 ( #25328, #67884, #18295 ),
 ( #91117, #59809, #26409 ),
 ( #8039, #83004, #58744 ),
 ( #34498, #40951, #59275 ),
 ( #50099, #81920, #99170 ),
 ( #100773, #1531, #67365 ),
 ( #57643, #35021, #50608 ),
 ( #106736, #65759, #26936 ),
 ( #24790, #9099, #32884 ),
 ( #42007, #58192, #9627 ),
 ( #49566, #92150, #33956 ),
 ( #10169, #98640, #16674 ),
 ( #90564, #51151, #42536 ),
 ( #75973, #17227, #82474 ),
 ( #974, #84069, #8575 ),
 ( #41477, #2068, #74364 ),
 ( #92690, #49022, #443 ) ),
 .UNSPECIFIED., .F., .F., .T. ) 
 B_SPLINE_SURFACE_WITH_KNOTS ( ( 4, 2, 2, 2, 2, 2, 2, 2, 2, 2, 2, 2, 4 ),
 ( 3, 3 ),
 ( 0.01269614743543319955, 0.01645309493989140920, 0.01739233181600596118, 0.01833156869212051315, 0.02021004244434962058, 0.02114927932046417602, 0.02208851619657872800, 0.02302775307269327998, 0.02396698994880783196, 0.02490622682492238393, 0.02584546370103693591, 0.02678470057715148789, 0.02772393745326604333 ),
 ( 0.000000000000000000, 1.000000000000000000 ),
 .UNSPECIFIED. ) 
 GEOMETRIC_REPRESENTATION_ITEM ( )  RATIONAL_B_SPLINE_SURFACE ( (
 ( 1.000000000000000000, 0.7779866052154990053, 1.000000000000000000),
 ( 1.000000000000000000, 0.7555083041612958850, 1.000000000000000000),
 ( 1.000000000000000000, 0.7303672838383610255, 1.000000000000000000),
 ( 1.000000000000000000, 0.6962732919722572911, 1.000000000000000000),
 ( 1.000000000000000000, 0.6893100548033399555, 1.000000000000000000),
 ( 1.000000000000000000, 0.6750693062836214953, 1.000000000000000000),
 ( 1.000000000000000000, 0.6677720645066671512, 1.000000000000000000),
 ( 1.000000000000000000, 0.6457877037097499162, 1.000000000000000000),
 ( 1.000000000000000000, 0.6308753259117235723, 1.000000000000000000),
 ( 1.000000000000000000, 0.6084032687353759794, 1.000000000000000000),
 ( 1.000000000000000000, 0.6008606624260669493, 1.000000000000000000),
 ( 1.000000000000000000, 0.5861844014193601238, 1.000000000000000000),
 ( 1.000000000000000000, 0.5790246786810088198, 1.000000000000000000),
 ( 1.000000000000000000, 0.5652570769870747247, 1.000000000000000000),
 ( 1.000000000000000000, 0.5586479634791106097, 1.000000000000000000),
 ( 1.000000000000000000, 0.5462697778676210980, 1.000000000000000000),
 ( 1.000000000000000000, 0.5405574414742128075, 1.000000000000000000),
 ( 1.000000000000000000, 0.5306463036818965806, 1.000000000000000000),
 ( 1.000000000000000000, 0.5264056264176346644, 1.000000000000000000),
 ( 1.000000000000000000, 0.5196980651061768874, 1.000000000000000000),
 ( 1.000000000000000000, 0.5172505343756695906, 1.000000000000000000),
 ( 1.000000000000000000, 0.5145634736035570311, 1.000000000000000000),
 ( 1.000000000000000000, 0.5142842565703922286, 1.000000000000000000),
 ( 1.000000000000000000, 0.5159055935738563470, 1.000000000000000000),
 ( 1.000000000000000000, 0.5178303183804268128, 1.000000000000000000),
 ( 1.000000000000000000, 0.5207636911093219689, 1.000000000000000000) ) ) 
 REPRESENTATION_ITEM ( '' )  SURFACE ( )  );
#75057 = CARTESIAN_POINT ( 'NONE',  ( -34.73928773455866548, 485.6865460664022294, -2.860109793110690912 ) ) ;
#75058 = ORIENTED_EDGE ( 'NONE', *, *, #91727, .F. ) ;
#75060 = EDGE_CURVE ( 'NONE', #13325, #23629, #95139, .T. ) ;
#75059 = B_SPLINE_CURVE_WITH_KNOTS ( 'NONE', 3,
 ( #25760, #42418, #49974, #18168 ),
 .UNSPECIFIED., .F., .F.,
 ( 4, 4 ),
 ( 5.204170427930421283E-18, 0.0002767692171812351329 ),
 .UNSPECIFIED. ) ;
#75061 = CARTESIAN_POINT ( 'NONE',  ( -90.33647909625912575, -29.99999999999991473, 190.1235012576946986 ) ) ;
#75062 = ORIENTED_EDGE ( 'NONE', *, *, #12136, .T. ) ;
#75063 = CARTESIAN_POINT ( 'NONE',  ( 3.430943074671123583, -4.332661967060490227, -17.58450835315055016 ) ) ;
#75064 = CARTESIAN_POINT ( 'NONE',  ( -16.04706613565624451, 4.602530725778174236, 3.432994500434128238 ) ) ;
#75065 = CARTESIAN_POINT ( 'NONE',  ( 24.60836828936892928, 305.5564293789130943, 10.31529206589142156 ) ) ;
#75066 = CIRCLE ( 'NONE', #64765, 5.000000000000001776 ) ;
#75067 = DIRECTION ( 'NONE',  ( 0.000000000000000000, -1.000000000000000000, 0.000000000000000000 ) ) ;
#75068 = CARTESIAN_POINT ( 'NONE',  ( -7.188101187500000044, -20.28125000204838813, -8.802885111219163269E-16 ) ) ;
#75069 = DIRECTION ( 'NONE',  ( -1.000000000000000000, -0.000000000000000000, 0.000000000000000000 ) ) ;
#75070 = ADVANCED_FACE ( 'NONE', ( #57455 ), #91658, .T. ) ;
#75071 = CARTESIAN_POINT ( 'NONE',  ( 4.000000000000000000, 4.898587196589412829E-16, -4.567799999999999194 ) ) ;
#75072 = ORIENTED_EDGE ( 'NONE', *, *, #32257, .T. ) ;
#75073 = CARTESIAN_POINT ( 'NONE',  ( 85.45692222432249707, -18.59276221248585159, 159.4212664435137015 ) ) ;
#75074 = CARTESIAN_POINT ( 'NONE',  ( -1.727368016638141196E-09, 38.95322581935191408, 63.66965480466879512 ) ) ;
#75075 = ORIENTED_EDGE ( 'NONE', *, *, #27122, .T. ) ;
#75076 = DIRECTION ( 'NONE',  ( -1.000000000000000000, -1.224606353822377258E-16, -0.000000000000000000 ) ) ;
#75077 = CARTESIAN_POINT ( 'NONE',  ( -16.64348903516517098, -1.200000000000000030E-05, 5.407797401561653672 ) ) ;
#75078 = DIRECTION ( 'NONE',  ( 0.000000000000000000, 0.000000000000000000, 1.000000000000000000 ) ) ;
#75079 = DIRECTION ( 'NONE',  ( 1.000000000000000000, 2.168404344971008868E-17, -0.000000000000000000 ) ) ;
#75080 = CARTESIAN_POINT ( 'NONE',  ( 35.11650669486618170, -3.999999999999998224, 0.000000000000000000 ) ) ;
#75081 = CARTESIAN_POINT ( 'NONE',  ( -26.96904186675336490, 306.9427295668461397, 10.87987742757496612 ) ) ;
#75082 = DIRECTION ( 'NONE',  ( -1.000000000000000000, -1.224606353822377258E-16, -0.000000000000000000 ) ) ;
#75083 = EDGE_CURVE ( 'NONE', #50026, #80953, #38659, .T. ) ;
#75084 = ORIENTED_EDGE ( 'NONE', *, *, #79774, .T. ) ;
#75085 =( NAMED_UNIT ( * ) SI_UNIT ( $, .STERADIAN. ) SOLID_ANGLE_UNIT ( ) );
#75086 = CARTESIAN_POINT ( 'NONE',  ( -1.918307803942188361, 301.4527163651389401, 9.816892514603376085 ) ) ;
#75087 =( NAMED_UNIT ( * ) PLANE_ANGLE_UNIT ( ) SI_UNIT ( $, .RADIAN. ) );
#75088 = CARTESIAN_POINT ( 'NONE',  ( 14.89106961510137062, 23.12249028321820532, -0.5049748053441320828 ) ) ;
#75089 = DIRECTION ( 'NONE',  ( -0.000000000000000000, -0.000000000000000000, -1.000000000000000000 ) ) ;
#75090 = CARTESIAN_POINT ( 'NONE',  ( 2.977408999572651815, -31.43750000204839168, 7.188101187500000933 ) ) ;
#75091 = CARTESIAN_POINT ( 'NONE',  ( 21.29975379448946171, 294.8969325209483259, -1.990407376643353210 ) ) ;
#75092 = CARTESIAN_POINT ( 'NONE',  ( 8.399631981393785196, 51.60902835563812374, 4.031152949374444461 ) ) ;
#75093 = EDGE_CURVE ( 'NONE', #81361, #103201, #97929, .T. ) ;
#75094 = CARTESIAN_POINT ( 'NONE',  ( 27.33349330513380337, 4.000000000000002665, 0.000000000000000000 ) ) ;
#75095 = CARTESIAN_POINT ( 'NONE',  ( -9.165151389911679658, 30.00000000000000000, 4.000000000000000000 ) ) ;
#75096 = ORIENTED_EDGE ( 'NONE', *, *, #101860, .T. ) ;
#75097 = CARTESIAN_POINT ( 'NONE',  ( 7.347880794884118356E-15, 50.00000000000000000, -60.00000000000000000 ) ) ;
#75098 = DIRECTION ( 'NONE',  ( 1.000000000000000000, -0.000000000000000000, -0.000000000000000000 ) ) ;
#75099 = CARTESIAN_POINT ( 'NONE',  ( -10.32854822922036853, 7.030784501320381352, -4.999999999999837463 ) ) ;
#75100 = FACE_OUTER_BOUND ( 'NONE', #83121, .T. ) ;
#75101 = TOROIDAL_SURFACE ( 'NONE', #30332, 12.00000000000000711, 3.000000000000000000 ) ;
#75102 = ORIENTED_EDGE ( 'NONE', *, *, #3193, .F. ) ;
#75103 = CARTESIAN_POINT ( 'NONE',  ( -30.00000000000001066, 464.2325109574570092, 15.22807244442123498 ) ) ;
#75104 = CARTESIAN_POINT ( 'NONE',  ( 20.00000000000000000, 12.99999999999999289, 0.000000000000000000 ) ) ;
#75105 = CARTESIAN_POINT ( 'NONE',  ( 107.5561821168135879, -57.67122918346473170, 113.7335151422611972 ) ) ;
#75106 = STYLED_ITEM ( 'NONE', ( #36805 ), #24876 ) ;
#75107 = EDGE_CURVE ( 'NONE', #64087, #94271, #76163, .T. ) ;
#75108 = CARTESIAN_POINT ( 'NONE',  ( 31.17406065558679629, 437.9984601485548978, 21.19262156861901403 ) ) ;
#75109 = DIRECTION ( 'NONE',  ( 1.000000000000000000, 2.168404344971008868E-17, 0.000000000000000000 ) ) ;
#75110 = FACE_BOUND ( 'NONE', #27410, .T. ) ;
#75111 = VECTOR ( 'NONE', #100782, 1000.000000000000000 ) ;
#75112 = CARTESIAN_POINT ( 'NONE',  ( 36.81747209427396683, 25.76191021544938664, 13.21972084597153696 ) ) ;
#75113 = CARTESIAN_POINT ( 'NONE',  ( -86.21883104017021537, -60.00000000000000000, 200.6728299286499180 ) ) ;
#75114 = STYLED_ITEM ( 'NONE', ( #39147 ), #23817 ) ;
#75115 = CONICAL_SURFACE ( 'NONE', #106069, 3.309500000000007880, 0.9599310885968770357 ) ;
#75116 = VECTOR ( 'NONE', #33259, 1000.000000000000000 ) ;
#75117 = LINE ( 'NONE', #84827, #21125 ) ;
#75118 = DIRECTION ( 'NONE',  ( -1.000000000000000000, -0.000000000000000000, -0.000000000000000000 ) ) ;
#75119 = DIRECTION ( 'NONE',  ( 0.000000000000000000, -1.000000000000000000, 0.000000000000000000 ) ) ;
#75120 = CARTESIAN_POINT ( 'NONE',  ( -84.74688199002078193, -42.96560158919115224, 184.9204503371174155 ) ) ;
#75121 = ORIENTED_EDGE ( 'NONE', *, *, #98815, .F. ) ;
#75122 =( GEOMETRIC_REPRESENTATION_CONTEXT ( 3 ) GLOBAL_UNCERTAINTY_ASSIGNED_CONTEXT ( ( #55527 ) ) GLOBAL_UNIT_ASSIGNED_CONTEXT ( ( #17837, #94919, #3773 ) ) REPRESENTATION_CONTEXT ( 'NONE', 'WORKASPACE' ) );
#75123 = ORIENTED_EDGE ( 'NONE', *, *, #71088, .T. ) ;
#75124 = CARTESIAN_POINT ( 'NONE',  ( 16.03926360544220486, 4.449054639248220866, 3.142406330836459372 ) ) ;
#75125 = EDGE_CURVE ( 'NONE', #77127, #11414, #72590, .T. ) ;
#75126 = CARTESIAN_POINT ( 'NONE',  ( -83.16184401887252875, -37.80642310000339990, -3.564082901337037868 ) ) ;
#75127 = B_SPLINE_CURVE_WITH_KNOTS ( 'NONE', 3,
 ( #106422, #63350, #88669, #96250, #39070, #30998, #72477, #22898 ),
 .UNSPECIFIED., .F., .F.,
 ( 4, 2, 2, 4 ),
 ( 0.004673709593152172194, 0.005837709341827658147, 0.007001709090503144967, 0.009329708587854115137 ),
 .UNSPECIFIED. ) ;
#75128 = AXIS2_PLACEMENT_3D ( 'NONE', #35727, #101490, #86390 ) ;
#75129 = CARTESIAN_POINT ( 'NONE',  ( -5.956988534971662475, 4.556784786910193397, -5.000000000000000000 ) ) ;
#75130 = CARTESIAN_POINT ( 'NONE',  ( 7.347880794884116778E-16, 70.00000000000000000, 5.999999999999998224 ) ) ;
#75131 = CARTESIAN_POINT ( 'NONE',  ( -1.467430646253637727, -3.559797132994073943E-15, 101.6319755442054458 ) ) ;
#75132 = CARTESIAN_POINT ( 'NONE',  ( -59.23741894013591036, 42.00000000000000711, -7.754160006507100356 ) ) ;
#75133 = EDGE_CURVE ( 'NONE', #55140, #34982, #105495, .T. ) ;
#75134 = CARTESIAN_POINT ( 'NONE',  ( -1.145927044342081135E-15, 61.34242035161803841, 9.357204421225127078 ) ) ;
#75135 = CARTESIAN_POINT ( 'NONE',  ( 25.54731711030018815, -59.99999999999990763, 43.65505808401614019 ) ) ;
#75136 = CARTESIAN_POINT ( 'NONE',  ( -35.45036406932465667, 436.3203772529668640, 5.179456583037453044 ) ) ;
#75137 = EDGE_CURVE ( 'NONE', #60348, #59296, #21095, .T. ) ;
#75138 = CARTESIAN_POINT ( 'NONE',  ( 32.64290048136811606, -14.21045842199427867, -35.33280650708731230 ) ) ;
#75139 = CARTESIAN_POINT ( 'NONE',  ( -67.07628553758745227, -42.96253981622765394, 94.37277177135563022 ) ) ;
#75140 = ORIENTED_EDGE ( 'NONE', *, *, #77329, .F. ) ;
#75141 = CARTESIAN_POINT ( 'NONE',  ( 69.92546618954501980, -29.99999999999995026, 127.5380661880360975 ) ) ;
#75142 = SURFACE_SIDE_STYLE ('',( #9341 ) ) ;
#75143 = CARTESIAN_POINT ( 'NONE',  ( 94.60551969766011382, -57.65569557003564682, -10.10694943204270047 ) ) ;
#75144 = ORIENTED_EDGE ( 'NONE', *, *, #66422, .F. ) ;
#75145 = CARTESIAN_POINT ( 'NONE',  ( 15.01526275298277824, 41.97362047124263285, -85.67312571145951949 ) ) ;
#75146 = ADVANCED_FACE ( 'NONE', ( #24081 ), #63470, .T. ) ;
#75147 = DIRECTION ( 'NONE',  ( 0.000000000000000000, 0.000000000000000000, -1.000000000000000000 ) ) ;
#75148 = ORIENTED_EDGE ( 'NONE', *, *, #31364, .T. ) ;
#75149 = CIRCLE ( 'NONE', #61407, 5.000000000000011546 ) ;
#75150 = CARTESIAN_POINT ( 'NONE',  ( 0.2711492888862935824, 13.85270131633358481, -7.000000000000011546 ) ) ;
#75151 = EDGE_CURVE ( 'NONE', #104988, #78191, #786, .T. ) ;
#75152 = FILL_AREA_STYLE_COLOUR ( '', #97828 ) ;
#75153 = DIRECTION ( 'NONE',  ( -1.000000000000000000, -0.000000000000000000, -0.000000000000000000 ) ) ;
#75154 = CARTESIAN_POINT ( 'NONE',  ( 7.188101187500001821, -13.06250000204838280, -2.977408999572650483 ) ) ;
#75155 = EDGE_CURVE ( 'NONE', #4042, #22420, #71012, .T. ) ;
#75156 = CARTESIAN_POINT ( 'NONE',  ( 4.419133455865365434, -6.108866147515648493, -7.026396753507436976 ) ) ;
#75157 = CONICAL_SURFACE ( 'NONE', #7948, 4.000000000000001776, 0.9599310885968808105 ) ;
#75158 = CARTESIAN_POINT ( 'NONE',  ( 25.22241582816893057, -4.285714285714295357, -1.650803255657548707 ) ) ;
#75159 = CARTESIAN_POINT ( 'NONE',  ( 6.928203230275509661, 105.0000000000000000, 4.000000000000001776 ) ) ;
#75160 = CARTESIAN_POINT ( 'NONE',  ( 13.50000000000000355, 7.794228634059978233, -11.79422863405993382 ) ) ;
#75161 = DIRECTION ( 'NONE',  ( -0.9623543818480316814, 0.1986072300191289164, 0.1855511032627455981 ) ) ;
#75162 = LINE ( 'NONE', #9357, #92629 ) ;
#75163 = ORIENTED_EDGE ( 'NONE', *, *, #9213, .T. ) ;
#75164 = CARTESIAN_POINT ( 'NONE',  ( -7.358394980812720476, 41.06696360374984067, -70.11548085267834551 ) ) ;
#75166 = CARTESIAN_POINT ( 'NONE',  ( 31.99605376666647771, -46.43077180847059537, 35.16619386691120752 ) ) ;
#75165 = CARTESIAN_POINT ( 'NONE',  ( -3.787335548944444241, -48.90784695949694338, 104.1352136098598606 ) ) ;
#75167 = CARTESIAN_POINT ( 'NONE',  ( -32.67323224503967083, 485.6332095909901341, 6.597358449828222504 ) ) ;
#75168 = ORIENTED_EDGE ( 'NONE', *, *, #40858, .F. ) ;
#75169 = ORIENTED_EDGE ( 'NONE', *, *, #18587, .T. ) ;
#75171 = FILL_AREA_STYLE ('',( #26160 ) ) ;
#75170 = CARTESIAN_POINT ( 'NONE',  ( 0.000000000000000000, 0.000000000000000000, -2.575493252495433261 ) ) ;
#75172 = CARTESIAN_POINT ( 'NONE',  ( 30.59999999999999787, 1.533819458162526451E-15, 0.000000000000000000 ) ) ;
#75173 = CARTESIAN_POINT ( 'NONE',  ( -15.67167025678515913, 294.5587403484931883, -10.06229237371755048 ) ) ;
#75174 = CARTESIAN_POINT ( 'NONE',  ( 99.17777777777777715, 4.172000000000019249, 5.109226446042768454E-16 ) ) ;
#75176 = PRESENTATION_LAYER_ASSIGNMENT (  '', '', ( #106190 ) ) ;
#75175 = DIRECTION ( 'NONE',  ( 0.000000000000000000, -1.000000000000000000, 0.000000000000000000 ) ) ;
#75177 = CARTESIAN_POINT ( 'NONE',  ( -37.56086443613940418, 463.3607749238124143, 20.02088289192456116 ) ) ;
#75178 = ORIENTED_EDGE ( 'NONE', *, *, #31441, .F. ) ;
#75179 = CARTESIAN_POINT ( 'NONE',  ( 80.24245568983633348, -60.00000000000000711, -27.79638001884161014 ) ) ;
#75180 = CIRCLE ( 'NONE', #14888, 5.000000000000002665 ) ;
#75181 = CARTESIAN_POINT ( 'NONE',  ( -9.956561055908920821, 45.46170052629869929, 15.37429631330336299 ) ) ;
#75182 = CARTESIAN_POINT ( 'NONE',  ( -7.000000000000000000, 8.572527594031471218E-16, -0.7256075382097185722 ) ) ;
#75183 = CARTESIAN_POINT ( 'NONE',  ( 23.86650669486618881, 1.474610560812782335E-15, 0.000000000000000000 ) ) ;
#75184 = ORIENTED_EDGE ( 'NONE', *, *, #84683, .T. ) ;
#75185 = AXIS2_PLACEMENT_3D ( 'NONE', #48824, #55331, #72063 ) ;
#75186 = CARTESIAN_POINT ( 'NONE',  ( 17.81438722625302518, 5.000000000000002665, 0.000000000000000000 ) ) ;
#75187 = ORIENTED_EDGE ( 'NONE', *, *, #91945, .F. ) ;
#75188 = ORIENTED_EDGE ( 'NONE', *, *, #5716, .T. ) ;
#75189 = CARTESIAN_POINT ( 'NONE',  ( 7.986539162393899716, 81.02672828942547767, -0.5321833565149893808 ) ) ;
#75190 = FACE_OUTER_BOUND ( 'NONE', #67859, .T. ) ;
#75191 = LINE ( 'NONE', #35860, #39750 ) ;
#75193 = CARTESIAN_POINT ( 'NONE',  ( 86.65316178196621877, -60.14505102782934642, 0.2230932978307594572 ) ) ;
#75192 = MECHANICAL_DESIGN_GEOMETRIC_PRESENTATION_REPRESENTATION (  '', ( #44195 ), #76971 ) ;
#75194 = VECTOR ( 'NONE', #66656, 1000.000000000000000 ) ;
#75195 = CARTESIAN_POINT ( 'NONE',  ( -36.15856845288970334, 304.2561437961289244, 0.1683646767355131690 ) ) ;
#75196 = DIRECTION ( 'NONE',  ( 1.000000000000000000, 0.000000000000000000, 0.000000000000000000 ) ) ;
#75197 = CARTESIAN_POINT ( 'NONE',  ( 12.50000000000000711, 39.74926845579918933, -65.00518738068748803 ) ) ;
#75198 = ORIENTED_EDGE ( 'NONE', *, *, #4807, .F. ) ;
#75200 = EDGE_CURVE ( 'NONE', #8257, #24684, #37579, .T. ) ;
#75199 = CARTESIAN_POINT ( 'NONE',  ( -43.02621584241283870, 434.6128289108255558, 16.97888786058999244 ) ) ;
#75201 = ORIENTED_EDGE ( 'NONE', *, *, #46332, .F. ) ;
#75202 = CARTESIAN_POINT ( 'NONE',  ( 9.761447470195587783, 51.33896531949353914, -2.428010505629565330 ) ) ;
#75203 = DIRECTION ( 'NONE',  ( -0.5735764363510512664, 0.8191520442889881348, 1.003171929053520309E-16 ) ) ;
#75204 = MECHANICAL_DESIGN_GEOMETRIC_PRESENTATION_REPRESENTATION (  '', ( #104541 ), #32187 ) ;
#75205 = AXIS2_PLACEMENT_3D ( 'NONE', #45764, #86778, #37717 ) ;
#75206 = AXIS2_PLACEMENT_3D ( 'NONE', #88034, #88559, #47548 ) ;
#75208 = VERTEX_POINT ( 'NONE', #82814 ) ;
#75207 = DIRECTION ( 'NONE',  ( 5.710694965406835788E-17, -0.7561819230143446147, -0.6543614439331888466 ) ) ;
#75209 = CARTESIAN_POINT ( 'NONE',  ( 71.21928858210435465, -36.01210335758921133, 103.8020605858352212 ) ) ;
#75210 = AXIS2_PLACEMENT_3D ( 'NONE', #91489, #93073, #36477 ) ;
#75211 = ORIENTED_EDGE ( 'NONE', *, *, #93690, .F. ) ;
#75212 = CARTESIAN_POINT ( 'NONE',  ( -16.52732684424165654, 43.98685724163156863, -87.77868211029610279 ) ) ;
#75213 = AXIS2_PLACEMENT_3D ( 'NONE', #68387, #46097, #96772 ) ;
#75214 = CARTESIAN_POINT ( 'NONE',  ( 7.188101187500000933, -23.56250000204838457, -2.977408999572650483 ) ) ;
#75215 = CARTESIAN_POINT ( 'NONE',  ( -94.22037892716120666, -57.65324192061454056, -13.00879341737615569 ) ) ;
#75216 = ORIENTED_EDGE ( 'NONE', *, *, #23275, .T. ) ;
#75217 = CARTESIAN_POINT ( 'NONE',  ( -37.52420436161200712, 473.1127600448368185, 17.51444808554655097 ) ) ;
#75218 = CARTESIAN_POINT ( 'NONE',  ( 103.0706911096362717, -45.28272344628067714, 185.1160168883092183 ) ) ;
#75219 = CARTESIAN_POINT ( 'NONE',  ( 5.933195299858810223, 51.26745231766517463, -8.366070215451848924 ) ) ;
#75220 = CARTESIAN_POINT ( 'NONE',  ( 34.83349330513379982, 1.593028355512270567E-15, 0.000000000000000000 ) ) ;
#75221 = CARTESIAN_POINT ( 'NONE',  ( -1.469576158976823947E-15, -23.56250000409677270, 8.000000000000000000 ) ) ;
#75222 = CARTESIAN_POINT ( 'NONE',  ( 43.18056654203890332, 485.1460802498596649, 5.477204712337894854 ) ) ;
#75223 = DIRECTION ( 'NONE',  ( -1.000000000000000000, 0.000000000000000000, 0.000000000000000000 ) ) ;
#75224 = EDGE_CURVE ( 'NONE', #48529, #79927, #26223, .T. ) ;
#75225 = VECTOR ( 'NONE', #14259, 1000.000000000000000 ) ;
#75226 = CARTESIAN_POINT ( 'NONE',  ( 9.221346651730838673, 31.04834020068337708, -3.869102247876034184 ) ) ;
#75227 = CARTESIAN_POINT ( 'NONE',  ( -20.97754405179127346, 294.8763868968453608, 9.942224931492237516 ) ) ;
#75228 = CARTESIAN_POINT ( 'NONE',  ( 107.8829176528319209, 572.1183258647163257, 155.1969486012868629 ) ) ;
#75229 = SURFACE_STYLE_FILL_AREA ( #56917 ) ;
#75230 = ORIENTED_EDGE ( 'NONE', *, *, #71198, .T. ) ;
#75231 = CARTESIAN_POINT ( 'NONE',  ( -5.477641402353350841, 41.99667695465397088, -59.64144010652168504 ) ) ;
#75232 = LINE ( 'NONE', #100581, #52796 ) ;
#75233 = MECHANICAL_DESIGN_GEOMETRIC_PRESENTATION_REPRESENTATION (  '', ( #80396 ), #73462 ) ;
#75234 = CARTESIAN_POINT ( 'NONE',  ( 44.57115381837846257, 434.3516557708408641, 14.78613344168310562 ) ) ;
#75235 = CARTESIAN_POINT ( 'NONE',  ( -84.36810463635728752, -30.00000000000000000, 164.3467819408754451 ) ) ;
#75236 = B_SPLINE_CURVE_WITH_KNOTS ( 'NONE', 3,
 ( #39829, #24197, #48426, #81316, #16065, #48948, #59203, #67817, #92613, #91570 ),
 .UNSPECIFIED., .F., .F.,
 ( 4, 2, 2, 2, 4 ),
 ( 0.000000000000000000, 0.001118707926289530140, 0.002237415852579060279, 0.003356123778868591503, 0.004474831705158123160 ),
 .UNSPECIFIED. ) ;
#75237 = VERTEX_POINT ( 'NONE', #75785 ) ;
#75238 = EDGE_LOOP ( 'NONE', ( #96521, #66300, #72485, #21633 ) ) ;
#75239 = CARTESIAN_POINT ( 'NONE',  ( 3.453949035417619218, -49.16871745132488059, 44.00840514944384552 ) ) ;
#75240 = CARTESIAN_POINT ( 'NONE',  ( 72.42338011058984648, -57.66707912199269970, 176.2281522364783655 ) ) ;
#75242 = CARTESIAN_POINT ( 'NONE',  ( -9.803861187004121902, 53.40458980087238672, 2.926399253106211962 ) ) ;
#75241 = CARTESIAN_POINT ( 'NONE',  ( -15.51358515996878573, 2.608314655049470687, -0.4154586159635258458 ) ) ;
#75243 = CARTESIAN_POINT ( 'NONE',  ( 6.366465994463423428, -21.85545340215044519, -38.54589836641859080 ) ) ;
#75244 = CARTESIAN_POINT ( 'NONE',  ( -0.8415708020617345131, 43.28585517694735785, 18.42785063933127532 ) ) ;
#75245 = PRODUCT_RELATED_PRODUCT_CATEGORY ( 'part', '', ( #99384 ) ) ;
#75246 = CARTESIAN_POINT ( 'NONE',  ( -32.89843394316242353, -59.99999999999999289, 44.77189468774703585 ) ) ;
#75247 = PRESENTATION_LAYER_ASSIGNMENT (  '', '', ( #11577 ) ) ;
#75248 = CARTESIAN_POINT ( 'NONE',  ( 54.03872891708841308, 6.856755485862130937E-15, 0.000000000000000000 ) ) ;
#75249 = CARTESIAN_POINT ( 'NONE',  ( 5.856562693840234424, 53.40179940001038972, 8.398636774803573957 ) ) ;
#75250 = CARTESIAN_POINT ( 'NONE',  ( -86.21536416698982919, -35.54068135687334262, 186.1489417679863152 ) ) ;
#75251 = EDGE_LOOP ( 'NONE', ( #11781, #48892, #17844, #95001, #62162 ) ) ;
#75252 = CARTESIAN_POINT ( 'NONE',  ( 30.04058829887667770, 13.07764605659135881, 42.05455409923722954 ) ) ;
#75253 = CARTESIAN_POINT ( 'NONE',  ( -6.078692300985167662, -35.99430252327623947, 29.87896141239675174 ) ) ;
#75254 = PRESENTATION_STYLE_ASSIGNMENT (( #100603 ) ) ;
#75255 = CARTESIAN_POINT ( 'NONE',  ( 86.73932400000002474, -41.70651791337262893, 189.2637588004315319 ) ) ;
#75257 = CARTESIAN_POINT ( 'NONE',  ( 4.618707958157409088, -65.43970587102317893, 13.10267263298003648 ) ) ;
#75256 = CARTESIAN_POINT ( 'NONE',  ( -42.47964311110575153, 356.5060619603087844, 15.81299726375038794 ) ) ;
#75258 = ORIENTED_EDGE ( 'NONE', *, *, #5995, .F. ) ;
#75259 = CARTESIAN_POINT ( 'NONE',  ( 5.500000036871884213, 42.00000000000000000, -68.91429207046176941 ) ) ;
#75260 = DIRECTION ( 'NONE',  ( 0.000000000000000000, -1.000000000000000000, 0.000000000000000000 ) ) ;
#75261 = EDGE_CURVE ( 'NONE', #65330, #18064, #65084, .T. ) ;
#75262 = DIRECTION ( 'NONE',  ( 0.000000000000000000, -0.9137523047319339176, 0.4062717386147834953 ) ) ;
#75263 = AXIS2_PLACEMENT_3D ( 'NONE', #72092, #13844, #45701 ) ;
#75264 = AXIS2_PLACEMENT_3D ( 'NONE', #79392, #102072, #85924 ) ;
#75265 = ADVANCED_FACE ( 'NONE', ( #27286 ), #60170, .T. ) ;
#75266 = CARTESIAN_POINT ( 'NONE',  ( 30.76801067634421116, 297.9428771719580027, -9.321789843264367548 ) ) ;
#75267 = CARTESIAN_POINT ( 'NONE',  ( 40.17205142263708240, 310.2804317922712016, -6.358608209531249500 ) ) ;
#75268 = EDGE_CURVE ( 'NONE', #34743, #20894, #15478, .T. ) ;
#75269 = DIRECTION ( 'NONE',  ( -1.000000000000000000, -0.000000000000000000, -0.000000000000000000 ) ) ;
#75270 = CARTESIAN_POINT ( 'NONE',  ( 106.8235258757864869, -14.21045842199432307, 178.1026719309843429 ) ) ;
#75271 = CARTESIAN_POINT ( 'NONE',  ( -84.55966185417285885, -22.11373329182813308, 156.8083849470275197 ) ) ;
#75272 = ORIENTED_EDGE ( 'NONE', *, *, #85701, .F. ) ;
#75273 = CARTESIAN_POINT ( 'NONE',  ( 80.40000000000000568, -4.171999999999998820, 0.000000000000000000 ) ) ;
#75274 = CARTESIAN_POINT ( 'NONE',  ( 52.56483885390524335, 49.99999999999999289, -38.23529411764707220 ) ) ;
#75275 = CONICAL_SURFACE ( 'NONE', #78736, 7.000000000000000000, 0.9599310885968753704 ) ;
#75276 = FACE_OUTER_BOUND ( 'NONE', #61265, .T. ) ;
#75277 =( GEOMETRIC_REPRESENTATION_CONTEXT ( 3 ) GLOBAL_UNCERTAINTY_ASSIGNED_CONTEXT ( ( #96632 ) ) GLOBAL_UNIT_ASSIGNED_CONTEXT ( ( #57067, #64140, #72205 ) ) REPRESENTATION_CONTEXT ( 'NONE', 'WORKASPACE' ) );
#75278 = AXIS2_PLACEMENT_3D ( 'NONE', #26399, #4737, #101828 ) ;
#75279 = DIRECTION ( 'NONE',  ( 0.000000000000000000, -1.000000000000000000, 0.000000000000000000 ) ) ;
#75280 = CARTESIAN_POINT ( 'NONE',  ( 2.849088492170978260, 70.33537520974232393, -4.999999999999997335 ) ) ;
#75281 = CARTESIAN_POINT ( 'NONE',  ( 6.326592304916277776, -5.253140224433048289, 4.564380808752273033 ) ) ;
#75282 = VERTEX_POINT ( 'NONE', #26746 ) ;
#75284 = CONICAL_SURFACE ( 'NONE', #99373, 4.000000000000001776, 0.9599310885968808105 ) ;
#75283 = CARTESIAN_POINT ( 'NONE',  ( -23.00081687371528716, 305.6505493688913475, 9.110661126385450004 ) ) ;
#75285 = ADVANCED_FACE ( 'NONE', ( #59623 ), #83341, .F. ) ;
#75286 = EDGE_LOOP ( 'NONE', ( #85181, #6005, #82318, #8571, #46635 ) ) ;
#75287 = CARTESIAN_POINT ( 'NONE',  ( 21.09715123528542691, 1.340359594676612611E-15, 0.000000000000000000 ) ) ;
#75288 = EDGE_CURVE ( 'NONE', #3119, #43338, #97805, .T. ) ;
#75289 = CARTESIAN_POINT ( 'NONE',  ( 6.249999999999998224, 8.000000000000000000, 0.000000000000000000 ) ) ;
#75290 = CARTESIAN_POINT ( 'NONE',  ( -7.500000000000007105, 39.99999999999998579, -68.91429205786793943 ) ) ;
#75291 = CARTESIAN_POINT ( 'NONE',  ( 37.84772257691316355, 50.00000000000000000, 50.69408796163846631 ) ) ;
#75292 = CARTESIAN_POINT ( 'NONE',  ( 5.000000000000000000, -14.08559933050961632, 11.75736354680376472 ) ) ;
#75294 = EDGE_CURVE ( 'NONE', #78094, #21685, #54042, .T. ) ;
#75293 = CARTESIAN_POINT ( 'NONE',  ( 46.00000000000000000, 436.1215487527605887, 10.84755050468337956 ) ) ;
#75295 = ORIENTED_EDGE ( 'NONE', *, *, #84834, .F. ) ;
#75296 = CARTESIAN_POINT ( 'NONE',  ( 111.2971332976971581, -59.99999999999998579, 155.0290638565942629 ) ) ;
#75298 = CARTESIAN_POINT ( 'NONE',  ( 18.55641751059849298, -18.59015957681733866, 27.35011673974152657 ) ) ;
#75297 = CARTESIAN_POINT ( 'NONE',  ( -101.1248876217780719, -29.99999999999996803, 198.7487848662925387 ) ) ;
#75299 = CARTESIAN_POINT ( 'NONE',  ( 38.85446894546473828, 460.8903912184138676, 2.218456751109172398 ) ) ;
#75300 = DIRECTION ( 'NONE',  ( -1.000000000000000000, -0.000000000000000000, -0.000000000000000000 ) ) ;
#75301 = CARTESIAN_POINT ( 'NONE',  ( -41.90450118112109124, -32.61544904257455357, 38.71841112228458570 ) ) ;
#75302 = AXIS2_PLACEMENT_3D ( 'NONE', #25083, #49855, #39142 ) ;
#75303 = DIRECTION ( 'NONE',  ( -1.000000000000000000, -0.000000000000000000, -0.000000000000000000 ) ) ;
#75304 = UNCERTAINTY_MEASURE_WITH_UNIT (LENGTH_MEASURE( 1.000000000000000082E-05 ), #42, 'distance_accuracy_value', 'NONE');
#75305 = ORIENTED_EDGE ( 'NONE', *, *, #34964, .T. ) ;
#75306 = CARTESIAN_POINT ( 'NONE',  ( 48.02835407290504577, -1.200000000000000030E-05, -16.85535821593549954 ) ) ;
#75307 = CARTESIAN_POINT ( 'NONE',  ( 8.559508646656407649, 53.68473964988125857, 4.031152949374444461 ) ) ;
#75308 = CARTESIAN_POINT ( 'NONE',  ( 31.00389226642222340, 485.8187364282109115, 14.27494812388583512 ) ) ;
#75309 = CARTESIAN_POINT ( 'NONE',  ( 0.000000000000000000, 0.000000000000000000, 0.000000000000000000 ) ) ;
#75310 = CARTESIAN_POINT ( 'NONE',  ( 6.147350651869627924, 3.811648262644351526E-18, 18.77631036323126423 ) ) ;
#75311 = ORIENTED_EDGE ( 'NONE', *, *, #19756, .T. ) ;
#75313 = B_SPLINE_CURVE_WITH_KNOTS ( 'NONE', 3,
 ( #76644, #3299, #4358, #11912, #44840, #27619, #86370, #59969 ),
 .UNSPECIFIED., .F., .F.,
 ( 4, 2, 2, 4 ),
 ( 0.007886720825438833446, 0.009850969036564030668, 0.01181521724768922615, 0.01574371366993962407 ),
 .UNSPECIFIED. ) ;
#75312 = CARTESIAN_POINT ( 'NONE',  ( -16.19972009820057934, 36.53460074923750511, -24.18132016187605160 ) ) ;
#75314 = EDGE_LOOP ( 'NONE', ( #9539, #58897, #45956, #63505, #71916, #106758 ) ) ;
#75315 = CARTESIAN_POINT ( 'NONE',  ( 81.58172074487495706, -30.00000000000000000, -7.858416217283744842 ) ) ;
#75316 = CARTESIAN_POINT ( 'NONE',  ( 46.79015243495871346, 13.37233443428286250, 15.81143384442388466 ) ) ;
#75317 = UNCERTAINTY_MEASURE_WITH_UNIT (LENGTH_MEASURE( 1.000000000000000082E-05 ), #36232, 'distance_accuracy_value', 'NONE');
#75318 = DIRECTION ( 'NONE',  ( 0.000000000000000000, -1.000000000000000000, 0.000000000000000000 ) ) ;
#75319 = STYLED_ITEM ( 'NONE', ( #25231 ), #101388 ) ;
#75320 = CARTESIAN_POINT ( 'NONE',  ( 86.61791453296140730, -30.00000000000000000, 68.11649954288937181 ) ) ;
#75321 = ORIENTED_EDGE ( 'NONE', *, *, #102673, .F. ) ;
#75322 = EDGE_LOOP ( 'NONE', ( #69974, #76801, #82813, #31625, #85719 ) ) ;
#75323 = EDGE_LOOP ( 'NONE', ( #49687, #5119, #103098, #32351 ) ) ;
#75324 = CARTESIAN_POINT ( 'NONE',  ( -46.77684132781872961, 13.57955522726351383, -15.57752954476176477 ) ) ;
#75325 = CARTESIAN_POINT ( 'NONE',  ( 0.000000000000000000, 47.77514352166374323, 0.000000000000000000 ) ) ;
#75326 = DIRECTION ( 'NONE',  ( -1.000000000000000000, -0.000000000000000000, -0.000000000000000000 ) ) ;
#75327 = CARTESIAN_POINT ( 'NONE',  ( -31.20656969146428139, 410.2463405114667125, 25.45169261709286701 ) ) ;
#75328 = DIRECTION ( 'NONE',  ( -1.000000000000000000, -1.224606353822377258E-16, -0.000000000000000000 ) ) ;
#75329 = CIRCLE ( 'NONE', #82255, 1.000000000000003553 ) ;
#75330 = ORIENTED_EDGE ( 'NONE', *, *, #60309, .T. ) ;
#75332 = ADVANCED_FACE ( 'NONE', ( #103257, #45037 ), #43954, .F. ) ;
#75331 = CARTESIAN_POINT ( 'NONE',  ( -8.737863884121393809, 49.99999999999999289, -90.03618980231146907 ) ) ;
#75333 = EDGE_LOOP ( 'NONE', ( #33290, #89274, #21596, #53277 ) ) ;
#75334 = CARTESIAN_POINT ( 'NONE',  ( 65.03872891708842019, 6.856755485862130937E-15, 0.000000000000000000 ) ) ;
#75335 = CARTESIAN_POINT ( 'NONE',  ( 74.24703944025202418, -38.32801400578732398, 162.5046052861644625 ) ) ;
#75336 = CARTESIAN_POINT ( 'NONE',  ( 5.947762761376473861, -2.501851166488373579, 6.500000000000000000 ) ) ;
#75337 = CARTESIAN_POINT ( 'NONE',  ( 27.19928665125400613, 307.3533174255223912, 10.98053163142592936 ) ) ;
#75338 = CARTESIAN_POINT ( 'NONE',  ( -5.647817967127105376, 246.5487359347119991, -2.038183545141165176 ) ) ;
#75339 = ORIENTED_EDGE ( 'NONE', *, *, #26371, .T. ) ;
#75340 = CARTESIAN_POINT ( 'NONE',  ( 12.39578842395471270, -8.431745484732026341, -12.16229915940863293 ) ) ;
#75341 = DIRECTION ( 'NONE',  ( -1.000000000000000000, -1.224606353822377258E-16, -0.000000000000000000 ) ) ;
#75342 = EDGE_CURVE ( 'NONE', #64079, #59238, #93577, .T. ) ;
#75343 = CARTESIAN_POINT ( 'NONE',  ( 6.849999999999999645, 4.618802153517001408, -8.000000000000000000 ) ) ;
#75344 = VERTEX_POINT ( 'NONE', #4030 ) ;
#75345 = B_SPLINE_CURVE_WITH_KNOTS ( 'NONE', 3,
 ( #5004, #37407, #63778, #96665, #23323, #29836, #86483, #22271, #95603, #103170, #12539, #87520, #46515, #30355, #63246, #55119, #88049, #14129, #40021, #83130, #74496, #24401 ),
 .UNSPECIFIED., .F., .F.,
 ( 4, 2, 2, 2, 2, 2, 2, 2, 2, 2, 4 ),
 ( 0.004989850371616175000, 0.005493891472670148560, 0.005997932573724122120, 0.006501973674778095680, 0.007006014775832068373, 0.007258035326359055586, 0.007510055876886042800, 0.008014096977940015493, 0.008518138078993989920, 0.008770158629520977134, 0.009022179180047966082 ),
 .UNSPECIFIED. ) ;
#75347 = CARTESIAN_POINT ( 'NONE',  ( -28.10757706655090260, 297.0759717083114992, 10.42362710127031455 ) ) ;
#75346 = SURFACE_STYLE_FILL_AREA ( #101761 ) ;
#75348 = DIRECTION ( 'NONE',  ( 0.000000000000000000, 0.000000000000000000, -1.000000000000000000 ) ) ;
#75349 = UNCERTAINTY_MEASURE_WITH_UNIT (LENGTH_MEASURE( 1.000000000000000082E-05 ), #4103, 'distance_accuracy_value', 'NONE');
#75350 = CARTESIAN_POINT ( 'NONE',  ( 29.66054107240687543, 5.000000000000003553, 0.000000000000000000 ) ) ;
#75351 = CARTESIAN_POINT ( 'NONE',  ( -2.387978478800934834, -7.281554020289646267, -7.069802615102040555 ) ) ;
#75352 = AXIS2_PLACEMENT_3D ( 'NONE', #42244, #34200, #67072 ) ;
#75353 = CARTESIAN_POINT ( 'NONE',  ( 34.26493447557741234, 490.0907185571251716, 11.27927472375406381 ) ) ;
#75354 = CARTESIAN_POINT ( 'NONE',  ( 9.693872975896447031, 294.6517661903899352, 2.542797243357461046 ) ) ;
#75355 = VECTOR ( 'NONE', #69154, 1000.000000000000000 ) ;
#75356 = CIRCLE ( 'NONE', #101163, 5.000000000000011546 ) ;
#75357 = VECTOR ( 'NONE', #46880, 1000.000000000000000 ) ;
#75358 = LINE ( 'NONE', #1458, #91511 ) ;
#75359 = CARTESIAN_POINT ( 'NONE',  ( 85.23953769841214978, -46.56070485338828036, 188.0803264966071140 ) ) ;
#75360 = ADVANCED_FACE ( 'NONE', ( #61212 ), #35906, .T. ) ;
#75361 =( NAMED_UNIT ( * ) SI_UNIT ( $, .STERADIAN. ) SOLID_ANGLE_UNIT ( ) );
#75362 = EDGE_LOOP ( 'NONE', ( #14898, #73254, #61498, #16210, #5676, #18807 ) ) ;
#75363 = CARTESIAN_POINT ( 'NONE',  ( 94.14372550659786043, -57.65224881985284355, -13.67576374388242044 ) ) ;
#75364 = CARTESIAN_POINT ( 'NONE',  ( 41.50820411079202898, 461.5963371455317770, 2.703439750996501800 ) ) ;
#75365 = CARTESIAN_POINT ( 'NONE',  ( 15.49793471085725471, 34.92650142558106552, -22.93080145367699174 ) ) ;
#75366 = CARTESIAN_POINT ( 'NONE',  ( -0.000000000000000000, 0.000000000000000000, -5.000000000000000000 ) ) ;
#75367 = CIRCLE ( 'NONE', #63312, 4.000000000000001776 ) ;
#75368 = ADVANCED_FACE ( 'NONE', ( #45565 ), #46166, .T. ) ;
#75369 = CARTESIAN_POINT ( 'NONE',  ( -81.39596208340545047, -30.00000000000000711, -1.917334220413669188 ) ) ;
#75370 = CIRCLE ( 'NONE', #9929, 5.000000000000011546 ) ;
#75371 = CARTESIAN_POINT ( 'NONE',  ( -28.99999999999998934, 0.000000000000000000, 0.000000000000000000 ) ) ;
#75372 = CARTESIAN_POINT ( 'NONE',  ( -8.000000000000001776, -29.84375000409677270, 3.313708498984759387 ) ) ;
#75373 = DIRECTION ( 'NONE',  ( 0.000000000000000000, 0.000000000000000000, 1.000000000000000000 ) ) ;
#75375 = DIRECTION ( 'NONE',  ( -1.000000000000000000, -0.000000000000000000, -0.000000000000000000 ) ) ;
#75374 = CARTESIAN_POINT ( 'NONE',  ( -9.645512969475880993, 246.9889684932426803, -2.645801731561377768 ) ) ;
#75376 =( GEOMETRIC_REPRESENTATION_CONTEXT ( 3 ) GLOBAL_UNCERTAINTY_ASSIGNED_CONTEXT ( ( #81832 ) ) GLOBAL_UNIT_ASSIGNED_CONTEXT ( ( #101047, #92956, #27745 ) ) REPRESENTATION_CONTEXT ( 'NONE', 'WORKASPACE' ) );
#75377 = CARTESIAN_POINT ( 'NONE',  ( -17.49999999999997513, 49.01643442013767782, 64.05028169109587566 ) ) ;
#75378 = DIRECTION ( 'NONE',  ( -1.000000000000000000, 0.000000000000000000, 0.000000000000000000 ) ) ;
#75379 = CARTESIAN_POINT ( 'NONE',  ( -37.18119764942264283, 491.8021068614480669, 12.56169729800564561 ) ) ;
#75380 = CARTESIAN_POINT ( 'NONE',  ( 4.589357672516646502, -83.93793969022777901, -3.865585121226772891 ) ) ;
#75381 = CARTESIAN_POINT ( 'NONE',  ( -2.500000000000002220, 0.000000000000000000, 0.000000000000000000 ) ) ;
#75382 = CARTESIAN_POINT ( 'NONE',  ( 43.51602118667805996, 463.0217781655570093, 9.924214466287779146 ) ) ;
#75383 = CARTESIAN_POINT ( 'NONE',  ( 13.46238992380946442, -16.89357091335954664, -34.49996823829238934 ) ) ;
#75384 = AXIS2_PLACEMENT_3D ( 'NONE', #87019, #15226, #96166 ) ;
#75385 = EDGE_CURVE ( 'NONE', #80736, #70311, #82327, .T. ) ;
#75386 = CARTESIAN_POINT ( 'NONE',  ( -21.78122564462103483, -56.88112741419036666, 34.12320410153837713 ) ) ;
#75387 = VERTEX_POINT ( 'NONE', #11568 ) ;
#75388 = DIRECTION ( 'NONE',  ( -1.000000000000000000, 0.000000000000000000, 0.000000000000000000 ) ) ;
#75389 = FILL_AREA_STYLE_COLOUR ( '', #33219 ) ;
#75390 = CIRCLE ( 'NONE', #32306, 4.000000000000007105 ) ;
#75391 = CARTESIAN_POINT ( 'NONE',  ( 7.500000000000000888, -3.000671055698259870, -20.99923901233272971 ) ) ;
#75392 = CARTESIAN_POINT ( 'NONE',  ( -62.37515747485122830, -29.51886346143869844, -24.10950783783387763 ) ) ;
#75393 =( BOUNDED_SURFACE ( )  B_SPLINE_SURFACE ( 3, 2, ( 
 ( #15543, #13945, #79751 ),
 ( #38783, #48437, #104556 ),
 ( #51631, #58679, #84549 ),
 ( #84007, #25824, #101266 ),
 ( #913, #91581, #92626 ),
 ( #33352, #43552, #68369 ),
 ( #10114, #1472, #33892 ),
 ( #34436, #42478, #75913 ) ),
 .UNSPECIFIED., .F., .F., .F. ) 
 B_SPLINE_SURFACE_WITH_KNOTS ( ( 4, 2, 2, 4 ),
 ( 3, 3 ),
 ( 0.03861844051980969916, 0.04325213341840641879, 0.04556897986770477860, 0.04788582631700313841 ),
 ( 0.000000000000000000, 1.000000000000000000 ),
 .UNSPECIFIED. ) 
 GEOMETRIC_REPRESENTATION_ITEM ( )  RATIONAL_B_SPLINE_SURFACE ( (
 ( 1.000000000000000000, 0.8047781759831923454, 1.000000000000000000),
 ( 1.000000000000000000, 0.8123762462799783979, 1.000000000000000000),
 ( 1.000000000000000000, 0.8190659850623762672, 1.000000000000000000),
 ( 1.000000000000000000, 0.8191937571010124985, 1.000000000000000000),
 ( 1.000000000000000000, 0.8176092952778098999, 1.000000000000000000),
 ( 1.000000000000000000, 0.8122962088598847386, 1.000000000000000000),
 ( 1.000000000000000000, 0.8086311330826182475, 1.000000000000000000),
 ( 1.000000000000000000, 0.8047712282214326551, 1.000000000000000000) ) ) 
 REPRESENTATION_ITEM ( '' )  SURFACE ( )  );
#75395 = CARTESIAN_POINT ( 'NONE',  ( -71.32987062739258022, -47.40883850356869544, -23.55053093366642614 ) ) ;
#75394 = FACE_OUTER_BOUND ( 'NONE', #7495, .T. ) ;
#75396 = ORIENTED_EDGE ( 'NONE', *, *, #97127, .T. ) ;
#75397 = AXIS2_PLACEMENT_3D ( 'NONE', #69310, #102186, #102726 ) ;
#75398 = CARTESIAN_POINT ( 'NONE',  ( -14.81135389224447962, 41.99477687821654115, -87.54767125253117399 ) ) ;
#75399 = ORIENTED_EDGE ( 'NONE', *, *, #83243, .F. ) ;
#75400 = CARTESIAN_POINT ( 'NONE',  ( 43.00000000000000000, 461.4080316921935605, 3.462976341553837045 ) ) ;
#75401 = AXIS2_PLACEMENT_3D ( 'NONE', #86877, #12950, #38334 ) ;
#75402 = CARTESIAN_POINT ( 'NONE',  ( -71.33171024911513314, -59.99999999999999289, -32.04526279259148680 ) ) ;
#75403 = VERTEX_POINT ( 'NONE', #44498 ) ;
#75404 = CYLINDRICAL_SURFACE ( 'NONE', #103184, 4.000000000000000000 ) ;
#75405 = CARTESIAN_POINT ( 'NONE',  ( -7.160168481740964985, 294.7244989119860747, -7.003737591215575264 ) ) ;
#75406 = CARTESIAN_POINT ( 'NONE',  ( 102.3341614162330728, -60.19240241467774410, 193.7986361862069771 ) ) ;
#75407 = VECTOR ( 'NONE', #17868, 1000.000000000000114 ) ;
#75409 = DIRECTION ( 'NONE',  ( 0.000000000000000000, 0.000000000000000000, 1.000000000000000000 ) ) ;
#75408 = CARTESIAN_POINT ( 'NONE',  ( 17.61650669486618881, 1.474610560812782335E-15, 0.000000000000000000 ) ) ;
#75410 = B_SPLINE_CURVE_WITH_KNOTS ( 'NONE', 3,
 ( #47687, #56841, #106456, #80587, #32613, #49277, #97305, #48218, #82181, #8298, #81121, #89766, #31551, #74089, #48742, #6707, #7761, #40667, #64434, #73551 ),
 .UNSPECIFIED., .F., .F.,
 ( 4, 2, 2, 2, 2, 2, 2, 2, 2, 4 ),
 ( 0.003812777391809711244, 0.004316388813495462828, 0.004820000235181215280, 0.005071805946024091072, 0.005323611656866966864, 0.005827223078552714111, 0.006330834500238463093, 0.006834445921924211208, 0.007338057343609960190, 0.007841668765295708304 ),
 .UNSPECIFIED. ) ;
#75411 = CIRCLE ( 'NONE', #89209, 4.000000000000000888 ) ;
#75412 = EDGE_LOOP ( 'NONE', ( #20023, #77471 ) ) ;
#75413 = ORIENTED_EDGE ( 'NONE', *, *, #39839, .T. ) ;
#75414 = EDGE_CURVE ( 'NONE', #99696, #69600, #102976, .T. ) ;
#75415 = ORIENTED_EDGE ( 'NONE', *, *, #15126, .F. ) ;
#75416 = CARTESIAN_POINT ( 'NONE',  ( 31.39562674014780796, 425.0116429153000581, 23.79458313699800698 ) ) ;
#75417 = EDGE_CURVE ( 'NONE', #14833, #31177, #78437, .T. ) ;
#75418 = DIRECTION ( 'NONE',  ( -0.000000000000000000, -0.000000000000000000, -1.000000000000000000 ) ) ;
#75419 = CARTESIAN_POINT ( 'NONE',  ( 16.48315964343914786, 45.94107222901599386, 4.157797401561416528 ) ) ;
#75420 = VERTEX_POINT ( 'NONE', #36961 ) ;
#75421 = CARTESIAN_POINT ( 'NONE',  ( -43.41290683822509067, 487.0833545439620593, 7.569976829064873236 ) ) ;
#75422 = DIRECTION ( 'NONE',  ( -0.5735764363510510444, -0.8191520442889883569, 0.000000000000000000 ) ) ;
#75423 = CARTESIAN_POINT ( 'NONE',  ( -13.00000000000003730, -85.00000000000000000, 0.000000000000000000 ) ) ;
#75424 = CARTESIAN_POINT ( 'NONE',  ( -52.60809588292248407, -57.67627119646954981, 84.38067992663381744 ) ) ;
#75425 = CARTESIAN_POINT ( 'NONE',  ( -30.63784394300852654, 16.09242744237241496, 40.03992687782040605 ) ) ;
#75426 = CARTESIAN_POINT ( 'NONE',  ( -30.24427031855517711, 312.0196691915732004, -8.325478004009855937 ) ) ;
#75427 = CARTESIAN_POINT ( 'NONE',  ( 6.683837171061806082, 7.911893696991934455, 7.436622852660996417E-19 ) ) ;
#75428 = VECTOR ( 'NONE', #18379, 1000.000000000000000 ) ;
#75429 = EDGE_CURVE ( 'NONE', #62158, #16331, #23125, .T. ) ;
#75430 = CARTESIAN_POINT ( 'NONE',  ( -87.30967359867977962, -14.21045842199447229, 28.19474181966119275 ) ) ;
#75431 = CARTESIAN_POINT ( 'NONE',  ( -14.54015256618497176, 142.2617268803927573, -5.000000000000000000 ) ) ;
#75432 = CARTESIAN_POINT ( 'NONE',  ( -50.83579864079804622, -56.83981948626792757, 58.27881635844277497 ) ) ;
#75433 = CARTESIAN_POINT ( 'NONE',  ( -0.6682463242654161917, 21.79871736972542351, 6.969258537597399439 ) ) ;
#75435 = ORIENTED_EDGE ( 'NONE', *, *, #14263, .T. ) ;
#75434 = MECHANICAL_DESIGN_GEOMETRIC_PRESENTATION_REPRESENTATION (  '', ( #68525 ), #106375 ) ;
#75436 = CARTESIAN_POINT ( 'NONE',  ( -94.29814206750670280, -37.67726954591325494, 192.9876237923781730 ) ) ;
#75437 = PRESENTATION_LAYER_ASSIGNMENT (  '', '', ( #94398 ) ) ;
#75438 = DIRECTION ( 'NONE',  ( -0.5735764363510497121, 0.8191520442889892450, 1.003171929053521665E-16 ) ) ;
#75439 = CARTESIAN_POINT ( 'NONE',  ( 9.493622844526626636, -1.977828722490834634, 15.48005331695811648 ) ) ;
#75440 = VERTEX_POINT ( 'NONE', #38537 ) ;
#75441 = PRESENTATION_STYLE_ASSIGNMENT (( #77581 ) ) ;
#75442 = CARTESIAN_POINT ( 'NONE',  ( 102.0795561180093358, -38.44427582207561045, 199.6449008483751584 ) ) ;
#75443 = CARTESIAN_POINT ( 'NONE',  ( 64.78349330513380266, 6.975173280561618775E-15, 0.000000000000000000 ) ) ;
#75444 = CARTESIAN_POINT ( 'NONE',  ( -5.911416617705733678, 51.88615443309979014, -6.184768123105757631 ) ) ;
#75445 = LINE ( 'NONE', #99176, #30710 ) ;
#75446 = CARTESIAN_POINT ( 'NONE',  ( 9.797174393178825657E-16, -5.000000000000000000, -8.000000000000000000 ) ) ;
#75447 = CARTESIAN_POINT ( 'NONE',  ( 87.64837357284261543, -29.99999999999999289, 185.8567712199668449 ) ) ;
#75448 = CARTESIAN_POINT ( 'NONE',  ( -11.49328356257545991, 43.46445839595169502, -13.79613624638143676 ) ) ;
#75449 = CARTESIAN_POINT ( 'NONE',  ( -35.97769258149595117, 482.2767054324580727, 15.66024800223706315 ) ) ;
#75450 = MECHANICAL_DESIGN_GEOMETRIC_PRESENTATION_REPRESENTATION (  '', ( #3165 ), #53065 ) ;
#75451 = ORIENTED_EDGE ( 'NONE', *, *, #29696, .F. ) ;
#75452 = ORIENTED_EDGE ( 'NONE', *, *, #95120, .T. ) ;
#75453 = CARTESIAN_POINT ( 'NONE',  ( 53.14594722454222619, -32.56895425823870482, 53.87332140664673830 ) ) ;
#75454 = DIRECTION ( 'NONE',  ( 0.000000000000000000, -1.000000000000000000, 0.000000000000000000 ) ) ;
#75455 = CARTESIAN_POINT ( 'NONE',  ( -7.500000000000008882, 42.00000000000000711, -70.16688272716517361 ) ) ;
#75456 = ORIENTED_EDGE ( 'NONE', *, *, #68361, .F. ) ;
#75458 = EDGE_CURVE ( 'NONE', #54691, #50266, #6670, .T. ) ;
#75457 = CARTESIAN_POINT ( 'NONE',  ( -90.65532507562996045, -38.34410233969092019, 9.200892734119188177 ) ) ;
#75459 = CONICAL_SURFACE ( 'NONE', #29025, 6.499999999999999112, 1.047197551196600296 ) ;
#75460 = VERTEX_POINT ( 'NONE', #87613 ) ;
#75461 = CARTESIAN_POINT ( 'NONE',  ( 1.405425595346621037E-06, -60.00000000000000000, -42.63907915653317104 ) ) ;
#75462 = CARTESIAN_POINT ( 'NONE',  ( 108.2517954523928267, -38.35773579516970955, 192.2690374787310077 ) ) ;
#75463 = CARTESIAN_POINT ( 'NONE',  ( 13.10137785350333672, 21.81893118045620028, -4.741824893705198107 ) ) ;
#75464 = CARTESIAN_POINT ( 'NONE',  ( 87.44082029972511805, -60.14831745977613764, 34.29351510052578789 ) ) ;
#75465 = CARTESIAN_POINT ( 'NONE',  ( -4.905843853654967113, -4.999999999999999112, -16.52456679617691293 ) ) ;
#75466 = CARTESIAN_POINT ( 'NONE',  ( -5.036189803708995605, -3.000000000000002665, -76.26213611645742674 ) ) ;
#75467 = CARTESIAN_POINT ( 'NONE',  ( 5.175128423391567978, -10.69566144610013225, -10.53077195007407596 ) ) ;
#75468 = AXIS2_PLACEMENT_3D ( 'NONE', #63133, #13494, #98659 ) ;
#75469 = EDGE_CURVE ( 'NONE', #78207, #7327, #43725, .T. ) ;
#75470 = CARTESIAN_POINT ( 'NONE',  ( -2.499999999999999112, -9.944422831621025693, 19.25618869330389060 ) ) ;
#75471 = FACE_OUTER_BOUND ( 'NONE', #50739, .T. ) ;
#75472 = ORIENTED_EDGE ( 'NONE', *, *, #87507, .F. ) ;
#75473 = CARTESIAN_POINT ( 'NONE',  ( 61.25147495611365400, -39.48591661841823708, 75.53939267858287110 ) ) ;
#75474 = EDGE_CURVE ( 'NONE', #9148, #86058, #61736, .T. ) ;
#75475 = DIRECTION ( 'NONE',  ( -1.000000000000000000, -1.224606353822377258E-16, -0.000000000000000000 ) ) ;
#75476 = LINE ( 'NONE', #76005, #71178 ) ;
#75477 = CARTESIAN_POINT ( 'NONE',  ( -36.77630017244687366, 485.3194367660009902, -3.124714951674963270 ) ) ;
#75478 = CIRCLE ( 'NONE', #8338, 5.000000000000010658 ) ;
#75479 = CARTESIAN_POINT ( 'NONE',  ( -40.24268529043574461, 341.6860726634804450, 21.00658913394816452 ) ) ;
#75480 = CARTESIAN_POINT ( 'NONE',  ( 2.503857664561936320E-16, -8.660254037844401509, -7.422398894150040505 ) ) ;
#75481 = CARTESIAN_POINT ( 'NONE',  ( 3.313708498984704320, -22.71874999999999645, -8.000000000000056843 ) ) ;
#75483 = EDGE_CURVE ( 'NONE', #29730, #90336, #22371, .T. ) ;
#75482 = CARTESIAN_POINT ( 'NONE',  ( -8.000000000000000000, -29.84374999999999289, -3.313708498984762496 ) ) ;
#75484 = CARTESIAN_POINT ( 'NONE',  ( 13.11091740201548284, -14.49516756936109374, 31.73904586483237367 ) ) ;
#75485 = COLOUR_RGB ( '', 0.08235294, 0.09019608, 0.10196078) ;
#75486 = ORIENTED_EDGE ( 'NONE', *, *, #23428, .T. ) ;
#75487 = CARTESIAN_POINT ( 'NONE',  ( 83.69513508649264111, -46.54032163251969223, 183.4101359782732743 ) ) ;
#75488 = CARTESIAN_POINT ( 'NONE',  ( 21.08349330513380337, 1.593028355512270567E-15, 0.000000000000000000 ) ) ;
#75489 = CARTESIAN_POINT ( 'NONE',  ( -38.53630335303979848, 439.2832101125267172, 23.70088186842717803 ) ) ;
#75490 = ORIENTED_EDGE ( 'NONE', *, *, #81811, .T. ) ;
#75491 = CYLINDRICAL_SURFACE ( 'NONE', #49723, 4.000000000000001776 ) ;
#75492 = CARTESIAN_POINT ( 'NONE',  ( 0.000000000000000000, 0.000000000000000000, -9.274828571428571422 ) ) ;
#75493 = SURFACE_STYLE_USAGE ( .BOTH. , #17811 ) ;
#75494 = CARTESIAN_POINT ( 'NONE',  ( 8.857351009221135385, -3.000000000000003109, -97.18047212223504516 ) ) ;
#75495 = CARTESIAN_POINT ( 'NONE',  ( -27.89011194084447354, -28.79345919575957424, -38.26979258636463044 ) ) ;
#75496 = EDGE_CURVE ( 'NONE', #86992, #15625, #30707, .T. ) ;
#75497 = CARTESIAN_POINT ( 'NONE',  ( 43.79854525262764753, -60.00000000000000000, 58.31034945498838340 ) ) ;
#75498 = PRESENTATION_LAYER_ASSIGNMENT (  '', '', ( #42778 ) ) ;
#75499 = AXIS2_PLACEMENT_3D ( 'NONE', #75423, #429, #25314 ) ;
#75500 = DIRECTION ( 'NONE',  ( -1.000000000000000000, 0.000000000000000000, 0.000000000000000000 ) ) ;
#75501 = CARTESIAN_POINT ( 'NONE',  ( 10.41373344803106171, -13.87117582527802817, 31.87275171603477730 ) ) ;
#75502 = EDGE_CURVE ( 'NONE', #42319, #25738, #88142, .T. ) ;
#75503 = CIRCLE ( 'NONE', #94480, 8.900000000000000355 ) ;
#75505 = CARTESIAN_POINT ( 'NONE',  ( -13.77400323909053981, 22.96304823656091543, 1.009181881714518836 ) ) ;
#75504 = CARTESIAN_POINT ( 'NONE',  ( -28.52852425489989585, -31.45698047945067444, 39.78088916245284423 ) ) ;
#75506 = CARTESIAN_POINT ( 'NONE',  ( -1.469576158976823947E-15, -28.06250000409677270, 8.000000000000000000 ) ) ;
#75507 = CARTESIAN_POINT ( 'NONE',  ( 40.17205142263708240, 310.2804317922712016, -6.358608209523628929 ) ) ;
#75508 = EDGE_CURVE ( 'NONE', #91137, #47413, #23420, .T. ) ;
#75509 = FACE_OUTER_BOUND ( 'NONE', #65527, .T. ) ;
#75510 = CIRCLE ( 'NONE', #4928, 0.5000000000000004441 ) ;
#75511 = SURFACE_STYLE_USAGE ( .BOTH. , #49094 ) ;
#75512 = ORIENTED_EDGE ( 'NONE', *, *, #74423, .T. ) ;
#75513 = CARTESIAN_POINT ( 'NONE',  ( 2.054367089437916238, -21.36431346866936920, -38.55161551619058002 ) ) ;
#75514 = CARTESIAN_POINT ( 'NONE',  ( -19.50000000000036593, 50.00000000000000711, 59.91915230424519478 ) ) ;
#75515 = UNCERTAINTY_MEASURE_WITH_UNIT (LENGTH_MEASURE( 1.000000000000000082E-05 ), #72696, 'distance_accuracy_value', 'NONE');
#75516 = CYLINDRICAL_SURFACE ( 'NONE', #82299, 4.000000000000000000 ) ;
#75517 = CARTESIAN_POINT ( 'NONE',  ( 36.97266421100042066, 437.4722577376851973, 4.366281382753225415 ) ) ;
#75519 = CARTESIAN_POINT ( 'NONE',  ( 53.90248938814917778, -47.40883931113200589, -29.08432012930690647 ) ) ;
#75518 = CARTESIAN_POINT ( 'NONE',  ( 5.207846658090203640, 54.22815785865637395, 6.031152949374456007 ) ) ;
#75520 = ORIENTED_EDGE ( 'NONE', *, *, #22484, .T. ) ;
#75521 = AXIS2_PLACEMENT_3D ( 'NONE', #17318, #50193, #83095 ) ;
#75522 = CARTESIAN_POINT ( 'NONE',  ( -5.909259836070535954, -88.86277204242071548, -1.072443315311454981 ) ) ;
#75523 = FILL_AREA_STYLE_COLOUR ( '', #46232 ) ;
#75524 = ORIENTED_EDGE ( 'NONE', *, *, #86503, .F. ) ;
#75525 = DIRECTION ( 'NONE',  ( 0.000000000000000000, -1.000000000000000000, 0.000000000000000000 ) ) ;
#75526 = AXIS2_PLACEMENT_3D ( 'NONE', #7504, #88982, #63662 ) ;
#75527 = CARTESIAN_POINT ( 'NONE',  ( -5.420469775605654128, 41.88321586335170821, -59.04137891894603030 ) ) ;
#75528 = VECTOR ( 'NONE', #49362, 1000.000000000000000 ) ;
#75529 = CARTESIAN_POINT ( 'NONE',  ( -10.00000000000000000, 0.000000000000000000, 10.00000000000000178 ) ) ;
#75530 = CARTESIAN_POINT ( 'NONE',  ( -100.9373344200095772, -60.00000000000000000, 86.53253016253701446 ) ) ;
#75531 = CARTESIAN_POINT ( 'NONE',  ( 37.33349330513379982, -7.703719777548943412E-31, 4.000000000000001776 ) ) ;
#75532 = DIRECTION ( 'NONE',  ( -1.000000000000000000, -0.000000000000000000, -0.000000000000000000 ) ) ;
#75533 = CARTESIAN_POINT ( 'NONE',  ( 37.54559764570182523, 464.1143081516207189, 19.43664670202678835 ) ) ;
#75534 = CARTESIAN_POINT ( 'NONE',  ( 42.23079339798729848, 460.7352525929352964, 2.726051457480590745 ) ) ;
#75536 = CARTESIAN_POINT ( 'NONE',  ( -15.35683281173281500, 2.987586243231799443, -2.780571802872013887 ) ) ;
#75535 = CARTESIAN_POINT ( 'NONE',  ( -33.97359119245064107, 434.1099241184709285, 11.80501937577160021 ) ) ;
#75537 = VECTOR ( 'NONE', #37584, 1000.000000000000000 ) ;
#75538 = CARTESIAN_POINT ( 'NONE',  ( -82.71515938753303487, -42.97701944449982392, 172.7384417419264082 ) ) ;
#75539 = ORIENTED_EDGE ( 'NONE', *, *, #50775, .T. ) ;
#75540 =( NAMED_UNIT ( * ) PLANE_ANGLE_UNIT ( ) SI_UNIT ( $, .RADIAN. ) );
#75541 = ORIENTED_EDGE ( 'NONE', *, *, #4191, .T. ) ;
#75542 = ORIENTED_EDGE ( 'NONE', *, *, #92928, .F. ) ;
#75543 = DIRECTION ( 'NONE',  ( -1.000000000000000000, -1.224606353822377258E-16, -0.000000000000000000 ) ) ;
#75544 = EDGE_CURVE ( 'NONE', #9203, #37220, #34802, .T. ) ;
#75545 = DIRECTION ( 'NONE',  ( -0.000000000000000000, 1.000000000000000000, -0.000000000000000000 ) ) ;
#75546 = ADVANCED_BREP_SHAPE_REPRESENTATION ( '', ( #54736, #10728 ), #93449 ) ;
#75547 = ORIENTED_EDGE ( 'NONE', *, *, #48976, .T. ) ;
#75548 = CARTESIAN_POINT ( 'NONE',  ( 32.03352823755274414, 487.4857469360636060, 8.014200094826978926 ) ) ;
#75549 = CARTESIAN_POINT ( 'NONE',  ( 23.58349330513380337, 1.593028355512270962E-15, 0.000000000000000000 ) ) ;
#75550 = AXIS2_PLACEMENT_3D ( 'NONE', #58277, #51230, #49107 ) ;
#75551 = CARTESIAN_POINT ( 'NONE',  ( -7.003653396366579464, -63.94293794440324064, -3.866846144092871196 ) ) ;
#75552 = CARTESIAN_POINT ( 'NONE',  ( -0.3345853057524721952, 54.28960170381152750, 7.792663449346018290 ) ) ;
#75553 = SURFACE_SIDE_STYLE ('',( #27050 ) ) ;
#75554 = CARTESIAN_POINT ( 'NONE',  ( -5.000000000000000000, -14.43224336012844589, 12.18680852295256933 ) ) ;
#75555 = EDGE_CURVE ( 'NONE', #90250, #22641, #104300, .T. ) ;
#75556 = CARTESIAN_POINT ( 'NONE',  ( 92.03798523278891253, -30.00000000000002842, 46.84723268580137301 ) ) ;
#75557 =( BOUNDED_SURFACE ( )  B_SPLINE_SURFACE ( 2, 3, ( 
 ( #101035, #19106, #4470, #10940, #29316, #11477, #45476, #43862 ),
 ( #60080, #102637, #51416, #92944, #10425, #44951, #51944, #35816 ),
 ( #69225, #37409, #43339, #94014, #70273, #76754, #36876, #68696 ) ),
 .UNSPECIFIED., .F., .F., .F. ) 
 B_SPLINE_SURFACE_WITH_KNOTS ( ( 3, 3 ),
 ( 4, 2, 2, 4 ),
 ( 0.000000000000000000, 1.000000000000000000 ),
 ( 5.707226654021456902, 5.953728167561664009, 6.612642446797508455, 6.859143960337715562 ),
 .UNSPECIFIED. ) 
 GEOMETRIC_REPRESENTATION_ITEM ( )  RATIONAL_B_SPLINE_SURFACE ( (
 ( 1.000000000000000000, 1.000000000000000000, 1.000000000000000000, 1.000000000000000000, 1.000000000000000000, 1.000000000000000000, 1.000000000000000000, 1.000000000000000000),
 ( 1.857142857142858317, 1.857142857142858317, 1.857142857142858317, 1.857142857142858317, 1.857142857142858317, 1.857142857142858317, 1.857142857142858317, 1.857142857142858317),
 ( 1.000000000000000000, 1.000000000000000000, 1.000000000000000000, 1.000000000000000000, 1.000000000000000000, 1.000000000000000000, 1.000000000000000000, 1.000000000000000000) ) ) 
 REPRESENTATION_ITEM ( '' )  SURFACE ( )  );
#75558 = CARTESIAN_POINT ( 'NONE',  ( -72.58684158890253002, -59.99999999999995026, 181.3884362157535008 ) ) ;
#75559 = CARTESIAN_POINT ( 'NONE',  ( -58.21460221941013202, -39.49442887122282997, 67.71575742886867033 ) ) ;
#75560 = VERTEX_POINT ( 'NONE', #6134 ) ;
#75561 = CARTESIAN_POINT ( 'NONE',  ( 6.241401647512419437, 15.44846771700987809, 3.173604836376809679 ) ) ;
#75562 = CARTESIAN_POINT ( 'NONE',  ( 77.24101806708192441, -59.99999999999518252, -32.07091152847338122 ) ) ;
#75563 = ORIENTED_EDGE ( 'NONE', *, *, #28464, .T. ) ;
#75564 = CARTESIAN_POINT ( 'NONE',  ( 7.180584945291298204, -46.43466603162036677, 31.61912980851609589 ) ) ;
#75565 = CARTESIAN_POINT ( 'NONE',  ( -103.1989685349693673, -52.71063798620885166, 189.5257644198029539 ) ) ;
#75566 = FACE_OUTER_BOUND ( 'NONE', #22775, .T. ) ;
#75567 = PRESENTATION_STYLE_ASSIGNMENT (( #27599 ) ) ;
#75569 = CARTESIAN_POINT ( 'NONE',  ( 0.000000000000000000, 50.50000000000000000, 0.000000000000000000 ) ) ;
#75568 = AXIS2_PLACEMENT_3D ( 'NONE', #8256, #49780, #51367 ) ;
#75570 = ORIENTED_EDGE ( 'NONE', *, *, #22073, .T. ) ;
#75571 = CARTESIAN_POINT ( 'NONE',  ( -4.464296094009080562, -13.01099471650159600, -0.1149164202474959318 ) ) ;
#75572 = CARTESIAN_POINT ( 'NONE',  ( -39.86639569183807907, -59.99999999999998579, 51.86916670227435588 ) ) ;
#75573 = CARTESIAN_POINT ( 'NONE',  ( -3.564365538402600730, -1.135065884989842067, 104.5953911288829659 ) ) ;
#75574 = CARTESIAN_POINT ( 'NONE',  ( 4.401442555609581635E-16, -19.15625000204838457, -7.188101187500000044 ) ) ;
#75575 = DIRECTION ( 'NONE',  ( 1.000000000000000000, 0.000000000000000000, 0.000000000000000000 ) ) ;
#75576 = CARTESIAN_POINT ( 'NONE',  ( 16.14668631625571393, -0.000000000000000000, 5.483261958891903376 ) ) ;
#75577 = CARTESIAN_POINT ( 'NONE',  ( -23.96375140441108442, 306.3052962357393199, 10.25885168886986243 ) ) ;
#75578 = CARTESIAN_POINT ( 'NONE',  ( 25.95507789760542039, 309.1386286255022924, 10.94030088463808070 ) ) ;
#75579 =( NAMED_UNIT ( * ) SI_UNIT ( $, .STERADIAN. ) SOLID_ANGLE_UNIT ( ) );
#75580 = CARTESIAN_POINT ( 'NONE',  ( 25.59999999999999787, -3.309499999999999886, 4.475777889183790779E-16 ) ) ;
#75581 = EDGE_CURVE ( 'NONE', #8034, #94433, #32575, .T. ) ;
#75582 = CARTESIAN_POINT ( 'NONE',  ( 99.13158141131964385, -59.99999999999998579, 109.9887192217465213 ) ) ;
#75583 = CARTESIAN_POINT ( 'NONE',  ( -29.95191136813465604, -18.65114050358700837, 29.35552943215963850 ) ) ;
#75584 = CARTESIAN_POINT ( 'NONE',  ( -4.174999999999998934, 5.112900386440198549E-16, -0.5776712190230098853 ) ) ;
#75585 = CARTESIAN_POINT ( 'NONE',  ( 44.80321014283884296, -42.98249604127523327, 44.34580923176882550 ) ) ;
#75586 = ORIENTED_EDGE ( 'NONE', *, *, #33515, .T. ) ;
#75587 = AXIS2_PLACEMENT_3D ( 'NONE', #105077, #39290, #72169 ) ;
#75588 = CARTESIAN_POINT ( 'NONE',  ( 43.71217423904119670, 435.6632154632235938, 9.092528312217329045 ) ) ;
#75590 = EDGE_CURVE ( 'NONE', #97744, #66787, #21547, .T. ) ;
#75589 = CARTESIAN_POINT ( 'NONE',  ( -76.83632878065965599, -38.44263010941451597, 183.5527664238933596 ) ) ;
#75591 = EDGE_LOOP ( 'NONE', ( #103974, #58844 ) ) ;
#75593 = CARTESIAN_POINT ( 'NONE',  ( 39.13885763974980136, 324.4948203046521371, 17.18769520460729439 ) ) ;
#75592 = DIRECTION ( 'NONE',  ( 1.000000000000000000, 0.000000000000000000, 0.000000000000000000 ) ) ;
#75594 = CARTESIAN_POINT ( 'NONE',  ( 79.51214466678966630, -60.00000000000007105, 169.4709273215115388 ) ) ;
#75595 = CARTESIAN_POINT ( 'NONE',  ( 16.58616928888088182, 36.42044334926447391, 24.29863715439284633 ) ) ;
#75596 = CARTESIAN_POINT ( 'NONE',  ( -6.931965282482035917, 41.62850913407595499, -59.01894715436439753 ) ) ;
#75597 = CIRCLE ( 'NONE', #103165, 9.999999999999998224 ) ;
#75598 = CARTESIAN_POINT ( 'NONE',  ( 9.246279647933182133, 15.99999999999999645, -3.826931552919425439 ) ) ;
#75599 = DIRECTION ( 'NONE',  ( 1.000000000000000000, 1.224606353822377258E-16, 0.000000000000000000 ) ) ;
#75600 = CARTESIAN_POINT ( 'NONE',  ( -24.35993018935220533, 306.6204276456223852, 9.332123231157906318 ) ) ;
#75601 = CARTESIAN_POINT ( 'NONE',  ( 17.83392795039140566, 45.30293236282059866, 5.798433727367392265 ) ) ;
#75602 = CARTESIAN_POINT ( 'NONE',  ( 106.3525110532974480, -60.00000000000000000, 118.5997609402804756 ) ) ;
#75603 = CARTESIAN_POINT ( 'NONE',  ( 82.42421628608209971, -5.000000000000000000, 6.123233995736778115E-16 ) ) ;
#75604 = ORIENTED_EDGE ( 'NONE', *, *, #71528, .T. ) ;
#75605 = EDGE_CURVE ( 'NONE', #57621, #30532, #23965, .T. ) ;
#75606 = AXIS2_PLACEMENT_3D ( 'NONE', #28622, #86318, #21582 ) ;
#75607 = CARTESIAN_POINT ( 'NONE',  ( -100.9483554910953416, -29.99999999999999289, 178.8210981605607799 ) ) ;
#75608 = ORIENTED_EDGE ( 'NONE', *, *, #102592, .T. ) ;
#75609 = CARTESIAN_POINT ( 'NONE',  ( 5.075566108724593128, -4.332661967060489339, -17.09624963492156269 ) ) ;
#75610 = CARTESIAN_POINT ( 'NONE',  ( 42.36808196472509991, 461.6713445545159971, 3.771400599639967322 ) ) ;
#75611 = CARTESIAN_POINT ( 'NONE',  ( 20.74847835458628964, 303.9423534201437747, 9.956307716536178631 ) ) ;
#75612 = DIRECTION ( 'NONE',  ( 0.000000000000000000, 0.000000000000000000, 1.000000000000000000 ) ) ;
#75613 = CARTESIAN_POINT ( 'NONE',  ( 4.401442555609581635E-16, -19.15625000204838457, -7.188101187500000044 ) ) ;
#75614 = AXIS2_PLACEMENT_3D ( 'NONE', #72411, #23358, #105315 ) ;
#75615 = CARTESIAN_POINT ( 'NONE',  ( 30.25691101598778943, 17.21809272184238893, -39.73659737107644219 ) ) ;
#75616 = AXIS2_PLACEMENT_3D ( 'NONE', #102770, #4078, #45612 ) ;
#75618 = ORIENTED_EDGE ( 'NONE', *, *, #38803, .F. ) ;
#75617 = PRESENTATION_STYLE_ASSIGNMENT (( #58920 ) ) ;
#75619 = CARTESIAN_POINT ( 'NONE',  ( 80.00145041154991077, -60.36562354243974227, 175.0908152758545668 ) ) ;
#75620 = CARTESIAN_POINT ( 'NONE',  ( -46.00000000000000000, 460.1242873147282353, 6.750975842490332113 ) ) ;
#75621 = AXIS2_PLACEMENT_3D ( 'NONE', #23899, #6605, #40047 ) ;
#75622 = ORIENTED_EDGE ( 'NONE', *, *, #37880, .T. ) ;
#75623 = CARTESIAN_POINT ( 'NONE',  ( 0.000000000000000000, 0.000000000000000000, 0.000000000000000000 ) ) ;
#75624 = CARTESIAN_POINT ( 'NONE',  ( 84.73333333333332007, 4.172000000000019249, 0.000000000000000000 ) ) ;
#75625 = CARTESIAN_POINT ( 'NONE',  ( 32.16914446836155861, 486.0693400665549007, 5.247150504716460162 ) ) ;
#75626 = FACE_OUTER_BOUND ( 'NONE', #2244, .T. ) ;
#75627 = CARTESIAN_POINT ( 'NONE',  ( -33.13214351254949719, 379.6169617581111879, 24.74988620700858633 ) ) ;
#75628 = CARTESIAN_POINT ( 'NONE',  ( -31.73507068214536631, 436.7267398747721359, 21.10082163792574406 ) ) ;
#75629 = EDGE_CURVE ( 'NONE', #54822, #13028, #64917, .T. ) ;
#75630 = VERTEX_POINT ( 'NONE', #46607 ) ;
#75631 = FACE_OUTER_BOUND ( 'NONE', #57536, .T. ) ;
#75632 = CLOSED_SHELL ( 'NONE', ( #5091, #31767, #27022, #12503, #16205, #41211, #4876, #80292, #16821, #57892, #12028, #32848, #52953, #74547, #90627, #12710, #56539, #37929, #72220, #6479, #96165, #42601, #88517, #87249, #57925, #4820, #99404, #54826, #88060, #45592, #105434, #96244, #34934, #71344, #28569, #91073, #1849, #16977, #23422, #42993, #66577, #16380, #52184, #28036, #3480, #76354, #30988, #98886, #71568, #83210, #19078, #68512, #103207, #102434, #8609, #103665, #28789, #58062, #48828, #89777, #16608, #15865, #11105, #71608, #4482, #50922, #36635, #68918, #88926, #50964, #68854, #98044, #32016, #97296, #47044, #57631, #86743, #79316, #98357, #10878, #66253, #11352, #63362, #66031, #5702, #78755, #55024, #31639, #21795, #45482, #1523, #44613, #33371, #89833, #104966, #22519, #87320, #7318, #106424, #52157, #82219, #23676, #89802, #48420, #22206, #9795, #38103, #14496, #30316, #105473, #6794, #39584, #6127, #63792, #33949, #52828, #32923, #93920, #27649, #88071, #39289, #1714, #7726, #49472, #8537, #7017, #60397, #58201, #98602, #50326, #57758, #42278, #77105, #66919, #25860, #34222, #75070, #81952, #25982, #18573, #44126, #50528, #63315, #86260, #45204, #101291, #74069, #14771, #103304, #303, #46208, #84721, #5574, #89272, #31408, #70499, #22342, #34293, #12783, #89969, #96885, #47041, #52008, #57218, #5903, #49329, #89784, #14132, #81575, #67358, #3082, #102190, #22813, #103668, #4611, #95034, #36155, #88270, #78495, #76764, #50802, #13972, #84219 ) ) ;
#75633 = CARTESIAN_POINT ( 'NONE',  ( 15.30771400658271908, 18.64284798592852965, 35.25047262264993719 ) ) ;
#75634 = CARTESIAN_POINT ( 'NONE',  ( 87.15768292724222022, -24.32275648668401047, 187.0112092941248534 ) ) ;
#75635 = EDGE_CURVE ( 'NONE', #30914, #25416, #106415, .T. ) ;
#75636 = DIRECTION ( 'NONE',  ( 0.000000000000000000, -1.000000000000000000, 0.000000000000000000 ) ) ;
#75637 = CARTESIAN_POINT ( 'NONE',  ( 7.188101187499999156, -32.75000000204839523, 2.977408999572654924 ) ) ;
#75638 = LINE ( 'NONE', #18497, #71541 ) ;
#75639 = CARTESIAN_POINT ( 'NONE',  ( 16.84999999999999787, 3.309500000000003439, 0.000000000000000000 ) ) ;
#75640 = AXIS2_PLACEMENT_3D ( 'NONE', #51900, #43816, #12496 ) ;
#75641 = DIRECTION ( 'NONE',  ( -1.000000000000000000, -1.224606353822377258E-16, -0.000000000000000000 ) ) ;
#75642 = CONTEXT_DEPENDENT_SHAPE_REPRESENTATION ( #60380, #94011 ) ;
#75643 = ORIENTED_EDGE ( 'NONE', *, *, #57229, .T. ) ;
#75644 = ADVANCED_FACE ( 'NONE', ( #33105 ), #52, .F. ) ;
#75645 = FACE_OUTER_BOUND ( 'NONE', #70726, .T. ) ;
#75646 = CARTESIAN_POINT ( 'NONE',  ( -5.888827218543791986, 4.654238857465189838, -4.999999999999999112 ) ) ;
#75647 =( NAMED_UNIT ( * ) PLANE_ANGLE_UNIT ( ) SI_UNIT ( $, .RADIAN. ) );
#75648 = ORIENTED_EDGE ( 'NONE', *, *, #63460, .T. ) ;
#75649 = CARTESIAN_POINT ( 'NONE',  ( -4.852941176470593199, 24.91666666666666430, -70.80672828634229177 ) ) ;
#75650 = CIRCLE ( 'NONE', #51558, 14.00000000000000000 ) ;
#75651 = CARTESIAN_POINT ( 'NONE',  ( 32.42201911889981858, 435.8451540523121821, 18.25951462285809868 ) ) ;
#75652 = CARTESIAN_POINT ( 'NONE',  ( -0.8349010936846665842, 12.93338910046981383, -49.56652387900988543 ) ) ;
#75653 = DIRECTION ( 'NONE',  ( 0.000000000000000000, -1.000000000000000000, 0.000000000000000000 ) ) ;
#75654 = SURFACE_STYLE_FILL_AREA ( #91335 ) ;
#75655 = CARTESIAN_POINT ( 'NONE',  ( -87.15574825653149560, -60.00000000000000711, 201.0783104021778342 ) ) ;
#75656 = AXIS2_PLACEMENT_3D ( 'NONE', #86436, #35229, #12500 ) ;
#75657 = TOROIDAL_SURFACE ( 'NONE', #96336, 12.00000000000003908, 1.000000000000000000 ) ;
#75658 = CARTESIAN_POINT ( 'NONE',  ( -7.500000000000000888, -3.000671055698259870, -20.99923901233272971 ) ) ;
#75659 = CARTESIAN_POINT ( 'NONE',  ( 55.00571552735602410, 6.975173280561618775E-15, 0.000000000000000000 ) ) ;
#75660 = FACE_OUTER_BOUND ( 'NONE', #69172, .T. ) ;
#75661 = CARTESIAN_POINT ( 'NONE',  ( -85.48278714503372555, -32.15310639930356018, 180.9904824015285385 ) ) ;
#75662 = EDGE_LOOP ( 'NONE', ( #55571, #51041, #12892, #88044, #35121 ) ) ;
#75663 = CARTESIAN_POINT ( 'NONE',  ( -5.124339073201918282, 53.50653926859659748, -8.531152949374524397 ) ) ;
#75664 = ORIENTED_EDGE ( 'NONE', *, *, #24718, .T. ) ;
#75665 = CARTESIAN_POINT ( 'NONE',  ( 4.898587196589412829E-16, -25.62499999999999645, -8.000000000000000000 ) ) ;
#75666 = EDGE_CURVE ( 'NONE', #9879, #83820, #8258, .T. ) ;
#75667 = CARTESIAN_POINT ( 'NONE',  ( 3.454253436624934892, -0.8414180287960449922, 103.7259032015043232 ) ) ;
#75668 = CARTESIAN_POINT ( 'NONE',  ( -84.03992301111506436, -45.26188587547530773, -11.64691007556465507 ) ) ;
#75669 = VECTOR ( 'NONE', #48864, 1000.000000000000000 ) ;
#75670 = CARTESIAN_POINT ( 'NONE',  ( -3.216749358080555954, -8.903395928605739584, -12.12543985758685672 ) ) ;
#75671 = ORIENTED_EDGE ( 'NONE', *, *, #4016, .T. ) ;
#75672 = CARTESIAN_POINT ( 'NONE',  ( -12.73573943988818336, -9.919073743022268630, 11.26376837308747803 ) ) ;
#75673 = CARTESIAN_POINT ( 'NONE',  ( -5.961320375100140012, -13.36618214390666814, 13.51689209302656813 ) ) ;
#75674 = CARTESIAN_POINT ( 'NONE',  ( 79.13121736037263076, 42.00000000000000000, 45.60838156036771096 ) ) ;
#75675 = EDGE_CURVE ( 'NONE', #18398, #105603, #96120, .T. ) ;
#75676 = ADVANCED_FACE ( 'NONE', ( #90791 ), #67581, .F. ) ;
#75677 = CARTESIAN_POINT ( 'NONE',  ( 32.09911992168216699, 438.9232547152094526, 23.66653216045977359 ) ) ;
#75678 = CARTESIAN_POINT ( 'NONE',  ( 57.89978660429063240, -59.99999999999999289, 101.6248911977562699 ) ) ;
#75679 = AXIS2_PLACEMENT_3D ( 'NONE', #74605, #685, #26125 ) ;
#75680 = FILL_AREA_STYLE_COLOUR ( '', #32504 ) ;
#75681 = CARTESIAN_POINT ( 'NONE',  ( -65.68019474265784652, -30.00000000000001776, -31.25134080541240422 ) ) ;
#75682 = CARTESIAN_POINT ( 'NONE',  ( -74.82224136490378896, -42.96559528526920246, 122.4759379343339134 ) ) ;
#75683 = VERTEX_POINT ( 'NONE', #41700 ) ;
#75684 = CARTESIAN_POINT ( 'NONE',  ( 69.27313422356952799, -59.99999999999999289, 151.6321682696899984 ) ) ;
#75685 = CARTESIAN_POINT ( 'NONE',  ( -64.33158975147043179, 40.83917765566846469, 9.759077203600947215 ) ) ;
#75686 = CARTESIAN_POINT ( 'NONE',  ( 42.26132763977452100, -59.99999999999998579, 60.38387368011249379 ) ) ;
#75687 = VERTEX_POINT ( 'NONE', #90252 ) ;
#75688 = DIRECTION ( 'NONE',  ( -1.000000000000000000, -1.224606353822377258E-16, -0.000000000000000000 ) ) ;
#75689 = CARTESIAN_POINT ( 'NONE',  ( 2.977408999572652260, -25.81250000204838813, 7.188101187500000044 ) ) ;
#75690 = AXIS2_PLACEMENT_3D ( 'NONE', #65767, #80336, #98126 ) ;
#75691 = DIRECTION ( 'NONE',  ( -1.000000000000000000, -1.224606353822377258E-16, -0.000000000000000000 ) ) ;
#75692 = ORIENTED_EDGE ( 'NONE', *, *, #4331, .T. ) ;
#75693 = DIRECTION ( 'NONE',  ( 0.8660254037844372643, 0.5000000000000024425, 0.000000000000000000 ) ) ;
#75694 = LINE ( 'NONE', #57372, #99244 ) ;
#75695 = LINE ( 'NONE', #1794, #12683 ) ;
#75696 = CARTESIAN_POINT ( 'NONE',  ( 24.00188669994001600, 304.6317240716171000, -9.832141748992357932 ) ) ;
#75697 = CARTESIAN_POINT ( 'NONE',  ( -5.082755093536325042, -12.59375000204838280, -5.082755093536325930 ) ) ;
#75698 = CARTESIAN_POINT ( 'NONE',  ( -8.000000000000000000, -17.93750000409676915, -9.797174393178825657E-16 ) ) ;
#75699 =( BOUNDED_CURVE ( )  B_SPLINE_CURVE ( 2, ( #17849, #93322, #85223, #101932, #67979, #44785, #27028, #60967, #92233 ),
 .UNSPECIFIED., .F., .F. ) 
 B_SPLINE_CURVE_WITH_KNOTS ( ( 3, 2, 2, 2, 3 ),
 ( 0.3676470588235294379, 0.3750000000000000000, 0.3823529411764705621, 0.3897058823529412352, 0.3970588235294117974 ),
 .UNSPECIFIED. ) 
 CURVE ( )  GEOMETRIC_REPRESENTATION_ITEM ( )  RATIONAL_B_SPLINE_CURVE ( ( 1.000000000000000000, 0.9238795325112867385, 1.000000000000000000, 0.9238795325112867385, 1.000000000000000000, 0.9238795325112867385, 1.000000000000000000, 0.9238795325112861834, 1.000000000000000666 ) ) 
 REPRESENTATION_ITEM ( '' )  );
#75700 = CARTESIAN_POINT ( 'NONE',  ( 3.040119806627095578, -0.8312265419168590741, 104.0101162232625995 ) ) ;
#75701 = DIRECTION ( 'NONE',  ( -0.000000000000000000, -1.000000000000000000, -0.000000000000000000 ) ) ;
#75702 = DIRECTION ( 'NONE',  ( -0.000000000000000000, -1.000000000000000000, -0.000000000000000000 ) ) ;
#75703 = CARTESIAN_POINT ( 'NONE',  ( -1.177401751624803428, 48.00000000000000711, -100.0000000000000142 ) ) ;
#75704 = ADVANCED_FACE ( 'NONE', ( #74583 ), #2279, .T. ) ;
#75705 = UNCERTAINTY_MEASURE_WITH_UNIT (LENGTH_MEASURE( 1.000000000000000082E-05 ), #15752, 'distance_accuracy_value', 'NONE');
#75706 = STYLED_ITEM ( 'NONE', ( #77088 ), #77159 ) ;
#75707 = VERTEX_POINT ( 'NONE', #51371 ) ;
#75708 = CARTESIAN_POINT ( 'NONE',  ( -7.392085442450220256, 40.93519827090806729, -70.13194593521265574 ) ) ;
#75710 = CARTESIAN_POINT ( 'NONE',  ( 31.50514675153943855, -25.60841695546642782, 31.14698023900106350 ) ) ;
#75709 =( NAMED_UNIT ( * ) SI_UNIT ( $, .STERADIAN. ) SOLID_ANGLE_UNIT ( ) );
#75711 = CARTESIAN_POINT ( 'NONE',  ( 35.41856067487186976, 369.9239349834528525, 4.703027911095471580 ) ) ;
#75712 = ORIENTED_EDGE ( 'NONE', *, *, #45550, .T. ) ;
#75713 = ADVANCED_FACE ( 'NONE', ( #659 ), #91772, .T. ) ;
#75714 = CARTESIAN_POINT ( 'NONE',  ( -1.231557862076259280, 16.44676558348158224, 50.25324543889210815 ) ) ;
#75715 = AXIS2_PLACEMENT_3D ( 'NONE', #80070, #37543, #13206 ) ;
#75716 = EDGE_LOOP ( 'NONE', ( #11760, #44666, #39288, #6327, #102484 ) ) ;
#75718 = CARTESIAN_POINT ( 'NONE',  ( -5.062487338738201892, -5.000000000000000888, 8.716223939771381879 ) ) ;
#75717 = CARTESIAN_POINT ( 'NONE',  ( 41.82792046605465686, 1.340359594676612611E-15, 0.000000000000000000 ) ) ;
#75719 = FACE_OUTER_BOUND ( 'NONE', #20237, .T. ) ;
#75720 = DIRECTION ( 'NONE',  ( -1.000000000000000000, -1.224606353822377258E-16, -0.000000000000000000 ) ) ;
#75721 = PRESENTATION_STYLE_ASSIGNMENT (( #25625 ) ) ;
#75722 = CARTESIAN_POINT ( 'NONE',  ( 32.66167952490037152, 465.7843590037583112, 12.50185730157094888 ) ) ;
#75723 = CARTESIAN_POINT ( 'NONE',  ( 0.7810335935915004857, 13.54372500177475835, -51.48049019060625398 ) ) ;
#75724 = ORIENTED_EDGE ( 'NONE', *, *, #65298, .T. ) ;
#75725 = AXIS2_PLACEMENT_3D ( 'NONE', #12257, #27970, #59774 ) ;
#75726 = CARTESIAN_POINT ( 'NONE',  ( 91.76163772444834876, -60.00000000000002132, -14.81080705115953577 ) ) ;
#75727 = CARTESIAN_POINT ( 'NONE',  ( -11.36440886748413881, 45.70401808670207799, -13.50555938308150594 ) ) ;
#75728 = DIRECTION ( 'NONE',  ( 0.000000000000000000, 1.000000000000000000, 0.000000000000000000 ) ) ;
#75729 = CARTESIAN_POINT ( 'NONE',  ( 38.02740175684945001, 490.5688714813351226, 12.25042287455591428 ) ) ;
#75730 = CARTESIAN_POINT ( 'NONE',  ( -48.02835407290534420, 14.94086294439724227, -16.85535821593460426 ) ) ;
#75731 = ORIENTED_EDGE ( 'NONE', *, *, #69696, .F. ) ;
#75732 = DIRECTION ( 'NONE',  ( 1.150791560227848297E-16, -0.3420201433256725987, 0.9396926207859068736 ) ) ;
#75733 = ORIENTED_EDGE ( 'NONE', *, *, #62511, .F. ) ;
#75734 = ORIENTED_EDGE ( 'NONE', *, *, #90948, .F. ) ;
#75735 = CARTESIAN_POINT ( 'NONE',  ( 7.150053860865849487, 83.21734546086022988, 3.590189269391289351 ) ) ;
#75736 =( NAMED_UNIT ( * ) SI_UNIT ( $, .STERADIAN. ) SOLID_ANGLE_UNIT ( ) );
#75737 = DIRECTION ( 'NONE',  ( 0.000000000000000000, -0.9846968979781746123, 0.1742756985702836880 ) ) ;
#75738 = CARTESIAN_POINT ( 'NONE',  ( 9.349999999999997868, 3.309500000000003439, 0.000000000000000000 ) ) ;
#75739 = CARTESIAN_POINT ( 'NONE',  ( 86.65522219368004642, -60.23071133352890882, -11.83452115418482897 ) ) ;
#75740 = CARTESIAN_POINT ( 'NONE',  ( -40.90488780024449511, 312.7491308540076602, -5.736144956087439795 ) ) ;
#75741 = CARTESIAN_POINT ( 'NONE',  ( -6.812116597003051943, 304.7372916636546165, -10.02434008908077345 ) ) ;
#75742 = MECHANICAL_DESIGN_GEOMETRIC_PRESENTATION_REPRESENTATION (  '', ( #48159 ), #24107 ) ;
#75743 =( LENGTH_UNIT ( ) NAMED_UNIT ( * ) SI_UNIT ( .MILLI., .METRE. ) );
#75744 = EDGE_LOOP ( 'NONE', ( #79448, #72293, #29258, #13963, #22924 ) ) ;
#75745 = CARTESIAN_POINT ( 'NONE',  ( -6.499999999999999112, -1.360915494589017838, -5.718331000733962277 ) ) ;
#75746 = ORIENTED_EDGE ( 'NONE', *, *, #84299, .F. ) ;
#75747 = CARTESIAN_POINT ( 'NONE',  ( -7.230783165911326194, -2.999999999999882760, -70.90935356276069967 ) ) ;
#75748 = CARTESIAN_POINT ( 'NONE',  ( 13.09999999999999787, 3.309500000000003439, 0.000000000000000000 ) ) ;
#75750 = EDGE_LOOP ( 'NONE', ( #11768, #57401 ) ) ;
#75749 = CARTESIAN_POINT ( 'NONE',  ( 0.000000000000000000, 0.000000000000000000, -7.554475477074167777 ) ) ;
#75751 = CARTESIAN_POINT ( 'NONE',  ( 74.27602980505658081, -60.31745848623394579, 133.2367107689713066 ) ) ;
#75752 = VERTEX_POINT ( 'NONE', #67047 ) ;
#75753 = CARTESIAN_POINT ( 'NONE',  ( 0.7777777777777719059, -54.00000000000000000, 40.97837836547555668 ) ) ;
#75754 = CARTESIAN_POINT ( 'NONE',  ( 20.97754405179121662, 294.8763868968453608, 9.942224931492262385 ) ) ;
#75755 = CARTESIAN_POINT ( 'NONE',  ( 7.188101187500000044, -23.65625000204838457, 0.000000000000000000 ) ) ;
#75756 = CARTESIAN_POINT ( 'NONE',  ( -94.60030117187078247, -57.66721437216608592, -3.115894729640209526 ) ) ;
#75757 = ADVANCED_FACE ( 'NONE', ( #82146 ), #40732, .T. ) ;
#75758 = ORIENTED_EDGE ( 'NONE', *, *, #15786, .T. ) ;
#75759 = MECHANICAL_DESIGN_GEOMETRIC_PRESENTATION_REPRESENTATION (  '', ( #56804 ), #6917 ) ;
#75760 = SURFACE_SIDE_STYLE ('',( #43406 ) ) ;
#75761 = B_SPLINE_CURVE_WITH_KNOTS ( 'NONE', 3,
 ( #28078, #21055, #93838, #83213, #53893, #86824, #11839, #25556, #36705, #101400 ),
 .UNSPECIFIED., .F., .F.,
 ( 4, 2, 2, 2, 4 ),
 ( 0.000000000000000000, 0.001010458115798221809, 0.002020916231596442750, 0.003031374347394663257, 0.004041832463192884632 ),
 .UNSPECIFIED. ) ;
#75762 = CARTESIAN_POINT ( 'NONE',  ( 0.000000000000000000, 0.000000000000000000, 4.000000000000000888 ) ) ;
#75763 = VECTOR ( 'NONE', #68222, 1000.000000000000000 ) ;
#75764 = CARTESIAN_POINT ( 'NONE',  ( 103.9999019992000342, -45.28271188782171919, 174.9196668792254172 ) ) ;
#75765 = AXIS2_PLACEMENT_3D ( 'NONE', #51634, #52694, #85621 ) ;
#75766 = CARTESIAN_POINT ( 'NONE',  ( -36.32243474800993255, 28.19842941503742750, -12.06008965998136517 ) ) ;
#75767 = DIRECTION ( 'NONE',  ( -1.000000000000000000, -1.224606353822377258E-16, -0.000000000000000000 ) ) ;
#75768 = CARTESIAN_POINT ( 'NONE',  ( -3.313708498984765161, -23.65625000409676915, 7.999999999999998224 ) ) ;
#75769 = CARTESIAN_POINT ( 'NONE',  ( -2.898330757982067934E-15, 60.00000000000000000, 23.66666666666665719 ) ) ;
#75770 = CARTESIAN_POINT ( 'NONE',  ( 42.33349330513380693, -4.000000000000000000, 4.898587196589415787E-16 ) ) ;
#75771 = CIRCLE ( 'NONE', #62019, 5.000000000000002665 ) ;
#75772 = CARTESIAN_POINT ( 'NONE',  ( 0.000000000000000000, -30.00000000000000000, 8.000000000000000000 ) ) ;
#75773 = DIRECTION ( 'NONE',  ( -1.000000000000000000, -0.000000000000000000, -0.000000000000000000 ) ) ;
#75774 = DIRECTION ( 'NONE',  ( -0.000000000000000000, -0.000000000000000000, 1.000000000000000000 ) ) ;
#75775 = DIRECTION ( 'NONE',  ( 1.000000000000000000, 7.806255641895631925E-17, 0.000000000000000000 ) ) ;
#75776 = ORIENTED_EDGE ( 'NONE', *, *, #48512, .F. ) ;
#75777 = CARTESIAN_POINT ( 'NONE',  ( -5.454982624654864054, 41.97810475128825658, -59.40149861125610897 ) ) ;
#75778 = ADVANCED_FACE ( 'NONE', ( #94523 ), #32569, .F. ) ;
#75779 = SURFACE_STYLE_FILL_AREA ( #90912 ) ;
#75780 = DIRECTION ( 'NONE',  ( 0.000000000000000000, 0.000000000000000000, 1.000000000000000000 ) ) ;
#75781 = AXIS2_PLACEMENT_3D ( 'NONE', #19918, #103440, #78616 ) ;
#75782 = CARTESIAN_POINT ( 'NONE',  ( -86.17540505562507747, -30.00000000000000355, 179.7358132287471904 ) ) ;
#75783 = ORIENTED_EDGE ( 'NONE', *, *, #77250, .F. ) ;
#75784 = CONICAL_SURFACE ( 'NONE', #29328, 4.174999999999998934, 0.9599310885968824758 ) ;
#75785 = CARTESIAN_POINT ( 'NONE',  ( -32.82691535583477105, 485.1045372766795367, 1.724905475514941999 ) ) ;
#75786 = CARTESIAN_POINT ( 'NONE',  ( 72.44228326075131008, -57.66666666020200438, 176.4071323493450620 ) ) ;
#75788 = CARTESIAN_POINT ( 'NONE',  ( 7.770228158362351145, 1.340359594676612611E-15, 0.000000000000000000 ) ) ;
#75787 = CARTESIAN_POINT ( 'NONE',  ( -14.65167870846473441, 2.576877453023403319, -3.244758155282446932 ) ) ;
#75790 = CARTESIAN_POINT ( 'NONE',  ( 41.29501498917274205, -33.32507052358980815, -37.31402353058274457 ) ) ;
#75789 = CIRCLE ( 'NONE', #68895, 5.000000000000000888 ) ;
#75791 = CARTESIAN_POINT ( 'NONE',  ( -16.11715839250255655, 21.56713793042588279, -2.163674775881553103 ) ) ;
#75792 = CARTESIAN_POINT ( 'NONE',  ( -43.21893375682410010, 435.1753267429568268, 16.08377476667729766 ) ) ;
#75793 = CARTESIAN_POINT ( 'NONE',  ( -47.80564746871677073, -60.00000000000000000, 66.57118741872818646 ) ) ;
#75794 = CARTESIAN_POINT ( 'NONE',  ( -31.18468355460609942, 439.5714648327614782, 23.11716509955518006 ) ) ;
#75795 = COLOUR_RGB ( '', 0.72549020, 0.75294118, 0.79215686) ;
#75796 = CARTESIAN_POINT ( 'NONE',  ( 62.59524157943331346, 48.00000000000000000, 18.50207713769442819 ) ) ;
#75797 = CARTESIAN_POINT ( 'NONE',  ( -86.38853201505308732, -17.19521753330991487, 181.4521117774834522 ) ) ;
#75798 = ORIENTED_EDGE ( 'NONE', *, *, #25435, .T. ) ;
#75799 = CARTESIAN_POINT ( 'NONE',  ( 9.797174393178825657E-16, 34.00000000000000000, 8.000000000000000000 ) ) ;
#75800 = CARTESIAN_POINT ( 'NONE',  ( -0.9975258024604992668, -32.51280156655929687, 29.30845022069559391 ) ) ;
#75801 = CARTESIAN_POINT ( 'NONE',  ( 7.000000000000000000, 0.000000000000000000, -6.724735318933162453 ) ) ;
#75803 = CARTESIAN_POINT ( 'NONE',  ( 5.330865973525591883, -66.88151609583364632, 14.05427752368915861 ) ) ;
#75802 = CARTESIAN_POINT ( 'NONE',  ( -40.93241935747697369, 325.6791013269530026, 9.457466926974674948 ) ) ;
#75804 = VERTEX_POINT ( 'NONE', #77257 ) ;
#75805 = EDGE_CURVE ( 'NONE', #103615, #44667, #62177, .T. ) ;
#75806 = CARTESIAN_POINT ( 'NONE',  ( -36.64884602963550009, 372.9174138272855998, 4.319931451223398611 ) ) ;
#75807 = CARTESIAN_POINT ( 'NONE',  ( 0.1697127678336000367, 28.20321630628727760, 38.25871777383677852 ) ) ;
#75808 = CARTESIAN_POINT ( 'NONE',  ( 43.50377727019363050, 435.9167426301696082, 18.24083946424737590 ) ) ;
#75809 = CONICAL_SURFACE ( 'NONE', #44808, 33.82893434829263413, 1.221730476396026610 ) ;
#75810 = CARTESIAN_POINT ( 'NONE',  ( 24.71680885386722792, 295.5449029855087701, -1.851325031251247699 ) ) ;
#75811 = CARTESIAN_POINT ( 'NONE',  ( 35.59667163540026280, 463.9592197885497171, -0.04846191499040426731 ) ) ;
#75812 = EDGE_CURVE ( 'NONE', #35969, #54043, #101285, .T. ) ;
#75813 =( LENGTH_UNIT ( ) NAMED_UNIT ( * ) SI_UNIT ( .MILLI., .METRE. ) );
#75814 = CARTESIAN_POINT ( 'NONE',  ( 15.59999999999999787, -3.309499999999999886, 0.000000000000000000 ) ) ;
#75815 = CARTESIAN_POINT ( 'NONE',  ( 114.2222497212829495, -60.00000000000000000, 162.1251737369585726 ) ) ;
#75816 = CARTESIAN_POINT ( 'NONE',  ( -78.76406686447538164, -60.31995527695700332, 162.6514910654201742 ) ) ;
#75817 = VERTEX_POINT ( 'NONE', #7064 ) ;
#75818 = CARTESIAN_POINT ( 'NONE',  ( 4.408728476930471644E-15, 0.000000000000000000, -15.00000000000000178 ) ) ;
#75819 = CARTESIAN_POINT ( 'NONE',  ( 20.59999999999999787, 1.533819458162526451E-15, 0.000000000000000000 ) ) ;
#75820 = SURFACE_STYLE_FILL_AREA ( #42928 ) ;
#75821 = CARTESIAN_POINT ( 'NONE',  ( 0.000000000000000000, 0.000000000000000000, 0.000000000000000000 ) ) ;
#75822 = CARTESIAN_POINT ( 'NONE',  ( 3.757222014067311378, 19.36722785790621870, -5.000000000000000888 ) ) ;
#75823 = CARTESIAN_POINT ( 'NONE',  ( 53.08934989192464826, -30.00000000000000000, 52.21148837440648549 ) ) ;
#75824 = ORIENTED_EDGE ( 'NONE', *, *, #28158, .F. ) ;
#75825 = CARTESIAN_POINT ( 'NONE',  ( -20.05499119796240137, 304.8398979948669876, 9.934468975907650545 ) ) ;
#75826 = ORIENTED_EDGE ( 'NONE', *, *, #82415, .T. ) ;
#75827 = SURFACE_STYLE_USAGE ( .BOTH. , #44543 ) ;
#75828 = CARTESIAN_POINT ( 'NONE',  ( 12.33349330513380337, -4.000000000000000888, 4.898587196589416773E-16 ) ) ;
#75829 = CARTESIAN_POINT ( 'NONE',  ( 32.11826742321338202, 487.8588087913172444, 8.620620385260318486 ) ) ;
#75830 = CARTESIAN_POINT ( 'NONE',  ( -5.405952399528404229, 41.79441213502661157, -58.87429169783612792 ) ) ;
#75831 = LINE ( 'NONE', #67749, #74887 ) ;
#75832 = ADVANCED_FACE ( 'NONE', ( #46480 ), #71796, .F. ) ;
#75833 = VECTOR ( 'NONE', #5417, 1000.000000000000000 ) ;
#75834 = DIRECTION ( 'NONE',  ( 0.000000000000000000, 0.000000000000000000, -1.000000000000000000 ) ) ;
#75835 = ORIENTED_EDGE ( 'NONE', *, *, #99395, .F. ) ;
#75836 = CARTESIAN_POINT ( 'NONE',  ( 105.6057910669374422, -60.00000000000002842, 198.6986277786460562 ) ) ;
#75838 = CARTESIAN_POINT ( 'NONE',  ( 20.85967906329956989, -22.07355929854739074, 28.15013364495181492 ) ) ;
#75837 = CARTESIAN_POINT ( 'NONE',  ( -72.58684158890253002, -59.99999999999995026, 181.3884362157535008 ) ) ;
#75840 = DIRECTION ( 'NONE',  ( -1.000000000000000000, -1.224606353822377258E-16, -0.000000000000000000 ) ) ;
#75839 = PRODUCT_DEFINITION_CONTEXT ( 'detailed design', #21797, 'design' ) ;
#75841 = DIRECTION ( 'NONE',  ( 0.000000000000000000, 0.000000000000000000, -1.000000000000000000 ) ) ;
#75842 = AXIS2_PLACEMENT_3D ( 'NONE', #49368, #41291, #74709 ) ;
#75843 = ADVANCED_FACE ( 'NONE', ( #79893 ), #71277, .T. ) ;
#75844 = CARTESIAN_POINT ( 'NONE',  ( -40.03125687598254956, -36.06455305613715012, 37.97989534578266557 ) ) ;
#75845 = CARTESIAN_POINT ( 'NONE',  ( -35.10078947235764701, 18.64284798593234171, -15.64789144405767729 ) ) ;
#75846 = UNCERTAINTY_MEASURE_WITH_UNIT (LENGTH_MEASURE( 1.000000000000000082E-05 ), #26225, 'distance_accuracy_value', 'NONE');
#75847 = ORIENTED_EDGE ( 'NONE', *, *, #18727, .T. ) ;
#75848 = DIRECTION ( 'NONE',  ( 0.000000000000000000, 0.000000000000000000, 1.000000000000000000 ) ) ;
#75849 = CARTESIAN_POINT ( 'NONE',  ( 7.345894760218278030, 54.30772485615508316, 2.470096959125457126 ) ) ;
#75850 = CARTESIAN_POINT ( 'NONE',  ( 6.073849149975367290, -15.27114203292411432, 14.38605564242082302 ) ) ;
#75851 = DIRECTION ( 'NONE',  ( 0.000000000000000000, -1.000000000000000000, 0.000000000000000000 ) ) ;
#75852 = EDGE_CURVE ( 'NONE', #19599, #57235, #63427, .T. ) ;
#75853 = CARTESIAN_POINT ( 'NONE',  ( 0.000000000000000000, 0.000000000000000000, 60.00000000000000000 ) ) ;
#75854 = CARTESIAN_POINT ( 'NONE',  ( -32.00531707493602340, 486.9465202150305458, 7.099108550606821666 ) ) ;
#75855 = VERTEX_POINT ( 'NONE', #47526 ) ;
#75856 = CARTESIAN_POINT ( 'NONE',  ( -15.64272365568267631, 37.16721670561515367, -22.45732330511674490 ) ) ;
#75857 = VERTEX_POINT ( 'NONE', #56672 ) ;
#75858 = CARTESIAN_POINT ( 'NONE',  ( 80.84629483389447557, -30.00000000000000000, 18.24997580178345657 ) ) ;
#75859 = CARTESIAN_POINT ( 'NONE',  ( 45.44999599557070269, 39.19940254507191213, -45.67500132316253314 ) ) ;
#75861 = DIRECTION ( 'NONE',  ( -0.5735764363510461594, 0.8191520442889916875, 1.003171929053524870E-16 ) ) ;
#75860 = AXIS2_PLACEMENT_3D ( 'NONE', #83825, #84904, #99468 ) ;
#75862 = CARTESIAN_POINT ( 'NONE',  ( 83.28217346054918835, -30.00000000000000000, 45.15196306360270739 ) ) ;
#75863 = AXIS2_PLACEMENT_3D ( 'NONE', #36383, #61152, #53055 ) ;
#75864 = CARTESIAN_POINT ( 'NONE',  ( -31.21769207662248391, 336.6603772009976865, 17.83294671529322173 ) ) ;
#75865 = ORIENTED_EDGE ( 'NONE', *, *, #77098, .T. ) ;
#75866 = ORIENTED_EDGE ( 'NONE', *, *, #62967, .F. ) ;
#75867 = ORIENTED_EDGE ( 'NONE', *, *, #67008, .T. ) ;
#75868 = CARTESIAN_POINT ( 'NONE',  ( -48.02835407290533709, 11.61227450977237119, -14.35535821593460248 ) ) ;
#75869 = CARTESIAN_POINT ( 'NONE',  ( 0.000000000000000000, 52.29617335651133914, 0.000000000000000000 ) ) ;
#75870 = CARTESIAN_POINT ( 'NONE',  ( -13.22953023205303857, 303.5546567990938343, 9.873837419613719746 ) ) ;
#75871 = CARTESIAN_POINT ( 'NONE',  ( 48.02835407290544367, -1.200000000000000030E-05, 15.60535821593427563 ) ) ;
#75872 = VERTEX_POINT ( 'NONE', #89595 ) ;
#75873 = CARTESIAN_POINT ( 'NONE',  ( 7.374560640985523996, 50.00000000000000000, -75.40399789250294305 ) ) ;
#75874 = CIRCLE ( 'NONE', #84425, 5.000000000000001776 ) ;
#75875 = ORIENTED_EDGE ( 'NONE', *, *, #55231, .T. ) ;
#75876 = DIRECTION ( 'NONE',  ( -1.000000000000000000, -0.000000000000000000, -0.000000000000000000 ) ) ;
#75877 = CARTESIAN_POINT ( 'NONE',  ( 75.76114055863986607, -38.36421291546669465, 176.4736164422936895 ) ) ;
#75878 = CARTESIAN_POINT ( 'NONE',  ( 33.00000000000000000, 435.0774731480752280, 11.67986145722084501 ) ) ;
#75879 = CARTESIAN_POINT ( 'NONE',  ( 32.00486866709039901, 300.3058852649511437, 11.16929972234588853 ) ) ;
#75880 = AXIS2_PLACEMENT_3D ( 'NONE', #72107, #105014, #23053 ) ;
#75881 = DIRECTION ( 'NONE',  ( 0.000000000000000000, 0.000000000000000000, 1.000000000000000000 ) ) ;
#75882 = VERTEX_POINT ( 'NONE', #72342 ) ;
#75883 = DIRECTION ( 'NONE',  ( 1.000000000000000000, 0.000000000000000000, 0.000000000000000000 ) ) ;
#75884 = CARTESIAN_POINT ( 'NONE',  ( 27.28205084651333223, 296.4635464116785215, 2.286800737873711853 ) ) ;
#75885 = DIRECTION ( 'NONE',  ( -1.000000000000000000, -1.224606353822377258E-16, -0.000000000000000000 ) ) ;
#75886 = ADVANCED_FACE ( 'NONE', ( #31904 ), #81467, .T. ) ;
#75887 = SURFACE_SIDE_STYLE ('',( #60273 ) ) ;
#75888 = ORIENTED_EDGE ( 'NONE', *, *, #52695, .T. ) ;
#75889 = SURFACE_STYLE_USAGE ( .BOTH. , #27929 ) ;
#75890 = CARTESIAN_POINT ( 'NONE',  ( 8.572527594031486009E-16, 195.0000000000000000, 7.000000000000011546 ) ) ;
#75891 = FACE_OUTER_BOUND ( 'NONE', #45153, .T. ) ;
#75892 = DIRECTION ( 'NONE',  ( -1.000000000000000000, 0.000000000000000000, 0.000000000000000000 ) ) ;
#75893 = CARTESIAN_POINT ( 'NONE',  ( 34.84618260875178208, 489.9833681528626812, 11.97975507378821725 ) ) ;
#75894 = AXIS2_PLACEMENT_3D ( 'NONE', #5475, #30304, #63192 ) ;
#75895 = EDGE_CURVE ( 'NONE', #4337, #20128, #104729, .T. ) ;
#75896 = DIRECTION ( 'NONE',  ( 0.000000000000000000, 0.000000000000000000, -1.000000000000000000 ) ) ;
#75897 = EDGE_CURVE ( 'NONE', #71589, #28086, #55079, .T. ) ;
#75898 = AXIS2_PLACEMENT_3D ( 'NONE', #57019, #89933, #15509 ) ;
#75899 = CARTESIAN_POINT ( 'NONE',  ( 46.00000000000000000, 461.9428920847516906, 12.03309428281970206 ) ) ;
#75900 = CARTESIAN_POINT ( 'NONE',  ( 85.56644655141936084, -39.27954688708853581, 185.6724605245946407 ) ) ;
#75901 = CARTESIAN_POINT ( 'NONE',  ( -3.819639294367488613, 133.7087141186266877, 4.999999999999997335 ) ) ;
#75902 = VERTEX_POINT ( 'NONE', #88537 ) ;
#75903 = CARTESIAN_POINT ( 'NONE',  ( 11.22734410610833145, -57.67099979598874882, -44.34944396839206604 ) ) ;
#75904 = DIRECTION ( 'NONE',  ( -0.000000000000000000, 1.000000000000000000, -0.000000000000000000 ) ) ;
#75905 = DIRECTION ( 'NONE',  ( 0.000000000000000000, 1.000000000000000000, 0.000000000000000000 ) ) ;
#75906 = EDGE_CURVE ( 'NONE', #69179, #104354, #34167, .T. ) ;
#75907 = CARTESIAN_POINT ( 'NONE',  ( 6.249999999999998224, 6.928203230275504332, -4.000000000000007994 ) ) ;
#75908 = CARTESIAN_POINT ( 'NONE',  ( -93.78806885821806816, -30.00000000000000000, 110.7017565295546859 ) ) ;
#75909 = AXIS2_PLACEMENT_3D ( 'NONE', #76510, #3708, #92697 ) ;
#75910 = AXIS2_PLACEMENT_3D ( 'NONE', #5679, #86100, #102793 ) ;
#75911 = CARTESIAN_POINT ( 'NONE',  ( 33.86650669486618881, 4.000000000000003553, 4.898587196589414801E-16 ) ) ;
#75912 = LINE ( 'NONE', #2011, #30804 ) ;
#75913 = CARTESIAN_POINT ( 'NONE',  ( -7.970070017554209407, 4.546953124339754737, -8.057670357645356773 ) ) ;
#75915 = DIRECTION ( 'NONE',  ( 0.000000000000000000, -1.000000000000000000, 0.000000000000000000 ) ) ;
#75914 = LINE ( 'NONE', #67307, #38104 ) ;
#75916 = SURFACE_STYLE_FILL_AREA ( #44634 ) ;
#75917 = CARTESIAN_POINT ( 'NONE',  ( -5.791862111366527621, -19.38500976431717149, 27.11074324704184235 ) ) ;
#75918 = CARTESIAN_POINT ( 'NONE',  ( -34.59893540551257018, 491.2022546151288793, 12.15065315885553865 ) ) ;
#75919 = CARTESIAN_POINT ( 'NONE',  ( 4.813555570991609578, -83.20526203482680216, -3.584128953194789968 ) ) ;
#75920 = DIRECTION ( 'NONE',  ( 0.000000000000000000, 0.000000000000000000, 1.000000000000000000 ) ) ;
#75921 = CARTESIAN_POINT ( 'NONE',  ( 0.1061556211655365900, -6.421950209808287013, -1.876855952934446847 ) ) ;
#75922 = CARTESIAN_POINT ( 'NONE',  ( 59.06535827412803030, -29.12722259196854679, -25.29134694357246005 ) ) ;
#75923 = CARTESIAN_POINT ( 'NONE',  ( -25.60069973378831776, -60.35510020081476767, 35.42683911583728218 ) ) ;
#75924 = AXIS2_PLACEMENT_3D ( 'NONE', #68606, #86915, #103607 ) ;
#75925 = EDGE_LOOP ( 'NONE', ( #84786, #85760, #60742, #81484, #92451 ) ) ;
#75926 = LINE ( 'NONE', #60306, #13456 ) ;
#75927 = DIRECTION ( 'NONE',  ( -1.000000000000000000, -0.000000000000000000, -0.000000000000000000 ) ) ;
#75928 = CARTESIAN_POINT ( 'NONE',  ( -7.986711519608433285, 81.02638096376567489, -0.5300249774147574033 ) ) ;
#75929 = CARTESIAN_POINT ( 'NONE',  ( -62.95843149965692476, -29.57568813394581042, -23.88512804728211947 ) ) ;
#75930 = AXIS2_PLACEMENT_3D ( 'NONE', #29494, #69915, #102816 ) ;
#75932 = CARTESIAN_POINT ( 'NONE',  ( -70.79846966789600060, -21.77035841021276852, -19.10124222137329753 ) ) ;
#75931 = DIRECTION ( 'NONE',  ( -0.000000000000000000, 1.000000000000000000, 0.000000000000000000 ) ) ;
#75933 = ORIENTED_EDGE ( 'NONE', *, *, #7820, .T. ) ;
#75934 = CIRCLE ( 'NONE', #60414, 8.000000000000000000 ) ;
#75935 = CARTESIAN_POINT ( 'NONE',  ( -36.28675805325661230, 437.5816793914590903, 4.254145058677060831 ) ) ;
#75936 = ORIENTED_EDGE ( 'NONE', *, *, #77028, .T. ) ;
#75937 = CARTESIAN_POINT ( 'NONE',  ( -2.078747088351100114, 50.00000000000001421, -98.00015842815599854 ) ) ;
#75938 = TOROIDAL_SURFACE ( 'NONE', #46689, 7.500000000000006217, 5.000000000000000000 ) ;
#75939 = ADVANCED_FACE ( 'NONE', ( #104707 ), #44551, .T. ) ;
#75940 =( GEOMETRIC_REPRESENTATION_CONTEXT ( 3 ) GLOBAL_UNCERTAINTY_ASSIGNED_CONTEXT ( ( #43995 ) ) GLOBAL_UNIT_ASSIGNED_CONTEXT ( ( #79333, #20095, #80920 ) ) REPRESENTATION_CONTEXT ( 'NONE', 'WORKASPACE' ) );
#75941 = PRESENTATION_STYLE_ASSIGNMENT (( #85646 ) ) ;
#75942 = FACE_BOUND ( 'NONE', #56091, .T. ) ;
#75943 = ORIENTED_EDGE ( 'NONE', *, *, #89996, .T. ) ;
#75944 = CARTESIAN_POINT ( 'NONE',  ( -7.944368338772524574, 53.91027570826472015, -3.880857395784224728 ) ) ;
#75945 = CARTESIAN_POINT ( 'NONE',  ( 100.6710202544833521, -52.75082832554577550, 193.6882445870123206 ) ) ;
#75946 = CARTESIAN_POINT ( 'NONE',  ( -7.986711519608433285, -6.026380963765670451, -0.5300249774147614001 ) ) ;
#75947 = EDGE_LOOP ( 'NONE', ( #17829, #97155, #82361, #55481 ) ) ;
#75948 = VERTEX_POINT ( 'NONE', #13564 ) ;
#75949 = ORIENTED_EDGE ( 'NONE', *, *, #87761, .T. ) ;
#75950 = CARTESIAN_POINT ( 'NONE',  ( 27.54067839420761388, 314.0233244279185669, 12.16855529173855821 ) ) ;
#75951 = ADVANCED_FACE ( 'NONE', ( #48579, #96626 ), #64783, .F. ) ;
#75952 = FACE_OUTER_BOUND ( 'NONE', #42061, .T. ) ;
#75953 = DIRECTION ( 'NONE',  ( 0.000000000000000000, 1.000000000000000000, 0.000000000000000000 ) ) ;
#75954 = ORIENTED_EDGE ( 'NONE', *, *, #25694, .F. ) ;
#75955 = PLANE ( 'NONE',  #78895 ) ;
#75956 =( LENGTH_UNIT ( ) NAMED_UNIT ( * ) SI_UNIT ( .MILLI., .METRE. ) );
#75957 = DIRECTION ( 'NONE',  ( 0.5735764363510440500, 0.8191520442889932418, 0.000000000000000000 ) ) ;
#75959 = CARTESIAN_POINT ( 'NONE',  ( -56.21986590610479340, -57.67573674557218766, 94.99882904018191709 ) ) ;
#75958 = AXIS2_PLACEMENT_3D ( 'NONE', #46489, #69191, #61639 ) ;
#75960 = CARTESIAN_POINT ( 'NONE',  ( -36.64823341582351901, 437.5392299810053487, 4.281405873620232505 ) ) ;
#75961 = CARTESIAN_POINT ( 'NONE',  ( -27.97565635352651015, 315.9216507687758053, 12.64980990155120999 ) ) ;
#75962 = CARTESIAN_POINT ( 'NONE',  ( -7.126148247341457242, 41.12758119229482645, -58.55282700859728351 ) ) ;
#75963 = CARTESIAN_POINT ( 'NONE',  ( -94.33288967953484416, -60.00000000000004263, 18.12646456170910625 ) ) ;
#75964 = CARTESIAN_POINT ( 'NONE',  ( -7.482490643626594107, 52.00342315862429388, 3.436133781616750316 ) ) ;
#75965 = CARTESIAN_POINT ( 'NONE',  ( -50.78802596981626039, -39.51418944723420168, 52.08018486103266298 ) ) ;
#75966 = CIRCLE ( 'NONE', #51864, 5.000000000000011546 ) ;
#75967 = FACE_BOUND ( 'NONE', #59075, .T. ) ;
#75968 = PRODUCT ( 'hex screw gradec_din_DIN EN 24018 - M10 x 40-WS', 'hex screw gradec_din_DIN EN 24018 - M10 x 40-WS', '', ( #38527 ) ) ;
#75969 = ORIENTED_EDGE ( 'NONE', *, *, #17028, .T. ) ;
#75970 = CARTESIAN_POINT ( 'NONE',  ( -8.000000000000001776, -13.15624999999999467, 3.313708498984759387 ) ) ;
#75971 = CARTESIAN_POINT ( 'NONE',  ( -9.371250387818031768, 295.2890354896795770, -10.04040834969037199 ) ) ;
#75972 = EDGE_CURVE ( 'NONE', #9067, #81556, #51369, .T. ) ;
#75973 = CARTESIAN_POINT ( 'NONE',  ( 15.92287723967830004, -2.181747968925803249, 14.84254035400510752 ) ) ;
#75974 = ORIENTED_EDGE ( 'NONE', *, *, #79195, .T. ) ;
#75975 =( NAMED_UNIT ( * ) SI_UNIT ( $, .STERADIAN. ) SOLID_ANGLE_UNIT ( ) );
#75976 = CARTESIAN_POINT ( 'NONE',  ( 79.09173631814320515, -38.70095664295953242, 191.1748961264769093 ) ) ;
#75977 = DIRECTION ( 'NONE',  ( 0.000000000000000000, -1.000000000000000000, 0.000000000000000000 ) ) ;
#75978 = CARTESIAN_POINT ( 'NONE',  ( -9.036570576874968452, -10.37119081301011292, -12.86120860535740640 ) ) ;
#75979 = CARTESIAN_POINT ( 'NONE',  ( -55.65414010186731986, 42.00000000000000000, 72.41885610124127481 ) ) ;
#75980 = CARTESIAN_POINT ( 'NONE',  ( 92.89497987163872494, -30.00000000000000355, 191.0944421695535027 ) ) ;
#75981 = DIRECTION ( 'NONE',  ( -1.000000000000000000, -1.224606353822377258E-16, -0.000000000000000000 ) ) ;
#75982 = DIRECTION ( 'NONE',  ( -1.000000000000000000, -1.224606353822377258E-16, -0.000000000000000000 ) ) ;
#75983 = AXIS2_PLACEMENT_3D ( 'NONE', #85024, #52111, #17644 ) ;
#75984 = ORIENTED_EDGE ( 'NONE', *, *, #40339, .T. ) ;
#75985 = VERTEX_POINT ( 'NONE', #7584 ) ;
#75986 = CARTESIAN_POINT ( 'NONE',  ( 51.42960542931152901, -36.04405707132738712, 52.00941032663666874 ) ) ;
#75987 = CARTESIAN_POINT ( 'NONE',  ( -46.00000000000000711, 435.9998667017527509, 13.49155791609234711 ) ) ;
#75988 = CARTESIAN_POINT ( 'NONE',  ( 21.08349330513380693, -4.000000000000000888, 4.898587196589416773E-16 ) ) ;
#75989 = ORIENTED_EDGE ( 'NONE', *, *, #106727, .F. ) ;
#75990 = CARTESIAN_POINT ( 'NONE',  ( -90.39311681537722620, -38.40169232996368720, -14.90399125691173587 ) ) ;
#75991 = ORIENTED_EDGE ( 'NONE', *, *, #3341, .F. ) ;
#75992 = CARTESIAN_POINT ( 'NONE',  ( 0.000000000000000000, 152.0000000000000000, 0.000000000000000000 ) ) ;
#75993 = CARTESIAN_POINT ( 'NONE',  ( 106.9399123034084766, -38.36500875113367925, 194.9488307172588009 ) ) ;
#75994 = CARTESIAN_POINT ( 'NONE',  ( 13.26904190672035888, 24.19056840945213338, -3.252525987528880780 ) ) ;
#75995 = CARTESIAN_POINT ( 'NONE',  ( 89.89766059151314437, -37.84859365328757974, 78.06384706745211588 ) ) ;
#75996 = CARTESIAN_POINT ( 'NONE',  ( 35.34137816767491103, 436.0137577674745444, 5.688536468115818145 ) ) ;
#75997 = CARTESIAN_POINT ( 'NONE',  ( -20.98870079052705861, 304.9248738074109610, -9.984468272890918428 ) ) ;
#75998 = FACE_OUTER_BOUND ( 'NONE', #47921, .T. ) ;
#75999 = CARTESIAN_POINT ( 'NONE',  ( -23.85927881108850457, 25.16624194764255762, -33.04187418837310020 ) ) ;
#76000 = CIRCLE ( 'NONE', #79469, 3.309500000000001663 ) ;
#76001 = DIRECTION ( 'NONE',  ( 0.000000000000000000, 0.000000000000000000, 1.000000000000000000 ) ) ;
#76002 = CARTESIAN_POINT ( 'NONE',  ( 7.849089830965388259, 81.65314728018610424, 0.000000000000000000 ) ) ;
#76003 = EDGE_LOOP ( 'NONE', ( #30770, #68742, #10435, #49124 ) ) ;
#76004 = CARTESIAN_POINT ( 'NONE',  ( 1.250381663246963759, 36.68826934548923191, 28.65663572643696000 ) ) ;
#76005 = CARTESIAN_POINT ( 'NONE',  ( 15.59999999999999787, -3.309499999999999886, 0.000000000000000000 ) ) ;
#76006 = ORIENTED_EDGE ( 'NONE', *, *, #736, .F. ) ;
#76007 = CARTESIAN_POINT ( 'NONE',  ( -38.08476327432922659, 485.5431326501830540, -4.039650833747947978 ) ) ;
#76008 = CARTESIAN_POINT ( 'NONE',  ( -40.91643043736473118, 378.4535619638084540, 26.47871939907729200 ) ) ;
#76009 = CARTESIAN_POINT ( 'NONE',  ( -38.32871752026355239, 25.24414280242103459, -13.21120402984903031 ) ) ;
#76010 = DIRECTION ( 'NONE',  ( 0.9984555975339683975, 9.637352644315584150E-17, 0.05555555555555554553 ) ) ;
#76011 = CARTESIAN_POINT ( 'NONE',  ( -8.000000000000001776, -29.65625000000000000, 3.313708498984758943 ) ) ;
#76012 = CARTESIAN_POINT ( 'NONE',  ( 38.66969219575074845, -25.75017430485813108, 35.13927043512571657 ) ) ;
#76013 = VECTOR ( 'NONE', #103310, 1000.000000000000000 ) ;
#76014 = AXIS2_PLACEMENT_3D ( 'NONE', #88379, #63580, #97495 ) ;
#76015 = DIRECTION ( 'NONE',  ( 0.000000000000000000, -1.000000000000000000, 0.000000000000000000 ) ) ;
#76016 = EDGE_LOOP ( 'NONE', ( #5951, #12832, #32091 ) ) ;
#76017 = CARTESIAN_POINT ( 'NONE',  ( 82.78694254221720428, -50.04262524950087965, 182.2087751002529501 ) ) ;
#76018 = CARTESIAN_POINT ( 'NONE',  ( 1.163414459189985485E-15, -2.000000000000000000, -9.500000000000000000 ) ) ;
#76019 = FACE_OUTER_BOUND ( 'NONE', #78382, .T. ) ;
#76020 = ORIENTED_EDGE ( 'NONE', *, *, #8222, .T. ) ;
#76021 = CARTESIAN_POINT ( 'NONE',  ( -33.00000000000000000, 500.0000000000002274, 0.000000000000000000 ) ) ;
#76022 = PRESENTATION_STYLE_ASSIGNMENT (( #16734 ) ) ;
#76023 = CARTESIAN_POINT ( 'NONE',  ( 12.12626197893212243, -3.000000000000002665, -94.24800833403466527 ) ) ;
#76024 = DIRECTION ( 'NONE',  ( -1.000000000000000000, 0.000000000000000000, 0.000000000000000000 ) ) ;
#76025 = ADVANCED_FACE ( 'NONE', ( #97140 ), #30784, .T. ) ;
#76026 = CARTESIAN_POINT ( 'NONE',  ( -18.63186175455728844, -25.33939609445413410, -38.50114773520279243 ) ) ;
#76027 = EDGE_CURVE ( 'NONE', #35260, #99128, #23285, .T. ) ;
#76028 = PRODUCT_CONTEXT ( 'NONE', #89957, 'mechanical' ) ;
#76029 = CIRCLE ( 'NONE', #62360, 4.000000000000001776 ) ;
#76030 = CARTESIAN_POINT ( 'NONE',  ( 53.68073265722826193, -60.00000000000000711, 81.53482892392325709 ) ) ;
#76031 = CARTESIAN_POINT ( 'NONE',  ( 27.25585338856197737, -30.58637391271707173, 39.18084608107302103 ) ) ;
#76032 = CARTESIAN_POINT ( 'NONE',  ( 0.000000000000000000, 0.000000000000000000, 4.000000000000000888 ) ) ;
#76033 = CARTESIAN_POINT ( 'NONE',  ( 5.437019438593272191, -12.93285032667489709, 32.09035593251934415 ) ) ;
#76035 = CARTESIAN_POINT ( 'NONE',  ( -14.81362254366326248, 21.99737691636699566, -4.398778852034027409 ) ) ;
#76034 = CARTESIAN_POINT ( 'NONE',  ( -27.50278574530640441, -30.75557938056827467, 39.29189916433056595 ) ) ;
#76036 = CARTESIAN_POINT ( 'NONE',  ( -9.948561005166130400, 88.86990273748200764, -1.045755304005127284 ) ) ;
#76037 = CARTESIAN_POINT ( 'NONE',  ( -7.188101187500002709, -9.312500002048384573, 2.977408999572648707 ) ) ;
#76038 = CARTESIAN_POINT ( 'NONE',  ( 28.84964340243799441, 297.0390576586646603, -1.524508641439632051 ) ) ;
#76039 = CARTESIAN_POINT ( 'NONE',  ( -5.276765049035077482, 6.073111908730296271, -7.634085501268425666 ) ) ;
#76040 = EDGE_LOOP ( 'NONE', ( #45136, #46996, #69350, #63932, #102963, #90821 ) ) ;
#76041 = CARTESIAN_POINT ( 'NONE',  ( 15.59999999999999787, 1.533819458162526451E-15, 0.000000000000000000 ) ) ;
#76042 = SURFACE_STYLE_USAGE ( .BOTH. , #28075 ) ;
#76043 = DIRECTION ( 'NONE',  ( 0.000000000000000000, 0.000000000000000000, 1.000000000000000000 ) ) ;
#76044 = LINE ( 'NONE', #10250, #61383 ) ;
#76046 = CARTESIAN_POINT ( 'NONE',  ( 34.25937177855836069, -21.77016779706914917, -28.20208921661981449 ) ) ;
#76045 = CARTESIAN_POINT ( 'NONE',  ( 43.86650669486618881, 4.000000000000003553, 4.898587196589414801E-16 ) ) ;
#76047 = ORIENTED_EDGE ( 'NONE', *, *, #60617, .F. ) ;
#76048 = B_SPLINE_CURVE_WITH_KNOTS ( 'NONE', 3,
 ( #63927, #56311, #89250, #81137, #5669, #22421 ),
 .UNSPECIFIED., .F., .F.,
 ( 4, 2, 4 ),
 ( 0.01067228061038545325, 0.01257272967564229682, 0.01447317874089914212 ),
 .UNSPECIFIED. ) ;
#76049 = CARTESIAN_POINT ( 'NONE',  ( 27.26388569244345916, 36.83098433723539245, 7.556984339685507202 ) ) ;
#76050 = CARTESIAN_POINT ( 'NONE',  ( 1.000000000000000444, -52.55160771104127093, 2.953793101315682623 ) ) ;
#76051 = VERTEX_POINT ( 'NONE', #80952 ) ;
#76052 = DIRECTION ( 'NONE',  ( 0.000000000000000000, 0.000000000000000000, -1.000000000000000000 ) ) ;
#76053 = EDGE_CURVE ( 'NONE', #64182, #42513, #23850, .T. ) ;
#76054 = DIRECTION ( 'NONE',  ( -0.5735764363510497121, 0.8191520442889892450, 1.003171929053521665E-16 ) ) ;
#76055 = SURFACE_STYLE_USAGE ( .BOTH. , #36718 ) ;
#76056 = CARTESIAN_POINT ( 'NONE',  ( -100.8737896469964426, -60.00000000000000000, 86.15980893726860756 ) ) ;
#76057 = DIRECTION ( 'NONE',  ( 1.000000000000000000, 0.000000000000000000, 0.000000000000000000 ) ) ;
#76058 = CARTESIAN_POINT ( 'NONE',  ( 1.305263714129178076, -8.377797850839296956, -7.792447862505341938 ) ) ;
#76059 = CARTESIAN_POINT ( 'NONE',  ( 26.27902093981875709, 306.9027577142574614, -9.548073367147230428 ) ) ;
#76060 = SURFACE_SIDE_STYLE ('',( #76592 ) ) ;
#76061 = CARTESIAN_POINT ( 'NONE',  ( 2.617478844989858722, -3.000000000000002665, -75.26027323389553203 ) ) ;
#76062 = CARTESIAN_POINT ( 'NONE',  ( -85.99911114356302733, -18.43252915325882313, 165.6345971928553240 ) ) ;
#76063 = ORIENTED_EDGE ( 'NONE', *, *, #29696, .T. ) ;
#76064 = CARTESIAN_POINT ( 'NONE',  ( 5.625019092414619948, 41.66287055497627989, -70.61600277306789053 ) ) ;
#76065 = VERTEX_POINT ( 'NONE', #42623 ) ;
#76066 = ORIENTED_EDGE ( 'NONE', *, *, #79397, .T. ) ;
#76067 = CARTESIAN_POINT ( 'NONE',  ( -16.98784884574818577, 303.5779498825697829, -10.05824724361832168 ) ) ;
#76068 = DIRECTION ( 'NONE',  ( 0.000000000000000000, -1.000000000000000000, 0.000000000000000000 ) ) ;
#76069 = ADVANCED_FACE ( 'NONE', ( #65317 ), #32971, .T. ) ;
#76070 = EDGE_CURVE ( 'NONE', #14235, #71609, #101361, .T. ) ;
#76071 = CARTESIAN_POINT ( 'NONE',  ( 68.45015997180047407, 4.898587196589294500E-16, -4.000000000000007105 ) ) ;
#76072 = ORIENTED_EDGE ( 'NONE', *, *, #64281, .F. ) ;
#76073 = B_SPLINE_CURVE_WITH_KNOTS ( 'NONE', 3,
 ( #47835, #16017, #7916, #48896, #81790, #90442 ),
 .UNSPECIFIED., .F., .F.,
 ( 4, 2, 4 ),
 ( 2.380733003145476372E-07, 0.001898835937927386775, 0.003797433802554458452 ),
 .UNSPECIFIED. ) ;
#76074 = DIRECTION ( 'NONE',  ( 1.000000000000000000, 0.000000000000000000, -0.000000000000000000 ) ) ;
#76075 =( NAMED_UNIT ( * ) SI_UNIT ( $, .STERADIAN. ) SOLID_ANGLE_UNIT ( ) );
#76076 = DIRECTION ( 'NONE',  ( -0.000000000000000000, -1.000000000000000000, -0.000000000000000000 ) ) ;
#76077 = CARTESIAN_POINT ( 'NONE',  ( -1.311584102661731199, 14.06480120835178305, 6.880471120297250387 ) ) ;
#76078 = CARTESIAN_POINT ( 'NONE',  ( 36.87655955837855259, 438.2068510013161813, 3.933030107424693167 ) ) ;
#76079 = LINE ( 'NONE', #36212, #101091 ) ;
#76080 = CARTESIAN_POINT ( 'NONE',  ( -97.53417455291598515, -56.34874176541392643, 195.8863760079639462 ) ) ;
#76081 = COLOUR_RGB ( '', 0.72549020, 0.75294118, 0.79215686) ;
#76082 = CARTESIAN_POINT ( 'NONE',  ( 90.16383085397569630, -14.21045842199434084, 52.56522323202336366 ) ) ;
#76083 = AXIS2_PLACEMENT_3D ( 'NONE', #5348, #104554, #71129 ) ;
#76084 = CARTESIAN_POINT ( 'NONE',  ( -98.15060533238310825, -14.21045842199422715, 197.6136055373540614 ) ) ;
#76085 = CARTESIAN_POINT ( 'NONE',  ( -59.17778066530962633, -49.91509818790471087, 74.96796009585710863 ) ) ;
#76086 = VERTEX_POINT ( 'NONE', #24357 ) ;
#76087 = DIRECTION ( 'NONE',  ( 0.000000000000000000, -1.000000000000000000, 0.000000000000000000 ) ) ;
#76088 = ORIENTED_EDGE ( 'NONE', *, *, #58436, .F. ) ;
#76089 = CARTESIAN_POINT ( 'NONE',  ( -102.1119726963908079, -37.82064582844866152, 183.3968591677531208 ) ) ;
#76090 = CARTESIAN_POINT ( 'NONE',  ( 22.61650669486618526, 4.000000000000003553, 4.898587196589414801E-16 ) ) ;
#76091 = CARTESIAN_POINT ( 'NONE',  ( -1.469576158976823947E-15, -19.06250000409677270, 8.000000000000000000 ) ) ;
#76092 = EDGE_CURVE ( 'NONE', #49621, #19990, #63489, .T. ) ;
#76093 = CARTESIAN_POINT ( 'NONE',  ( 16.51905981272403423, 42.00139749746823981, -87.79004739960673476 ) ) ;
#76094 = EDGE_LOOP ( 'NONE', ( #1010, #68441, #78582, #4549 ) ) ;
#76095 = CARTESIAN_POINT ( 'NONE',  ( 5.096247963225427391, -4.999999999999998224, -73.00359695309825270 ) ) ;
#76096 = CARTESIAN_POINT ( 'NONE',  ( -74.06050393588230918, -60.00000000000000000, 172.8376900993954735 ) ) ;
#76097 = CARTESIAN_POINT ( 'NONE',  ( -3.358578016107228947, -0.9723468250023499237, 104.2746939430698205 ) ) ;
#76098 = CARTESIAN_POINT ( 'NONE',  ( 2.977408999572650927, -19.25000000204838813, -7.188101187500001821 ) ) ;
#76099 = DIRECTION ( 'NONE',  ( -1.000000000000000000, -1.224606353822377258E-16, -0.000000000000000000 ) ) ;
#76100 = LINE ( 'NONE', #83137, #47755 ) ;
#76101 = DIRECTION ( 'NONE',  ( 0.000000000000000000, -1.000000000000000000, 0.000000000000000000 ) ) ;
#76102 = CARTESIAN_POINT ( 'NONE',  ( 82.57687275821095341, -41.66704177847501001, -14.02669740995510494 ) ) ;
#76103 = EDGE_CURVE ( 'NONE', #75460, #99989, #13489, .T. ) ;
#76104 = CARTESIAN_POINT ( 'NONE',  ( 11.88147559491878269, -10.57770090359279003, 10.63809983876897824 ) ) ;
#76105 = CARTESIAN_POINT ( 'NONE',  ( -15.42241126771893889, 46.21736870922991613, -5.091656527549202060 ) ) ;
#76106 =( LENGTH_UNIT ( ) NAMED_UNIT ( * ) SI_UNIT ( .MILLI., .METRE. ) );
#76107 = UNCERTAINTY_MEASURE_WITH_UNIT (LENGTH_MEASURE( 1.000000000000000082E-05 ), #79735, 'distance_accuracy_value', 'NONE');
#76108 = CARTESIAN_POINT ( 'NONE',  ( -30.76582839458128049, -60.33262561358965570, 37.12003127044696527 ) ) ;
#76109 = VECTOR ( 'NONE', #72879, 1000.000000000000114 ) ;
#76110 = CARTESIAN_POINT ( 'NONE',  ( 2.649924368967711441, 20.85987309459008898, 6.482037363235274796 ) ) ;
#76111 = UNCERTAINTY_MEASURE_WITH_UNIT (LENGTH_MEASURE( 1.000000000000000082E-05 ), #10225, 'distance_accuracy_value', 'NONE');
#76112 = CARTESIAN_POINT ( 'NONE',  ( 43.67629986226869221, -29.16024730390979869, 39.50635445105871923 ) ) ;
#76113 = CIRCLE ( 'NONE', #77814, 3.309500000000001663 ) ;
#76114 = LINE ( 'NONE', #2211, #81721 ) ;
#76115 = EDGE_CURVE ( 'NONE', #86142, #86773, #41566, .T. ) ;
#76116 = CARTESIAN_POINT ( 'NONE',  ( -6.928203230275511437, 85.26526156932591505, 4.000000000000001776 ) ) ;
#76117 = CARTESIAN_POINT ( 'NONE',  ( -86.44246846762395364, -38.61868829427960748, 199.2842396746591760 ) ) ;
#76118 = EDGE_LOOP ( 'NONE', ( #35398, #102796, #29431, #38351, #58500 ) ) ;
#76120 = CARTESIAN_POINT ( 'NONE',  ( -43.04469050570867239, 434.7734435962895532, 9.248231035232469921 ) ) ;
#76119 = CARTESIAN_POINT ( 'NONE',  ( 77.87040428542300674, -38.35599188746820687, -27.73370404319807037 ) ) ;
#76121 = DIRECTION ( 'NONE',  ( 0.5735764363510491570, -0.8191520442889895781, 1.003171929053522035E-16 ) ) ;
#76122 = CARTESIAN_POINT ( 'NONE',  ( -48.48458519718469972, 8.810627846918883677, -16.77132102101082012 ) ) ;
#76123 = CARTESIAN_POINT ( 'NONE',  ( -7.500000000000006217, 40.19558924101049513, -59.64746548774058965 ) ) ;
#76124 = CARTESIAN_POINT ( 'NONE',  ( 6.924711585765388477, 40.92328497145224020, -70.90711766198887744 ) ) ;
#76125 = CARTESIAN_POINT ( 'NONE',  ( 13.50000000000000178, 0.000000000000000000, -13.00000000000000000 ) ) ;
#76126 = DIRECTION ( 'NONE',  ( -0.000000000000000000, 1.000000000000000000, -0.000000000000000000 ) ) ;
#76127 = CARTESIAN_POINT ( 'NONE',  ( 7.500000000000000000, -4.330127018922200755, -7.422398894150036064 ) ) ;
#76128 = CARTESIAN_POINT ( 'NONE',  ( 109.7562981413315697, -59.99999999999999289, 141.5450222497400148 ) ) ;
#76129 = CARTESIAN_POINT ( 'NONE',  ( 11.89131030317610183, -5.000000000000000888, 6.123233995736769241E-16 ) ) ;
#76130 = EDGE_CURVE ( 'NONE', #88140, #32552, #41043, .T. ) ;
#76131 = CARTESIAN_POINT ( 'NONE',  ( -7.045965687440310710, -66.30392463786034796, 3.790395326974320689 ) ) ;
#76132 = ORIENTED_EDGE ( 'NONE', *, *, #64591, .F. ) ;
#76133 = CARTESIAN_POINT ( 'NONE',  ( -99.71302761529223346, -29.99999999999998224, 150.1575047744225913 ) ) ;
#76134 = VERTEX_POINT ( 'NONE', #59364 ) ;
#76135 = LINE ( 'NONE', #92315, #21836 ) ;
#76136 = CARTESIAN_POINT ( 'NONE',  ( 0.000000000000000000, -50.00000000000000000, 112.0000000000000000 ) ) ;
#76137 = CARTESIAN_POINT ( 'NONE',  ( 31.21850725759788503, 336.6757834771444777, 17.83627441276912151 ) ) ;
#76138 = CARTESIAN_POINT ( 'NONE',  ( 33.09999999999999432, 3.309500000000003439, 4.052968581778167743E-16 ) ) ;
#76139 = CARTESIAN_POINT ( 'NONE',  ( 5.082755093536324154, -21.21875000204838813, 5.082755093536326818 ) ) ;
#76140 =( NAMED_UNIT ( * ) SI_UNIT ( $, .STERADIAN. ) SOLID_ANGLE_UNIT ( ) );
#76141 = UNCERTAINTY_MEASURE_WITH_UNIT (LENGTH_MEASURE( 1.000000000000000082E-05 ), #23130, 'distance_accuracy_value', 'NONE');
#76142 = CARTESIAN_POINT ( 'NONE',  ( 0.000000000000000000, 0.000000000000000000, -8.000000000000000000 ) ) ;
#76143 = ORIENTED_EDGE ( 'NONE', *, *, #3202, .F. ) ;
#76144 = CARTESIAN_POINT ( 'NONE',  ( 83.49137038316719384, -32.53379486668217169, 163.2796185419070696 ) ) ;
#76145 = CARTESIAN_POINT ( 'NONE',  ( -4.051286199644071218, -1.398729870307597878, 103.8758286790405236 ) ) ;
#76146 = CARTESIAN_POINT ( 'NONE',  ( 1.126429428730186588, -7.232124035235067083, -6.344710093416095376 ) ) ;
#76147 = ORIENTED_EDGE ( 'NONE', *, *, #15996, .T. ) ;
#76148 = CIRCLE ( 'NONE', #57190, 2.000000000000000000 ) ;
#76149 = FACE_OUTER_BOUND ( 'NONE', #65249, .T. ) ;
#76150 = CARTESIAN_POINT ( 'NONE',  ( -47.44867487729145239, 16.35164899989666054, 16.71951642917255398 ) ) ;
#76151 = CARTESIAN_POINT ( 'NONE',  ( 38.17803095905032507, 27.65683721262864125, -11.10447198242798272 ) ) ;
#76152 = CARTESIAN_POINT ( 'NONE',  ( 5.691929483231187525, -5.629165124598856984, -3.250000000000002220 ) ) ;
#76153 = CONICAL_SURFACE ( 'NONE', #14164, 6.500000000000000888, 0.8987552595851637793 ) ;
#76154 = DIRECTION ( 'NONE',  ( 1.000000000000000000, 0.000000000000000000, 0.000000000000000000 ) ) ;
#76155 = CARTESIAN_POINT ( 'NONE',  ( 0.000000000000000000, -14.49999999999999822, 0.000000000000000000 ) ) ;
#76156 = ADVANCED_FACE ( 'NONE', ( #26491 ), #86933, .F. ) ;
#76157 = ORIENTED_EDGE ( 'NONE', *, *, #4440, .T. ) ;
#76158 = B_SPLINE_CURVE_WITH_KNOTS ( 'NONE', 3,
 ( #73047, #88734, #29476, #96312, #14826, #39664, #14290, #47194, #62353, #80094, #89268, #6200, #39137, #64468, #23492, #1279, #49308, #33170, #9377, #16426 ),
 .UNSPECIFIED., .F., .F.,
 ( 4, 2, 2, 2, 2, 2, 2, 2, 2, 4 ),
 ( 0.007186367946188911872, 0.007690128173786097560, 0.008193888401383284115, 0.008697648628980470670, 0.009201408856577655490, 0.009705169084174842045, 0.01020892931177202687, 0.01046080942557061841, 0.01071268953936920648, 0.01121644976696637569 ),
 .UNSPECIFIED. ) ;
#76159 = DIRECTION ( 'NONE',  ( -1.000000000000000000, -0.000000000000000000, -0.000000000000000000 ) ) ;
#76160 = ADVANCED_FACE ( 'NONE', ( #27020 ), #54831, .T. ) ;
#76161 = CARTESIAN_POINT ( 'NONE',  ( -5.000000000000000000, -54.98008964862484760, 9.870798784359230638 ) ) ;
#76162 = CARTESIAN_POINT ( 'NONE',  ( 14.78104354000378251, 22.77915615417240147, 2.489457476759114218 ) ) ;
#76163 = CIRCLE ( 'NONE', #53766, 4.250000000000000000 ) ;
#76164 = LINE ( 'NONE', #28200, #70566 ) ;
#76165 = CARTESIAN_POINT ( 'NONE',  ( 7.188101187499999156, -26.75000000204838457, 2.977408999572654924 ) ) ;
#76166 = DIRECTION ( 'NONE',  ( -1.000000000000000000, -1.224606353822377258E-16, -0.000000000000000000 ) ) ;
#76167 = CARTESIAN_POINT ( 'NONE',  ( 7.000000000000000000, 0.000000000000000000, -12.27439246179028309 ) ) ;
#76168 = CARTESIAN_POINT ( 'NONE',  ( -48.02835407290533709, 11.61227450977237119, -14.35535821593460248 ) ) ;
#76169 = ORIENTED_EDGE ( 'NONE', *, *, #63155, .T. ) ;
#76170 = DIRECTION ( 'NONE',  ( -1.000000000000000000, -1.224606353822377258E-16, -0.000000000000000000 ) ) ;
#76171 = CARTESIAN_POINT ( 'NONE',  ( 4.699999999999999289, -3.752776749732579020, -6.500000000000000888 ) ) ;
#76172 = CARTESIAN_POINT ( 'NONE',  ( -6.339665615494448403, 4.010265277135025563, -5.000000000000000000 ) ) ;
#76173 =( NAMED_UNIT ( * ) SI_UNIT ( $, .STERADIAN. ) SOLID_ANGLE_UNIT ( ) );
#76174 = ADVANCED_FACE ( 'NONE', ( #103000 ), #36686, .T. ) ;
#76175 = CIRCLE ( 'NONE', #53779, 7.499999999992679633 ) ;
#76176 = EDGE_LOOP ( 'NONE', ( #100280, #3813, #41231, #43498 ) ) ;
#76177 = DIRECTION ( 'NONE',  ( -0.000000000000000000, -0.000000000000000000, -1.000000000000000000 ) ) ;
#76178 = SURFACE_STYLE_FILL_AREA ( #59493 ) ;
#76179 = AXIS2_PLACEMENT_3D ( 'NONE', #91789, #17910, #50762 ) ;
#76180 = ORIENTED_EDGE ( 'NONE', *, *, #5735, .T. ) ;
#76181 = CARTESIAN_POINT ( 'NONE',  ( 32.65674990438940739, 434.9893739305006193, 13.53244902892662438 ) ) ;
#76182 = EDGE_CURVE ( 'NONE', #50002, #29335, #18695, .T. ) ;
#76183 = CARTESIAN_POINT ( 'NONE',  ( -1.251112176197288095, 10.43734136627239728, -50.60533220255923226 ) ) ;
#76184 = CARTESIAN_POINT ( 'NONE',  ( 16.05785784214673129, 4.775831776474256607, -3.710403933782447261 ) ) ;
#76185 = CARTESIAN_POINT ( 'NONE',  ( 36.92547957880908882, 25.96841499943989362, 11.08204091492609322 ) ) ;
#76186 = CARTESIAN_POINT ( 'NONE',  ( -77.98089275376243279, -60.00000000000000000, 192.8200721109930669 ) ) ;
#76187 = CARTESIAN_POINT ( 'NONE',  ( 19.09326099321046755, 49.66527553188159771, 61.75128748409139234 ) ) ;
#76189 = AXIS2_PLACEMENT_3D ( 'NONE', #32656, #40708, #57411 ) ;
#76188 = CARTESIAN_POINT ( 'NONE',  ( 9.268351869679383626, 44.06619222810213188, -13.41315172291116475 ) ) ;
#76190 =( NAMED_UNIT ( * ) SI_UNIT ( $, .STERADIAN. ) SOLID_ANGLE_UNIT ( ) );
#76191 = CARTESIAN_POINT ( 'NONE',  ( -85.02386936141340357, -39.35437566379916063, 183.7573501001193961 ) ) ;
#76192 = CARTESIAN_POINT ( 'NONE',  ( -23.21751746555244722, -1.200000000000000030E-05, 31.95617127781060773 ) ) ;
#76193 = ORIENTED_EDGE ( 'NONE', *, *, #21568, .F. ) ;
#76194 = CARTESIAN_POINT ( 'NONE',  ( 23.86650669486618881, 4.898587196589411843E-16, -4.000000000000000888 ) ) ;
#76195 = EDGE_CURVE ( 'NONE', #74698, #3656, #56519, .T. ) ;
#76196 = CARTESIAN_POINT ( 'NONE',  ( 3.352941176471718965, -1.200583151107622815, 104.5794940929782797 ) ) ;
#76197 = CARTESIAN_POINT ( 'NONE',  ( -84.01129673064754400, -45.26989356464081027, 2.482293978573416826 ) ) ;
#76198 = PRESENTATION_STYLE_ASSIGNMENT (( #43316 ) ) ;
#76199 = CARTESIAN_POINT ( 'NONE',  ( -45.40507512465600115, 439.2794387026467575, 6.273370203490043373 ) ) ;
#76200 = CARTESIAN_POINT ( 'NONE',  ( -16.32412570343894131, 43.58760925489881544, 6.626709406305174355 ) ) ;
#76201 = CARTESIAN_POINT ( 'NONE',  ( -15.08194089903437352, -6.425657694783502905, 13.55734734230695970 ) ) ;
#76202 = CARTESIAN_POINT ( 'NONE',  ( 28.29586762127448551, 36.29923524811977131, -9.196630039856511729 ) ) ;
#76203 = CARTESIAN_POINT ( 'NONE',  ( -72.41885610115926397, 42.00000000000000000, -55.65414010186705696 ) ) ;
#76204 = CARTESIAN_POINT ( 'NONE',  ( -43.59756234217317683, 434.3244621007142996, 14.55946156040369921 ) ) ;
#76205 = CARTESIAN_POINT ( 'NONE',  ( 71.62958147348905413, -29.99999999999999645, 135.6714503744467493 ) ) ;
#76206 = FILL_AREA_STYLE ('',( #43847 ) ) ;
#76207 = CARTESIAN_POINT ( 'NONE',  ( -80.19882167783929106, -30.00000000000005684, -24.77908391697505053 ) ) ;
#76208 = CARTESIAN_POINT ( 'NONE',  ( -73.18360275706602636, -39.49101380701564068, 113.0608591253020876 ) ) ;
#76209 = ORIENTED_EDGE ( 'NONE', *, *, #41219, .T. ) ;
#76210 = CARTESIAN_POINT ( 'NONE',  ( 67.91784306603950938, -14.21045842199442077, 108.3249851056250321 ) ) ;
#76211 = CARTESIAN_POINT ( 'NONE',  ( -56.10248074403467911, 40.83957962598827862, -33.37184059469758068 ) ) ;
#76212 = CARTESIAN_POINT ( 'NONE',  ( 22.25033068898240174, -60.00000000000493827, 42.95758340851298840 ) ) ;
#76213 = VERTEX_POINT ( 'NONE', #76579 ) ;
#76214 = CARTESIAN_POINT ( 'NONE',  ( 8.398714108050164384, 51.60933059333073913, -4.031152949374811278 ) ) ;
#76215 = CARTESIAN_POINT ( 'NONE',  ( -2.977408999572650039, -25.06250000204838813, -7.188101187500000933 ) ) ;
#76216 = CONICAL_SURFACE ( 'NONE', #12708, 4.000000000000007105, 0.9599310885968835860 ) ;
#76217 = CARTESIAN_POINT ( 'NONE',  ( -0.3341299038094548424, 28.19050081788694229, -38.29257118597956122 ) ) ;
#76218 = VERTEX_POINT ( 'NONE', #61497 ) ;
#76219 =( NAMED_UNIT ( * ) PLANE_ANGLE_UNIT ( ) SI_UNIT ( $, .RADIAN. ) );
#76220 = VERTEX_POINT ( 'NONE', #2694 ) ;
#76221 = LINE ( 'NONE', #35270, #13105 ) ;
#76222 = AXIS2_PLACEMENT_3D ( 'NONE', #19446, #12350, #12877 ) ;
#76223 = CARTESIAN_POINT ( 'NONE',  ( 46.79169002450413473, 18.53182619689592769, -15.81978731893121015 ) ) ;
#76224 = CARTESIAN_POINT ( 'NONE',  ( -52.24845625772812951, -60.00000000001954703, 84.50696348291317861 ) ) ;
#76225 = CARTESIAN_POINT ( 'NONE',  ( 32.54608566124238678, 315.7613049388691593, -7.144893715508695564 ) ) ;
#76226 = CARTESIAN_POINT ( 'NONE',  ( 7.188101187500001821, -16.06250000204838457, -2.977408999572650483 ) ) ;
#76227 = CARTESIAN_POINT ( 'NONE',  ( -85.18896233714281152, -59.99999999999995737, -15.68185129854840554 ) ) ;
#76228 = STYLED_ITEM ( 'NONE', ( #6267 ), #52016 ) ;
#76229 = CARTESIAN_POINT ( 'NONE',  ( 1.232060836821106786, -0.008527515973728574603, 101.3403412146573004 ) ) ;
#76230 = DIRECTION ( 'NONE',  ( -0.5735764363510494901, -0.8191520442889894671, 0.000000000000000000 ) ) ;
#76231 = CARTESIAN_POINT ( 'NONE',  ( -7.996668422907487361, 49.99999999999999289, -91.14546720082822162 ) ) ;
#76232 = ADVANCED_FACE ( 'NONE', ( #10256 ), #60960, .T. ) ;
#76233 = CARTESIAN_POINT ( 'NONE',  ( 0.000000000000000000, 2.000000000000000000, 0.000000000000000000 ) ) ;
#76234 = CARTESIAN_POINT ( 'NONE',  ( 39.41219261697651177, 436.7611714244556538, 5.258763975274515445 ) ) ;
#76235 = VERTEX_POINT ( 'NONE', #3240 ) ;
#76236 =( LENGTH_UNIT ( ) NAMED_UNIT ( * ) SI_UNIT ( .MILLI., .METRE. ) );
#76237 = AXIS2_PLACEMENT_3D ( 'NONE', #89669, #81534, #7659 ) ;
#76238 = CARTESIAN_POINT ( 'NONE',  ( 33.15956608574755649, -56.83790991451342478, 37.61396027134895803 ) ) ;
#76239 = CARTESIAN_POINT ( 'NONE',  ( 22.03900363279161567, -4.285714285712638016, 12.70248734011606828 ) ) ;
#76240 = ORIENTED_EDGE ( 'NONE', *, *, #92748, .F. ) ;
#76241 = EDGE_CURVE ( 'NONE', #33098, #39859, #75478, .T. ) ;
#76242 = CARTESIAN_POINT ( 'NONE',  ( -22.59054144479424409, 25.42936075388009343, -33.04960633241812928 ) ) ;
#76243 = ORIENTED_EDGE ( 'NONE', *, *, #32591, .T. ) ;
#76245 = CARTESIAN_POINT ( 'NONE',  ( -1.010569909552581080, 43.89392652721726762, -16.74618260332281139 ) ) ;
#76244 = CARTESIAN_POINT ( 'NONE',  ( -26.78880536180239247, 34.86538589505409647, -7.595015278602215147 ) ) ;
#76246 = CARTESIAN_POINT ( 'NONE',  ( 4.872636759907720716, 41.00341855746686548, -70.74912513459382524 ) ) ;
#76247 = DIRECTION ( 'NONE',  ( 0.000000000000000000, -1.000000000000000000, 0.000000000000000000 ) ) ;
#76248 =( REPRESENTATION_RELATIONSHIP ('NONE','NONE', #69581, #7490 ) REPRESENTATION_RELATIONSHIP_WITH_TRANSFORMATION ( #61077 )SHAPE_REPRESENTATION_RELATIONSHIP( ) );
#76249 = CARTESIAN_POINT ( 'NONE',  ( 31.08349330513380693, 4.000000000000003553, 0.000000000000000000 ) ) ;
#76250 = EDGE_CURVE ( 'NONE', #43396, #34171, #77255, .T. ) ;
#76251 = FACE_OUTER_BOUND ( 'NONE', #35689, .T. ) ;
#76252 = LINE ( 'NONE', #68168, #26401 ) ;
#76253 = ORIENTED_EDGE ( 'NONE', *, *, #56998, .F. ) ;
#76254 = CARTESIAN_POINT ( 'NONE',  ( 90.46693666255114863, -59.99999999999999289, -18.03047012885635780 ) ) ;
#76255 = CARTESIAN_POINT ( 'NONE',  ( 6.500000000000000888, 0.000000000000000000, 1.734723475976807094E-15 ) ) ;
#76256 = EDGE_CURVE ( 'NONE', #12690, #35868, #52308, .T. ) ;
#76257 = CARTESIAN_POINT ( 'NONE',  ( 39.41275501334703080, 489.7121233615675919, 11.67778311875517971 ) ) ;
#76258 = AXIS2_PLACEMENT_3D ( 'NONE', #17154, #73223, #25816 ) ;
#76259 = CARTESIAN_POINT ( 'NONE',  ( 7.347880794884120722E-16, -99.99999999999997158, -6.000000000000000888 ) ) ;
#76260 = ORIENTED_EDGE ( 'NONE', *, *, #57320, .T. ) ;
#76261 = CARTESIAN_POINT ( 'NONE',  ( -81.87262150750494527, -30.00000000000330402, 194.0511874815462079 ) ) ;
#76262 = ORIENTED_EDGE ( 'NONE', *, *, #93644, .T. ) ;
#76263 = ORIENTED_EDGE ( 'NONE', *, *, #66304, .T. ) ;
#76264 = CARTESIAN_POINT ( 'NONE',  ( 6.943482370013978944, 84.47151629739275336, 3.973876482044366387 ) ) ;
#76265 = DIRECTION ( 'NONE',  ( -1.000000000000000000, -1.224606353822377258E-16, -0.000000000000000000 ) ) ;
#76266 = CARTESIAN_POINT ( 'NONE',  ( -4.000000000000000000, 0.000000000000000000, -5.703399999999999359 ) ) ;
#76267 = CARTESIAN_POINT ( 'NONE',  ( 85.37367768935722268, -60.20197548581520408, -15.42114807968834889 ) ) ;
#76268 = CIRCLE ( 'NONE', #81403, 1.000000000000000888 ) ;
#76269 = CARTESIAN_POINT ( 'NONE',  ( -37.17800977877799085, 306.1414503807761207, 0.6316131526643408156 ) ) ;
#76270 = CARTESIAN_POINT ( 'NONE',  ( -13.56845119367292263, 303.5479323376442835, -10.06459098692300280 ) ) ;
#76271 = DIRECTION ( 'NONE',  ( 0.000000000000000000, -1.000000000000000000, 0.000000000000000000 ) ) ;
#76272 = ORIENTED_EDGE ( 'NONE', *, *, #23809, .F. ) ;
#76273 = CARTESIAN_POINT ( 'NONE',  ( -42.93430011344045738, 435.4574193744091986, 17.27214342660893465 ) ) ;
#76274 = VERTEX_POINT ( 'NONE', #28084 ) ;
#76275 = CARTESIAN_POINT ( 'NONE',  ( 48.26938392169741121, 11.04962899253383313, -14.37319483549308785 ) ) ;
#76276 = FACE_OUTER_BOUND ( 'NONE', #50268, .T. ) ;
#76277 = CIRCLE ( 'NONE', #29810, 3.309500000000007880 ) ;
#76279 = ORIENTED_EDGE ( 'NONE', *, *, #90736, .T. ) ;
#76278 = CARTESIAN_POINT ( 'NONE',  ( 5.929606399591413890, 51.27011112052321096, 8.358468156669783156 ) ) ;
#76280 = CARTESIAN_POINT ( 'NONE',  ( 74.51115553146181014, -22.12425664901256184, 106.6295879739541874 ) ) ;
#76281 = ORIENTED_EDGE ( 'NONE', *, *, #6918, .F. ) ;
#76282 = CARTESIAN_POINT ( 'NONE',  ( 4.001372801367517162, -48.64733069984636415, 43.58293009944993202 ) ) ;
#76283 = FACE_OUTER_BOUND ( 'NONE', #88090, .T. ) ;
#76284 = CARTESIAN_POINT ( 'NONE',  ( 5.082755093536324154, -22.34375000204838457, 5.082755093536326818 ) ) ;
#76285 = CARTESIAN_POINT ( 'NONE',  ( -90.36739715925041594, -57.66608071200965213, -21.81949331871602382 ) ) ;
#76286 = EDGE_CURVE ( 'NONE', #4323, #93999, #100268, .T. ) ;
#76287 = ORIENTED_EDGE ( 'NONE', *, *, #69013, .T. ) ;
#76288 =( NAMED_UNIT ( * ) SI_UNIT ( $, .STERADIAN. ) SOLID_ANGLE_UNIT ( ) );
#76289 = LINE ( 'NONE', #90355, #12733 ) ;
#76290 = CARTESIAN_POINT ( 'NONE',  ( 105.2361638501777321, -52.71710886096133208, 175.0655424517120764 ) ) ;
#76291 = ADVANCED_FACE ( 'NONE', ( #36184 ), #11846, .T. ) ;
#76292 = DIRECTION ( 'NONE',  ( -1.000000000000000000, -0.000000000000000000, -0.000000000000000000 ) ) ;
#76293 = CARTESIAN_POINT ( 'NONE',  ( 5.000000000000000000, 6.123233995736766282E-16, -7.131971428571428184 ) ) ;
#76294 = CARTESIAN_POINT ( 'NONE',  ( -8.000000000000001776, -19.34375000409676915, 3.313708498984758943 ) ) ;
#76295 = CARTESIAN_POINT ( 'NONE',  ( 0.000000000000000000, 29.08768991669519721, 0.000000000000000000 ) ) ;
#76296 = DIRECTION ( 'NONE',  ( 0.000000000000000000, -1.000000000000000000, 0.000000000000000000 ) ) ;
#76297 = CARTESIAN_POINT ( 'NONE',  ( -36.64823341582350480, 437.5392299810052350, 4.281405873620236946 ) ) ;
#76298 = CARTESIAN_POINT ( 'NONE',  ( 0.000000000000000000, 6.123233995736767268E-16, -5.000000000000000888 ) ) ;
#76299 = CARTESIAN_POINT ( 'NONE',  ( 51.88291765283142354, 443.7702288992139188, 638.4430204996707516 ) ) ;
#76300 = DIRECTION ( 'NONE',  ( 1.000000000000000000, 0.000000000000000000, 0.000000000000000000 ) ) ;
#76301 = VERTEX_POINT ( 'NONE', #65053 ) ;
#76302 = FACE_OUTER_BOUND ( 'NONE', #56879, .T. ) ;
#76303 = DIRECTION ( 'NONE',  ( -1.000000000000000000, -1.224606353822377258E-16, -0.000000000000000000 ) ) ;
#76304 = LINE ( 'NONE', #67701, #48033 ) ;
#76305 = CARTESIAN_POINT ( 'NONE',  ( -89.01444542118139225, -30.00000000000000711, 188.7229723381737756 ) ) ;
#76306 = ORIENTED_EDGE ( 'NONE', *, *, #61923, .T. ) ;
#76307 = DIRECTION ( 'NONE',  ( 0.000000000000000000, 0.000000000000000000, -1.000000000000000000 ) ) ;
#76308 = PRESENTATION_LAYER_ASSIGNMENT (  '', '', ( #507 ) ) ;
#76309 = CARTESIAN_POINT ( 'NONE',  ( 80.41579346481609036, -57.50937429630823061, 199.2392246321336415 ) ) ;
#76311 = CARTESIAN_POINT ( 'NONE',  ( 43.70848695378473536, 435.5669781845215311, 16.96397918787648607 ) ) ;
#76310 = PRESENTATION_STYLE_ASSIGNMENT (( #9433 ) ) ;
#76312 = ORIENTED_EDGE ( 'NONE', *, *, #103018, .T. ) ;
#76313 = CARTESIAN_POINT ( 'NONE',  ( 68.10834181227042450, -38.11564430089239863, -31.83369359602357918 ) ) ;
#76314 = CARTESIAN_POINT ( 'NONE',  ( 31.84999999999999787, 3.309500000000003439, 0.000000000000000000 ) ) ;
#76315 = CARTESIAN_POINT ( 'NONE',  ( -44.17836536378455037, 435.2619773020561524, 14.65562696767985074 ) ) ;
#76316 = CARTESIAN_POINT ( 'NONE',  ( -38.80661513268031371, -59.99999999999999289, 50.49608698167829601 ) ) ;
#76317 = CARTESIAN_POINT ( 'NONE',  ( -32.03584064644572749, 439.7197644807975507, 23.90968771023494455 ) ) ;
#76318 = CARTESIAN_POINT ( 'NONE',  ( -86.79595722784087286, -31.74947768238279977, 186.8232286397415862 ) ) ;
#76319 = VERTEX_POINT ( 'NONE', #90398 ) ;
#76320 = DIRECTION ( 'NONE',  ( -1.000000000000000000, -1.224606353822377258E-16, -0.000000000000000000 ) ) ;
#76321 = CARTESIAN_POINT ( 'NONE',  ( -3.991702196745004372, -25.54931392864318340, 28.14104528548392636 ) ) ;
#76322 = CARTESIAN_POINT ( 'NONE',  ( -1.888156768555025566, -49.90642900039781438, 101.9303284617053578 ) ) ;
#76323 =( BOUNDED_SURFACE ( )  B_SPLINE_SURFACE ( 3, 2, ( 
 ( #689, #49812, #49269 ),
 ( #16382, #7750, #16934 ),
 ( #42787, #58447, #1778 ),
 ( #41195, #82716, #1232 ),
 ( #67607, #74080, #66533 ),
 ( #65476, #34202, #40660 ),
 ( #33653, #99407, #57894 ),
 ( #25589, #9336, #26130 ),
 ( #73543, #17470, #100486 ),
 ( #89758, #32605, #98366 ),
 ( #56834, #67074, #66000 ),
 ( #75136, #50859, #165 ) ),
 .UNSPECIFIED., .F., .F., .F. ) 
 B_SPLINE_SURFACE_WITH_KNOTS ( ( 4, 2, 2, 2, 2, 4 ),
 ( 3, 3 ),
 ( 5.421010862427522170E-19, 0.0004396180695635565935, 0.0008792361391271126449, 0.001758472278254224856, 0.002637708417381336851, 0.003516944556508449279 ),
 ( 0.000000000000000000, 1.000000000000000000 ),
 .UNSPECIFIED. ) 
 GEOMETRIC_REPRESENTATION_ITEM ( )  RATIONAL_B_SPLINE_SURFACE ( (
 ( 1.000000000000000000, 0.9193453746270702220, 1.000000000000000000),
 ( 1.000000000000000000, 0.9231392589453282227, 1.000000000000000000),
 ( 1.000000000000000000, 0.9252300355217707439, 1.000000000000000000),
 ( 1.000000000000000000, 0.9257136340830524057, 1.000000000000000000),
 ( 1.000000000000000000, 0.9240662039546210238, 1.000000000000000000),
 ( 1.000000000000000000, 0.9140412217422946295, 1.000000000000000000),
 ( 1.000000000000000000, 0.9005671153104095605, 1.000000000000000000),
 ( 1.000000000000000000, 0.8672639112272950701, 1.000000000000000000),
 ( 1.000000000000000000, 0.8470036231255452241, 1.000000000000000000),
 ( 1.000000000000000000, 0.8036658034632763181, 1.000000000000000000),
 ( 1.000000000000000000, 0.7801896332603067696, 1.000000000000000000),
 ( 1.000000000000000000, 0.7557288854856922811, 1.000000000000000000) ) ) 
 REPRESENTATION_ITEM ( '' )  SURFACE ( )  );
#76324 = AXIS2_PLACEMENT_3D ( 'NONE', #58499, #740, #9381 ) ;
#76325 = CARTESIAN_POINT ( 'NONE',  ( 99.17777777777777715, -4.171999999999998820, 5.616230220889773285E-16 ) ) ;
#76326 = VERTEX_POINT ( 'NONE', #72609 ) ;
#76327 = CARTESIAN_POINT ( 'NONE',  ( 7.500000000000007105, 39.99999999999998579, -68.91429205785453860 ) ) ;
#76328 = COLOUR_RGB ( '', 0.09019608, 0.27058824, 0.51372549) ;
#76329 = CARTESIAN_POINT ( 'NONE',  ( -5.880230824525982669, -4.999999999999742428, -15.32427097195931864 ) ) ;
#76330 = CARTESIAN_POINT ( 'NONE',  ( 2.235495008889195345E-15, -15.58845726811994759, -13.00000000000000000 ) ) ;
#76331 = AXIS2_PLACEMENT_3D ( 'NONE', #3733, #42577, #69528 ) ;
#76332 = CARTESIAN_POINT ( 'NONE',  ( 23.66085433736493471, 295.2283149760944525, -9.919964171137618081 ) ) ;
#76333 = CARTESIAN_POINT ( 'NONE',  ( 45.43339346675878687, 430.7348383325900727, 7.234598910837349628 ) ) ;
#76334 = DIRECTION ( 'NONE',  ( -0.000000000000000000, -0.000000000000000000, 1.000000000000000000 ) ) ;
#76335 = CARTESIAN_POINT ( 'NONE',  ( 8.718949332298615573, 53.63223895871195879, -4.031152949375384154 ) ) ;
#76336 = CARTESIAN_POINT ( 'NONE',  ( 100.4059631369621570, -60.00000000000003553, 69.07260714096372567 ) ) ;
#76337 = CARTESIAN_POINT ( 'NONE',  ( -83.25441183928721500, -18.68590906670072371, 143.1452550271331177 ) ) ;
#76338 = EDGE_LOOP ( 'NONE', ( #37887, #90160, #15734, #87219, #9952, #104810, #46799, #33276 ) ) ;
#76339 = DIRECTION ( 'NONE',  ( 0.000000000000000000, -1.000000000000000000, 0.000000000000000000 ) ) ;
#76340 = CARTESIAN_POINT ( 'NONE',  ( 5.728413875956875678, 253.5806422645339637, 1.802282772585232173 ) ) ;
#76341 = CARTESIAN_POINT ( 'NONE',  ( 23.63580155301217189, -57.67366959424659711, 42.85678083413705508 ) ) ;
#76342 = DIRECTION ( 'NONE',  ( 0.000000000000000000, 1.000000000000000000, 0.000000000000000000 ) ) ;
#76343 = CARTESIAN_POINT ( 'NONE',  ( 3.225563553360571767, 36.35307765080715825, -4.999999999999999112 ) ) ;
#76344 = FACE_OUTER_BOUND ( 'NONE', #57854, .T. ) ;
#76345 = ORIENTED_EDGE ( 'NONE', *, *, #11209, .F. ) ;
#76346 = UNCERTAINTY_MEASURE_WITH_UNIT (LENGTH_MEASURE( 1.000000000000000082E-05 ), #70229, 'distance_accuracy_value', 'NONE');
#76347 = CARTESIAN_POINT ( 'NONE',  ( 31.30845532010006949, 439.0134050661394554, 22.67842551736903189 ) ) ;
#76348 = ORIENTED_EDGE ( 'NONE', *, *, #64402, .F. ) ;
#76349 = DIRECTION ( 'NONE',  ( 0.8191520442889881348, 0.000000000000000000, 0.5735764363510513775 ) ) ;
#76350 = CARTESIAN_POINT ( 'NONE',  ( 5.406991766687864853, 42.00000000000000000, -69.18631089694002867 ) ) ;
#76351 = EDGE_CURVE ( 'NONE', #40837, #24456, #98471, .T. ) ;
#76352 = CARTESIAN_POINT ( 'NONE',  ( -62.34828826644581312, 50.00000000000000000, -10.72527895994686986 ) ) ;
#76353 = CARTESIAN_POINT ( 'NONE',  ( 5.000000000000039968, -13.46492586503063293, 12.82257630554847694 ) ) ;
#76354 = ADVANCED_FACE ( 'NONE', ( #48849 ), #106498, .T. ) ;
#76355 = ORIENTED_EDGE ( 'NONE', *, *, #78794, .T. ) ;
#76356 = CARTESIAN_POINT ( 'NONE',  ( -13.00000000000003730, -65.00000000000000000, -4.000000000000002665 ) ) ;
#76358 = CARTESIAN_POINT ( 'NONE',  ( 21.41473547131232991, -42.95433426084449735, 31.73274252099677639 ) ) ;
#76357 = CARTESIAN_POINT ( 'NONE',  ( -78.25705875637353870, -14.21045842199447939, 182.3370610225134953 ) ) ;
#76359 = EDGE_CURVE ( 'NONE', #77653, #52640, #41307, .T. ) ;
#76360 = CARTESIAN_POINT ( 'NONE',  ( 110.0428892116505040, 17.51648154115788358, -55.02144460582523777 ) ) ;
#76361 = CARTESIAN_POINT ( 'NONE',  ( 0.000000000000000000, 49.00000000000000000, 0.000000000000000000 ) ) ;
#76362 = CARTESIAN_POINT ( 'NONE',  ( -40.12004793384570434, -60.26222130539476041, 43.34212177527130194 ) ) ;
#76363 = CARTESIAN_POINT ( 'NONE',  ( -36.68673791898479664, 18.64284798593215342, -11.44574982652938999 ) ) ;
#76364 = UNCERTAINTY_MEASURE_WITH_UNIT (LENGTH_MEASURE( 1.000000000000000082E-05 ), #44633, 'distance_accuracy_value', 'NONE');
#76365 = ORIENTED_EDGE ( 'NONE', *, *, #87637, .T. ) ;
#76366 = SURFACE_STYLE_FILL_AREA ( #8975 ) ;
#76367 = DIRECTION ( 'NONE',  ( -0.000000000000000000, -1.000000000000000000, -0.000000000000000000 ) ) ;
#76368 = CARTESIAN_POINT ( 'NONE',  ( -13.72588371288480857, -57.01106425417226120, 29.76328409196439750 ) ) ;
#76369 =( GEOMETRIC_REPRESENTATION_CONTEXT ( 3 ) GLOBAL_UNCERTAINTY_ASSIGNED_CONTEXT ( ( #28754 ) ) GLOBAL_UNIT_ASSIGNED_CONTEXT ( ( #93708, #34965, #86168 ) ) REPRESENTATION_CONTEXT ( 'NONE', 'WORKASPACE' ) );
#76370 = DIRECTION ( 'NONE',  ( 1.000000000000000000, 1.224606353822377258E-16, 0.000000000000000000 ) ) ;
#76371 = CARTESIAN_POINT ( 'NONE',  ( 6.585468679846623985, 7.640532685286893333, -0.2337908078075575935 ) ) ;
#76372 = CARTESIAN_POINT ( 'NONE',  ( -30.00000000000000355, 486.7182699440880356, 5.240683647336917161 ) ) ;
#76373 = EDGE_LOOP ( 'NONE', ( #60768, #48156, #49588, #76157, #18053 ) ) ;
#76374 = CARTESIAN_POINT ( 'NONE',  ( -15.64878411475348408, 36.78373704832288382, -23.72567384382504585 ) ) ;
#76375 = ORIENTED_EDGE ( 'NONE', *, *, #105012, .F. ) ;
#76376 = CARTESIAN_POINT ( 'NONE',  ( 99.27928464162405930, -30.00000000000000000, 188.1417282079006839 ) ) ;
#76377 = CARTESIAN_POINT ( 'NONE',  ( 42.15373538487478555, 39.53920096513062532, -50.09085211413447070 ) ) ;
#76378 = AXIS2_PLACEMENT_3D ( 'NONE', #2411, #53102, #86025 ) ;
#76380 = EDGE_CURVE ( 'NONE', #74905, #76835, #59218, .T. ) ;
#76379 = CARTESIAN_POINT ( 'NONE',  ( 66.74444444444444002, -3.309500000000000774, 4.475777889183797681E-16 ) ) ;
#76381 = CARTESIAN_POINT ( 'NONE',  ( 83.66451334722914623, -30.00000000000000711, 48.10376369561402754 ) ) ;
#76382 = SURFACE_STYLE_FILL_AREA ( #43503 ) ;
#76383 = ORIENTED_EDGE ( 'NONE', *, *, #94623, .T. ) ;
#76384 = ORIENTED_EDGE ( 'NONE', *, *, #41028, .T. ) ;
#76385 = ORIENTED_EDGE ( 'NONE', *, *, #94376, .T. ) ;
#76387 = ORIENTED_EDGE ( 'NONE', *, *, #10963, .F. ) ;
#76386 = CARTESIAN_POINT ( 'NONE',  ( -32.81992448453854649, 465.7192846569213884, 11.17271167765305506 ) ) ;
#76388 = DIRECTION ( 'NONE',  ( -1.000000000000000000, 0.000000000000000000, 0.000000000000000000 ) ) ;
#76389 = MECHANICAL_DESIGN_GEOMETRIC_PRESENTATION_REPRESENTATION (  '', ( #7459 ), #73198 ) ;
#76390 = CARTESIAN_POINT ( 'NONE',  ( -19.83463548332447601, 303.8035096162418540, 9.926734387303332241 ) ) ;
#76391 = CARTESIAN_POINT ( 'NONE',  ( 5.909155701201247446, -13.86261680188730772, 1.073778020691672941 ) ) ;
#76392 = CARTESIAN_POINT ( 'NONE',  ( -31.22086652946737217, 398.4027782038555756, 25.40425845524832482 ) ) ;
#76393 = ORIENTED_EDGE ( 'NONE', *, *, #52613, .T. ) ;
#76394 = CARTESIAN_POINT ( 'NONE',  ( 9.999999999999989342, 49.99999999999999289, -83.69100306251233690 ) ) ;
#76395 = VERTEX_POINT ( 'NONE', #70631 ) ;
#76396 = DIRECTION ( 'NONE',  ( -1.000000000000000000, -1.224606353822377258E-16, -0.000000000000000000 ) ) ;
#76397 = CARTESIAN_POINT ( 'NONE',  ( 75.45370944691039483, -38.35105784206446344, 173.7888497777023815 ) ) ;
#76398 = CARTESIAN_POINT ( 'NONE',  ( 5.285714285714282923, 0.1991252733425875887, 103.1763305333244318 ) ) ;
#76399 = CARTESIAN_POINT ( 'NONE',  ( 25.28412188507380165, 304.8344537246382515, 10.37783159469212357 ) ) ;
#76400 = CARTESIAN_POINT ( 'NONE',  ( -5.728413875956867685, 246.4193577354659510, 1.802282772585255266 ) ) ;
#76401 = STYLED_ITEM ( 'NONE', ( #15664 ), #17835 ) ;
#76402 = ORIENTED_EDGE ( 'NONE', *, *, #81398, .T. ) ;
#76403 = CARTESIAN_POINT ( 'NONE',  ( 29.28872172473180768, 8.962789800749073166, -42.04350091203807693 ) ) ;
#76404 = DIRECTION ( 'NONE',  ( 0.000000000000000000, 0.000000000000000000, -1.000000000000000000 ) ) ;
#76405 = CARTESIAN_POINT ( 'NONE',  ( 99.17777777777777715, 1.023464760207051730E-14, 0.000000000000000000 ) ) ;
#76406 = AXIS2_PLACEMENT_3D ( 'NONE', #41776, #91409, #17522 ) ;
#76407 = CARTESIAN_POINT ( 'NONE',  ( 0.000000000000000000, 45.00000000000000711, 0.000000000000000000 ) ) ;
#76408 = EDGE_CURVE ( 'NONE', #42218, #102336, #77163, .T. ) ;
#76409 = CARTESIAN_POINT ( 'NONE',  ( -5.656854249492379694, -20.93749999999999289, -5.656854249492380582 ) ) ;
#76411 = EDGE_LOOP ( 'NONE', ( #14580, #50498, #67780 ) ) ;
#76410 = MECHANICAL_DESIGN_GEOMETRIC_PRESENTATION_REPRESENTATION (  '', ( #72933 ), #50531 ) ;
#76413 = CARTESIAN_POINT ( 'NONE',  ( 7.551892080562055298, -88.00987702539381985, 2.647003822403974471 ) ) ;
#76412 = DIRECTION ( 'NONE',  ( 0.000000000000000000, 0.000000000000000000, 1.000000000000000000 ) ) ;
#76414 = CARTESIAN_POINT ( 'NONE',  ( -4.628159615119684211, -2.310801729693849005, 102.5435725457685834 ) ) ;
#76415 = FACE_OUTER_BOUND ( 'NONE', #20743, .T. ) ;
#76416 = CARTESIAN_POINT ( 'NONE',  ( 0.04725809328185524155, -9.175759667312531676, -8.057670357645365655 ) ) ;
#76417 = DIRECTION ( 'NONE',  ( 0.000000000000000000, 0.000000000000000000, 1.000000000000000000 ) ) ;
#76418 = ADVANCED_FACE ( 'NONE', ( #6812 ), #91053, .T. ) ;
#76419 = EDGE_CURVE ( 'NONE', #39650, #92807, #3195, .T. ) ;
#76420 = PRESENTATION_STYLE_ASSIGNMENT (( #36550 ) ) ;
#76421 = DIRECTION ( 'NONE',  ( -1.000000000000000000, -1.224606353822377258E-16, -0.000000000000000000 ) ) ;
#76422 = CARTESIAN_POINT ( 'NONE',  ( 85.55340563104743978, -61.06305125096141495, 193.9660559021026813 ) ) ;
#76423 = CARTESIAN_POINT ( 'NONE',  ( -27.10511071441193565, 34.75829513984539432, -7.556984339685824281 ) ) ;
#76424 = CARTESIAN_POINT ( 'NONE',  ( -8.340586800786125465, 120.4027948985839913, 5.000000000000000000 ) ) ;
#76425 = VERTEX_POINT ( 'NONE', #13432 ) ;
#76426 = CARTESIAN_POINT ( 'NONE',  ( 61.19758744976927289, -57.67094294300110136, -37.37908601888510418 ) ) ;
#76427 = SURFACE_SIDE_STYLE ('',( #44624 ) ) ;
#76428 = CARTESIAN_POINT ( 'NONE',  ( -46.00000000000000000, 459.9277931459707247, 6.461582622321701663 ) ) ;
#76429 =( NAMED_UNIT ( * ) SI_UNIT ( $, .STERADIAN. ) SOLID_ANGLE_UNIT ( ) );
#76430 = CARTESIAN_POINT ( 'NONE',  ( -90.85589696943300453, -30.00000000000000711, 93.50266285681084355 ) ) ;
#76431 = ADVANCED_FACE ( 'NONE', ( #89863 ), #40771, .T. ) ;
#76432 = CARTESIAN_POINT ( 'NONE',  ( 104.3757837139179117, -5.000000000000000000, 0.000000000000000000 ) ) ;
#76433 = CARTESIAN_POINT ( 'NONE',  ( 26.08349330513380693, 1.593028355512270962E-15, 0.000000000000000000 ) ) ;
#76435 = DIRECTION ( 'NONE',  ( -1.000000000000000000, -0.000000000000000000, -0.000000000000000000 ) ) ;
#76434 = CARTESIAN_POINT ( 'NONE',  ( -9.918010731619586906, 246.2084831515677195, -1.300854425901577516 ) ) ;
#76436 = EDGE_CURVE ( 'NONE', #78081, #15372, #23563, .T. ) ;
#76437 = CARTESIAN_POINT ( 'NONE',  ( 6.311611455838505691, -49.69043234645462803, 39.49845025518488484 ) ) ;
#76438 = CARTESIAN_POINT ( 'NONE',  ( -8.966563029945419316, -20.28652515761861608, 27.26759621302640824 ) ) ;
#76439 = CARTESIAN_POINT ( 'NONE',  ( -19.25089800403961959, 49.99999999999999289, 60.24512152074786542 ) ) ;
#76440 = CARTESIAN_POINT ( 'NONE',  ( -42.89416851001919895, 486.3091028888858887, 6.394136786226152225 ) ) ;
#76441 = FACE_OUTER_BOUND ( 'NONE', #26424, .T. ) ;
#76442 = COLOUR_RGB ( '', 0.66274510, 0.83137255, 0.94901961) ;
#76443 = ADVANCED_FACE ( 'NONE', ( #81216 ), #40243, .T. ) ;
#76444 = CARTESIAN_POINT ( 'NONE',  ( 52.95862039844607239, -28.11919995386964644, -27.17888508974323614 ) ) ;
#76445 = AXIS2_PLACEMENT_3D ( 'NONE', #27568, #3786, #103533 ) ;
#76446 = CARTESIAN_POINT ( 'NONE',  ( -24.40073486819268211, -25.56284969913130567, 29.25320355220248203 ) ) ;
#76447 = ORIENTED_EDGE ( 'NONE', *, *, #84430, .T. ) ;
#76448 = CARTESIAN_POINT ( 'NONE',  ( 6.769785244694104698, 9.417081608196284037, -1.797443303175162876 ) ) ;
#76449 = CARTESIAN_POINT ( 'NONE',  ( -9.645512969475854348, 108.0110315067572770, -2.645801731561390646 ) ) ;
#76450 = CARTESIAN_POINT ( 'NONE',  ( -20.33180723614214358, -46.43912101697812744, 32.18596333272415677 ) ) ;
#76451 = VECTOR ( 'NONE', #5403, 1000.000000000000000 ) ;
#76452 = CARTESIAN_POINT ( 'NONE',  ( -48.68264843209982473, -27.19707998762441292, -28.31473230945048059 ) ) ;
#76454 = CARTESIAN_POINT ( 'NONE',  ( 39.67350626972746142, 485.2175160376946224, -4.383017744911751556 ) ) ;
#76453 = FACE_OUTER_BOUND ( 'NONE', #23162, .T. ) ;
#76455 = ORIENTED_EDGE ( 'NONE', *, *, #55803, .T. ) ;
#76456 = CARTESIAN_POINT ( 'NONE',  ( -36.19868307047016742, 437.5496401283068622, 4.275188479071593939 ) ) ;
#76457 = ORIENTED_EDGE ( 'NONE', *, *, #82938, .T. ) ;
#76458 = DIRECTION ( 'NONE',  ( 0.000000000000000000, 0.000000000000000000, 1.000000000000000000 ) ) ;
#76459 = ADVANCED_FACE ( 'NONE', ( #15970 ), #41834, .T. ) ;
#76460 = CARTESIAN_POINT ( 'NONE',  ( 15.43760447746161546, 2.782577468887291072, 1.950845582985621940 ) ) ;
#76461 = CARTESIAN_POINT ( 'NONE',  ( 0.000000000000000000, 2.253471898105741801E-15, 6.500000000000000000 ) ) ;
#76462 = ORIENTED_EDGE ( 'NONE', *, *, #50059, .F. ) ;
#76463 = SURFACE_STYLE_FILL_AREA ( #51657 ) ;
#76464 =( NAMED_UNIT ( * ) SI_UNIT ( $, .STERADIAN. ) SOLID_ANGLE_UNIT ( ) );
#76465 = CARTESIAN_POINT ( 'NONE',  ( 99.83641921256408125, -45.27153168086159241, 192.7518997590976539 ) ) ;
#76467 = CARTESIAN_POINT ( 'NONE',  ( -7.003653396366583905, -8.942937944403233530, -3.866846144092864535 ) ) ;
#76466 = CARTESIAN_POINT ( 'NONE',  ( 19.65497437631472977, -25.11138553214667368, 28.50946425220601554 ) ) ;
#76468 = VERTEX_POINT ( 'NONE', #9454 ) ;
#76469 = ORIENTED_EDGE ( 'NONE', *, *, #12182, .F. ) ;
#76470 = ORIENTED_EDGE ( 'NONE', *, *, #47201, .T. ) ;
#76471 = CARTESIAN_POINT ( 'NONE',  ( 25.69418243244179934, 306.7938479978786859, 10.60760969656614172 ) ) ;
#76472 = CIRCLE ( 'NONE', #81612, 3.309500000000007880 ) ;
#76473 = CARTESIAN_POINT ( 'NONE',  ( -3.313708498984779371, -28.53124999999999289, -7.999999999999981348 ) ) ;
#76474 = CARTESIAN_POINT ( 'NONE',  ( 9.653963884811064489, 53.40254541166815017, 3.408400523946627292 ) ) ;
#76475 = EDGE_LOOP ( 'NONE', ( #106524, #49305, #42159, #72704, #101032 ) ) ;
#76476 = ADVANCED_FACE ( 'NONE', ( #59636 ), #92510, .T. ) ;
#76477 = PRESENTATION_LAYER_ASSIGNMENT (  '', '', ( #78181 ) ) ;
#76478 = FACE_BOUND ( 'NONE', #100945, .T. ) ;
#76479 = CARTESIAN_POINT ( 'NONE',  ( 0.000000000000000000, -50.00000000000000000, 112.0000000000000000 ) ) ;
#76480 = VECTOR ( 'NONE', #89024, 1000.000000000000000 ) ;
#76482 = B_SPLINE_CURVE_WITH_KNOTS ( 'NONE', 3,
 ( #54150, #15833, #31522, #65455, #14227, #104855, #81603, #7205, #47133, #48189, #105895, #64404, #32042, #24502, #97277, #63880, #55221, #64922, #88147, #80028, #23426, #55736 ),
 .UNSPECIFIED., .F., .F.,
 ( 4, 2, 2, 2, 2, 2, 2, 2, 2, 2, 4 ),
 ( 0.007110638423152015018, 0.007613994425099801511, 0.008117350427047587136, 0.008620706428995374496, 0.008872384429969270778, 0.009124062430943168794, 0.009375740431917065076, 0.009627418432890963093, 0.01013077443483876260, 0.01063413043678656383, 0.01113748643873436334 ),
 .UNSPECIFIED. ) ;
#76481 = CARTESIAN_POINT ( 'NONE',  ( 20.11650669486618881, 0.000000000000000000, 4.000000000000000888 ) ) ;
#76483 = CARTESIAN_POINT ( 'NONE',  ( -83.34872437439757675, -59.99999999999513278, -28.64704504306356370 ) ) ;
#76484 = CARTESIAN_POINT ( 'NONE',  ( 7.551560007654697593, -68.00910351806993503, -2.648022159607834602 ) ) ;
#76485 = LINE ( 'NONE', #83515, #45967 ) ;
#76486 = DIRECTION ( 'NONE',  ( -1.000000000000000000, -1.224606353822377258E-16, -0.000000000000000000 ) ) ;
#76487 = CARTESIAN_POINT ( 'NONE',  ( -86.89976874444957389, -30.00000000000007105, -18.81729257278660583 ) ) ;
#76488 = EDGE_CURVE ( 'NONE', #96258, #65330, #96294, .T. ) ;
#76489 = CARTESIAN_POINT ( 'NONE',  ( -44.14911905790362567, 464.3766534541991291, 9.623404994943159707 ) ) ;
#76490 = ADVANCED_FACE ( 'NONE', ( #18120 ), #10527, .T. ) ;
#76491 = CARTESIAN_POINT ( 'NONE',  ( -50.66715319276153195, -18.73003936557022797, 44.89420085366170809 ) ) ;
#76492 = ORIENTED_EDGE ( 'NONE', *, *, #37050, .F. ) ;
#76493 = CARTESIAN_POINT ( 'NONE',  ( -0.5366512190794670012, 21.81880124593116221, 6.980675135559732958 ) ) ;
#76494 = ORIENTED_EDGE ( 'NONE', *, *, #99492, .T. ) ;
#76495 = CARTESIAN_POINT ( 'NONE',  ( 0.000000000000000000, 52.29617335651133914, 0.000000000000000000 ) ) ;
#76496 = CARTESIAN_POINT ( 'NONE',  ( 12.61650669486618881, 1.474610560812782335E-15, 0.000000000000000000 ) ) ;
#76497 = ADVANCED_FACE ( 'NONE', ( #50444 ), #91981, .F. ) ;
#76498 = CARTESIAN_POINT ( 'NONE',  ( 4.903871675326607615, -7.979141926985056976, -3.461400506969853463 ) ) ;
#76499 = VERTEX_POINT ( 'NONE', #2967 ) ;
#76500 = CARTESIAN_POINT ( 'NONE',  ( 5.981691436642411652, 246.0273090080588361, -0.5384679144502751980 ) ) ;
#76501 = CARTESIAN_POINT ( 'NONE',  ( 89.19545386432166367, -30.00000000004024159, 14.25136593696676179 ) ) ;
#76502 = DIRECTION ( 'NONE',  ( 0.000000000000000000, 0.000000000000000000, -1.000000000000000000 ) ) ;
#76503 = SURFACE_STYLE_USAGE ( .BOTH. , #102381 ) ;
#76505 = ADVANCED_FACE ( 'NONE', ( #19219 ), #29257, .T. ) ;
#76504 = CARTESIAN_POINT ( 'NONE',  ( 7.099152780515114891, 41.70084721948487072, -59.82719249545999674 ) ) ;
#76506 = CARTESIAN_POINT ( 'NONE',  ( 23.70422451876635250, 42.00000000000004263, -88.20421627930062414 ) ) ;
#76507 = CARTESIAN_POINT ( 'NONE',  ( 89.77911554397552152, -29.99999999999999645, 189.6830308129038087 ) ) ;
#76508 = PRODUCT_DEFINITION_SHAPE ( 'NONE', 'NONE',  #102301 ) ;
#76509 = CARTESIAN_POINT ( 'NONE',  ( -11.54078658013951397, 43.31764940862575486, -14.27918301262186063 ) ) ;
#76510 = CARTESIAN_POINT ( 'NONE',  ( 30.56153846153846132, 1.411358822780289120E-15, 0.000000000000000000 ) ) ;
#76511 = PRESENTATION_LAYER_ASSIGNMENT (  '', '', ( #54097 ) ) ;
#76512 = EDGE_LOOP ( 'NONE', ( #18687, #74260, #58619, #68724, #96864 ) ) ;
#76513 = ORIENTED_EDGE ( 'NONE', *, *, #90136, .F. ) ;
#76514 = CARTESIAN_POINT ( 'NONE',  ( 52.39836483974727344, -39.50506518785934418, 55.00803164924739974 ) ) ;
#76515 = CARTESIAN_POINT ( 'NONE',  ( 5.373715277452113526, 41.43915641971339170, -58.48990532576927848 ) ) ;
#76516 = LINE ( 'NONE', #51706, #96199 ) ;
#76517 = EDGE_LOOP ( 'NONE', ( #20290, #51480, #14253, #4645, #11673 ) ) ;
#76518 = CARTESIAN_POINT ( 'NONE',  ( -87.73394717290364042, -38.36776824219355575, -19.93160110628211967 ) ) ;
#76519 = VERTEX_POINT ( 'NONE', #98307 ) ;
#76520 = CARTESIAN_POINT ( 'NONE',  ( 110.3445969107558824, -38.35603028189417785, 183.6558594675337872 ) ) ;
#76521 = CARTESIAN_POINT ( 'NONE',  ( 11.88722850048356960, 16.71180228297125936, 9.289706601079268822 ) ) ;
#76522 = CARTESIAN_POINT ( 'NONE',  ( 87.30608338596761087, -45.28275021690784286, 53.23273715140581430 ) ) ;
#76523 = CARTESIAN_POINT ( 'NONE',  ( -16.75187969033532553, 34.99134772383131065, 21.80698433968612093 ) ) ;
#76524 = CARTESIAN_POINT ( 'NONE',  ( 0.000000000000000000, -3.035766082959412415E-15, 8.000000000000000000 ) ) ;
#76525 = VECTOR ( 'NONE', #80697, 1000.000000000000000 ) ;
#76526 = FACE_OUTER_BOUND ( 'NONE', #93387, .T. ) ;
#76527 = AXIS2_PLACEMENT_3D ( 'NONE', #23578, #56425, #81234 ) ;
#76528 = FACE_OUTER_BOUND ( 'NONE', #77617, .T. ) ;
#76529 = CARTESIAN_POINT ( 'NONE',  ( 8.020869781912113083, 104.2554943876038180, 0.000000000000000000 ) ) ;
#76530 = ORIENTED_EDGE ( 'NONE', *, *, #45458, .F. ) ;
#76531 = DIRECTION ( 'NONE',  ( 1.000000000000000000, -0.000000000000000000, -0.000000000000000000 ) ) ;
#76532 = CARTESIAN_POINT ( 'NONE',  ( 7.036764705882358584, 40.00000000373366049, -71.06385277390856459 ) ) ;
#76533 = CARTESIAN_POINT ( 'NONE',  ( 0.000000000000000000, 0.000000000000000000, -13.00000000000000000 ) ) ;
#76534 = VERTEX_POINT ( 'NONE', #64875 ) ;
#76535 = CARTESIAN_POINT ( 'NONE',  ( -34.82075917463970427, 344.3979323805427839, 0.4374665251995884518 ) ) ;
#76536 = CARTESIAN_POINT ( 'NONE',  ( -34.73046204960461836, 304.6187811521189701, 12.21458540402294091 ) ) ;
#76537 = CARTESIAN_POINT ( 'NONE',  ( 0.000000000000000000, 4.898587196589412829E-16, -4.000000000000000000 ) ) ;
#76538 = CARTESIAN_POINT ( 'NONE',  ( 8.000000000000000000, -22.99999999999999289, 0.000000000000000000 ) ) ;
#76539 = CARTESIAN_POINT ( 'NONE',  ( 4.898587196589412829E-16, -24.12499999999999289, -8.000000000000000000 ) ) ;
#76540 = PRESENTATION_STYLE_ASSIGNMENT (( #44196 ) ) ;
#76541 = EDGE_CURVE ( 'NONE', #104233, #58364, #80785, .T. ) ;
#76542 = CARTESIAN_POINT ( 'NONE',  ( 15.39058602336948667, 44.07990289552515151, -5.264532584975986751 ) ) ;
#76543 = ORIENTED_EDGE ( 'NONE', *, *, #94713, .F. ) ;
#76544 = CARTESIAN_POINT ( 'NONE',  ( 85.66370408561847682, -25.20792820135650203, 174.6146224505659177 ) ) ;
#76545 = DIRECTION ( 'NONE',  ( 0.000000000000000000, 0.000000000000000000, -1.000000000000000000 ) ) ;
#76546 = CARTESIAN_POINT ( 'NONE',  ( 6.162888688655344893, 3.752776749732562589, -6.500000000000000888 ) ) ;
#76547 = ORIENTED_EDGE ( 'NONE', *, *, #35494, .T. ) ;
#76548 = CARTESIAN_POINT ( 'NONE',  ( -89.51184282953521176, -45.26536304831822122, 67.81581898571103295 ) ) ;
#76549 = CARTESIAN_POINT ( 'NONE',  ( 8.999999999999994671, -46.00000000000000000, 42.58845726811989607 ) ) ;
#76550 = CARTESIAN_POINT ( 'NONE',  ( -13.73780227957491284, -3.000000000000002665, -78.37846873786676838 ) ) ;
#76551 = DIRECTION ( 'NONE',  ( -0.000000000000000000, 1.000000000000000000, 0.000000000000000000 ) ) ;
#76552 = CARTESIAN_POINT ( 'NONE',  ( -27.80883096284195588, -28.76322849883876742, -38.27309149394403676 ) ) ;
#76553 =( GEOMETRIC_REPRESENTATION_CONTEXT ( 3 ) GLOBAL_UNCERTAINTY_ASSIGNED_CONTEXT ( ( #76111 ) ) GLOBAL_UNIT_ASSIGNED_CONTEXT ( ( #10225, #83577, #43141 ) ) REPRESENTATION_CONTEXT ( 'NONE', 'WORKASPACE' ) );
#76555 = CIRCLE ( 'NONE', #67949, 4.000000000000001776 ) ;
#76554 = APPLICATION_PROTOCOL_DEFINITION ( 'draft international standard', 'automotive_design', 1998, #52789 ) ;
#76556 = CARTESIAN_POINT ( 'NONE',  ( 41.54280867975291613, -60.00000000000000711, 54.42080625159498197 ) ) ;
#76557 = CARTESIAN_POINT ( 'NONE',  ( 30.67417392544069443, -32.89657424032979804, 40.97062061678585820 ) ) ;
#76558 = CARTESIAN_POINT ( 'NONE',  ( 7.744168461338428955, 108.4625406171515465, 2.019395720771551606 ) ) ;
#76559 = CARTESIAN_POINT ( 'NONE',  ( 27.26803836058585517, -20.37211081801200052, 31.76419521842516858 ) ) ;
#76561 = CARTESIAN_POINT ( 'NONE',  ( -12.34390528153764421, 20.39976729514925680, 6.763647308493165866 ) ) ;
#76560 = CARTESIAN_POINT ( 'NONE',  ( -27.47606363769024185, -30.73727070043888432, 39.27975643966717456 ) ) ;
#76562 = EDGE_CURVE ( 'NONE', #8034, #63533, #6726, .T. ) ;
#76563 = CARTESIAN_POINT ( 'NONE',  ( 0.6295717893779785301, 294.8518027745081440, -10.00000000019932855 ) ) ;
#76564 = CARTESIAN_POINT ( 'NONE',  ( 45.17824257314219949, 354.4244853104167987, 3.762393652172960845 ) ) ;
#76565 = CARTESIAN_POINT ( 'NONE',  ( 44.78945892759311675, 0.000000000000000000, 5.000000000000002665 ) ) ;
#76566 = DIRECTION ( 'NONE',  ( 0.000000000000000000, 0.000000000000000000, -1.000000000000000000 ) ) ;
#76567 = EDGE_LOOP ( 'NONE', ( #41220, #21273, #44764, #80867, #68871 ) ) ;
#76568 = EDGE_CURVE ( 'NONE', #22777, #67117, #102160, .T. ) ;
#76569 = CARTESIAN_POINT ( 'NONE',  ( -11.82165952410163356, 294.5900423753296309, -10.05563889079273210 ) ) ;
#76570 = CARTESIAN_POINT ( 'NONE',  ( -17.49999999999995381, 51.99573851567584626, 60.30773471724109669 ) ) ;
#76571 = DIRECTION ( 'NONE',  ( -1.000000000000000000, 0.000000000000000000, 0.000000000000000000 ) ) ;
#76572 = CARTESIAN_POINT ( 'NONE',  ( -6.499999999999999112, -3.752776749732587902, -6.064240316920403551 ) ) ;
#76575 = CARTESIAN_POINT ( 'NONE',  ( 9.686630580550103176, -60.22816686990648805, -36.71166719284434521 ) ) ;
#76574 = CARTESIAN_POINT ( 'NONE',  ( 9.798380800342677333, 253.4680065431550986, -2.010350564680340568 ) ) ;
#76573 = B_SPLINE_CURVE_WITH_KNOTS ( 'NONE', 3,
 ( #27664, #77766, #86932, #44882 ),
 .UNSPECIFIED., .F., .F.,
 ( 4, 4 ),
 ( 0.0009266594673085438907, 0.02188556764208124394 ),
 .UNSPECIFIED. ) ;
#76576 = AXIS2_PLACEMENT_3D ( 'NONE', #72271, #45884, #64204 ) ;
#76577 = ORIENTED_EDGE ( 'NONE', *, *, #26697, .T. ) ;
#76578 = LINE ( 'NONE', #11845, #75428 ) ;
#76579 = CARTESIAN_POINT ( 'NONE',  ( 0.5805565836007605673, -3.752776749732561257, 6.500000000000000000 ) ) ;
#76580 = VERTEX_POINT ( 'NONE', #58923 ) ;
#76581 = CARTESIAN_POINT ( 'NONE',  ( 5.000000000000000000, 6.123233995736766282E-16, -7.131971428571428184 ) ) ;
#76582 = CARTESIAN_POINT ( 'NONE',  ( 30.55529413189656651, 11.20957620317260428, -39.95174307500007416 ) ) ;
#76583 = CARTESIAN_POINT ( 'NONE',  ( 84.73333333333332007, 1.023464760207051730E-14, 0.000000000000000000 ) ) ;
#76585 = AXIS2_PLACEMENT_3D ( 'NONE', #1645, #17335, #41061 ) ;
#76584 = PRODUCT_DEFINITION ( 'UNKNOWN', '', #43929, #15473 ) ;
#76586 = CARTESIAN_POINT ( 'NONE',  ( -94.20106335591412972, -60.00000000000000711, 42.96664062321771382 ) ) ;
#76587 = PRESENTATION_STYLE_ASSIGNMENT (( #83614 ) ) ;
#76588 = CONICAL_SURFACE ( 'NONE', #30131, 3.309500000000007880, 0.9599310885968770357 ) ;
#76589 = DIRECTION ( 'NONE',  ( 0.000000000000000000, -1.000000000000000000, 0.000000000000000000 ) ) ;
#76590 = AXIS2_PLACEMENT_3D ( 'NONE', #76727, #9864, #35792 ) ;
#76591 = DIRECTION ( 'NONE',  ( -0.8191520442889975717, 0.000000000000000000, -0.5735764363510378328 ) ) ;
#76592 = SURFACE_STYLE_FILL_AREA ( #34590 ) ;
#76593 = AXIS2_PLACEMENT_3D ( 'NONE', #47173, #6724, #71993 ) ;
#76595 = LINE ( 'NONE', #26505, #4702 ) ;
#76594 = CARTESIAN_POINT ( 'NONE',  ( 7.996668422910687468, -3.000000000000002665, -91.14546720082027775 ) ) ;
#76596 = CARTESIAN_POINT ( 'NONE',  ( -83.25572694177012067, -39.48114288256212490, 172.2748129000959239 ) ) ;
#76597 = ORIENTED_EDGE ( 'NONE', *, *, #36297, .F. ) ;
#76598 = TOROIDAL_SURFACE ( 'NONE', #26691, 9.500000000000000000, 2.000000000000000000 ) ;
#76599 = CARTESIAN_POINT ( 'NONE',  ( -44.21332904831280075, 435.2494715644501753, 14.45449769377407101 ) ) ;
#76600 = ORIENTED_EDGE ( 'NONE', *, *, #2307, .T. ) ;
#76601 = CIRCLE ( 'NONE', #804, 15.00000000000000000 ) ;
#76602 = EDGE_LOOP ( 'NONE', ( #51871, #73031, #39455, #103020 ) ) ;
#76603 = DIRECTION ( 'NONE',  ( -1.000000000000000000, -1.224606353822377258E-16, -0.000000000000000000 ) ) ;
#76604 = ORIENTED_EDGE ( 'NONE', *, *, #54631, .F. ) ;
#76605 = DIRECTION ( 'NONE',  ( 1.000000000000000000, 1.224606353822377258E-16, 0.000000000000000000 ) ) ;
#76606 = CARTESIAN_POINT ( 'NONE',  ( -112.4702214903622490, -57.67117150189849895, 147.0458187677821797 ) ) ;
#76607 = CARTESIAN_POINT ( 'NONE',  ( 7.413471587080152858, -12.64352159168328171, -3.013058070223546991 ) ) ;
#76608 = CARTESIAN_POINT ( 'NONE',  ( 0.01688885742776732868, 7.321065037175427115, 3.319543390096037605 ) ) ;
#76609 = DIRECTION ( 'NONE',  ( 0.000000000000000000, -0.000000000000000000, 1.000000000000000000 ) ) ;
#76610 = CARTESIAN_POINT ( 'NONE',  ( 66.26095113931063452, -1.232595164407830946E-29, 4.000000000000007105 ) ) ;
#76611 = DIRECTION ( 'NONE',  ( -1.000000000000000000, -1.224606353822377258E-16, -0.000000000000000000 ) ) ;
#76612 = CARTESIAN_POINT ( 'NONE',  ( 107.3070812967312833, -60.00000000000004263, 109.8435067956896063 ) ) ;
#76613 = EDGE_CURVE ( 'NONE', #43945, #18398, #29120, .T. ) ;
#76614 = CARTESIAN_POINT ( 'NONE',  ( -71.28683113122063730, -60.00000000000007816, 168.6212938583825292 ) ) ;
#76615 = CARTESIAN_POINT ( 'NONE',  ( -59.37701284200993967, -46.44061691160312222, 73.85501160776004781 ) ) ;
#76616 = ORIENTED_EDGE ( 'NONE', *, *, #47791, .T. ) ;
#76617 = CARTESIAN_POINT ( 'NONE',  ( 6.561040333616081632, 16.17219201178938448, 2.450206053579249144 ) ) ;
#76618 = VERTEX_POINT ( 'NONE', #40072 ) ;
#76619 = CARTESIAN_POINT ( 'NONE',  ( -104.3760552791074616, -52.71020495745255374, 184.8450785601530981 ) ) ;
#76620 = CARTESIAN_POINT ( 'NONE',  ( -5.082755093536325042, -9.968750002048384573, -5.082755093536325930 ) ) ;
#76621 = CARTESIAN_POINT ( 'NONE',  ( 19.61638200451619696, 0.000000000000000000, 5.000000000000002665 ) ) ;
#76622 = CARTESIAN_POINT ( 'NONE',  ( 14.75116209840774850, 43.55504285524111907, -90.22050492864485705 ) ) ;
#76623 = VERTEX_POINT ( 'NONE', #625 ) ;
#76624 = CARTESIAN_POINT ( 'NONE',  ( 19.49614903793134246, 49.99973670987868957, 59.99522355992422007 ) ) ;
#76625 = CARTESIAN_POINT ( 'NONE',  ( -46.09484555436212361, -60.00000000000000000, 62.82384042436929406 ) ) ;
#76626 = CARTESIAN_POINT ( 'NONE',  ( -3.279721613087240417, -0.7058048543959732912, 103.5044187069696306 ) ) ;
#76627 = CARTESIAN_POINT ( 'NONE',  ( 2.977408999572651815, -12.31250000204838635, 7.188101187500000933 ) ) ;
#76628 = LINE ( 'NONE', #27607, #49910 ) ;
#76630 = ADVANCED_FACE ( 'NONE', ( #32541 ), #54912, .F. ) ;
#76629 = CARTESIAN_POINT ( 'NONE',  ( 6.936184427528457874, 0.000000000000000000, 0.000000000000000000 ) ) ;
#76631 = CIRCLE ( 'NONE', #35340, 4.000000000000003553 ) ;
#76632 = CARTESIAN_POINT ( 'NONE',  ( 2.083846472846741813E-15, -8.673617379884035472E-16, 17.01589776168603407 ) ) ;
#76633 = CARTESIAN_POINT ( 'NONE',  ( -12.22950890273588165, -4.580576956129855049, -12.66933385000461065 ) ) ;
#76634 = CARTESIAN_POINT ( 'NONE',  ( -6.837824896291514243, 3.947820044545419016, -6.564402953523714501 ) ) ;
#76635 = ADVANCED_FACE ( 'NONE', ( #16871 ), #8759, .T. ) ;
#76636 = PRESENTATION_STYLE_ASSIGNMENT (( #18435 ) ) ;
#76637 =( NAMED_UNIT ( * ) PLANE_ANGLE_UNIT ( ) SI_UNIT ( $, .RADIAN. ) );
#76638 = CARTESIAN_POINT ( 'NONE',  ( -7.500000000000006217, 31.97088361167177339, -52.67517300286423421 ) ) ;
#76639 = FACE_OUTER_BOUND ( 'NONE', #27819, .T. ) ;
#76640 = CARTESIAN_POINT ( 'NONE',  ( -29.80762567245044181, -53.38692201229141432, 35.51366752434432073 ) ) ;
#76641 = DIRECTION ( 'NONE',  ( 0.000000000000000000, -1.000000000000000000, 0.000000000000000000 ) ) ;
#76642 = CARTESIAN_POINT ( 'NONE',  ( 45.35554677126504686, -25.70144366515250312, 40.33168379963065320 ) ) ;
#76643 = DIRECTION ( 'NONE',  ( 0.000000000000000000, 1.000000000000000000, 0.000000000000000000 ) ) ;
#76644 = CARTESIAN_POINT ( 'NONE',  ( 6.750000000000017764, 11.69134295108991317, 0.000000000000000000 ) ) ;
#76645 = CARTESIAN_POINT ( 'NONE',  ( -97.66009619792869501, -38.48092223747977414, 201.0359958989743348 ) ) ;
#76646 = EDGE_LOOP ( 'NONE', ( #57041, #86911, #34213, #8334 ) ) ;
#76648 = DIRECTION ( 'NONE',  ( 1.000000000000000000, -0.000000000000000000, -0.000000000000000000 ) ) ;
#76647 = CARTESIAN_POINT ( 'NONE',  ( -9.500000000000003553, -5.000000000000000000, -68.91429205785459544 ) ) ;
#76649 = CARTESIAN_POINT ( 'NONE',  ( 80.86587616991319294, -60.00000000000004263, 181.8178842116407736 ) ) ;
#76650 = CARTESIAN_POINT ( 'NONE',  ( -19.19191325036121398, 49.76861282268819053, 61.57617224385840871 ) ) ;
#76651 = CARTESIAN_POINT ( 'NONE',  ( -7.303354903313936219, 41.37531411535626802, -59.25981086040365398 ) ) ;
#76652 = CARTESIAN_POINT ( 'NONE',  ( 5.209799036363110147, 40.00000000078713214, -70.92874456541859729 ) ) ;
#76653 = DIRECTION ( 'NONE',  ( -1.000000000000000000, -0.000000000000000000, -0.000000000000000000 ) ) ;
#76654 = CARTESIAN_POINT ( 'NONE',  ( -1.469576158976823947E-15, -18.87499999999999289, 8.000000000000000000 ) ) ;
#76655 = CARTESIAN_POINT ( 'NONE',  ( 18.09999999999999787, 3.309500000000003439, 0.000000000000000000 ) ) ;
#76656 = CARTESIAN_POINT ( 'NONE',  ( 112.2398407305392283, -59.99999999999999289, 172.8131785719580478 ) ) ;
#76657 = B_SPLINE_CURVE_WITH_KNOTS ( 'NONE', 3,
 ( #87518, #23321, #14127, #62712 ),
 .UNSPECIFIED., .F., .F.,
 ( 4, 4 ),
 ( 0.000000000000000000, 0.0007558628827966600407 ),
 .UNSPECIFIED. ) ;
#76658 = CARTESIAN_POINT ( 'NONE',  ( -17.49999999999999645, -2.499999999999999556, 25.00000000000000000 ) ) ;
#76659 = CARTESIAN_POINT ( 'NONE',  ( -7.743982712349853692, -68.46213014760736826, 2.020119794285911041 ) ) ;
#76660 = ORIENTED_EDGE ( 'NONE', *, *, #41026, .T. ) ;
#76661 = CARTESIAN_POINT ( 'NONE',  ( 1.509254614533404926, -49.97510739924324952, 101.6144273468640478 ) ) ;
#76662 = CARTESIAN_POINT ( 'NONE',  ( -78.22574516621017438, -30.00000000000003197, -15.67709204907202469 ) ) ;
#76663 = ORIENTED_EDGE ( 'NONE', *, *, #12497, .F. ) ;
#76665 = DIRECTION ( 'NONE',  ( -1.000000000000000000, -0.000000000000000000, -0.000000000000000000 ) ) ;
#76664 =( NAMED_UNIT ( * ) SI_UNIT ( $, .STERADIAN. ) SOLID_ANGLE_UNIT ( ) );
#76666 = CARTESIAN_POINT ( 'NONE',  ( 4.852941176470594975, -4.999999999999998224, -70.80672828634229177 ) ) ;
#76667 = CARTESIAN_POINT ( 'NONE',  ( 31.59878246649166300, 345.3114421961439007, 19.61614401236478145 ) ) ;
#76668 = CARTESIAN_POINT ( 'NONE',  ( 6.784953749580444615, 41.67963532863181797, -59.00226812211813154 ) ) ;
#76669 = CARTESIAN_POINT ( 'NONE',  ( -7.188101187500002709, -18.68750000204838102, 2.977408999572648707 ) ) ;
#76670 = VECTOR ( 'NONE', #71084, 1000.000000000000000 ) ;
#76671 = ADVANCED_FACE ( 'NONE', ( #91296 ), #18074, .F. ) ;
#76672 = CONICAL_SURFACE ( 'NONE', #59521, 5.000000000000000000, 0.9599310885968804774 ) ;
#76673 = AXIS2_PLACEMENT_3D ( 'NONE', #62764, #95657, #54630 ) ;
#76674 = AXIS2_PLACEMENT_3D ( 'NONE', #93340, #20026, #18954 ) ;
#76675 = CARTESIAN_POINT ( 'NONE',  ( 0.000000000000000000, 15.00000000000000000, 0.000000000000000000 ) ) ;
#76676 = PRESENTATION_LAYER_ASSIGNMENT (  '', '', ( #61222 ) ) ;
#76678 = ORIENTED_EDGE ( 'NONE', *, *, #50717, .T. ) ;
#76677 = FACE_OUTER_BOUND ( 'NONE', #11236, .T. ) ;
#76679 = CARTESIAN_POINT ( 'NONE',  ( 84.05649254118333147, -22.13809807529134588, 152.7230919644917435 ) ) ;
#76680 = CARTESIAN_POINT ( 'NONE',  ( -3.567967761888314548, -0.9297753284056393674, 103.4762329555118185 ) ) ;
#76681 = CIRCLE ( 'NONE', #47350, 5.000000000000001776 ) ;
#76682 = CARTESIAN_POINT ( 'NONE',  ( 9.948688207305194098, 88.87023149490184437, -1.044946705213433358 ) ) ;
#76683 = ORIENTED_EDGE ( 'NONE', *, *, #79954, .T. ) ;
#76684 = DIRECTION ( 'NONE',  ( -1.000000000000000000, -0.000000000000000000, -0.000000000000000000 ) ) ;
#76685 = DIRECTION ( 'NONE',  ( 0.000000000000000000, 1.000000000000000000, 0.000000000000000000 ) ) ;
#76686 = CARTESIAN_POINT ( 'NONE',  ( 38.81305289857993301, 27.34046816746474562, -12.01329072166396372 ) ) ;
#76687 = CARTESIAN_POINT ( 'NONE',  ( 69.18888888888888289, 3.309500000000014541, 0.000000000000000000 ) ) ;
#76688 = CARTESIAN_POINT ( 'NONE',  ( 24.34999999999999787, 3.309500000000003439, 4.052968581778167743E-16 ) ) ;
#76689 = CARTESIAN_POINT ( 'NONE',  ( 0.9531427616335313990, 13.93692614003196262, 51.31255756095965381 ) ) ;
#76690 = SURFACE_STYLE_FILL_AREA ( #51348 ) ;
#76691 = ORIENTED_EDGE ( 'NONE', *, *, #22998, .T. ) ;
#76692 = B_SPLINE_CURVE_WITH_KNOTS ( 'NONE', 3,
 ( #33937, #100749, #51132, #26916, #51669, #44669, #3672, #53798, #38189, #52736, #95870, #86201, #29568, #62968, #21997, #54849 ),
 .UNSPECIFIED., .F., .F.,
 ( 4, 2, 2, 2, 2, 2, 2, 4 ),
 ( 4.213851856174009611E-17, 0.0003803734300660355032, 0.0007607468601320289394, 0.001141120290198022105, 0.001521493720264015595, 0.001901867150330008869, 0.002282240580396002142, 0.003042987440528005169 ),
 .UNSPECIFIED. ) ;
#76693 = CARTESIAN_POINT ( 'NONE',  ( 0.000000000000000000, 0.000000000000000000, 0.000000000000000000 ) ) ;
#76694 = CYLINDRICAL_SURFACE ( 'NONE', #18550, 4.000000000000000000 ) ;
#76695 = CARTESIAN_POINT ( 'NONE',  ( 86.90659302068790737, -24.33240570756411714, 186.0895709266965525 ) ) ;
#76696 = DIRECTION ( 'NONE',  ( 0.000000000000000000, -1.000000000000000000, 0.000000000000000000 ) ) ;
#76697 = CARTESIAN_POINT ( 'NONE',  ( -7.188101187500002709, -22.81250000204838813, 2.977408999572648707 ) ) ;
#76698 = DIRECTION ( 'NONE',  ( 0.000000000000000000, 1.000000000000000000, 0.000000000000000000 ) ) ;
#76699 = CARTESIAN_POINT ( 'NONE',  ( 5.062272329166140672, -5.000000000000001776, 8.716576110310610304 ) ) ;
#76700 = EDGE_CURVE ( 'NONE', #106589, #98095, #79027, .T. ) ;
#76701 = DIRECTION ( 'NONE',  ( 0.000000000000000000, 1.000000000000000000, 0.000000000000000000 ) ) ;
#76702 = CONTEXT_DEPENDENT_SHAPE_REPRESENTATION ( #80326, #52663 ) ;
#76703 = ORIENTED_EDGE ( 'NONE', *, *, #18279, .T. ) ;
#76704 = CARTESIAN_POINT ( 'NONE',  ( 34.35000000000000142, 3.309500000000003439, 4.052968581778167743E-16 ) ) ;
#76705 = FILL_AREA_STYLE ('',( #85897 ) ) ;
#76706 = CARTESIAN_POINT ( 'NONE',  ( -10.11479301378070517, 7.336058586181116503, 0.000000000000000000 ) ) ;
#76707 = EDGE_CURVE ( 'NONE', #5701, #77653, #68733, .T. ) ;
#76708 = DIRECTION ( 'NONE',  ( -0.000000000000000000, 1.000000000000000000, 0.000000000000000000 ) ) ;
#76709 = ORIENTED_EDGE ( 'NONE', *, *, #58820, .T. ) ;
#76710 = FACE_BOUND ( 'NONE', #63524, .T. ) ;
#76711 = CARTESIAN_POINT ( 'NONE',  ( -33.33807306172103324, 464.2324349908527665, 17.97546588382418875 ) ) ;
#76712 = ORIENTED_EDGE ( 'NONE', *, *, #95248, .T. ) ;
#76713 = DIRECTION ( 'NONE',  ( 1.081159191512680572E-15, -0.07486943176528189359, 0.9971933454386585627 ) ) ;
#76714 = FACE_OUTER_BOUND ( 'NONE', #82738, .T. ) ;
#76715 = CARTESIAN_POINT ( 'NONE',  ( -17.94999111897422495, 36.38767359518977429, 23.42285042635046466 ) ) ;
#76716 = CARTESIAN_POINT ( 'NONE',  ( -108.5008973690249263, -60.00000000000000000, 194.7175470961265091 ) ) ;
#76717 = CARTESIAN_POINT ( 'NONE',  ( 1.714505518806294638E-15, -78.00000000000000000, 13.00000000000000000 ) ) ;
#76718 = CARTESIAN_POINT ( 'NONE',  ( 0.000000000000000000, 0.000000000000000000, -9.975036109638290682 ) ) ;
#76719 = CARTESIAN_POINT ( 'NONE',  ( 56.96666666666666856, 3.309500000000014541, 0.000000000000000000 ) ) ;
#76720 = CARTESIAN_POINT ( 'NONE',  ( -84.42943966653459142, -42.97677127786843698, 183.7511723405210660 ) ) ;
#76721 = AXIS2_PLACEMENT_3D ( 'NONE', #19720, #94095, #28880 ) ;
#76722 = EDGE_CURVE ( 'NONE', #3187, #94269, #47531, .T. ) ;
#76723 = CARTESIAN_POINT ( 'NONE',  ( -4.727426639335938319, 54.30178277073695625, -6.161806174029161198 ) ) ;
#76724 = VERTEX_POINT ( 'NONE', #85872 ) ;
#76725 = DIRECTION ( 'NONE',  ( 1.000000000000000000, 1.224606353822377258E-16, 0.000000000000000000 ) ) ;
#76727 = CARTESIAN_POINT ( 'NONE',  ( 0.000000000000000000, 0.000000000000000000, 0.000000000000000000 ) ) ;
#76726 = CIRCLE ( 'NONE', #54306, 4.000000000000000888 ) ;
#76728 = CARTESIAN_POINT ( 'NONE',  ( -86.70007003831202042, -60.15181208265720869, -0.3940414372618840644 ) ) ;
#76729 = FILL_AREA_STYLE ('',( #33645 ) ) ;
#76730 = CARTESIAN_POINT ( 'NONE',  ( -5.563220219054898941, 5.178627182129336148, -5.000000000000000000 ) ) ;
#76731 = AXIS2_PLACEMENT_3D ( 'NONE', #60234, #52101, #26289 ) ;
#76732 = AXIS2_PLACEMENT_3D ( 'NONE', #1812, #84353, #26679 ) ;
#76733 = CARTESIAN_POINT ( 'NONE',  ( -14.46338899916045406, -7.735849041625655786, 12.85468258354162963 ) ) ;
#76734 = CARTESIAN_POINT ( 'NONE',  ( 27.86843456301890853, 36.37502626979712517, -9.810812331909650297 ) ) ;
#76735 =( LENGTH_UNIT ( ) NAMED_UNIT ( * ) SI_UNIT ( .MILLI., .METRE. ) );
#76736 = CARTESIAN_POINT ( 'NONE',  ( 75.43375447319739635, -30.00000000000006395, 160.3035121353613306 ) ) ;
#76737 = CARTESIAN_POINT ( 'NONE',  ( -18.71440884245025060, 61.34242035161803841, 9.357204421225125301 ) ) ;
#76738 = CARTESIAN_POINT ( 'NONE',  ( -89.98348853342757536, -29.99999999999992184, -2.848863062743723695 ) ) ;
#76739 = CARTESIAN_POINT ( 'NONE',  ( -67.10393046265450323, -60.34011039881914940, 104.4197148593212745 ) ) ;
#76740 = ORIENTED_EDGE ( 'NONE', *, *, #36645, .F. ) ;
#76741 = CARTESIAN_POINT ( 'NONE',  ( 78.42589391212746364, -14.21045842199428222, 185.4806485215488010 ) ) ;
#76742 = CARTESIAN_POINT ( 'NONE',  ( 39.08472187170780643, 40.83956871101882058, 52.27844079319547177 ) ) ;
#76743 = CARTESIAN_POINT ( 'NONE',  ( 61.10636555069866205, -57.67115655538963637, -37.40363315934200727 ) ) ;
#76744 = AXIS2_PLACEMENT_3D ( 'NONE', #35838, #94034, #103716 ) ;
#76746 = ORIENTED_EDGE ( 'NONE', *, *, #106429, .F. ) ;
#76745 = AXIS2_PLACEMENT_3D ( 'NONE', #63508, #14385, #105017 ) ;
#76747 = CARTESIAN_POINT ( 'NONE',  ( 23.09999999999999432, 1.533819458162526451E-15, 0.000000000000000000 ) ) ;
#76749 = AXIS2_PLACEMENT_3D ( 'NONE', #45974, #71295, #39481 ) ;
#76748 = CARTESIAN_POINT ( 'NONE',  ( -7.188101187500002709, -27.68750000204838457, 2.977408999572647819 ) ) ;
#76750 = CARTESIAN_POINT ( 'NONE',  ( -1.101781001986523512, 27.52342745690481962, -40.11163141724147607 ) ) ;
#76751 = ORIENTED_EDGE ( 'NONE', *, *, #86111, .T. ) ;
#76752 = DIRECTION ( 'NONE',  ( -1.000000000000000000, -1.224606353822377258E-16, -0.000000000000000000 ) ) ;
#76753 = EDGE_LOOP ( 'NONE', ( #8275, #5544, #49440, #15904, #22114, #26020, #83180, #97468, #64100, #60846 ) ) ;
#76754 = CARTESIAN_POINT ( 'NONE',  ( 6.019162162300498053, 39.99999999999999289, -71.20548073448658499 ) ) ;
#76755 = CARTESIAN_POINT ( 'NONE',  ( 47.90297653514665654, 15.22282649863775283, -16.85535821593543560 ) ) ;
#76756 = CARTESIAN_POINT ( 'NONE',  ( -68.05622514284931412, -60.00000000002930278, 143.8904575097929524 ) ) ;
#76757 = CARTESIAN_POINT ( 'NONE',  ( -10.93254357274233435, 43.80611415629375927, 13.04138954228639236 ) ) ;
#76758 = CARTESIAN_POINT ( 'NONE',  ( -5.082755093536325042, -11.09375000204838457, -5.082755093536325930 ) ) ;
#76759 = CARTESIAN_POINT ( 'NONE',  ( -48.90230676976804602, 14.54998273526353358, 14.70096925929783716 ) ) ;
#76760 = AXIS2_PLACEMENT_3D ( 'NONE', #13136, #12605, #62783 ) ;
#76761 = FACE_OUTER_BOUND ( 'NONE', #24174, .T. ) ;
#76762 = DIRECTION ( 'NONE',  ( -0.000000000000000000, 1.000000000000000000, -0.000000000000000000 ) ) ;
#76763 = CARTESIAN_POINT ( 'NONE',  ( 11.99999999999999467, 50.00000000000000000, -86.57079632498522415 ) ) ;
#76764 = ADVANCED_FACE ( 'NONE', ( #51339 ), #13562, .T. ) ;
#76765 = CARTESIAN_POINT ( 'NONE',  ( 5.047120108843204278, -5.746297884371397657, -0.1007566405101845003 ) ) ;
#76766 = CARTESIAN_POINT ( 'NONE',  ( 39.99946440396829672, 437.0919103049818091, 5.547728658186661832 ) ) ;
#76767 = UNCERTAINTY_MEASURE_WITH_UNIT (LENGTH_MEASURE( 1.000000000000000082E-05 ), #12915, 'distance_accuracy_value', 'NONE');
#76768 = EDGE_LOOP ( 'NONE', ( #95375, #106494 ) ) ;
#76769 = CARTESIAN_POINT ( 'NONE',  ( 5.833333333391885311, -3.737948356782987869, 103.8776713793679107 ) ) ;
#76771 = CARTESIAN_POINT ( 'NONE',  ( 32.34925479044390073, -53.37185119530935395, 36.58498206500041050 ) ) ;
#76770 = CARTESIAN_POINT ( 'NONE',  ( 25.21823338009918203, 5.000000000000002665, 0.000000000000000000 ) ) ;
#76772 = CARTESIAN_POINT ( 'NONE',  ( -13.66642973271509831, 3.860411657743955287E-12, 17.78317311657911404 ) ) ;
#76773 = EDGE_CURVE ( 'NONE', #2627, #97763, #100957, .T. ) ;
#76774 = EDGE_LOOP ( 'NONE', ( #97592, #34994, #63952, #11098, #48473 ) ) ;
#76775 = CARTESIAN_POINT ( 'NONE',  ( -8.737863883542573262, 48.00000000000000711, -79.96381019629099285 ) ) ;
#76777 = CARTESIAN_POINT ( 'NONE',  ( 5.274401269815139237, 6.074457022762083547, -7.633824513837112136 ) ) ;
#76776 = CARTESIAN_POINT ( 'NONE',  ( -25.89532866215253648, 35.00241476997732093, -9.162145777036789340 ) ) ;
#76778 = DIRECTION ( 'NONE',  ( 0.000000000000000000, 1.000000000000000000, 0.000000000000000000 ) ) ;
#76779 = CARTESIAN_POINT ( 'NONE',  ( -43.35553785604018628, 484.2706869242194898, -0.02741892262543544484 ) ) ;
#76780 = CARTESIAN_POINT ( 'NONE',  ( -33.76105693399936314, 471.3091059247023509, 5.717665057388538585 ) ) ;
#76781 = CARTESIAN_POINT ( 'NONE',  ( 32.84088564781233543, 464.9638558180852215, 11.24476942535933155 ) ) ;
#76782 = VERTEX_POINT ( 'NONE', #69666 ) ;
#76783 = CARTESIAN_POINT ( 'NONE',  ( 91.87114596397952937, -59.99999999999999289, 10.38462266140972901 ) ) ;
#76784 = CARTESIAN_POINT ( 'NONE',  ( -11.27248856952037315, 45.76231435389451718, -13.37350896801532230 ) ) ;
#76785 =( NAMED_UNIT ( * ) SI_UNIT ( $, .STERADIAN. ) SOLID_ANGLE_UNIT ( ) );
#76786 = CARTESIAN_POINT ( 'NONE',  ( -35.53807395028670868, 391.2493183892675006, 6.679337639029564677 ) ) ;
#76787 = CARTESIAN_POINT ( 'NONE',  ( -6.565380407527345419, 40.29402549571846492, -71.20315154365353294 ) ) ;
#76788 = CARTESIAN_POINT ( 'NONE',  ( -46.83658167332212230, 18.87978240383743156, -15.22028160905640171 ) ) ;
#76789 = ORIENTED_EDGE ( 'NONE', *, *, #73121, .T. ) ;
#76790 = CARTESIAN_POINT ( 'NONE',  ( -82.19042405889051395, -29.99999999993295319, 194.5077282965602308 ) ) ;
#76791 = EDGE_LOOP ( 'NONE', ( #77791, #62430, #25047, #56997 ) ) ;
#76792 = DIRECTION ( 'NONE',  ( 0.000000000000000000, 0.000000000000000000, 1.000000000000000000 ) ) ;
#76793 = CARTESIAN_POINT ( 'NONE',  ( 6.445370176742030388, -7.262437273739259957, -1.101027156348882041 ) ) ;
#76794 = CARTESIAN_POINT ( 'NONE',  ( 7.894787914004607998, 1.238680740843649375E-13, -7.591390474663426424 ) ) ;
#76795 = CARTESIAN_POINT ( 'NONE',  ( 59.89460441624491693, 6.975173280561618775E-15, 0.000000000000000000 ) ) ;
#76796 = CARTESIAN_POINT ( 'NONE',  ( 83.64821297929979949, -45.27682201357416858, -13.05452488542865908 ) ) ;
#76797 = CARTESIAN_POINT ( 'NONE',  ( -38.86455081257312116, 307.2518422178578703, -7.111262733053415275 ) ) ;
#76798 = CARTESIAN_POINT ( 'NONE',  ( -3.416845212125001030, 304.8518027757642699, -9.000000000435770531 ) ) ;
#76799 = CARTESIAN_POINT ( 'NONE',  ( -17.83514733193546320, 45.00000000000000711, 62.69713390834871802 ) ) ;
#76800 = CARTESIAN_POINT ( 'NONE',  ( 9.953549941019165459, 46.18635266956800223, -12.94124874758495025 ) ) ;
#76801 = ORIENTED_EDGE ( 'NONE', *, *, #58055, .T. ) ;
#76802 = CARTESIAN_POINT ( 'NONE',  ( -6.499999999999999112, 1.392044006195858774, -6.058542048163744198 ) ) ;
#76803 = ORIENTED_EDGE ( 'NONE', *, *, #9617, .F. ) ;
#76804 = EDGE_CURVE ( 'NONE', #57410, #49495, #92330, .T. ) ;
#76805 = CARTESIAN_POINT ( 'NONE',  ( 56.22793774957824553, 6.975173280561618775E-15, 0.000000000000000000 ) ) ;
#76806 = DIRECTION ( 'NONE',  ( -1.000000000000000000, -0.000000000000000000, -0.000000000000000000 ) ) ;
#76808 = VERTEX_POINT ( 'NONE', #69150 ) ;
#76807 = CARTESIAN_POINT ( 'NONE',  ( 72.85555555555556850, -3.309500000000000774, 4.475777889183797681E-16 ) ) ;
#76809 = CARTESIAN_POINT ( 'NONE',  ( 77.86593331225071779, -18.66659222900301529, 117.1557179363761776 ) ) ;
#76810 = EDGE_CURVE ( 'NONE', #64587, #6669, #10111, .T. ) ;
#76811 = VERTEX_POINT ( 'NONE', #20099 ) ;
#76812 = CARTESIAN_POINT ( 'NONE',  ( 2.206083527337586947, -53.79085494686012225, 40.82659048662283396 ) ) ;
#76813 = LINE ( 'NONE', #75754, #57864 ) ;
#76814 = CARTESIAN_POINT ( 'NONE',  ( 7.188101187499999156, -26.75000000204838457, 2.977408999572654924 ) ) ;
#76815 = CARTESIAN_POINT ( 'NONE',  ( -71.68202686650683120, -57.67896093159416893, 168.8233993379761557 ) ) ;
#76816 = EDGE_CURVE ( 'NONE', #55657, #17355, #73854, .T. ) ;
#76817 = CIRCLE ( 'NONE', #97504, 4.000000000000007105 ) ;
#76818 = ORIENTED_EDGE ( 'NONE', *, *, #23728, .T. ) ;
#76819 = DIRECTION ( 'NONE',  ( 0.000000000000000000, -1.000000000000000000, 0.000000000000000000 ) ) ;
#76820 = CONICAL_SURFACE ( 'NONE', #44111, 5.000000000000010658, 0.9599310885968697082 ) ;
#76821 = CARTESIAN_POINT ( 'NONE',  ( 106.4724362242300231, -60.15149996984498415, 175.2116150193959925 ) ) ;
#76822 = CARTESIAN_POINT ( 'NONE',  ( 5.373223245032201945, 51.33044523536907633, -8.531152949374597227 ) ) ;
#76823 = FACE_OUTER_BOUND ( 'NONE', #28290, .T. ) ;
#76824 = CONICAL_SURFACE ( 'NONE', #95792, 6.499999999999999112, 1.047197551196600296 ) ;
#76825 = CARTESIAN_POINT ( 'NONE',  ( -8.000000000000001776, -16.34375000409677270, 3.313708498984758943 ) ) ;
#76826 = AXIS2_PLACEMENT_3D ( 'NONE', #38865, #64210, #71731 ) ;
#76827 = CARTESIAN_POINT ( 'NONE',  ( -50.11900266124489889, -29.71120325244069704, 46.80446231702884319 ) ) ;
#76828 = CIRCLE ( 'NONE', #90619, 4.000000000000007105 ) ;
#76829 = LINE ( 'NONE', #3487, #9481 ) ;
#76830 = AXIS2_PLACEMENT_3D ( 'NONE', #106444, #25034, #90814 ) ;
#76831 = DIRECTION ( 'NONE',  ( -1.000000000000000000, -0.000000000000000000, -0.000000000000000000 ) ) ;
#76832 = FACE_BOUND ( 'NONE', #64200, .T. ) ;
#76833 = CARTESIAN_POINT ( 'NONE',  ( 16.58291765283142993, 410.1183258646379386, 267.1969486012845891 ) ) ;
#76834 = FACE_OUTER_BOUND ( 'NONE', #88237, .T. ) ;
#76835 = VERTEX_POINT ( 'NONE', #10867 ) ;
#76836 = CARTESIAN_POINT ( 'NONE',  ( 44.21332904831252364, 435.2494715644490952, 14.45449769377161253 ) ) ;
#76837 = CARTESIAN_POINT ( 'NONE',  ( 11.06459909230147254, -4.984765618719626090, -12.57729599004233911 ) ) ;
#76838 = STYLED_ITEM ( 'NONE', ( #65966 ), #14500 ) ;
#76839 = CARTESIAN_POINT ( 'NONE',  ( 0.7798757358128801664, 8.372270557959069492, 51.48139209962896956 ) ) ;
#76840 = B_SPLINE_CURVE_WITH_KNOTS ( 'NONE', 3,
 ( #49309, #16428, #64983, #89798, #98921, #25080, #8331, #83814, #57938, #41235, #82758, #8860 ),
 .UNSPECIFIED., .F., .F.,
 ( 4, 2, 2, 2, 2, 4 ),
 ( 0.01037482654577543718, 0.01123049164366662390, 0.01208615674155781063, 0.01251398929050340399, 0.01294182183944899735, 0.01379748693734018233 ),
 .UNSPECIFIED. ) ;
#76841 = CARTESIAN_POINT ( 'NONE',  ( -84.86665315508184904, -30.00000000000000000, 169.0604416911780845 ) ) ;
#76842 = EDGE_CURVE ( 'NONE', #37991, #68633, #102563, .T. ) ;
#76843 = ORIENTED_EDGE ( 'NONE', *, *, #67120, .T. ) ;
#76844 = AXIS2_PLACEMENT_3D ( 'NONE', #30271, #48538, #63160 ) ;
#76845 = CARTESIAN_POINT ( 'NONE',  ( -8.480908980008681652, -4.333298119783866476, 15.78559285099031761 ) ) ;
#76846 = CARTESIAN_POINT ( 'NONE',  ( 81.23040402425959883, -57.51494128387065530, 199.9225175390093057 ) ) ;
#76847 = CARTESIAN_POINT ( 'NONE',  ( 44.19868099429156416, 435.2430970659377749, 14.45534906870892655 ) ) ;
#76848 = ADVANCED_FACE ( 'NONE', ( #68621 ), #73144, .T. ) ;
#76849 = CARTESIAN_POINT ( 'NONE',  ( 66.47564502340144088, -38.00297273520690311, -32.36529662817321196 ) ) ;
#76850 = CARTESIAN_POINT ( 'NONE',  ( 7.500000000000005329, -3.000000000000000000, -52.94236561372729000 ) ) ;
#76851 = CARTESIAN_POINT ( 'NONE',  ( -40.62042009610185289, 488.7249922674023992, 10.90475042733557309 ) ) ;
#76852 = PRODUCT_DEFINITION_SHAPE ( 'NONE', 'NONE',  #81205 ) ;
#76853 = CARTESIAN_POINT ( 'NONE',  ( -50.53461628407922035, -60.00000000000000000, 73.14908014348027621 ) ) ;
#76854 = CARTESIAN_POINT ( 'NONE',  ( -60.62677696746903422, 48.00000000000000000, 24.18439665018601303 ) ) ;
#76855 = CIRCLE ( 'NONE', #20100, 4.250000000000000000 ) ;
#76856 = CARTESIAN_POINT ( 'NONE',  ( -86.57471651473815655, -42.81671748233412700, 189.2810910813386158 ) ) ;
#76857 = VERTEX_POINT ( 'NONE', #46449 ) ;
#76858 = DIRECTION ( 'NONE',  ( -1.224646799147353454E-16, 0.000000000000000000, -1.000000000000000000 ) ) ;
#76859 = CARTESIAN_POINT ( 'NONE',  ( -1.000736805672570284, -35.99444417918818573, 29.88872398946706710 ) ) ;
#76860 = VECTOR ( 'NONE', #96141, 1000.000000000000000 ) ;
#76861 = CARTESIAN_POINT ( 'NONE',  ( -42.58368830533729721, 480.4992008869074311, 9.550881666320744756 ) ) ;
#76862 = CARTESIAN_POINT ( 'NONE',  ( -27.30328935667969859, 296.4063755745402204, 2.273684783268656417 ) ) ;
#76863 = ORIENTED_EDGE ( 'NONE', *, *, #14725, .F. ) ;
#76864 = CARTESIAN_POINT ( 'NONE',  ( -36.37334183242405317, 355.3971063992966037, 1.747594907370741524 ) ) ;
#76865 = FACE_OUTER_BOUND ( 'NONE', #10133, .T. ) ;
#76866 = CARTESIAN_POINT ( 'NONE',  ( -4.640047946013393876, -5.000000000000039968, -15.63625121056854184 ) ) ;
#76867 = CARTESIAN_POINT ( 'NONE',  ( 37.33349330513379982, -4.000000000000000000, 4.898587196589415787E-16 ) ) ;
#76868 = CARTESIAN_POINT ( 'NONE',  ( 24.99721807548662866, 295.6203948953991585, -1.835103857512845105 ) ) ;
#76869 = CARTESIAN_POINT ( 'NONE',  ( 20.24579557674108088, 304.8297271373347144, -10.00469232190996927 ) ) ;
#76870 = CARTESIAN_POINT ( 'NONE',  ( 15.59999999999999787, 1.533819458162526451E-15, 0.000000000000000000 ) ) ;
#76871 = CARTESIAN_POINT ( 'NONE',  ( 8.880941803279268854, 53.58345806519636056, -4.000118153562265633 ) ) ;
#76872 = CARTESIAN_POINT ( 'NONE',  ( 93.27827242126578255, -14.21045842199433729, 72.77868743038563082 ) ) ;
#76873 = CARTESIAN_POINT ( 'NONE',  ( -82.15122001469303825, -25.62513163106009983, 144.0135065024727510 ) ) ;
#76874 = EDGE_LOOP ( 'NONE', ( #90447, #79159 ) ) ;
#76875 = CARTESIAN_POINT ( 'NONE',  ( 36.84999999999999432, -3.309499999999999886, 4.475777889183790779E-16 ) ) ;
#76876 = CARTESIAN_POINT ( 'NONE',  ( 4.905194654929182718, 252.0239439501984009, 3.459476078998841242 ) ) ;
#76877 = CARTESIAN_POINT ( 'NONE',  ( 35.39667604442171012, -57.69563824998493118, 49.54500168928262127 ) ) ;
#76878 = APPLICATION_CONTEXT ( 'automotive_design' ) ;
#76879 = FACE_OUTER_BOUND ( 'NONE', #72369, .T. ) ;
#76880 = CARTESIAN_POINT ( 'NONE',  ( 44.48086712839104706, 338.5312796060234177, 0.5033553857222125005 ) ) ;
#76881 = CARTESIAN_POINT ( 'NONE',  ( 19.00000000000000711, 4.000000000000000888, -1.500000000000000444 ) ) ;
#76882 = ORIENTED_EDGE ( 'NONE', *, *, #75083, .T. ) ;
#76883 = CARTESIAN_POINT ( 'NONE',  ( 39.44615384615384812, 4.172000000000003261, 5.109226446042759579E-16 ) ) ;
#76884 = CARTESIAN_POINT ( 'NONE',  ( 31.38018240640768397, 439.2446336569565233, 22.99622140208172993 ) ) ;
#76885 = CARTESIAN_POINT ( 'NONE',  ( -1.320432766682874540E-15, -30.03125000204838813, 7.188101187500000044 ) ) ;
#76886 = ORIENTED_EDGE ( 'NONE', *, *, #76562, .T. ) ;
#76887 = SURFACE_STYLE_USAGE ( .BOTH. , #27335 ) ;
#76888 = DIRECTION ( 'NONE',  ( 0.000000000000000000, 0.000000000000000000, -1.000000000000000000 ) ) ;
#76889 = CARTESIAN_POINT ( 'NONE',  ( 6.602502617004377683, 41.80321047191768002, -70.07543148703942393 ) ) ;
#76890 = EDGE_CURVE ( 'NONE', #48389, #16756, #79338, .T. ) ;
#76891 = AXIS2_PLACEMENT_3D ( 'NONE', #7308, #32696, #72585 ) ;
#76892 = CARTESIAN_POINT ( 'NONE',  ( 5.774137037018601148, 50.00000000000000000, 63.00000000000000000 ) ) ;
#76893 = CARTESIAN_POINT ( 'NONE',  ( 22.57792046605466041, 6.123233995736770227E-16, -5.000000000000002665 ) ) ;
#76894 = B_SPLINE_CURVE_WITH_KNOTS ( 'NONE', 3,
 ( #76327, #20285, #93597, #53135 ),
 .UNSPECIFIED., .F., .F.,
 ( 4, 4 ),
 ( 0.000000000000000000, 1.000000000000000000 ),
 .UNSPECIFIED. ) ;
#76895 = DIRECTION ( 'NONE',  ( -1.000000000000000000, 0.000000000000000000, 0.000000000000000000 ) ) ;
#76896 = EDGE_LOOP ( 'NONE', ( #55612, #63833, #38842, #58269, #40563 ) ) ;
#76897 = CARTESIAN_POINT ( 'NONE',  ( 56.55061434549805455, -59.99999999999997868, -36.49602911317763443 ) ) ;
#76898 = AXIS2_PLACEMENT_3D ( 'NONE', #56002, #87886, #54415 ) ;
#76900 = CARTESIAN_POINT ( 'NONE',  ( 23.79183319049619172, -42.95491878026204091, 32.10493902695667856 ) ) ;
#76899 = CARTESIAN_POINT ( 'NONE',  ( -78.42710814205257464, -14.21045842199423070, 185.4825180806740548 ) ) ;
#76902 = CARTESIAN_POINT ( 'NONE',  ( 98.18081844100635180, 27.55047179872464724, -49.09040922050316880 ) ) ;
#76901 = PRODUCT_DEFINITION_CONTEXT ( 'detailed design', #45249, 'design' ) ;
#76903 = EDGE_CURVE ( 'NONE', #76395, #70292, #87665, .T. ) ;
#76904 = CARTESIAN_POINT ( 'NONE',  ( -37.87181877912480843, -56.81674967764890027, 40.67228283883505213 ) ) ;
#76905 = UNCERTAINTY_MEASURE_WITH_UNIT (LENGTH_MEASURE( 1.000000000000000082E-05 ), #98561, 'distance_accuracy_value', 'NONE');
#76906 =( GEOMETRIC_REPRESENTATION_CONTEXT ( 3 ) GLOBAL_UNCERTAINTY_ASSIGNED_CONTEXT ( ( #24797 ) ) GLOBAL_UNIT_ASSIGNED_CONTEXT ( ( #40714, #87698, #88225 ) ) REPRESENTATION_CONTEXT ( 'NONE', 'WORKASPACE' ) );
#76907 = ORIENTED_EDGE ( 'NONE', *, *, #797, .T. ) ;
#76908 = CARTESIAN_POINT ( 'NONE',  ( -15.38541618194247640, -4.285714285714296246, 20.05453516056600805 ) ) ;
#76909 = CARTESIAN_POINT ( 'NONE',  ( -43.77569424703144563, 434.3726356145336922, 11.96512969951308847 ) ) ;
#76910 = CARTESIAN_POINT ( 'NONE',  ( 14.29190075645216851, 12.99999999999999289, 0.000000000000000000 ) ) ;
#76911 = CIRCLE ( 'NONE', #33904, 13.50000000000000000 ) ;
#76912 = TOROIDAL_SURFACE ( 'NONE', #7991, 74.46152422706630603, 60.00000000000000000 ) ;
#76913 = CARTESIAN_POINT ( 'NONE',  ( 46.00000000000000000, 500.0000000000002274, 15.00000000000000711 ) ) ;
#76914 = CARTESIAN_POINT ( 'NONE',  ( 7.550180524134850302, -61.99440752786815523, 2.651855549982495397 ) ) ;
#76915 = CARTESIAN_POINT ( 'NONE',  ( -16.14595037866683924, 6.775806037745283561, 6.185188124841822344 ) ) ;
#76916 = ORIENTED_EDGE ( 'NONE', *, *, #54593, .T. ) ;
#76917 = CARTESIAN_POINT ( 'NONE',  ( -15.97435091970899812, 37.21084721865047129, -22.07459719473156312 ) ) ;
#76918 = VERTEX_POINT ( 'NONE', #53984 ) ;
#76919 = CARTESIAN_POINT ( 'NONE',  ( 96.80237214965333692, -29.99999999999995737, 129.0906176702744119 ) ) ;
#76920 = CARTESIAN_POINT ( 'NONE',  ( -12.51486567167142283, 5.260823752922433982, -8.146766300809140660 ) ) ;
#76921 = VECTOR ( 'NONE', #104153, 1000.000000000000000 ) ;
#76922 = CARTESIAN_POINT ( 'NONE',  ( -5.092539576892242792, -82.55676532791565592, 3.177249149099057313 ) ) ;
#76923 = CONICAL_SURFACE ( 'NONE', #70071, 4.172000000000009479, 0.9599310885968813656 ) ;
#76924 = CARTESIAN_POINT ( 'NONE',  ( 86.64224646343546965, -29.99999999999998934, 68.26920213384829594 ) ) ;
#76925 = CARTESIAN_POINT ( 'NONE',  ( -32.16765682584846786, 415.4409746963033854, 25.54514402344307555 ) ) ;
#76926 = ORIENTED_EDGE ( 'NONE', *, *, #14563, .F. ) ;
#76927 = EDGE_CURVE ( 'NONE', #31480, #83314, #79627, .T. ) ;
#76928 = ORIENTED_EDGE ( 'NONE', *, *, #102337, .T. ) ;
#76929 = VERTEX_POINT ( 'NONE', #55569 ) ;
#76930 = CYLINDRICAL_SURFACE ( 'NONE', #88769, 4.000000000000002665 ) ;
#76931 = CARTESIAN_POINT ( 'NONE',  ( -19.50000000000000000, 12.99999999999999289, 0.000000000000000000 ) ) ;
#76932 = CARTESIAN_POINT ( 'NONE',  ( 0.000000000000000000, 6.123233995736770227E-16, -5.000000000000002665 ) ) ;
#76933 = CARTESIAN_POINT ( 'NONE',  ( 38.45073040354913729, 439.3073909824421435, 23.72287809797798630 ) ) ;
#76934 = CARTESIAN_POINT ( 'NONE',  ( -31.42031127665597623, 438.9001181076657758, 23.11845042760961988 ) ) ;
#76935 = CARTESIAN_POINT ( 'NONE',  ( 55.26095113931063452, 6.856755485862130937E-15, 0.000000000000000000 ) ) ;
#76936 = ORIENTED_EDGE ( 'NONE', *, *, #93217, .T. ) ;
#76937 = CARTESIAN_POINT ( 'NONE',  ( 1.308996937483428491, 49.99999999999999289, -95.00000000000001421 ) ) ;
#76938 = ORIENTED_EDGE ( 'NONE', *, *, #73666, .F. ) ;
#76939 = CARTESIAN_POINT ( 'NONE',  ( -5.191144708981716427, -62.35969914478732079, 3.015512395308852067 ) ) ;
#76940 = CARTESIAN_POINT ( 'NONE',  ( 71.08629748639575041, -38.32842814543181476, 140.5624642575193661 ) ) ;
#76941 = DIRECTION ( 'NONE',  ( 1.000000000000000000, 1.224606353822377258E-16, 0.000000000000000000 ) ) ;
#76942 = CARTESIAN_POINT ( 'NONE',  ( 21.31062199470357044, 303.0145930226796622, 9.972157899344148646 ) ) ;
#76943 = CIRCLE ( 'NONE', #82087, 5.000000000000010658 ) ;
#76944 = CARTESIAN_POINT ( 'NONE',  ( -4.472135954999578722, 249.9999999999999432, -4.000000000000002665 ) ) ;
#76945 = ORIENTED_EDGE ( 'NONE', *, *, #93514, .F. ) ;
#76946 = CARTESIAN_POINT ( 'NONE',  ( 1.262844703064978993E-15, -3.000000000000002665, -95.00000000000000000 ) ) ;
#76947 = CIRCLE ( 'NONE', #40750, 4.250000000000000000 ) ;
#76948 = FACE_OUTER_BOUND ( 'NONE', #65448, .T. ) ;
#76949 = CARTESIAN_POINT ( 'NONE',  ( 32.43844611059790850, 299.9187617745382113, 3.072456096697431693 ) ) ;
#76950 = CARTESIAN_POINT ( 'NONE',  ( 37.06438722625302518, 5.000000000000002665, 0.000000000000000000 ) ) ;
#76951 = ADVANCED_FACE ( 'NONE', ( #14583 ), #8409, .F. ) ;
#76952 = VERTEX_POINT ( 'NONE', #29249 ) ;
#76953 = CARTESIAN_POINT ( 'NONE',  ( 6.928203230275508773, -85.00000000000000000, 4.000000000000001776 ) ) ;
#76954 = SURFACE_SIDE_STYLE ('',( #103369 ) ) ;
#76955 = CARTESIAN_POINT ( 'NONE',  ( -0.3875187462267188354, -8.436519985397220367, -7.781689322728342795 ) ) ;
#76956 = CARTESIAN_POINT ( 'NONE',  ( 4.061773079301143952, 294.8078983759118614, 9.927667266017472514 ) ) ;
#76957 = CARTESIAN_POINT ( 'NONE',  ( 0.000000000000000000, 0.000000000000000000, 0.000000000000000000 ) ) ;
#76958 = B_SPLINE_CURVE_WITH_KNOTS ( 'NONE', 3,
 ( #11549, #44477, #68211, #45545, #77368, #95155, #78417, #102167, #4010, #86016, #2402, #3484, #36424, #53094, #77902, #43412, #36940, #4536, #37478, #62270, #87066, #101108, #27268, #60153, #93017, #89176, #63850, #105873, #14732, #80005 ),
 .UNSPECIFIED., .F., .F.,
 ( 4, 2, 2, 2, 2, 2, 2, 2, 2, 2, 2, 2, 2, 2, 4 ),
 ( 0.01036701337735199818, 0.01128271447498712179, 0.01219841557262224367, 0.01311411667025736728, 0.01357196721907492735, 0.01402981776789248743, 0.01448766831671004750, 0.01471659359111883100, 0.01494551886552761451, 0.01517444413993639801, 0.01540336941434517978, 0.01586121996316274332, 0.01631907051198030686, 0.01677692106079787041, 0.01769262215843298361 ),
 .UNSPECIFIED. ) ;
#76959 = CARTESIAN_POINT ( 'NONE',  ( 6.781345014477444977, 3.590342129888846046, -6.122077150241850063 ) ) ;
#76960 = CARTESIAN_POINT ( 'NONE',  ( 85.99589102735485824, -35.58585133369340525, 185.3973540908802988 ) ) ;
#76961 = CARTESIAN_POINT ( 'NONE',  ( 17.96008057617807196, 36.59330496951920964, -22.69888471349237946 ) ) ;
#76962 = CIRCLE ( 'NONE', #23638, 0.9999999999999991118 ) ;
#76963 = CARTESIAN_POINT ( 'NONE',  ( -9.061657590037185628, 137.7585088365954107, -1.734723475898753647E-15 ) ) ;
#76964 = ORIENTED_EDGE ( 'NONE', *, *, #86147, .F. ) ;
#76965 = CARTESIAN_POINT ( 'NONE',  ( 53.00244648738614472, -57.67085655565274749, -39.32701979258551006 ) ) ;
#76966 = CARTESIAN_POINT ( 'NONE',  ( -1.058054217398702423, 6.894685612232783534, -0.3576316571898418006 ) ) ;
#76967 = CARTESIAN_POINT ( 'NONE',  ( 35.22510507712048167, 436.7812103362905987, 6.088528189192170537 ) ) ;
#76968 =( BOUNDED_SURFACE ( )  B_SPLINE_SURFACE ( 3, 2, ( 
 ( #90870, #34789, #60123 ),
 ( #35317, #49862, #10988 ),
 ( #43905, #1832, #83823 ),
 ( #51985, #83296, #50913 ),
 ( #99466, #92987, #76793 ),
 ( #92439, #51457, #26178 ) ),
 .UNSPECIFIED., .F., .F., .F. ) 
 B_SPLINE_SURFACE_WITH_KNOTS ( ( 4, 2, 4 ),
 ( 3, 3 ),
 ( 0.003199762745116010217, 0.007302762474435760612, 0.01140576220375551057 ),
 ( 0.000000000000000000, 1.000000000000000000 ),
 .UNSPECIFIED. ) 
 GEOMETRIC_REPRESENTATION_ITEM ( )  RATIONAL_B_SPLINE_SURFACE ( (
 ( 1.000000000000000000, 0.8047731410850426093, 1.000000000000000000),
 ( 1.000000000000000000, 0.8125552299153950830, 1.000000000000000000),
 ( 1.000000000000000000, 0.8191520442892971099, 1.000000000000000000),
 ( 1.000000000000000000, 0.8191520442886824904, 1.000000000000000000),
 ( 1.000000000000000000, 0.8125552299158561587, 1.000000000000000000),
 ( 1.000000000000000000, 0.8047731410850428313, 1.000000000000000000) ) ) 
 REPRESENTATION_ITEM ( '' )  SURFACE ( )  );
#76969 = CARTESIAN_POINT ( 'NONE',  ( -89.54384241208562401, -30.00000000000000355, 85.81002042860349377 ) ) ;
#76970 = EDGE_CURVE ( 'NONE', #67283, #74698, #103618, .T. ) ;
#76971 =( GEOMETRIC_REPRESENTATION_CONTEXT ( 3 ) GLOBAL_UNCERTAINTY_ASSIGNED_CONTEXT ( ( #86095 ) ) GLOBAL_UNIT_ASSIGNED_CONTEXT ( ( #79374, #104176, #103655 ) ) REPRESENTATION_CONTEXT ( 'NONE', 'WORKASPACE' ) );
#76972 = CARTESIAN_POINT ( 'NONE',  ( 0.000000000000000000, -30.00000000000000000, 0.000000000000000000 ) ) ;
#76973 = CARTESIAN_POINT ( 'NONE',  ( 0.03252858621208985779, -57.67120202567194553, 41.61186624302497705 ) ) ;
#76974 = EDGE_CURVE ( 'NONE', #17242, #104368, #22922, .T. ) ;
#76976 = CARTESIAN_POINT ( 'NONE',  ( 35.58361799548379167, 1.482358050883964840E-15, 0.000000000000000000 ) ) ;
#76975 = CARTESIAN_POINT ( 'NONE',  ( -9.798380800342682662, 246.5319934568448730, -2.010350564680316143 ) ) ;
#76977 = EDGE_CURVE ( 'NONE', #86973, #82907, #41152, .T. ) ;
#76978 = DIRECTION ( 'NONE',  ( 0.000000000000000000, 1.000000000000000000, 0.000000000000000000 ) ) ;
#76979 = CARTESIAN_POINT ( 'NONE',  ( -26.51146395532327205, -28.75509375596147166, 30.19052060091659229 ) ) ;
#76980 = CARTESIAN_POINT ( 'NONE',  ( -35.97836163551201594, 491.7764920885232414, 12.54497382757487323 ) ) ;
#76981 =( NAMED_UNIT ( * ) SI_UNIT ( $, .STERADIAN. ) SOLID_ANGLE_UNIT ( ) );
#76982 = DIRECTION ( 'NONE',  ( 0.000000000000000000, 0.000000000000000000, 1.000000000000000000 ) ) ;
#76983 = COLOUR_RGB ( '', 0.31764706, 0.68627451, 0.89019608) ;
#76984 = AXIS2_PLACEMENT_3D ( 'NONE', #32161, #88273, #80683 ) ;
#76985 = EDGE_CURVE ( 'NONE', #79406, #337, #47336, .T. ) ;
#76986 = CARTESIAN_POINT ( 'NONE',  ( 64.09672519251849110, -29.67724580561281300, -23.43488640169166715 ) ) ;
#76987 = CARTESIAN_POINT ( 'NONE',  ( -23.57229190052912315, -35.99927206564916560, 30.88733768663876589 ) ) ;
#76988 = STYLED_ITEM ( 'NONE', ( #29444 ), #4960 ) ;
#76989 = EDGE_CURVE ( 'NONE', #58522, #16331, #105727, .T. ) ;
#76990 = EDGE_LOOP ( 'NONE', ( #1265, #57540, #91987, #62583 ) ) ;
#76991 = CARTESIAN_POINT ( 'NONE',  ( 42.19179521601819260, 485.4956273777428919, -3.824025998174083618 ) ) ;
#76992 = CARTESIAN_POINT ( 'NONE',  ( -9.165151389911679658, 105.0000000000000000, 4.000000000000001776 ) ) ;
#76993 = CONICAL_SURFACE ( 'NONE', #27072, 3.309500000000007880, 0.9599310885968770357 ) ;
#76994 = CARTESIAN_POINT ( 'NONE',  ( -18.63541348317560420, -22.07126658726433988, 27.94047467926784023 ) ) ;
#76996 = CARTESIAN_POINT ( 'NONE',  ( 0.7834951455711054447, 37.11066583794674756, -27.51244135688735071 ) ) ;
#76995 = DIRECTION ( 'NONE',  ( 0.000000000000000000, 0.000000000000000000, 1.000000000000000000 ) ) ;
#76997 = VERTEX_POINT ( 'NONE', #73350 ) ;
#76998 = DIRECTION ( 'NONE',  ( -1.000000000000000000, -1.224606353822377258E-16, -0.000000000000000000 ) ) ;
#76999 = ORIENTED_EDGE ( 'NONE', *, *, #97368, .F. ) ;
#77000 = CYLINDRICAL_SURFACE ( 'NONE', #75725, 1.250000000000001110 ) ;
#77001 = DIRECTION ( 'NONE',  ( -1.000000000000000000, -1.224606353822377258E-16, -0.000000000000000000 ) ) ;
#77002 = FACE_OUTER_BOUND ( 'NONE', #69073, .T. ) ;
#77003 = EDGE_LOOP ( 'NONE', ( #49425, #13451, #44237 ) ) ;
#77004 = LINE ( 'NONE', #3121, #575 ) ;
#77005 = CARTESIAN_POINT ( 'NONE',  ( 104.9449258806604064, -60.15148239079525183, 188.0245670500678443 ) ) ;
#77007 = DIRECTION ( 'NONE',  ( 0.000000000000000000, -1.000000000000000000, 0.000000000000000000 ) ) ;
#77006 = SURFACE_STYLE_FILL_AREA ( #54841 ) ;
#77008 = AXIS2_PLACEMENT_3D ( 'NONE', #85814, #19512, #43732 ) ;
#77009 = ORIENTED_EDGE ( 'NONE', *, *, #64563, .T. ) ;
#77010 = ORIENTED_EDGE ( 'NONE', *, *, #42092, .T. ) ;
#77011 = STYLED_ITEM ( 'NONE', ( #77884 ), #101792 ) ;
#77012 = ORIENTED_EDGE ( 'NONE', *, *, #40929, .T. ) ;
#77013 = CARTESIAN_POINT ( 'NONE',  ( 22.98868130639473861, 305.6447374718524657, 9.109369938318858217 ) ) ;
#77014 = CARTESIAN_POINT ( 'NONE',  ( 0.000000000000000000, 0.000000000000000000, 0.000000000000000000 ) ) ;
#77015 = SURFACE_STYLE_USAGE ( .BOTH. , #21468 ) ;
#77016 = ORIENTED_EDGE ( 'NONE', *, *, #20361, .F. ) ;
#77017 = EDGE_CURVE ( 'NONE', #84046, #15159, #58393, .T. ) ;
#77018 = DIRECTION ( 'NONE',  ( -1.000000000000000000, 0.000000000000000000, 0.000000000000000000 ) ) ;
#77019 = CARTESIAN_POINT ( 'NONE',  ( -4.966176470918028052, 41.64999999999999147, -70.47555194646973575 ) ) ;
#77020 =( LENGTH_UNIT ( ) NAMED_UNIT ( * ) SI_UNIT ( .MILLI., .METRE. ) );
#77021 = CARTESIAN_POINT ( 'NONE',  ( -39.20652242405842713, -59.99999999998065903, -42.13619399682325906 ) ) ;
#77022 = DIRECTION ( 'NONE',  ( 0.000000000000000000, 0.000000000000000000, 1.000000000000000000 ) ) ;
#77023 = CARTESIAN_POINT ( 'NONE',  ( -34.06332199976886699, 330.0526646846329299, -3.810096259360388427 ) ) ;
#77024 = CARTESIAN_POINT ( 'NONE',  ( 97.15356149169568312, 1.016364837396684119E-14, 0.000000000000000000 ) ) ;
#77025 = CARTESIAN_POINT ( 'NONE',  ( -94.49493096136262693, -59.99999999999997158, -13.89135613746328701 ) ) ;
#77026 = EDGE_CURVE ( 'NONE', #45089, #70572, #24012, .T. ) ;
#77028 = EDGE_CURVE ( 'NONE', #11109, #5281, #44893, .T. ) ;
#77027 = CARTESIAN_POINT ( 'NONE',  ( -8.559508646656370345, 51.55638410492942114, 4.031152949374564365 ) ) ;
#77029 = MECHANICAL_DESIGN_GEOMETRIC_PRESENTATION_REPRESENTATION (  '', ( #49691 ), #56531 ) ;
#77030 = CARTESIAN_POINT ( 'NONE',  ( -47.84767795939104218, -60.28261157666721459, 53.82599118737805810 ) ) ;
#77031 = ORIENTED_EDGE ( 'NONE', *, *, #18904, .F. ) ;
#77032 = CARTESIAN_POINT ( 'NONE',  ( 5.000000000000000888, 0.000000000000000000, -25.03750572909317285 ) ) ;
#77033 = ORIENTED_EDGE ( 'NONE', *, *, #57378, .T. ) ;
#77034 = LINE ( 'NONE', #67363, #106299 ) ;
#77035 = STYLED_ITEM ( 'NONE', ( #69961 ), #7331 ) ;
#77036 = CARTESIAN_POINT ( 'NONE',  ( -9.148737761767405274, 294.6669993733668775, -4.042064116724770173 ) ) ;
#77037 = EDGE_CURVE ( 'NONE', #37114, #42466, #98171, .T. ) ;
#77038 = CARTESIAN_POINT ( 'NONE',  ( 4.813555570991616683, -8.205262034826786177, -3.584128953194781975 ) ) ;
#77039 = ORIENTED_EDGE ( 'NONE', *, *, #68361, .T. ) ;
#77040 = DIRECTION ( 'NONE',  ( -1.000000000000000000, -1.224606353822377258E-16, -0.000000000000000000 ) ) ;
#77041 = CARTESIAN_POINT ( 'NONE',  ( 82.23984288647631047, -30.00000000000165912, -23.31778023025261248 ) ) ;
#77042 = FACE_OUTER_BOUND ( 'NONE', #91999, .T. ) ;
#77043 = CARTESIAN_POINT ( 'NONE',  ( 3.352941176470587425, -48.79941684889505638, 104.5794940929807382 ) ) ;
#77044 = CARTESIAN_POINT ( 'NONE',  ( 6.690415142086856726, 41.73276191905608812, -59.04972836783017698 ) ) ;
#77045 = CARTESIAN_POINT ( 'NONE',  ( 23.57730434123481800, 18.64316884710268596, -30.67950393663962672 ) ) ;
#77046 = CARTESIAN_POINT ( 'NONE',  ( 88.94591903970945168, -30.00000000000000000, 188.6279831367985764 ) ) ;
#77047 = CARTESIAN_POINT ( 'NONE',  ( -11.38829015755950635, 43.21651619172995851, -14.75358294640981249 ) ) ;
#77048 = CARTESIAN_POINT ( 'NONE',  ( -0.3379147738798968792, 37.19680971541975367, 27.28503007046158402 ) ) ;
#77049 = EDGE_CURVE ( 'NONE', #49442, #99488, #27487, .T. ) ;
#77050 = ORIENTED_EDGE ( 'NONE', *, *, #56319, .T. ) ;
#77051 = ORIENTED_EDGE ( 'NONE', *, *, #101780, .F. ) ;
#77052 = CARTESIAN_POINT ( 'NONE',  ( 53.32874875972302675, -53.37299379156652890, 62.19724302110672198 ) ) ;
#77053 = CARTESIAN_POINT ( 'NONE',  ( 89.99999999999997158, 500000.0000000000582, 188.5238439516623146 ) ) ;
#77054 = CARTESIAN_POINT ( 'NONE',  ( -43.27801297234302780, 485.1608390498441850, -2.258185464243190221 ) ) ;
#77055 = ADVANCED_FACE ( 'NONE', ( #73893 ), #28481, .F. ) ;
#77056 = VERTEX_POINT ( 'NONE', #15130 ) ;
#77057 = CARTESIAN_POINT ( 'NONE',  ( -88.31393190425067985, -38.37506173642456275, -19.13771254034035607 ) ) ;
#77058 = VERTEX_POINT ( 'NONE', #17804 ) ;
#77059 = DIRECTION ( 'NONE',  ( -0.3900125511322734551, -0.5465874153436415250, -0.7410346870067915370 ) ) ;
#77060 = CARTESIAN_POINT ( 'NONE',  ( 110.2492766163225184, -38.35601179711003539, 184.3364095030646865 ) ) ;
#77061 = CARTESIAN_POINT ( 'NONE',  ( 12.35017993402607317, 20.41240526430823365, 6.749814137266258562 ) ) ;
#77063 = CARTESIAN_POINT ( 'NONE',  ( 86.38361104131109869, -60.13166636963751444, 4.011411551973763423 ) ) ;
#77062 = STYLED_ITEM ( 'NONE', ( #55182 ), #24546 ) ;
#77064 = CIRCLE ( 'NONE', #30515, 5.000000000000002665 ) ;
#77065 = CARTESIAN_POINT ( 'NONE',  ( 39.95479119095725906, 335.6566949496817642, 19.74082504813667782 ) ) ;
#77067 = AXIS2_PLACEMENT_3D ( 'NONE', #53032, #93504, #2336 ) ;
#77066 = CARTESIAN_POINT ( 'NONE',  ( 27.02022815836235026, 1.340359594676612611E-15, 0.000000000000000000 ) ) ;
#77068 = CARTESIAN_POINT ( 'NONE',  ( 2.374770270499908964, -6.910312371746204718, -13.35351085777521085 ) ) ;
#77069 = CIRCLE ( 'NONE', #30593, 4.000000000000001776 ) ;
#77070 = CARTESIAN_POINT ( 'NONE',  ( 26.08349330513380337, -7.703719777548943412E-31, 4.000000000000001776 ) ) ;
#77071 = CARTESIAN_POINT ( 'NONE',  ( 8.441132293785154062, 123.9914807902427327, -1.229386795015411088E-12 ) ) ;
#77072 = TOROIDAL_SURFACE ( 'NONE', #3004, 17.00000000000000000, 2.000000000000000000 ) ;
#77073 = ORIENTED_EDGE ( 'NONE', *, *, #50111, .F. ) ;
#77074 = CARTESIAN_POINT ( 'NONE',  ( -9.090909090909093493, 16.00000000000000000, -4.165977904505304252 ) ) ;
#77075 = CARTESIAN_POINT ( 'NONE',  ( 7.493977565380718353, 40.56334570848421350, -69.29067317619599464 ) ) ;
#77076 = CARTESIAN_POINT ( 'NONE',  ( -32.15310320217081852, 439.7024266304582625, 23.94087012106557566 ) ) ;
#77077 = EDGE_LOOP ( 'NONE', ( #35682, #32406, #42933, #23490 ) ) ;
#77078 = DIRECTION ( 'NONE',  ( 1.000000000000000000, 0.000000000000000000, 0.000000000000000000 ) ) ;
#77079 = CARTESIAN_POINT ( 'NONE',  ( -38.42297841453999752, 318.8661547594436456, 15.79363851032234045 ) ) ;
#77080 = DIRECTION ( 'NONE',  ( 0.000000000000000000, 0.000000000000000000, -1.000000000000000000 ) ) ;
#77081 = DIRECTION ( 'NONE',  ( -1.000000000000000000, -1.224606353822377258E-16, -0.000000000000000000 ) ) ;
#77082 = CARTESIAN_POINT ( 'NONE',  ( -3.313708498984765161, -23.46875000000000000, 7.999999999999998224 ) ) ;
#77083 = CARTESIAN_POINT ( 'NONE',  ( -16.93153427181588100, -15.84522097637744409, 31.52956385905993031 ) ) ;
#77084 = AXIS2_PLACEMENT_3D ( 'NONE', #53588, #78388, #4505 ) ;
#77085 = CARTESIAN_POINT ( 'NONE',  ( 0.000000000000000000, 0.000000000000000000, 1.734723475976807094E-15 ) ) ;
#77086 = ORIENTED_EDGE ( 'NONE', *, *, #7797, .F. ) ;
#77087 = CARTESIAN_POINT ( 'NONE',  ( 86.38910116964329688, -17.91566640048721482, 174.1185442106061032 ) ) ;
#77089 = CONICAL_SURFACE ( 'NONE', #22065, 3.400000000000000355, 0.9599310885968748153 ) ;
#77088 = PRESENTATION_STYLE_ASSIGNMENT (( #68481 ) ) ;
#77090 = CARTESIAN_POINT ( 'NONE',  ( -15.43446081147251014, 46.13172121994918484, 5.765148793919729897 ) ) ;
#77091 = VERTEX_POINT ( 'NONE', #36148 ) ;
#77092 = CARTESIAN_POINT ( 'NONE',  ( -93.17158877072618850, -37.82072235447289899, 97.15439343368484515 ) ) ;
#77093 = DIRECTION ( 'NONE',  ( 1.224646799147349509E-16, 0.000000000000000000, -1.000000000000000000 ) ) ;
#77094 = DIRECTION ( 'NONE',  ( 1.000000000000000000, 0.000000000000000000, -0.000000000000000000 ) ) ;
#77095 = CARTESIAN_POINT ( 'NONE',  ( 14.92100282753648344, -3.000000000000003109, -82.95543583085692774 ) ) ;
#77096 = VECTOR ( 'NONE', #28929, 1000.000000000000000 ) ;
#77097 = CARTESIAN_POINT ( 'NONE',  ( -27.77832180966715114, -28.75187696444542595, -38.27432471080516052 ) ) ;
#77098 = EDGE_CURVE ( 'NONE', #16922, #21366, #53316, .T. ) ;
#77099 = B_SPLINE_CURVE_WITH_KNOTS ( 'NONE', 3,
 ( #75533, #100868, #92780, #33503, #43700, #17320, #2703, #35651, #82567, #101419, #57737, #8671 ),
 .UNSPECIFIED., .F., .F.,
 ( 4, 2, 2, 2, 2, 4 ),
 ( 5.282959581270353437E-15, 0.001731416251740865511, 0.003462832503476448356, 0.004328540629344262980, 0.005194248755212077170, 0.006925665006947724633 ),
 .UNSPECIFIED. ) ;
#77100 = CARTESIAN_POINT ( 'NONE',  ( 36.36503303793942621, -59.99999999999998579, 47.71482123089194261 ) ) ;
#77101 = CARTESIAN_POINT ( 'NONE',  ( 30.26725086609628335, -32.62914588997867327, 40.72554252228815130 ) ) ;
#77102 = FILL_AREA_STYLE ('',( #12883 ) ) ;
#77103 = CARTESIAN_POINT ( 'NONE',  ( 34.89228459837880791, -24.01504711961399607, 33.45256225496395786 ) ) ;
#77104 = ADVANCED_FACE ( 'NONE', ( #28051 ), #37796, .T. ) ;
#77105 = ADVANCED_FACE ( 'NONE', ( #11809 ), #42589, .T. ) ;
#77106 = AXIS2_PLACEMENT_3D ( 'NONE', #34629, #1123, #91253 ) ;
#77108 = CARTESIAN_POINT ( 'NONE',  ( -14.71476209775949151, 21.86062043620323436, 4.643882332649849509 ) ) ;
#77107 = CARTESIAN_POINT ( 'NONE',  ( 34.25382146508943748, 436.5998831423237334, 6.438976971928319415 ) ) ;
#77109 = ADVANCED_FACE ( 'NONE', ( #1583 ), #18857, .T. ) ;
#77110 = CARTESIAN_POINT ( 'NONE',  ( 5.645355559246219457, 301.6283892719084179, -10.01771515668981039 ) ) ;
#77111 = CARTESIAN_POINT ( 'NONE',  ( 71.17283260602091843, -38.00000000000000000, -21.88484610531455488 ) ) ;
#77112 = CARTESIAN_POINT ( 'NONE',  ( 43.66598739136852458, 384.2106680610543208, 15.34735960979999980 ) ) ;
#77113 = ORIENTED_EDGE ( 'NONE', *, *, #103584, .T. ) ;
#77114 = DIRECTION ( 'NONE',  ( 0.000000000000000000, 0.000000000000000000, 1.000000000000000000 ) ) ;
#77115 = CARTESIAN_POINT ( 'NONE',  ( -17.49999999999991473, 51.99998113221733576, 59.93765433267815013 ) ) ;
#77116 = EDGE_CURVE ( 'NONE', #59152, #43534, #79097, .T. ) ;
#77117 = ORIENTED_EDGE ( 'NONE', *, *, #13590, .T. ) ;
#77118 = PRESENTATION_STYLE_ASSIGNMENT (( #35636 ) ) ;
#77119 = LINE ( 'NONE', #69570, #95323 ) ;
#77120 = CARTESIAN_POINT ( 'NONE',  ( 5.999511540169427448, -61.00073269114566443, -0.2833228702578399760 ) ) ;
#77122 = CARTESIAN_POINT ( 'NONE',  ( -19.18585068438267882, -47.40892052979416604, -34.01666544723598662 ) ) ;
#77121 = DIRECTION ( 'NONE',  ( 1.000000000000000000, 0.000000000000000000, 0.000000000000000000 ) ) ;
#77123 = ORIENTED_EDGE ( 'NONE', *, *, #39352, .F. ) ;
#77124 = CARTESIAN_POINT ( 'NONE',  ( 0.000000000000000000, 0.000000000000000000, 0.000000000000000000 ) ) ;
#77125 = DIRECTION ( 'NONE',  ( 0.5735764363510470476, -0.8191520442889911324, 1.003171929053524007E-16 ) ) ;
#77126 = VECTOR ( 'NONE', #51799, 1000.000000000000000 ) ;
#77127 = VERTEX_POINT ( 'NONE', #52813 ) ;
#77128 = CARTESIAN_POINT ( 'NONE',  ( 16.36650669486618881, -3.999999999999998224, 0.000000000000000000 ) ) ;
#77129 = CARTESIAN_POINT ( 'NONE',  ( 30.90717084365905976, 9.524046525576030930, -40.57283699552807121 ) ) ;
#77130 = CARTESIAN_POINT ( 'NONE',  ( -10.00000000000000000, 15.00000000000000000, 10.00000000000000000 ) ) ;
#77131 = CARTESIAN_POINT ( 'NONE',  ( -92.06016183752583970, -60.00000000000002132, 5.047127910554535468 ) ) ;
#77132 = MECHANICAL_DESIGN_GEOMETRIC_PRESENTATION_REPRESENTATION (  '', ( #18655 ), #94394 ) ;
#77133 = CARTESIAN_POINT ( 'NONE',  ( 0.000000000000000000, -4.000000000000003553, 112.0000000000000000 ) ) ;
#77134 = AXIS2_PLACEMENT_3D ( 'NONE', #93198, #35528, #102348 ) ;
#77135 = DIRECTION ( 'NONE',  ( -1.000000000000000000, -1.224606353822377258E-16, -0.000000000000000000 ) ) ;
#77136 = CIRCLE ( 'NONE', #29008, 15.00000000000001421 ) ;
#77137 = CARTESIAN_POINT ( 'NONE',  ( 39.08187240373737126, 460.7913535929789077, 2.155912156265418655 ) ) ;
#77138 = CARTESIAN_POINT ( 'NONE',  ( -34.42712901035238815, 435.4031854876006378, 9.698380883803752184 ) ) ;
#77139 = CARTESIAN_POINT ( 'NONE',  ( -85.31458647159905695, -22.02019807324484546, 163.9776401941061863 ) ) ;
#77140 = ORIENTED_EDGE ( 'NONE', *, *, #11871, .T. ) ;
#77141 = CARTESIAN_POINT ( 'NONE',  ( -43.58619280597381618, 434.9882623928566545, 14.52865984557642065 ) ) ;
#77142 = EDGE_LOOP ( 'NONE', ( #29368, #18545, #65654, #95651, #62127 ) ) ;
#77143 = VERTEX_POINT ( 'NONE', #76018 ) ;
#77144 = MECHANICAL_DESIGN_GEOMETRIC_PRESENTATION_REPRESENTATION (  '', ( #78829 ), #22046 ) ;
#77145 = CARTESIAN_POINT ( 'NONE',  ( 2.761899744546835519E-15, 0.000000000000000000, -22.55262289886175964 ) ) ;
#77146 = CARTESIAN_POINT ( 'NONE',  ( 17.39901153685599411, -4.999999999999999112, 2.593512410380747646 ) ) ;
#77147 = CARTESIAN_POINT ( 'NONE',  ( 2.503857664561936320E-16, -8.660254037844401509, -7.422398894150040505 ) ) ;
#77148 = CARTESIAN_POINT ( 'NONE',  ( 80.40000000000000568, 1.023464760207051730E-14, 0.000000000000000000 ) ) ;
#77149 = VERTEX_POINT ( 'NONE', #10742 ) ;
#77150 = CONICAL_SURFACE ( 'NONE', #44443, 4.172000000000001485, 0.9599310885968750373 ) ;
#77151 = SURFACE_STYLE_USAGE ( .BOTH. , #78723 ) ;
#77152 = CARTESIAN_POINT ( 'NONE',  ( -94.22037892716120666, -57.65324192061454056, -13.00879341737615569 ) ) ;
#77153 = CARTESIAN_POINT ( 'NONE',  ( -4.903871675326605839, -67.02085807301496345, -3.461400506969857016 ) ) ;
#77154 = DIRECTION ( 'NONE',  ( -1.000000000000000000, 0.000000000000000000, 0.000000000000000000 ) ) ;
#77155 = CARTESIAN_POINT ( 'NONE',  ( -9.797936955406314041, 101.5332831022951865, -2.012343231877593563 ) ) ;
#77156 = CARTESIAN_POINT ( 'NONE',  ( 20.11650669486618881, 1.474610560812782335E-15, 0.000000000000000000 ) ) ;
#77157 = SURFACE_STYLE_FILL_AREA ( #62067 ) ;
#77158 = CARTESIAN_POINT ( 'NONE',  ( 94.42187179517443951, -29.99999999999998934, 63.29523499578382228 ) ) ;
#77159 = ADVANCED_FACE ( 'NONE', ( #92739 ), #103279, .T. ) ;
#77160 = CARTESIAN_POINT ( 'NONE',  ( -77.10962715007582347, -30.00000000000002842, 176.8398472105207020 ) ) ;
#77161 = CARTESIAN_POINT ( 'NONE',  ( -58.62493915070122341, -46.44083934075592879, 71.88410043818807083 ) ) ;
#77162 = AXIS2_PLACEMENT_3D ( 'NONE', #83789, #1252, #91892 ) ;
#77163 = B_SPLINE_CURVE_WITH_KNOTS ( 'NONE', 3,
 ( #24099, #37768, #29675, #56941, #33239, #45828 ),
 .UNSPECIFIED., .F., .F.,
 ( 4, 2, 4 ),
 ( 2.380733003139562229E-07, 0.001898835937927378101, 0.003797433802554441972 ),
 .UNSPECIFIED. ) ;
#77164 = VERTEX_POINT ( 'NONE', #11269 ) ;
#77165 = CARTESIAN_POINT ( 'NONE',  ( 5.763898627153208665, 13.53725938914606353, 3.972597389303859750 ) ) ;
#77166 = ORIENTED_EDGE ( 'NONE', *, *, #61304, .T. ) ;
#77167 = CARTESIAN_POINT ( 'NONE',  ( -103.9498368666699832, -45.26547174848818855, 177.1723940409133604 ) ) ;
#77168 = CARTESIAN_POINT ( 'NONE',  ( 2.977408999572650927, -10.25000000204838813, -7.188101187500000933 ) ) ;
#77169 = DIRECTION ( 'NONE',  ( 0.9746329792208491272, 0.000000000000000000, -0.2238091951084492937 ) ) ;
#77170 = AXIS2_PLACEMENT_3D ( 'NONE', #78632, #61964, #4767 ) ;
#77171 = FACE_OUTER_BOUND ( 'NONE', #42555, .T. ) ;
#77172 = ORIENTED_EDGE ( 'NONE', *, *, #2980, .F. ) ;
#77173 = CARTESIAN_POINT ( 'NONE',  ( 7.500000000000003553, -2.999999999999876099, -69.80246343544249044 ) ) ;
#77174 = CARTESIAN_POINT ( 'NONE',  ( 93.97977184163765685, -5.000000000000000888, 6.123233995736779101E-16 ) ) ;
#77175 = CARTESIAN_POINT ( 'NONE',  ( -7.188101187500001821, -17.37500000204838813, -2.977408999572651371 ) ) ;
#77176 = CARTESIAN_POINT ( 'NONE',  ( -20.00000000000000000, 12.99999999999999467, 7.500000000000000000 ) ) ;
#77177 = DIRECTION ( 'NONE',  ( 0.000000000000000000, -1.000000000000000000, 0.000000000000000000 ) ) ;
#77178 = CARTESIAN_POINT ( 'NONE',  ( 7.986452802927061612, -81.02690242308115387, 0.5332468218996310183 ) ) ;
#77179 = CARTESIAN_POINT ( 'NONE',  ( 85.18902050349326771, -60.00000000000000000, -15.68190703514374107 ) ) ;
#77180 = CYLINDRICAL_SURFACE ( 'NONE', #55503, 5.000000000000000888 ) ;
#77181 = EDGE_CURVE ( 'NONE', #73080, #54176, #36678, .T. ) ;
#77182 = CARTESIAN_POINT ( 'NONE',  ( -9.206359606520587491, 139.5792630852731691, 0.000000000000000000 ) ) ;
#77183 = CARTESIAN_POINT ( 'NONE',  ( -7.499999999939189976, 33.41357786079682768, -51.06910100954272735 ) ) ;
#77184 = CARTESIAN_POINT ( 'NONE',  ( -31.09282792621365132, -29.07633572334400185, 31.64039428921726227 ) ) ;
#77185 = AXIS2_PLACEMENT_3D ( 'NONE', #31390, #22232, #29799 ) ;
#77186 = CARTESIAN_POINT ( 'NONE',  ( 47.76287223254053771, -25.68661234867465382, 43.12975209083432304 ) ) ;
#77187 = FACE_OUTER_BOUND ( 'NONE', #31025, .T. ) ;
#77189 = MECHANICAL_DESIGN_GEOMETRIC_PRESENTATION_REPRESENTATION (  '', ( #4815 ), #94366 ) ;
#77188 = CARTESIAN_POINT ( 'NONE',  ( -17.49999999999997513, 50.00000000000000000, 100.0000000000000000 ) ) ;
#77190 = CARTESIAN_POINT ( 'NONE',  ( -100.2185995264695322, -38.46493287070022404, 200.4360577060224955 ) ) ;
#77191 = ORIENTED_EDGE ( 'NONE', *, *, #53498, .T. ) ;
#77193 = CARTESIAN_POINT ( 'NONE',  ( -37.88504238421052861, 464.3115779013460269, 20.35635421822102131 ) ) ;
#77192 = CARTESIAN_POINT ( 'NONE',  ( -9.500000000000005329, -5.000000000000000000, -52.94236561372726868 ) ) ;
#77194 = CARTESIAN_POINT ( 'NONE',  ( -19.22370335506887429, 49.79722359267143617, 61.51281625664049102 ) ) ;
#77195 = CARTESIAN_POINT ( 'NONE',  ( -7.409230666798462650, 40.77747091125806378, -58.95054567335854756 ) ) ;
#77196 = CARTESIAN_POINT ( 'NONE',  ( 6.057904175366206623, 41.61856606260997893, -70.65344123640606711 ) ) ;
#77197 = CARTESIAN_POINT ( 'NONE',  ( 0.4053525175236797340, 3.145852061456238413, -6.500000000000000000 ) ) ;
#77198 = CARTESIAN_POINT ( 'NONE',  ( 4.999999999999999112, -58.90829211404609111, 11.71895889478539665 ) ) ;
#77199 = CYLINDRICAL_SURFACE ( 'NONE', #103802, 1.250000000000001110 ) ;
#77200 = AXIS2_PLACEMENT_3D ( 'NONE', #46499, #79393, #5510 ) ;
#77201 = EDGE_CURVE ( 'NONE', #74331, #50990, #60402, .T. ) ;
#77202 = CARTESIAN_POINT ( 'NONE',  ( 112.1773567419170377, -59.99999999999999289, 169.0791235005425790 ) ) ;
#77203 = MECHANICAL_DESIGN_GEOMETRIC_PRESENTATION_REPRESENTATION (  '', ( #49619 ), #23868 ) ;
#77204 = CARTESIAN_POINT ( 'NONE',  ( -7.999912353029502654, -68.99982470603094953, -0.2691822806795026723 ) ) ;
#77205 = ORIENTED_EDGE ( 'NONE', *, *, #32278, .F. ) ;
#77206 = CARTESIAN_POINT ( 'NONE',  ( -81.57272358321040429, -29.99999999999999289, -5.204509085996302353 ) ) ;
#77207 = ORIENTED_EDGE ( 'NONE', *, *, #13899, .F. ) ;
#77209 = CARTESIAN_POINT ( 'NONE',  ( 10.11650669486618881, 1.474610560812782335E-15, 0.000000000000000000 ) ) ;
#77208 = CARTESIAN_POINT ( 'NONE',  ( -55.85004154032156265, -38.34489998747773143, 83.90154939705580261 ) ) ;
#77210 = CARTESIAN_POINT ( 'NONE',  ( 46.00000000000000711, 438.0199209727295511, 11.62474111259973775 ) ) ;
#77211 = DIRECTION ( 'NONE',  ( -1.000000000000000000, -0.000000000000000000, -0.000000000000000000 ) ) ;
#77213 = FACE_OUTER_BOUND ( 'NONE', #106037, .T. ) ;
#77212 = CIRCLE ( 'NONE', #49628, 8.750000000000033751 ) ;
#77214 = PRESENTATION_LAYER_ASSIGNMENT (  '', '', ( #85862 ) ) ;
#77215 = CARTESIAN_POINT ( 'NONE',  ( -2.977408999572654480, -11.00000000204838635, 7.188101187499999156 ) ) ;
#77216 = AXIS2_PLACEMENT_3D ( 'NONE', #24310, #81425, #23237 ) ;
#77217 = ADVANCED_FACE ( 'NONE', ( #59322 ), #51524, .T. ) ;
#77218 = VECTOR ( 'NONE', #50156, 1000.000000000000000 ) ;
#77219 = CARTESIAN_POINT ( 'NONE',  ( 29.85155995213039049, 18.03343143632517709, -39.61445771744218547 ) ) ;
#77221 = ORIENTED_EDGE ( 'NONE', *, *, #51547, .F. ) ;
#77220 = CARTESIAN_POINT ( 'NONE',  ( -33.49627437238255112, 465.2401082457186590, 8.307162268441771857 ) ) ;
#77222 = CARTESIAN_POINT ( 'NONE',  ( 84.69268008423972560, -28.96262395815541524, 169.4286736083946892 ) ) ;
#77223 = CARTESIAN_POINT ( 'NONE',  ( 21.67692307692307452, -4.171999999999999709, 0.000000000000000000 ) ) ;
#77224 = CARTESIAN_POINT ( 'NONE',  ( 46.08349330513379982, 4.000000000000003553, 0.000000000000000000 ) ) ;
#77225 = VERTEX_POINT ( 'NONE', #91692 ) ;
#77226 = CARTESIAN_POINT ( 'NONE',  ( -9.970195021759442611, 302.6460196488377505, -10.04373974541436887 ) ) ;
#77227 = CARTESIAN_POINT ( 'NONE',  ( 17.07926083379644311, 34.90888828800229504, 21.84001637439316568 ) ) ;
#77228 = CARTESIAN_POINT ( 'NONE',  ( 4.898587196589412829E-16, -28.62499999999999289, -8.000000000000000000 ) ) ;
#77229 = CARTESIAN_POINT ( 'NONE',  ( 5.799999999999999822, 6.928203230275505220, -4.000000000000006217 ) ) ;
#77230 = CARTESIAN_POINT ( 'NONE',  ( 0.2958821552773560626, 18.79221613348494913, 49.28340278884313364 ) ) ;
#77231 =( NAMED_UNIT ( * ) PLANE_ANGLE_UNIT ( ) SI_UNIT ( $, .RADIAN. ) );
#77232 = ORIENTED_EDGE ( 'NONE', *, *, #102723, .T. ) ;
#77233 = EDGE_CURVE ( 'NONE', #741, #73917, #85969, .T. ) ;
#77234 = AXIS2_PLACEMENT_3D ( 'NONE', #11298, #27551, #60431 ) ;
#77235 = CARTESIAN_POINT ( 'NONE',  ( 31.14131030317610538, 1.482358050883964840E-15, 0.000000000000000000 ) ) ;
#77236 = CARTESIAN_POINT ( 'NONE',  ( 30.95568101991391430, 18.64284798592769476, 22.77427805268053262 ) ) ;
#77237 = CARTESIAN_POINT ( 'NONE',  ( 86.57905893650337248, -16.99609905251657338, 184.8754976615798284 ) ) ;
#77238 = EDGE_CURVE ( 'NONE', #8439, #64182, #96474, .T. ) ;
#77240 = CARTESIAN_POINT ( 'NONE',  ( -12.29994342143133856, 5.683500474366485200, -8.444376441994753790 ) ) ;
#77239 = CARTESIAN_POINT ( 'NONE',  ( 43.58525199863880317, 435.7810069860513522, 17.82023302324629199 ) ) ;
#77241 = EDGE_CURVE ( 'NONE', #59690, #101469, #13646, .T. ) ;
#77242 = AXIS2_PLACEMENT_3D ( 'NONE', #6454, #39390, #80879 ) ;
#77243 = CARTESIAN_POINT ( 'NONE',  ( 5.082755093536324154, -25.34375000204838813, 5.082755093536326818 ) ) ;
#77244 = UNCERTAINTY_MEASURE_WITH_UNIT (LENGTH_MEASURE( 1.000000000000000082E-05 ), #64804, 'distance_accuracy_value', 'NONE');
#77245 = LINE ( 'NONE', #70741, #102518 ) ;
#77246 = CARTESIAN_POINT ( 'NONE',  ( 0.000000000000000000, -5.000000000000000000, 10.00000000000000000 ) ) ;
#77247 = CARTESIAN_POINT ( 'NONE',  ( 41.18601555923955715, 436.5297812499078987, 21.34108204767431616 ) ) ;
#77248 = ORIENTED_EDGE ( 'NONE', *, *, #81590, .T. ) ;
#77249 = CARTESIAN_POINT ( 'NONE',  ( 41.12904442321167409, 485.7386261246315939, -4.649563818470188181 ) ) ;
#77250 = EDGE_CURVE ( 'NONE', #57315, #76301, #44703, .T. ) ;
#77251 = PRESENTATION_STYLE_ASSIGNMENT (( #60554 ) ) ;
#77252 = CARTESIAN_POINT ( 'NONE',  ( -9.943426265976000877, 7.591391547524681371, -5.000000000000000000 ) ) ;
#77253 = FILL_AREA_STYLE_COLOUR ( '', #80712 ) ;
#77254 = ORIENTED_EDGE ( 'NONE', *, *, #26377, .T. ) ;
#77255 = CIRCLE ( 'NONE', #37649, 3.309500000000001663 ) ;
#77256 = CARTESIAN_POINT ( 'NONE',  ( -7.562525622355496857, 52.15248883143013359, -2.008797297745641863 ) ) ;
#77257 = CARTESIAN_POINT ( 'NONE',  ( 4.699999999999999289, 7.505553499465139389, 0.000000000000000000 ) ) ;
#77258 = ORIENTED_EDGE ( 'NONE', *, *, #1063, .F. ) ;
#77259 = CIRCLE ( 'NONE', #25562, 4.000000000000007105 ) ;
#77260 = CARTESIAN_POINT ( 'NONE',  ( 33.06682630402978873, 435.0798260220875591, 15.58372260938782539 ) ) ;
#77261 = CARTESIAN_POINT ( 'NONE',  ( -0.8446698455446330911, 8.504696595714664298, -51.42477032456711328 ) ) ;
#77262 = CARTESIAN_POINT ( 'NONE',  ( 32.82269234420716231, 485.2607240917815830, 5.823166218282061379 ) ) ;
#77263 =( LENGTH_UNIT ( ) NAMED_UNIT ( * ) SI_UNIT ( .MILLI., .METRE. ) );
#77264 = UNCERTAINTY_MEASURE_WITH_UNIT (LENGTH_MEASURE( 1.000000000000000082E-05 ), #2316, 'distance_accuracy_value', 'NONE');
#77265 = CARTESIAN_POINT ( 'NONE',  ( -108.5660005441912972, -60.00000000000000711, 194.5918078993309166 ) ) ;
#77266 = FILL_AREA_STYLE ('',( #101541 ) ) ;
#77267 = CARTESIAN_POINT ( 'NONE',  ( 25.11650669486618881, 4.898587196589413815E-16, -4.000000000000000888 ) ) ;
#77269 = AXIS2_PLACEMENT_3D ( 'NONE', #11738, #101827, #60339 ) ;
#77268 = DIRECTION ( 'NONE',  ( 0.000000000000000000, 1.000000000000000000, 0.000000000000000000 ) ) ;
#77270 = CARTESIAN_POINT ( 'NONE',  ( -45.43339346675878687, 430.7348383325900727, 7.234598910837349628 ) ) ;
#77271 = CARTESIAN_POINT ( 'NONE',  ( -82.96224355738017664, -50.06567045369714464, 183.0600446902855083 ) ) ;
#77272 = FILL_AREA_STYLE_COLOUR ( '', #41895 ) ;
#77273 =( BOUNDED_CURVE ( )  B_SPLINE_CURVE ( 2, ( #36058, #68394, #52183 ),
 .UNSPECIFIED., .F., .F. ) 
 B_SPLINE_CURVE_WITH_KNOTS ( ( 3, 3 ),
 ( 0.000000000000000000, 1.000000000000000000 ),
 .UNSPECIFIED. ) 
 CURVE ( )  GEOMETRIC_REPRESENTATION_ITEM ( )  RATIONAL_B_SPLINE_CURVE ( ( 1.000000000000000000, 1.857142857142858317, 1.000000000000000000 ) ) 
 REPRESENTATION_ITEM ( '' )  );
#77274 = ORIENTED_EDGE ( 'NONE', *, *, #72946, .F. ) ;
#77275 = CARTESIAN_POINT ( 'NONE',  ( -4.269529794339158357, 302.8261475903860855, 9.931633466322995929 ) ) ;
#77276 = FACE_OUTER_BOUND ( 'NONE', #36803, .T. ) ;
#77277 = CARTESIAN_POINT ( 'NONE',  ( -82.58559367277240426, -37.83348976570933075, 5.520925785892475623 ) ) ;
#77278 = DIRECTION ( 'NONE',  ( -1.000000000000000000, 0.000000000000000000, 0.000000000000000000 ) ) ;
#77279 = SURFACE_SIDE_STYLE ('',( #44384 ) ) ;
#77280 = CARTESIAN_POINT ( 'NONE',  ( 8.588409832247142717, 128.2015064896668264, -5.000000000000000000 ) ) ;
#77282 = DIRECTION ( 'NONE',  ( -1.000000000000000000, 0.000000000000000000, 0.000000000000000000 ) ) ;
#77281 = AXIS2_PLACEMENT_3D ( 'NONE', #38566, #40133, #64428 ) ;
#77283 = CARTESIAN_POINT ( 'NONE',  ( -72.41885610115939187, 42.00000000000000000, 55.65414010178468374 ) ) ;
#77284 = CIRCLE ( 'NONE', #42867, 57.21727615095610275 ) ;
#77285 = CARTESIAN_POINT ( 'NONE',  ( 73.20367453073632191, -59.99999999999985789, 185.6239686060362146 ) ) ;
#77286 = EDGE_CURVE ( 'NONE', #48079, #7253, #92877, .T. ) ;
#77287 = CARTESIAN_POINT ( 'NONE',  ( -86.49433777984398830, -14.21045842199439946, 11.85125679505764928 ) ) ;
#77288 = CARTESIAN_POINT ( 'NONE',  ( -69.97160914037661428, -53.38730675860333719, 110.0502627141849956 ) ) ;
#77289 = ORIENTED_EDGE ( 'NONE', *, *, #70424, .F. ) ;
#77290 = CARTESIAN_POINT ( 'NONE',  ( 79.57068731991196842, -14.21045842199434794, 190.0104166006057085 ) ) ;
#77291 = CARTESIAN_POINT ( 'NONE',  ( -49.76137878681610260, 40.83833847419749219, 41.92585938202696383 ) ) ;
#77292 = CARTESIAN_POINT ( 'NONE',  ( 81.55124166166723398, -57.67115036738129419, -29.31836794746244124 ) ) ;
#77293 = AXIS2_PLACEMENT_3D ( 'NONE', #3097, #52698, #2019 ) ;
#77294 = VERTEX_POINT ( 'NONE', #5846 ) ;
#77295 = CARTESIAN_POINT ( 'NONE',  ( 14.00175760317098117, -58.00025725680810496, 26.85746939222903151 ) ) ;
#77296 = CARTESIAN_POINT ( 'NONE',  ( -5.082755093536326818, -23.09375000204838457, 5.082755093536325042 ) ) ;
#77297 = CARTESIAN_POINT ( 'NONE',  ( -4.496882872040837142, -9.462113345103771778, 3.972797206970396733 ) ) ;
#77298 = ORIENTED_EDGE ( 'NONE', *, *, #43117, .T. ) ;
#77299 = VERTEX_POINT ( 'NONE', #53869 ) ;
#77300 = DIRECTION ( 'NONE',  ( 0.000000000000000000, -1.000000000000000000, 0.000000000000000000 ) ) ;
#77301 = CARTESIAN_POINT ( 'NONE',  ( -91.90915390750564029, -59.99999999999997158, 16.42317985402541325 ) ) ;
#77302 = DIRECTION ( 'NONE',  ( 0.000000000000000000, 0.000000000000000000, -1.000000000000000000 ) ) ;
#77303 = CARTESIAN_POINT ( 'NONE',  ( -2.977408999572650039, -9.687500002048384573, -7.188101187500001821 ) ) ;
#77304 = LINE ( 'NONE', #2333, #72249 ) ;
#77305 = CARTESIAN_POINT ( 'NONE',  ( 1.289261528792995382, -0.01360727255291783316, 101.4143542463165204 ) ) ;
#77306 = DIRECTION ( 'NONE',  ( 3.997486475784785298E-16, 0.5626279437268310035, 0.8267102254948331952 ) ) ;
#77307 = CARTESIAN_POINT ( 'NONE',  ( -3.140974613990812792, 50.00000000000000000, -73.31232788067644890 ) ) ;
#77308 = EDGE_CURVE ( 'NONE', #22182, #61560, #35939, .T. ) ;
#77309 = CARTESIAN_POINT ( 'NONE',  ( 23.21751746555144180, 27.38103382803512176, -33.20617127781698485 ) ) ;
#77310 = CARTESIAN_POINT ( 'NONE',  ( 40.20451861284013262, 437.0088225241108262, 5.689194366316798757 ) ) ;
#77311 = AXIS2_PLACEMENT_3D ( 'NONE', #73928, #32978, #65848 ) ;
#77312 = ORIENTED_EDGE ( 'NONE', *, *, #42293, .T. ) ;
#77313 =( NAMED_UNIT ( * ) PLANE_ANGLE_UNIT ( ) SI_UNIT ( $, .RADIAN. ) );
#77315 = CARTESIAN_POINT ( 'NONE',  ( 32.18313561787557120, -32.55190988895232351, 32.69763082105384200 ) ) ;
#77314 = CARTESIAN_POINT ( 'NONE',  ( 5.126143460586249034, 52.11941149169467735, -6.031152949374488870 ) ) ;
#77316 = CARTESIAN_POINT ( 'NONE',  ( 3.301606509414619861, -4.285714285714286476, 25.22241582816893413 ) ) ;
#77317 = ORIENTED_EDGE ( 'NONE', *, *, #91189, .F. ) ;
#77318 = CARTESIAN_POINT ( 'NONE',  ( 35.40902385155721532, 484.3229957183398824, -1.494454771037330376 ) ) ;
#77319 = VECTOR ( 'NONE', #66444, 1000.000000000000000 ) ;
#77320 = B_SPLINE_CURVE_WITH_KNOTS ( 'NONE', 3,
 ( #12698, #69894, #53183, #70950 ),
 .UNSPECIFIED., .F., .F.,
 ( 4, 4 ),
 ( 0.000000000000000000, 0.003677212860670048700 ),
 .UNSPECIFIED. ) ;
#77322 = CARTESIAN_POINT ( 'NONE',  ( 6.701893401236465486, 41.44328394225253476, -70.59544911815949320 ) ) ;
#77321 = DIRECTION ( 'NONE',  ( 0.000000000000000000, -1.000000000000000000, 0.000000000000000000 ) ) ;
#77323 = DIRECTION ( 'NONE',  ( -1.000000000000000000, -1.224606353822377258E-16, -0.000000000000000000 ) ) ;
#77324 = CARTESIAN_POINT ( 'NONE',  ( 73.33904886068935980, 6.975173280561618775E-15, 0.000000000000000000 ) ) ;
#77325 = CARTESIAN_POINT ( 'NONE',  ( -9.500000000000007105, -5.000000000000000000, -68.91429205785459544 ) ) ;
#77326 = CYLINDRICAL_SURFACE ( 'NONE', #56901, 5.000000000000000888 ) ;
#77327 = CARTESIAN_POINT ( 'NONE',  ( 61.11682663846713837, 4.000000000000014211, 0.000000000000000000 ) ) ;
#77328 = ORIENTED_EDGE ( 'NONE', *, *, #101121, .F. ) ;
#77329 = EDGE_CURVE ( 'NONE', #32616, #20548, #82104, .T. ) ;
#77330 = CARTESIAN_POINT ( 'NONE',  ( 92.00718413779456739, -60.00000000000000711, 6.061572897356207967 ) ) ;
#77331 = COLOUR_RGB ( '', 0.66274510, 0.83137255, 0.94901961) ;
#77332 = PRESENTATION_STYLE_ASSIGNMENT (( #19138 ) ) ;
#77333 = CARTESIAN_POINT ( 'NONE',  ( -36.72880825614078759, 408.9631818827540997, 6.288650551464858296 ) ) ;
#77334 = EDGE_CURVE ( 'NONE', #48529, #82621, #66613, .T. ) ;
#77335 = CARTESIAN_POINT ( 'NONE',  ( -4.933292134499193793, 41.54835750584372533, -70.57172791559196412 ) ) ;
#77336 = CARTESIAN_POINT ( 'NONE',  ( -11.46558483138156603, 15.01111260705223849, -9.824584598569959581 ) ) ;
#77337 = VERTEX_POINT ( 'NONE', #98442 ) ;
#77338 = CARTESIAN_POINT ( 'NONE',  ( -107.6467995412221939, -30.00000000000500222, 189.8238950325566918 ) ) ;
#77339 = ORIENTED_EDGE ( 'NONE', *, *, #52484, .T. ) ;
#77340 = AXIS2_PLACEMENT_3D ( 'NONE', #73120, #106025, #32170 ) ;
#77341 = CARTESIAN_POINT ( 'NONE',  ( -9.269255467170962604, -55.04472406073652024, 23.24713075214419433 ) ) ;
#77342 = CARTESIAN_POINT ( 'NONE',  ( 0.000000000000000000, 0.5000000000000000000, 0.000000000000000000 ) ) ;
#77343 = CARTESIAN_POINT ( 'NONE',  ( 46.84999999999999432, 1.533819458162526451E-15, 0.000000000000000000 ) ) ;
#77344 = CARTESIAN_POINT ( 'NONE',  ( 16.12882272094003611, 21.28108484452593174, -2.990375923983669360 ) ) ;
#77345 = CARTESIAN_POINT ( 'NONE',  ( 83.26603652480599749, -45.27681178268631612, -13.97111306700649180 ) ) ;
#77346 = CARTESIAN_POINT ( 'NONE',  ( -7.188101187500002709, -29.18750000204839523, 2.977408999572648707 ) ) ;
#77347 = CARTESIAN_POINT ( 'NONE',  ( 62.59428447264396311, 6.856755485862130937E-15, 0.000000000000000000 ) ) ;
#77348 = CLOSED_SHELL ( 'NONE', ( #61965, #61625, #60035, #14100, #40125, #82826, #63328, #5453, #37161, #45875, #52834, #70768, #96497, #104197, #65013, #8664, #34817, #15924, #9224, #61612, #88323, #36850, #14323, #21377, #94617, #104040, #51156, #102410, #60412, #84099, #12955, #46395, #80780, #83387, #33651, #15256, #30390, #39950, #74334, #64919, #92362, #34430, #22656, #21139, #28191, #44640, #71209, #15596, #26496, #85165, #102368, #67377, #79170, #105478, #28146, #22773, #67665, #90210, #26724 ) ) ;
#77349 = ORIENTED_EDGE ( 'NONE', *, *, #19889, .F. ) ;
#77350 = CARTESIAN_POINT ( 'NONE',  ( -10.00000000000000355, 15.00000000000000000, -10.00000000000000000 ) ) ;
#77351 = VERTEX_POINT ( 'NONE', #25117 ) ;
#77352 = CARTESIAN_POINT ( 'NONE',  ( 49.25933966097094441, 7.764757817614878377, -15.83577412118909677 ) ) ;
#77353 =( NAMED_UNIT ( * ) PLANE_ANGLE_UNIT ( ) SI_UNIT ( $, .RADIAN. ) );
#77355 = ORIENTED_EDGE ( 'NONE', *, *, #32925, .T. ) ;
#77354 = DIRECTION ( 'NONE',  ( 0.000000000000000000, 1.000000000000000000, 0.000000000000000000 ) ) ;
#77356 = CARTESIAN_POINT ( 'NONE',  ( 74.24595519639049712, -25.59685389213801443, 107.9157497212091528 ) ) ;
#77357 = CONICAL_SURFACE ( 'NONE', #30871, 3.309500000000001663, 0.9599310885968770357 ) ;
#77358 = ORIENTED_EDGE ( 'NONE', *, *, #90893, .F. ) ;
#77359 = CARTESIAN_POINT ( 'NONE',  ( 2.783573587432064400, -49.58977995685751239, 44.41792197296597777 ) ) ;
#77360 = CARTESIAN_POINT ( 'NONE',  ( 5.082755093536325930, -17.46875000204838457, -5.082755093536325042 ) ) ;
#77361 = CARTESIAN_POINT ( 'NONE',  ( -71.40526007946631637, -57.68007955256489083, 166.0300312729133623 ) ) ;
#77362 = ORIENTED_EDGE ( 'NONE', *, *, #57360, .F. ) ;
#77363 = SURFACE_SIDE_STYLE ('',( #94632 ) ) ;
#77364 = CARTESIAN_POINT ( 'NONE',  ( -18.10430355215808973, 43.96790572561079102, -85.61069757033331484 ) ) ;
#77365 = CARTESIAN_POINT ( 'NONE',  ( 4.474408960159419024, 9.482498132260746004, 5.000000000000000888 ) ) ;
#77366 = AXIS2_PLACEMENT_3D ( 'NONE', #36542, #38129, #78021 ) ;
#77367 = CARTESIAN_POINT ( 'NONE',  ( -37.83989825151947173, 491.0717236019712573, 13.27726931866635596 ) ) ;
#77368 = CARTESIAN_POINT ( 'NONE',  ( 48.60160210973891992, 15.38206115941115470, -14.48795722268628872 ) ) ;
#77369 = CARTESIAN_POINT ( 'NONE',  ( 3.313708498984762496, -20.46875000409677270, 7.999999999999998224 ) ) ;
#77370 = CARTESIAN_POINT ( 'NONE',  ( -52.75365474858949000, -30.00000000000000711, 51.53900060926203253 ) ) ;
#77371 = DIRECTION ( 'NONE',  ( 0.000000000000000000, -1.000000000000000000, 0.000000000000000000 ) ) ;
#77372 = FACE_OUTER_BOUND ( 'NONE', #10929, .T. ) ;
#77373 = CARTESIAN_POINT ( 'NONE',  ( 9.334514330295428763, 31.78622737681786958, -3.588704711590615215 ) ) ;
#77374 = DIRECTION ( 'NONE',  ( 0.000000000000000000, 0.000000000000000000, 1.000000000000000000 ) ) ;
#77375 = DIRECTION ( 'NONE',  ( 0.000000000000000000, 1.000000000000000000, 0.000000000000000000 ) ) ;
#77376 = CARTESIAN_POINT ( 'NONE',  ( 6.522118525112259313, -30.00000000000000355, -3.363504998894041975 ) ) ;
#77377 = ORIENTED_EDGE ( 'NONE', *, *, #96603, .T. ) ;
#77378 = CARTESIAN_POINT ( 'NONE',  ( -2.409582269539474186, -53.72452336040274901, 40.79253407940785081 ) ) ;
#77379 = FACE_OUTER_BOUND ( 'NONE', #78472, .T. ) ;
#77380 = EDGE_CURVE ( 'NONE', #53956, #56662, #72242, .T. ) ;
#77381 = CARTESIAN_POINT ( 'NONE',  ( 0.5336880547914685247, 8.009115710655695608, 51.63698046263905184 ) ) ;
#77382 = CARTESIAN_POINT ( 'NONE',  ( -75.51516288543760425, -29.99999999999999289, -27.33247042156351725 ) ) ;
#77383 = CARTESIAN_POINT ( 'NONE',  ( -84.87290633932420292, -30.00000000000000000, 169.1199384629161102 ) ) ;
#77384 = EDGE_CURVE ( 'NONE', #72737, #76534, #243, .T. ) ;
#77385 = ORIENTED_EDGE ( 'NONE', *, *, #86409, .T. ) ;
#77386 = VECTOR ( 'NONE', #82942, 1000.000000000000000 ) ;
#77387 = CARTESIAN_POINT ( 'NONE',  ( -13.75294187979978666, -4.333298119783973945, -11.48770422822915727 ) ) ;
#77388 = CARTESIAN_POINT ( 'NONE',  ( 81.43375511528206800, -57.51667291745025778, 200.0811565040724815 ) ) ;
#77389 = EDGE_CURVE ( 'NONE', #91653, #41746, #9966, .T. ) ;
#77390 = CARTESIAN_POINT ( 'NONE',  ( 2.617478843592800697, 48.00000000000000711, -75.26027323331685182 ) ) ;
#77391 = COLOUR_RGB ( '', 0.08235294, 0.09019608, 0.10196078) ;
#77392 = CARTESIAN_POINT ( 'NONE',  ( 28.29337419442703094, -28.94310075340867172, -38.25297961115466450 ) ) ;
#77393 = CARTESIAN_POINT ( 'NONE',  ( -16.14595037822576273, 20.23371447306055870, -4.922994507639441686 ) ) ;
#77394 = DIRECTION ( 'NONE',  ( -0.5735764363510494901, -0.8191520442889894671, 0.000000000000000000 ) ) ;
#77395 = CARTESIAN_POINT ( 'NONE',  ( -71.96544483848215634, -60.00000000000000000, 154.0212030161015946 ) ) ;
#77396 = CARTESIAN_POINT ( 'NONE',  ( -31.92502370130780065, 439.7300840721472923, 23.86368504749432518 ) ) ;
#77397 = CARTESIAN_POINT ( 'NONE',  ( -84.89981489726106645, -57.47619647151204703, 192.0086891560063407 ) ) ;
#77398 = EDGE_LOOP ( 'NONE', ( #89471, #79118, #63677, #85350, #84275 ) ) ;
#77399 = CARTESIAN_POINT ( 'NONE',  ( -42.19180677453721273, 462.2931784592651638, 3.389262873192026682 ) ) ;
#77400 = CARTESIAN_POINT ( 'NONE',  ( -5.051437835758245676, -35.99424957357602040, 29.87887688983398959 ) ) ;
#77401 = CARTESIAN_POINT ( 'NONE',  ( -7.099152841014172211, 41.70084716954765724, -59.82719248405098256 ) ) ;
#77402 = CARTESIAN_POINT ( 'NONE',  ( 0.000000000000000000, 0.000000000000000000, -9.449444346342716017 ) ) ;
#77403 = PRODUCT_DEFINITION_SHAPE ( 'NONE', 'NONE',  #6702 ) ;
#77404 = CARTESIAN_POINT ( 'NONE',  ( -7.316272466829250476, 54.23236173032573504, 3.143061027692354514 ) ) ;
#77405 = VERTEX_POINT ( 'NONE', #770 ) ;
#77406 = CARTESIAN_POINT ( 'NONE',  ( 18.09999999999999787, 1.533819458162526451E-15, 0.000000000000000000 ) ) ;
#77407 =( GEOMETRIC_REPRESENTATION_CONTEXT ( 3 ) GLOBAL_UNCERTAINTY_ASSIGNED_CONTEXT ( ( #101717 ) ) GLOBAL_UNIT_ASSIGNED_CONTEXT ( ( #35068, #51740, #67418 ) ) REPRESENTATION_CONTEXT ( 'NONE', 'WORKASPACE' ) );
#77408 = CARTESIAN_POINT ( 'NONE',  ( -37.56673239365849781, -1.200000000000000030E-05, 10.95617127781066102 ) ) ;
#77409 = DIRECTION ( 'NONE',  ( -0.7071067811865456854, 0.000000000000000000, 0.7071067811865493491 ) ) ;
#77410 = ORIENTED_EDGE ( 'NONE', *, *, #76241, .T. ) ;
#77411 = CARTESIAN_POINT ( 'NONE',  ( 17.50213914152930883, 50.00000000000000000, 63.56338360167926282 ) ) ;
#77412 = CARTESIAN_POINT ( 'NONE',  ( 30.24427031855517711, 312.0196691915732004, -8.325478004009855937 ) ) ;
#77413 = LINE ( 'NONE', #33786, #34042 ) ;
#77414 = CARTESIAN_POINT ( 'NONE',  ( 8.559508646656350805, 53.68473964988125857, -4.031152949374623873 ) ) ;
#77415 = EDGE_CURVE ( 'NONE', #45384, #4872, #80853, .T. ) ;
#77416 = CIRCLE ( 'NONE', #30954, 4.000000000000001776 ) ;
#77417 = CARTESIAN_POINT ( 'NONE',  ( 99.88996038257948840, -14.21045842199439946, 111.7630621600675198 ) ) ;
#77418 = CARTESIAN_POINT ( 'NONE',  ( -80.37466735423569730, -46.44052868790205935, 156.8257416479256960 ) ) ;
#77419 = EDGE_LOOP ( 'NONE', ( #43336, #3521, #70452, #91689, #27018, #91660, #48490, #61189, #97381, #66137, #97954, #37154, #51301, #96709, #79532, #88898, #61112, #36001, #12159, #81427, #49265, #9921, #27768, #12342, #13430, #71211, #466, #57897, #20714, #37038, #57308, #28383 ) ) ;
#77420 = CARTESIAN_POINT ( 'NONE',  ( 43.71297783477850629, 485.1278128289774827, -1.116606130290134002 ) ) ;
#77421 = DIRECTION ( 'NONE',  ( 0.000000000000000000, 0.000000000000000000, 1.000000000000000000 ) ) ;
#77422 = CARTESIAN_POINT ( 'NONE',  ( 43.21692225861351488, -57.68546145064757980, 61.44301319263212235 ) ) ;
#77423 = CARTESIAN_POINT ( 'NONE',  ( 6.289692432696790014, -0.6629690750393451015, -6.828989928337169779 ) ) ;
#77424 = CARTESIAN_POINT ( 'NONE',  ( 33.59630659472934866, 315.8721021973062193, -6.875841742740135487 ) ) ;
#77425 = COLOUR_RGB ( '', 0.08235294, 0.09019608, 0.10196078) ;
#77426 = CARTESIAN_POINT ( 'NONE',  ( 43.71335306921149311, 464.5235014653563894, 7.258763594095269056 ) ) ;
#77427 = ORIENTED_EDGE ( 'NONE', *, *, #8679, .T. ) ;
#77428 = UNCERTAINTY_MEASURE_WITH_UNIT (LENGTH_MEASURE( 1.000000000000000082E-05 ), #89013, 'distance_accuracy_value', 'NONE');
#77429 = CARTESIAN_POINT ( 'NONE',  ( -33.00000000000000000, 489.5971041675261404, 10.80646835458718868 ) ) ;
#77430 = DIRECTION ( 'NONE',  ( 0.000000000000000000, 0.000000000000000000, 1.000000000000000000 ) ) ;
#77431 = CARTESIAN_POINT ( 'NONE',  ( 2.977408999572651815, -22.43750000204838813, 7.188101187500000933 ) ) ;
#77432 = EDGE_LOOP ( 'NONE', ( #10667, #94911, #24686, #66906, #14124 ) ) ;
#77433 = CARTESIAN_POINT ( 'NONE',  ( 63.56127108291158123, -1.232595164407830946E-29, 4.000000000000007105 ) ) ;
#77434 = CARTESIAN_POINT ( 'NONE',  ( 1.544939622599074580, 15.00000000000000000, 9.999999999999998224 ) ) ;
#77435 = CARTESIAN_POINT ( 'NONE',  ( 7.125691916903466705, 41.67430808309654822, -69.26730091920677523 ) ) ;
#77436 = EDGE_CURVE ( 'NONE', #83791, #46974, #8491, .T. ) ;
#77437 = CARTESIAN_POINT ( 'NONE',  ( -63.03617022294436367, 49.99999999995993250, -16.93907820454377244 ) ) ;
#77438 = CARTESIAN_POINT ( 'NONE',  ( 6.531352669123184462, -12.73774374834599321, -7.942415274083415078 ) ) ;
#77439 = LINE ( 'NONE', #20324, #92585 ) ;
#77440 = ORIENTED_EDGE ( 'NONE', *, *, #1983, .F. ) ;
#77441 = CARTESIAN_POINT ( 'NONE',  ( 55.19382646853485141, -60.00000000000000000, -36.81090248795683806 ) ) ;
#77443 = CARTESIAN_POINT ( 'NONE',  ( 23.23955225627396359, -25.55842996810111956, 29.06036204385301502 ) ) ;
#77442 = CARTESIAN_POINT ( 'NONE',  ( -40.90223414571102012, -60.00000000000005684, 57.82070650035302606 ) ) ;
#77444 = MECHANICAL_DESIGN_GEOMETRIC_PRESENTATION_REPRESENTATION (  '', ( #60224 ), #63673 ) ;
#77445 = CARTESIAN_POINT ( 'NONE',  ( 4.143270396293103855E-15, 58.72416816948006613, -16.91618513671782509 ) ) ;
#77446 = CARTESIAN_POINT ( 'NONE',  ( -34.47814148916032906, -36.03572155392134135, 34.37536576405466349 ) ) ;
#77447 = UNCERTAINTY_MEASURE_WITH_UNIT (LENGTH_MEASURE( 1.000000000000000082E-05 ), #69444, 'distance_accuracy_value', 'NONE');
#77448 = B_SPLINE_CURVE_WITH_KNOTS ( 'NONE', 3,
 ( #49782, #68652, #3369, #70228, #21185, #77256, #100992, #10377, #19600, #3902, #11434, #52431, #27150, #36314, #92897, #43818, #85348, #85902 ),
 .UNSPECIFIED., .F., .F.,
 ( 4, 2, 2, 2, 2, 2, 2, 2, 4 ),
 ( 0.003275144142300112030, 0.003781209443760275707, 0.004287274745220439817, 0.004793340046680603060, 0.005046372697410685983, 0.005299405348140768905, 0.005805470649600934750, 0.006311535951061099728, 0.007323666553981426214 ),
 .UNSPECIFIED. ) ;
#77449 = ORIENTED_EDGE ( 'NONE', *, *, #14366, .F. ) ;
#77450 = FILL_AREA_STYLE ('',( #13755 ) ) ;
#77451 = CARTESIAN_POINT ( 'NONE',  ( 71.17283260602091843, -38.00000000000000000, -21.88484610531455488 ) ) ;
#77452 = CARTESIAN_POINT ( 'NONE',  ( 6.920567593065738876, -12.35473601147218403, 8.513547508574102807 ) ) ;
#77453 = AXIS2_PLACEMENT_3D ( 'NONE', #91676, #75475, #50641 ) ;
#77454 = CARTESIAN_POINT ( 'NONE',  ( -1.251141718528236524, 51.63899026595163377, -9.149171384829717368 ) ) ;
#77455 = LINE ( 'NONE', #28953, #31008 ) ;
#77456 =( NAMED_UNIT ( * ) PLANE_ANGLE_UNIT ( ) SI_UNIT ( $, .RADIAN. ) );
#77457 = ORIENTED_EDGE ( 'NONE', *, *, #19197, .T. ) ;
#77458 =( NAMED_UNIT ( * ) SI_UNIT ( $, .STERADIAN. ) SOLID_ANGLE_UNIT ( ) );
#77459 = EDGE_CURVE ( 'NONE', #18, #48447, #104975, .T. ) ;
#77460 = CARTESIAN_POINT ( 'NONE',  ( 18.91791044776121211, 46.94999999999998153, 62.18611311450882795 ) ) ;
#77461 = ORIENTED_EDGE ( 'NONE', *, *, #80919, .F. ) ;
#77462 = CARTESIAN_POINT ( 'NONE',  ( 90.62888254124575838, -30.00000000000016698, 190.3062381107464205 ) ) ;
#77463 = DIRECTION ( 'NONE',  ( 0.000000000000000000, -1.000000000000000000, 0.000000000000000000 ) ) ;
#77464 = CARTESIAN_POINT ( 'NONE',  ( -5.383284837158154978, -81.99950656484222122, 2.657356347551699027 ) ) ;
#77465 = CARTESIAN_POINT ( 'NONE',  ( 81.36361026003625341, -30.00000000000001066, -10.37120595110931198 ) ) ;
#77466 = EDGE_CURVE ( 'NONE', #97131, #77056, #58471, .T. ) ;
#77467 = CARTESIAN_POINT ( 'NONE',  ( -31.59843708504450532, 345.3014512875046194, 19.61421373405919510 ) ) ;
#77468 = ORIENTED_EDGE ( 'NONE', *, *, #70882, .T. ) ;
#77469 = VECTOR ( 'NONE', #55367, 1000.000000000000000 ) ;
#77470 = EDGE_LOOP ( 'NONE', ( #53914, #27280, #67366, #82234, #101589 ) ) ;
#77471 = ORIENTED_EDGE ( 'NONE', *, *, #1284, .T. ) ;
#77472 = CARTESIAN_POINT ( 'NONE',  ( -46.77752740700942979, 13.53072847091731035, -15.64014710929908780 ) ) ;
#77473 = SURFACE_SIDE_STYLE ('',( #20355 ) ) ;
#77474 = DIRECTION ( 'NONE',  ( 0.5735764363510491570, -0.8191520442889895781, 1.003171929053522035E-16 ) ) ;
#77475 = CARTESIAN_POINT ( 'NONE',  ( 4.595881407952573383, -11.06625433201323894, -3.857520671226066344 ) ) ;
#77476 = CARTESIAN_POINT ( 'NONE',  ( -17.40642114240819183, 43.24861748976680786, -6.412094953349521731 ) ) ;
#77477 = CARTESIAN_POINT ( 'NONE',  ( -7.002619243997878939, -86.05007318013817041, -3.868708944012999584 ) ) ;
#77478 = CARTESIAN_POINT ( 'NONE',  ( 50.94745919686199898, 50.00000000000000000, -37.05882352941176805 ) ) ;
#77480 = ORIENTED_EDGE ( 'NONE', *, *, #11571, .T. ) ;
#77479 = COLOUR_RGB ( '', 0.08235294, 0.09019608, 0.10196078) ;
#77481 = CARTESIAN_POINT ( 'NONE',  ( -7.374560640982810611, 50.00000000000000000, -75.40399789251387119 ) ) ;
#77482 = VERTEX_POINT ( 'NONE', #74162 ) ;
#77483 = CARTESIAN_POINT ( 'NONE',  ( 11.84999999999999787, -3.309499999999999886, 4.475777889183790779E-16 ) ) ;
#77484 = CARTESIAN_POINT ( 'NONE',  ( -41.46910480219017359, 484.7338956289797238, -3.418960549711475672 ) ) ;
#77485 = EDGE_CURVE ( 'NONE', #95526, #27550, #100039, .T. ) ;
#77486 = CARTESIAN_POINT ( 'NONE',  ( 26.59919547731570333, 296.3152804941264549, 10.25407297267763873 ) ) ;
#77487 = DIRECTION ( 'NONE',  ( -1.000000000000000000, -1.224606353822377258E-16, -0.000000000000000000 ) ) ;
#77488 = CARTESIAN_POINT ( 'NONE',  ( 59.57614690027234161, -42.96215887157280378, 72.74039141137150466 ) ) ;
#77489 = ADVANCED_FACE ( 'NONE', ( #1317 ), #34410, .F. ) ;
#77490 = ORIENTED_EDGE ( 'NONE', *, *, #97127, .F. ) ;
#77491 = CARTESIAN_POINT ( 'NONE',  ( 28.45522292534169395, 11.90502831567345865, -41.11935372236962394 ) ) ;
#77492 = CARTESIAN_POINT ( 'NONE',  ( -33.00000000000000000, 450.0000000000002274, 25.20242257375371864 ) ) ;
#77493 = CARTESIAN_POINT ( 'NONE',  ( 31.56956794793236298, 299.1326689194955861, 2.890017757335089144 ) ) ;
#77494 = AXIS2_PLACEMENT_3D ( 'NONE', #35431, #77983, #92564 ) ;
#77495 = DIRECTION ( 'NONE',  ( -1.000000000000000000, -0.000000000000000000, -0.000000000000000000 ) ) ;
#77496 = ORIENTED_EDGE ( 'NONE', *, *, #102807, .F. ) ;
#77497 = AXIS2_PLACEMENT_3D ( 'NONE', #82671, #75089, #8776 ) ;
#77498 = DIRECTION ( 'NONE',  ( 0.000000000000000000, 0.000000000000000000, 1.000000000000000000 ) ) ;
#77499 = FACE_OUTER_BOUND ( 'NONE', #89793, .T. ) ;
#77500 = SURFACE_STYLE_USAGE ( .BOTH. , #52673 ) ;
#77501 = CARTESIAN_POINT ( 'NONE',  ( 12.23754451682550481, 302.5837290440147171, 9.880035480020872285 ) ) ;
#77502 = SURFACE_STYLE_FILL_AREA ( #100692 ) ;
#77503 = CONICAL_SURFACE ( 'NONE', #65407, 5.000000000000001776, 0.9599310885968803664 ) ;
#77505 = AXIS2_PLACEMENT_3D ( 'NONE', #60108, #1274, #100524 ) ;
#77504 = CARTESIAN_POINT ( 'NONE',  ( 9.246271506234593929, 16.00000000000000000, 3.826949319562315655 ) ) ;
#77506 = CARTESIAN_POINT ( 'NONE',  ( 86.42926278269462159, -20.84806595176807775, 182.4259795259146131 ) ) ;
#77507 = DIRECTION ( 'NONE',  ( 0.000000000000000000, 0.000000000000000000, 1.000000000000000000 ) ) ;
#77508 = AXIS2_PLACEMENT_3D ( 'NONE', #46112, #94679, #36985 ) ;
#77509 = CARTESIAN_POINT ( 'NONE',  ( -8.147102310908991285, 111.6559345260855594, 5.000000000000000888 ) ) ;
#77510 = ORIENTED_EDGE ( 'NONE', *, *, #93296, .T. ) ;
#77511 = CARTESIAN_POINT ( 'NONE',  ( -7.703920929261754758, 4.447860822324860131, -7.917989418073283048 ) ) ;
#77512 =( LENGTH_UNIT ( ) NAMED_UNIT ( * ) SI_UNIT ( .MILLI., .METRE. ) );
#77513 = CARTESIAN_POINT ( 'NONE',  ( -7.036764705886677795, 40.29466777512107001, -71.06385277390548083 ) ) ;
#77514 = CARTESIAN_POINT ( 'NONE',  ( 34.36795306836310715, 436.8606731934561367, 5.945192215386652990 ) ) ;
#77515 = CARTESIAN_POINT ( 'NONE',  ( -95.80473717211435769, -30.00000000000001066, 122.9249465891220154 ) ) ;
#77516 = EDGE_CURVE ( 'NONE', #85444, #12840, #106530, .T. ) ;
#77517 = CARTESIAN_POINT ( 'NONE',  ( -1.860380241283050795, -6.431462466365337249, -0.1499059597315451076 ) ) ;
#77518 = CARTESIAN_POINT ( 'NONE',  ( 19.25747578669735560, -57.67183159647834856, 42.11888666598880349 ) ) ;
#77519 = EDGE_CURVE ( 'NONE', #54088, #10153, #86055, .T. ) ;
#77521 = CARTESIAN_POINT ( 'NONE',  ( 74.60950000000003968, 0.000000000000000000, 4.000000000000000000 ) ) ;
#77520 = DIRECTION ( 'NONE',  ( 0.000000000000000000, 0.000000000000000000, -1.000000000000000000 ) ) ;
#77522 = CARTESIAN_POINT ( 'NONE',  ( 5.918685970911453431, -50.53352564182060291, 39.68924167665423397 ) ) ;
#77523 = DIRECTION ( 'NONE',  ( 0.000000000000000000, 0.000000000000000000, 1.000000000000000000 ) ) ;
#77524 = CARTESIAN_POINT ( 'NONE',  ( -37.00811329507524761, 491.8246567885113336, 12.57632236122367431 ) ) ;
#77525 = CARTESIAN_POINT ( 'NONE',  ( 6.849999999999999645, 4.618802153517001408, -8.000000000000000000 ) ) ;
#77526 = CARTESIAN_POINT ( 'NONE',  ( 18.03091750576567165, -17.98938779324448589, -33.98685254711978843 ) ) ;
#77527 = CARTESIAN_POINT ( 'NONE',  ( -24.33670979648132260, -60.35801636503134660, 35.15369266868731302 ) ) ;
#77528 = VERTEX_POINT ( 'NONE', #82257 ) ;
#77529 = CARTESIAN_POINT ( 'NONE',  ( 9.797174393178825657E-16, -30.00000000000000000, 8.000000000000000000 ) ) ;
#77530 = CARTESIAN_POINT ( 'NONE',  ( -9.918579450955565591, 108.7930391296868891, 1.297207292923863164 ) ) ;
#77531 = CARTESIAN_POINT ( 'NONE',  ( -19.10073062131051813, -42.95807464531029041, 31.48258065302363917 ) ) ;
#77533 = CARTESIAN_POINT ( 'NONE',  ( 0.5678904221582695699, 36.34682479118509946, -29.61666878930105895 ) ) ;
#77532 = SURFACE_STYLE_FILL_AREA ( #68923 ) ;
#77534 = EDGE_CURVE ( 'NONE', #10685, #78701, #84206, .T. ) ;
#77535 = ORIENTED_EDGE ( 'NONE', *, *, #80711, .T. ) ;
#77536 = CARTESIAN_POINT ( 'NONE',  ( 6.692649149972418776, -4.003391779698783459, -6.852343209863736462 ) ) ;
#77537 = ORIENTED_EDGE ( 'NONE', *, *, #62129, .T. ) ;
#77538 = LINE ( 'NONE', #94260, #73934 ) ;
#77539 = AXIS2_PLACEMENT_3D ( 'NONE', #101130, #27290, #60173 ) ;
#77540 = CARTESIAN_POINT ( 'NONE',  ( 15.88105853605375906, 3.776612129046490907, 3.593753328290308247 ) ) ;
#77541 = EDGE_CURVE ( 'NONE', #93631, #44057, #39546, .T. ) ;
#77542 = CARTESIAN_POINT ( 'NONE',  ( 0.05613245601036488674, 1.278525034529254034, 6.499999999999999112 ) ) ;
#77543 = ORIENTED_EDGE ( 'NONE', *, *, #92073, .F. ) ;
#77544 = DIRECTION ( 'NONE',  ( -1.000000000000000000, -0.000000000000000000, -0.000000000000000000 ) ) ;
#77545 = CARTESIAN_POINT ( 'NONE',  ( 1.590636543732056207, 50.00000000000000711, -97.00013170160131892 ) ) ;
#77546 = CARTESIAN_POINT ( 'NONE',  ( 99.87804525097007513, -37.83975434610595556, 190.7999962905255416 ) ) ;
#77548 = CARTESIAN_POINT ( 'NONE',  ( -7.619753052866897747, -6.825484971928266198, -2.447276542590447246 ) ) ;
#77547 = CARTESIAN_POINT ( 'NONE',  ( 42.46716861921755282, -36.08067099156355795, 40.09748578553070075 ) ) ;
#77549 = VERTEX_POINT ( 'NONE', #90899 ) ;
#77550 = AXIS2_PLACEMENT_3D ( 'NONE', #67783, #60773, #11654 ) ;
#77551 = ORIENTED_EDGE ( 'NONE', *, *, #95294, .F. ) ;
#77552 = ORIENTED_EDGE ( 'NONE', *, *, #67729, .T. ) ;
#77553 = CARTESIAN_POINT ( 'NONE',  ( 25.61036159288622471, 308.3346455602268747, 9.743090724280190074 ) ) ;
#77554 = CIRCLE ( 'NONE', #31097, 4.000000000000000888 ) ;
#77555 = CARTESIAN_POINT ( 'NONE',  ( 32.61650669486618881, 1.474610560812782335E-15, 0.000000000000000000 ) ) ;
#77556 = CARTESIAN_POINT ( 'NONE',  ( -14.58934900096332221, 5.487773041241340799, -6.668063844691409336 ) ) ;
#77558 = ADVANCED_FACE ( 'NONE', ( #49890 ), #41272, .T. ) ;
#77557 = ORIENTED_EDGE ( 'NONE', *, *, #35028, .T. ) ;
#77559 = B_SPLINE_CURVE_WITH_KNOTS ( 'NONE', 3,
 ( #59687, #75310, #1407, #51571, #43495, #35432, #16555, #49438, #98524, #24671, #77984, #19794, #102795, #102255, #85561, #53185, #68847, #11097, #94173, #85013, #20338, #44022 ),
 .UNSPECIFIED., .F., .F.,
 ( 4, 2, 2, 2, 2, 2, 2, 2, 2, 2, 4 ),
 ( 0.000000000000000000, 0.002352169759828700267, 0.003528254639743051702, 0.004704339519657403136, 0.005292381959614579287, 0.005880424399571757173, 0.007056509279486109475, 0.007644551719443283891, 0.008232594159400459174, 0.008820636599357634458, 0.009408679039314809742 ),
 .UNSPECIFIED. ) ;
#77560 = DIRECTION ( 'NONE',  ( 1.000000000000000000, 0.000000000000000000, 0.000000000000000000 ) ) ;
#77561 = CARTESIAN_POINT ( 'NONE',  ( -5.977866729378733091, 41.99823429243535600, -69.20734196604240651 ) ) ;
#77562 = CARTESIAN_POINT ( 'NONE',  ( -81.47225727030453868, -60.00000000000972022, -29.83846400447649572 ) ) ;
#77563 = CIRCLE ( 'NONE', #53469, 17.00000000000000000 ) ;
#77564 = CARTESIAN_POINT ( 'NONE',  ( 6.928203230275506108, -65.26883324508997930, -4.000000000000002665 ) ) ;
#77565 = CARTESIAN_POINT ( 'NONE',  ( 1.494050092659831947E-08, -60.00000000000000000, -44.99999999996099120 ) ) ;
#77566 = CARTESIAN_POINT ( 'NONE',  ( 8.012433108796550130, -5.000000000000000000, 14.34039711613852575 ) ) ;
#77567 = CARTESIAN_POINT ( 'NONE',  ( -13.14242568365673414, 42.00000000000000000, -92.43215185528094935 ) ) ;
#77569 = CARTESIAN_POINT ( 'NONE',  ( 6.078557589344583789, -35.99144002894028205, 29.87849275132226623 ) ) ;
#77568 = CARTESIAN_POINT ( 'NONE',  ( -88.10255448128359035, -14.21045842199438347, 36.33746784607973268 ) ) ;
#77570 = DIRECTION ( 'NONE',  ( -0.000000000000000000, 1.000000000000000000, -0.000000000000000000 ) ) ;
#77571 = CARTESIAN_POINT ( 'NONE',  ( -48.53286934315175216, -22.21852483483064944, 43.06535966011481520 ) ) ;
#77572 = AXIS2_PLACEMENT_3D ( 'NONE', #200, #40691, #89789 ) ;
#77573 = VERTEX_POINT ( 'NONE', #26730 ) ;
#77574 = CARTESIAN_POINT ( 'NONE',  ( 26.69900261086841198, 1.482358050883964840E-15, 0.000000000000000000 ) ) ;
#77575 = VERTEX_POINT ( 'NONE', #8370 ) ;
#77576 = CARTESIAN_POINT ( 'NONE',  ( 0.3594682699208841536, 7.865263358805581362, -51.69874683107578051 ) ) ;
#77577 = DIRECTION ( 'NONE',  ( 0.000000000000000000, -1.000000000000000000, 0.000000000000000000 ) ) ;
#77578 = CIRCLE ( 'NONE', #44871, 1.000000000000000000 ) ;
#77579 = DIRECTION ( 'NONE',  ( 0.000000000000000000, -1.000000000000000000, 0.000000000000000000 ) ) ;
#77580 = ORIENTED_EDGE ( 'NONE', *, *, #74149, .F. ) ;
#77581 = SURFACE_STYLE_USAGE ( .BOTH. , #36100 ) ;
#77582 = VERTEX_POINT ( 'NONE', #41799 ) ;
#77583 = CARTESIAN_POINT ( 'NONE',  ( 83.85445948688673923, -30.00000000001250555, -22.01549710744075128 ) ) ;
#77584 =( LENGTH_UNIT ( ) NAMED_UNIT ( * ) SI_UNIT ( .MILLI., .METRE. ) );
#77585 = DIRECTION ( 'NONE',  ( 0.000000000000000000, -1.000000000000000000, 0.000000000000000000 ) ) ;
#77586 = CARTESIAN_POINT ( 'NONE',  ( 30.67950393662592745, 18.64316884711713485, 23.57730434126678887 ) ) ;
#77587 = CARTESIAN_POINT ( 'NONE',  ( 100.4840130108101590, -29.99999999999999289, 182.9441996911958199 ) ) ;
#77588 = EDGE_CURVE ( 'NONE', #87281, #104590, #92475, .T. ) ;
#77589 = CARTESIAN_POINT ( 'NONE',  ( 0.000000000000000000, 0.000000000000000000, 0.000000000000000000 ) ) ;
#77590 = ORIENTED_EDGE ( 'NONE', *, *, #56497, .T. ) ;
#77591 = VERTEX_POINT ( 'NONE', #50940 ) ;
#77592 = ORIENTED_EDGE ( 'NONE', *, *, #77415, .T. ) ;
#77593 = CARTESIAN_POINT ( 'NONE',  ( 53.88422520731434417, -39.49949140040651940, 57.94306328001776052 ) ) ;
#77594 = FACE_OUTER_BOUND ( 'NONE', #101718, .T. ) ;
#77595 = CIRCLE ( 'NONE', #48306, 0.5000000000000004441 ) ;
#77596 = CARTESIAN_POINT ( 'NONE',  ( 0.000000000000000000, 0.000000000000000000, 0.000000000000000000 ) ) ;
#77597 = ADVANCED_FACE ( 'NONE', ( #76823 ), #98106, .T. ) ;
#77598 = ORIENTED_EDGE ( 'NONE', *, *, #6324, .F. ) ;
#77599 = CARTESIAN_POINT ( 'NONE',  ( -91.30995688543926292, -38.40037703328827945, -10.42389467339130427 ) ) ;
#77600 = VERTEX_POINT ( 'NONE', #86551 ) ;
#77601 = CARTESIAN_POINT ( 'NONE',  ( -17.49999999999997513, 50.00000000000000000, -500000.0000000000582 ) ) ;
#77602 = CARTESIAN_POINT ( 'NONE',  ( 109.5686109773386079, -38.35602074723220767, 188.1120185359518189 ) ) ;
#77603 = CARTESIAN_POINT ( 'NONE',  ( 12.06580744102501157, 19.80956736058091749, 7.339492630969226106 ) ) ;
#77604 = CARTESIAN_POINT ( 'NONE',  ( 86.42441512864074582, -60.13267006415080829, 3.363400338305296167 ) ) ;
#77605 = CARTESIAN_POINT ( 'NONE',  ( 33.14123094351160859, 415.5030858634154356, 25.77660549537051082 ) ) ;
#77606 = CARTESIAN_POINT ( 'NONE',  ( 4.442085480450892909, -13.39242828886014358, -9.057376035804651337 ) ) ;
#77607 = CARTESIAN_POINT ( 'NONE',  ( 5.818834259648034468, 0.6677920147391552819, 6.499999999999999112 ) ) ;
#77608 = EDGE_CURVE ( 'NONE', #65192, #55329, #35348, .T. ) ;
#77609 = CARTESIAN_POINT ( 'NONE',  ( -44.32955949054232292, 435.2565657989985652, 11.97827722465822475 ) ) ;
#77610 = CARTESIAN_POINT ( 'NONE',  ( 7.955546711085368372, 53.39389859137057925, 5.000000000007370105 ) ) ;
#77612 = ORIENTED_EDGE ( 'NONE', *, *, #29073, .T. ) ;
#77611 =( BOUNDED_SURFACE ( )  B_SPLINE_SURFACE ( 2, 3, ( 
 ( #47817, #47296, #46254, #62972 ),
 ( #79140, #80193, #39237, #72111 ),
 ( #62445, #29061, #53801, #105020 ) ),
 .UNSPECIFIED., .F., .F., .F. ) 
 B_SPLINE_SURFACE_WITH_KNOTS ( ( 3, 3 ),
 ( 4, 4 ),
 ( 0.000000000000000000, 1.000000000000000000 ),
 ( 5.953728167561664009, 6.612642446797508455 ),
 .UNSPECIFIED. ) 
 GEOMETRIC_REPRESENTATION_ITEM ( )  RATIONAL_B_SPLINE_SURFACE ( (
 ( 1.000000000000000000, 1.000000000000000000, 1.000000000000000000, 1.000000000000000000),
 ( 1.857142857142858317, 1.857142857142858317, 1.857142857142858317, 1.857142857142858317),
 ( 1.000000000000000000, 1.000000000000000000, 1.000000000000000000, 1.000000000000000000) ) ) 
 REPRESENTATION_ITEM ( '' )  SURFACE ( )  );
#77613 = CARTESIAN_POINT ( 'NONE',  ( 6.162888688655344005, 3.752776749732565253, 6.499999999999997335 ) ) ;
#77614 = CARTESIAN_POINT ( 'NONE',  ( 7.500000000000005329, 40.00000000029777425, -69.29143158580563977 ) ) ;
#77615 = VECTOR ( 'NONE', #8188, 1000.000000000000227 ) ;
#77616 = DIRECTION ( 'NONE',  ( -1.000000000000000000, 0.000000000000000000, 0.000000000000000000 ) ) ;
#77617 = EDGE_LOOP ( 'NONE', ( #15947, #33189, #45865, #23695 ) ) ;
#77618 = CARTESIAN_POINT ( 'NONE',  ( -21.70127168875638546, 305.0664967217661001, -8.954259079442119074 ) ) ;
#77619 = CARTESIAN_POINT ( 'NONE',  ( -36.73440919039663299, 310.3360335768772416, 13.64782109026154977 ) ) ;
#77620 = CARTESIAN_POINT ( 'NONE',  ( 1.078140322363270668E-05, -30.00000000000000000, 28.88964995960238014 ) ) ;
#77621 =( NAMED_UNIT ( * ) SI_UNIT ( $, .STERADIAN. ) SOLID_ANGLE_UNIT ( ) );
#77622 = CARTESIAN_POINT ( 'NONE',  ( 4.898587196589412829E-16, -21.12499999999999289, -8.000000000000000000 ) ) ;
#77623 = CARTESIAN_POINT ( 'NONE',  ( 21.54994887520524216, -17.71005473222516002, 31.43420972831726701 ) ) ;
#77624 = FACE_OUTER_BOUND ( 'NONE', #33344, .T. ) ;
#77625 = ORIENTED_EDGE ( 'NONE', *, *, #47201, .F. ) ;
#77626 = CARTESIAN_POINT ( 'NONE',  ( 85.13153603772909150, -35.77587323764717553, 181.7315888882555441 ) ) ;
#77627 = SURFACE_SIDE_STYLE ('',( #100295 ) ) ;
#77628 = CARTESIAN_POINT ( 'NONE',  ( -16.64348903516517098, 45.88445698070336221, 4.157797401561652784 ) ) ;
#77629 = VERTEX_POINT ( 'NONE', #94081 ) ;
#77630 = CARTESIAN_POINT ( 'NONE',  ( -95.54514223258487959, -52.71027819635147438, 96.31137204281640152 ) ) ;
#77631 = CARTESIAN_POINT ( 'NONE',  ( 7.470345474798855081E-15, 44.00000000000000711, -61.00000000000000000 ) ) ;
#77632 = CARTESIAN_POINT ( 'NONE',  ( -12.12626197892902269, -5.000000000002062350, -94.24800833403607214 ) ) ;
#77633 = CARTESIAN_POINT ( 'NONE',  ( 0.000000000000000000, 0.000000000000000000, -9.274828571428571422 ) ) ;
#77634 = CARTESIAN_POINT ( 'NONE',  ( 6.162888688655344005, 3.752776749732561257, -6.499999999999999112 ) ) ;
#77635 = AXIS2_PLACEMENT_3D ( 'NONE', #874, #33851, #43515 ) ;
#77636 = EDGE_CURVE ( 'NONE', #20792, #91765, #15500, .T. ) ;
#77637 = B_SPLINE_CURVE_WITH_KNOTS ( 'NONE', 3,
 ( #31015, #40654, #63893, #14777 ),
 .UNSPECIFIED., .F., .F.,
 ( 4, 4 ),
 ( 0.000000000000000000, 0.003416952886430368354 ),
 .UNSPECIFIED. ) ;
#77638 = VECTOR ( 'NONE', #41290, 1000.000000000000114 ) ;
#77639 = CARTESIAN_POINT ( 'NONE',  ( 25.49733103399898937, -59.99999999999998579, 41.30705873576198428 ) ) ;
#77640 = DIRECTION ( 'NONE',  ( -1.000000000000000000, -0.000000000000000000, -0.000000000000000000 ) ) ;
#77641 = CIRCLE ( 'NONE', #48363, 4.000000000000000888 ) ;
#77642 = CARTESIAN_POINT ( 'NONE',  ( 0.9999999999999941158, -1.734723475976807094E-15, 101.0455488498966758 ) ) ;
#77643 = CARTESIAN_POINT ( 'NONE',  ( 50.71626818303565898, -29.81274633916111938, 47.79517027631969484 ) ) ;
#77644 = EDGE_CURVE ( 'NONE', #11338, #2153, #57635, .T. ) ;
#77646 = CARTESIAN_POINT ( 'NONE',  ( -10.23422886744656068, 16.30953289564795483, 10.09620275774212139 ) ) ;
#77645 = CARTESIAN_POINT ( 'NONE',  ( 33.00000000000000000, 435.0774731480752280, 11.67986145722084501 ) ) ;
#77647 = CIRCLE ( 'NONE', #44936, 4.000000000000000888 ) ;
#77648 = CARTESIAN_POINT ( 'NONE',  ( 7.416584036454647588, 294.7171783682853743, -6.719350101588912771 ) ) ;
#77649 = CARTESIAN_POINT ( 'NONE',  ( 27.47093694407817210, 296.2799286419132727, -9.692114557243211692 ) ) ;
#77650 = CARTESIAN_POINT ( 'NONE',  ( 37.75894927425606085, 307.4551686108193849, 0.9580216366009680629 ) ) ;
#77651 = FACE_OUTER_BOUND ( 'NONE', #1824, .T. ) ;
#77652 = CARTESIAN_POINT ( 'NONE',  ( 5.819846122303830249, 6.321060697774945503, -2.051601713727019494 ) ) ;
#77653 = VERTEX_POINT ( 'NONE', #61739 ) ;
#77654 = CARTESIAN_POINT ( 'NONE',  ( -23.21751746555244722, 28.11705169068991594, 30.70617127781060418 ) ) ;
#77655 = PRODUCT_DEFINITION_SHAPE ( 'NONE', 'NONE',  #106792 ) ;
#77656 = CARTESIAN_POINT ( 'NONE',  ( -17.49999999999997158, 51.95328275803299789, 61.04403218099716355 ) ) ;
#77657 = EDGE_LOOP ( 'NONE', ( #101449, #82243 ) ) ;
#77658 = CARTESIAN_POINT ( 'NONE',  ( -8.953164881677507125, -1.467082799477942734, 15.49915330648462231 ) ) ;
#77659 = DIRECTION ( 'NONE',  ( 0.8191520442889884679, 0.000000000000000000, 0.5735764363510508224 ) ) ;
#77660 = DIRECTION ( 'NONE',  ( 1.000000000000000000, 1.224606353822377258E-16, 0.000000000000000000 ) ) ;
#77662 = CARTESIAN_POINT ( 'NONE',  ( 3.170868525710598185, -47.40887100352247785, -34.77119744858119788 ) ) ;
#77661 = CARTESIAN_POINT ( 'NONE',  ( 9.989435848181802413, 253.9738029252842182, -0.5278651953176168865 ) ) ;
#77663 = EDGE_CURVE ( 'NONE', #55140, #41735, #74006, .T. ) ;
#77664 = ORIENTED_EDGE ( 'NONE', *, *, #20965, .T. ) ;
#77665 =( GEOMETRIC_REPRESENTATION_CONTEXT ( 3 ) GLOBAL_UNCERTAINTY_ASSIGNED_CONTEXT ( ( #81727 ) ) GLOBAL_UNIT_ASSIGNED_CONTEXT ( ( #78317, #23838, #88545 ) ) REPRESENTATION_CONTEXT ( 'NONE', 'WORKASPACE' ) );
#77666 = CARTESIAN_POINT ( 'NONE',  ( 0.000000000000000000, 0.000000000000000000, -25.03750572909317285 ) ) ;
#77667 = FILL_AREA_STYLE_COLOUR ( '', #78946 ) ;
#77668 = VERTEX_POINT ( 'NONE', #45020 ) ;
#77669 = VECTOR ( 'NONE', #21349, 1000.000000000000114 ) ;
#77670 = CARTESIAN_POINT ( 'NONE',  ( -7.000000000000000000, 8.572527594031473190E-16, -6.275264681066861527 ) ) ;
#77671 = AXIS2_PLACEMENT_3D ( 'NONE', #32121, #71494, #31087 ) ;
#77672 = DIRECTION ( 'NONE',  ( -1.000000000000000000, -1.224606353822377258E-16, -0.000000000000000000 ) ) ;
#77673 = CARTESIAN_POINT ( 'NONE',  ( -92.23484866504666968, -60.00000000000000000, 2.411054607516263992 ) ) ;
#77674 = ORIENTED_EDGE ( 'NONE', *, *, #37496, .T. ) ;
#77675 = CARTESIAN_POINT ( 'NONE',  ( 1.797870618340624782, 41.33266196706066609, -58.72278032361231936 ) ) ;
#77676 = DIRECTION ( 'NONE',  ( -1.000000000000000000, -1.224606353822377258E-16, -0.000000000000000000 ) ) ;
#77677 = DIRECTION ( 'NONE',  ( 0.000000000000000000, 0.000000000000000000, 1.000000000000000000 ) ) ;
#77679 = CARTESIAN_POINT ( 'NONE',  ( -9.381593208289377372, 27.98561361880494047, -3.465401811657804476 ) ) ;
#77678 =( REPRESENTATION_RELATIONSHIP ('NONE','NONE', #69581, #22031 ) REPRESENTATION_RELATIONSHIP_WITH_TRANSFORMATION ( #54529 )SHAPE_REPRESENTATION_RELATIONSHIP( ) );
#77680 = DIRECTION ( 'NONE',  ( 0.000000000000000000, 0.000000000000000000, 1.000000000000000000 ) ) ;
#77681 = CARTESIAN_POINT ( 'NONE',  ( -82.61596774746847416, -39.49479684367577903, 166.2316737952538688 ) ) ;
#77682 = ORIENTED_EDGE ( 'NONE', *, *, #65720, .F. ) ;
#77683 = CARTESIAN_POINT ( 'NONE',  ( -16.90642566761263410, 0.000000000000000000, 2.220638482676595693 ) ) ;
#77684 = VERTEX_POINT ( 'NONE', #43935 ) ;
#77685 = VERTEX_POINT ( 'NONE', #84930 ) ;
#77686 = CARTESIAN_POINT ( 'NONE',  ( -16.64670748671521494, -5.000000000000000000, -1.019662339604523460 ) ) ;
#77687 = CARTESIAN_POINT ( 'NONE',  ( -2.669532029060316614, -70.32879813054786666, 13.25462063025687165 ) ) ;
#77688 = VERTEX_POINT ( 'NONE', #69293 ) ;
#77689 = VECTOR ( 'NONE', #25898, 1000.000000000000000 ) ;
#77690 = SURFACE_SIDE_STYLE ('',( #44801 ) ) ;
#77691 = CARTESIAN_POINT ( 'NONE',  ( -87.28812347660355897, -57.67005709194983609, -25.16891244813248818 ) ) ;
#77692 = CARTESIAN_POINT ( 'NONE',  ( -5.476751506168961114, -68.16357122866992313, -2.461144630687911228 ) ) ;
#77693 = LINE ( 'NONE', #3802, #16914 ) ;
#77694 = CARTESIAN_POINT ( 'NONE',  ( -9.165151389911679658, 105.0000000000000000, 4.000000000000001776 ) ) ;
#77695 = FILL_AREA_STYLE ('',( #36744 ) ) ;
#77696 = DIRECTION ( 'NONE',  ( 0.000000000000000000, 1.000000000000000000, -1.224646799147353207E-16 ) ) ;
#77697 = CARTESIAN_POINT ( 'NONE',  ( 94.33250250775739687, -60.00000000000007105, 18.12814013139226077 ) ) ;
#77698 = CARTESIAN_POINT ( 'NONE',  ( -78.26172670240529783, -14.21045842199445275, 161.8221046207387985 ) ) ;
#77699 = CARTESIAN_POINT ( 'NONE',  ( -57.60680526892024744, -18.66794027853511295, 57.28622852526675047 ) ) ;
#77700 = ORIENTED_EDGE ( 'NONE', *, *, #51806, .T. ) ;
#77701 =( NAMED_UNIT ( * ) SI_UNIT ( $, .STERADIAN. ) SOLID_ANGLE_UNIT ( ) );
#77702 = ORIENTED_EDGE ( 'NONE', *, *, #16330, .F. ) ;
#77703 = CARTESIAN_POINT ( 'NONE',  ( -103.3338068315771210, -45.26544286762020874, 183.6154355829563372 ) ) ;
#77704 = CARTESIAN_POINT ( 'NONE',  ( -89.99999999999997158, -52.00000000000000000, 196.0238439516549818 ) ) ;
#77705 = LINE ( 'NONE', #3283, #61569 ) ;
#77706 = ORIENTED_EDGE ( 'NONE', *, *, #85574, .T. ) ;
#77707 = CARTESIAN_POINT ( 'NONE',  ( 9.500000025475724641, -4.999999999999998224, -69.85526497429231085 ) ) ;
#77708 = SURFACE_STYLE_FILL_AREA ( #103566 ) ;
#77709 = CARTESIAN_POINT ( 'NONE',  ( 36.35284819509398346, 26.07822863538820002, -11.89625673952615159 ) ) ;
#77710 = CARTESIAN_POINT ( 'NONE',  ( 5.082755093536324154, -16.71875000204838813, 5.082755093536326818 ) ) ;
#77711 = CIRCLE ( 'NONE', #51821, 5.000000000000000000 ) ;
#77712 = CARTESIAN_POINT ( 'NONE',  ( -1.128077836147719282, 302.8478239976500390, 9.936168295454388399 ) ) ;
#77713 = DIRECTION ( 'NONE',  ( -1.000000000000000000, -1.224606353822377258E-16, -0.000000000000000000 ) ) ;
#77714 = CARTESIAN_POINT ( 'NONE',  ( -20.97754405179121662, 294.8763868968453608, 9.942224931492262385 ) ) ;
#77715 = AXIS2_PLACEMENT_3D ( 'NONE', #81684, #65534, #749 ) ;
#77716 = DIRECTION ( 'NONE',  ( -1.000000000000000000, -0.000000000000000000, -0.000000000000000000 ) ) ;
#77717 = CARTESIAN_POINT ( 'NONE',  ( -8.383456159752070036, 30.02471915937834623, -0.000000000000000000 ) ) ;
#77718 = CARTESIAN_POINT ( 'NONE',  ( -15.55855383130854364, 46.20420475984592201, -4.781350493801898693 ) ) ;
#77719 = EDGE_CURVE ( 'NONE', #7464, #56846, #63723, .T. ) ;
#77720 = CARTESIAN_POINT ( 'NONE',  ( 8.099999999999999645, 7.505553499465140277, 0.000000000000000000 ) ) ;
#77721 = CARTESIAN_POINT ( 'NONE',  ( -27.52811649691203755, -60.34835150324916242, 35.96130197689507924 ) ) ;
#77722 = EDGE_CURVE ( 'NONE', #7253, #48079, #96437, .T. ) ;
#77723 = LINE ( 'NONE', #69109, #105859 ) ;
#77724 = CARTESIAN_POINT ( 'NONE',  ( 47.01846914081971107, -42.98288543070874823, 47.24321920347014725 ) ) ;
#77725 = VERTEX_POINT ( 'NONE', #85464 ) ;
#77726 = CARTESIAN_POINT ( 'NONE',  ( -32.62589942841216128, 485.9514140855798132, 7.203752716014093060 ) ) ;
#77727 = CARTESIAN_POINT ( 'NONE',  ( 1.990040563172386960E-15, 46.21383923812596350, 16.25000000000000000 ) ) ;
#77728 = EDGE_CURVE ( 'NONE', #64513, #34348, #10335, .T. ) ;
#77729 = AXIS2_PLACEMENT_3D ( 'NONE', #23126, #48422, #89438 ) ;
#77730 = CARTESIAN_POINT ( 'NONE',  ( -87.32121499277974408, -38.58266683294037591, 199.6815565422783152 ) ) ;
#77731 = ORIENTED_EDGE ( 'NONE', *, *, #20001, .F. ) ;
#77732 = CARTESIAN_POINT ( 'NONE',  ( -4.250000000000000000, 5.204748896376250699E-16, -4.814498510800145681 ) ) ;
#77733 = CARTESIAN_POINT ( 'NONE',  ( 14.11595029532510992, 2.410436752314608633, -5.024000119269073750 ) ) ;
#77734 = CARTESIAN_POINT ( 'NONE',  ( -18.91765097186078748, 48.32803790483924899, 62.18241277266358935 ) ) ;
#77735 = CARTESIAN_POINT ( 'NONE',  ( 23.58349330513380337, 1.593028355512270567E-15, 0.000000000000000000 ) ) ;
#77736 = CARTESIAN_POINT ( 'NONE',  ( 6.422424208505636223, 41.30029441423581460, -70.89074253712280438 ) ) ;
#77737 = ADVANCED_FACE ( 'NONE', ( #20781 ), #60674, .F. ) ;
#77738 = CARTESIAN_POINT ( 'NONE',  ( -31.03678703374864156, 438.6650838204933507, 21.86890379898568426 ) ) ;
#77739 = CARTESIAN_POINT ( 'NONE',  ( 4.999999999999999112, -53.41517366205636108, 9.165057039496462110 ) ) ;
#77740 = CARTESIAN_POINT ( 'NONE',  ( 7.500000000000000888, -2.886751345948136205, -7.198902722707429369 ) ) ;
#77741 = CARTESIAN_POINT ( 'NONE',  ( 108.8449848764237373, -60.00000000000002132, 194.0276147426650653 ) ) ;
#77742 = EDGE_CURVE ( 'NONE', #74990, #96186, #76958, .T. ) ;
#77743 = CARTESIAN_POINT ( 'NONE',  ( 43.10000000000000142, 1.533819458162526451E-15, 0.000000000000000000 ) ) ;
#77744 = VERTEX_POINT ( 'NONE', #71381 ) ;
#77745 = CONICAL_SURFACE ( 'NONE', #50164, 4.000000000000001776, 0.9599310885968774798 ) ;
#77746 = CARTESIAN_POINT ( 'NONE',  ( -81.42503152479930861, -30.00000000000000000, -2.337591129561404912 ) ) ;
#77747 = EDGE_LOOP ( 'NONE', ( #92069, #4727, #61371, #66279 ) ) ;
#77748 = CARTESIAN_POINT ( 'NONE',  ( 5.183352296222792255, 2.622636543482688154, -23.48691144851825996 ) ) ;
#77749 = CARTESIAN_POINT ( 'NONE',  ( 12.48579759839974734, -3.547635786644434575, -13.69895377872215114 ) ) ;
#77750 = CARTESIAN_POINT ( 'NONE',  ( 6.162888688655347558, -7.505553499465142053, -3.129864801432410934E-16 ) ) ;
#77751 = CARTESIAN_POINT ( 'NONE',  ( 7.188101187500001821, -13.43750000204838457, -2.977408999572650483 ) ) ;
#77752 = AXIS2_PLACEMENT_3D ( 'NONE', #31818, #17231, #56591 ) ;
#77753 = CARTESIAN_POINT ( 'NONE',  ( 9.596002107491598210, -5.000000000000002665, -92.37456064098007857 ) ) ;
#77754 = TOROIDAL_SURFACE ( 'NONE', #65727, 74.46152422706630603, 68.00000000000000000 ) ;
#77755 = FACE_OUTER_BOUND ( 'NONE', #95489, .T. ) ;
#77757 = EDGE_LOOP ( 'NONE', ( #25448, #103027, #74075, #95886 ) ) ;
#77756 = CARTESIAN_POINT ( 'NONE',  ( -32.95589646111131543, 464.8957215206405067, 10.75300444715554171 ) ) ;
#77758 = CARTESIAN_POINT ( 'NONE',  ( 84.97744274634288786, -25.49365950938402037, 166.4570684673164749 ) ) ;
#77759 = CARTESIAN_POINT ( 'NONE',  ( -3.963177594439675655, -1.288758772720862256, 103.9032426698856995 ) ) ;
#77760 = CARTESIAN_POINT ( 'NONE',  ( 9.165151389911679658, 85.26710781282915264, -4.000000000000000000 ) ) ;
#77761 = ORIENTED_EDGE ( 'NONE', *, *, #42293, .F. ) ;
#77762 = CARTESIAN_POINT ( 'NONE',  ( -20.87150057907853551, 302.8935307529103511, -9.991130529295787710 ) ) ;
#77763 = SURFACE_STYLE_FILL_AREA ( #85876 ) ;
#77764 = CARTESIAN_POINT ( 'NONE',  ( 0.000000000000000000, 0.000000000000000000, 0.000000000000000000 ) ) ;
#77765 = CARTESIAN_POINT ( 'NONE',  ( -29.14573983020256520, 13.65694994997194023, -39.72476874530827473 ) ) ;
#77766 = CARTESIAN_POINT ( 'NONE',  ( -42.59614121018025656, 472.7198067255875458, 11.67823714611271768 ) ) ;
#77767 = ORIENTED_EDGE ( 'NONE', *, *, #36452, .T. ) ;
#77768 = EDGE_CURVE ( 'NONE', #29102, #21068, #58553, .T. ) ;
#77769 = AXIS2_PLACEMENT_3D ( 'NONE', #4110, #54220, #38614 ) ;
#77770 = CARTESIAN_POINT ( 'NONE',  ( -4.324913936355902599, -48.88822604074822920, 104.4044995709990076 ) ) ;
#77772 = FACE_OUTER_BOUND ( 'NONE', #85585, .T. ) ;
#77771 = SHAPE_REPRESENTATION ( 'hex bolt gradeab_din_DIN EN 24014 - M8 x 70 x 22-S', ( #10728 ), #66175 ) ;
#77773 = DIRECTION ( 'NONE',  ( 0.000000000000000000, 0.000000000000000000, -1.000000000000000000 ) ) ;
#77774 = EDGE_CURVE ( 'NONE', #72013, #14549, #73103, .T. ) ;
#77775 = ADVANCED_FACE ( 'NONE', ( #7176 ), #22875, .F. ) ;
#77777 = CARTESIAN_POINT ( 'NONE',  ( -43.55054245096678756, 486.2288135416363275, 8.070792277557934824 ) ) ;
#77776 = CARTESIAN_POINT ( 'NONE',  ( 45.59999999999999432, 1.533819458162526451E-15, 0.000000000000000000 ) ) ;
#77778 = CARTESIAN_POINT ( 'NONE',  ( 2.977408999572650927, -24.87500000204838457, -7.188101187500001821 ) ) ;
#77779 = CARTESIAN_POINT ( 'NONE',  ( -30.00000000000000000, 488.8442721620238558, 4.433647275927475206 ) ) ;
#77780 = FACE_OUTER_BOUND ( 'NONE', #89983, .T. ) ;
#77781 = CARTESIAN_POINT ( 'NONE',  ( 6.061707334725029206, -5.000000000000000000, -95.47772246152658226 ) ) ;
#77782 = EDGE_LOOP ( 'NONE', ( #9748, #31499, #100315, #89806 ) ) ;
#77783 = CIRCLE ( 'NONE', #31302, 5.000000000000001776 ) ;
#77784 = AXIS2_PLACEMENT_3D ( 'NONE', #91561, #73756, #17668 ) ;
#77785 = CYLINDRICAL_SURFACE ( 'NONE', #99116, 4.000000000000000000 ) ;
#77786 = CARTESIAN_POINT ( 'NONE',  ( 40.11650669486618881, 1.474610560812782335E-15, 0.000000000000000000 ) ) ;
#77787 = PRESENTATION_LAYER_ASSIGNMENT (  '', '', ( #60640 ) ) ;
#77788 = CARTESIAN_POINT ( 'NONE',  ( -9.832775748058654841, 7.875845744486726474, -5.000000000000000888 ) ) ;
#77789 = CARTESIAN_POINT ( 'NONE',  ( 38.58349330513380693, 4.000000000000002665, 0.000000000000000000 ) ) ;
#77790 = EDGE_CURVE ( 'NONE', #37936, #98735, #1708, .T. ) ;
#77791 = ORIENTED_EDGE ( 'NONE', *, *, #31487, .F. ) ;
#77792 = FACE_OUTER_BOUND ( 'NONE', #93556, .T. ) ;
#77793 = ORIENTED_EDGE ( 'NONE', *, *, #40757, .T. ) ;
#77794 = ADVANCED_FACE ( 'NONE', ( #103762 ), #75784, .F. ) ;
#77795 = LINE ( 'NONE', #45435, #40261 ) ;
#77796 = CARTESIAN_POINT ( 'NONE',  ( -0.1556861026017113125, 7.763710170093361285, -51.74238828694827674 ) ) ;
#77797 = CARTESIAN_POINT ( 'NONE',  ( 9.176645556628256983, 104.4726096759327021, 3.973966573947712799 ) ) ;
#77798 = CARTESIAN_POINT ( 'NONE',  ( -109.1326555875536286, -60.00000000000000000, 193.4862587518598502 ) ) ;
#77799 = CARTESIAN_POINT ( 'NONE',  ( 28.09999999999999787, 1.533819458162526451E-15, 0.000000000000000000 ) ) ;
#77800 = CARTESIAN_POINT ( 'NONE',  ( 6.289692432696789126, 0.6629690750393447685, 6.828989928337166226 ) ) ;
#77801 = CARTESIAN_POINT ( 'NONE',  ( 5.931261341847957169, 53.39841463849090530, -8.357466982193816563 ) ) ;
#77802 = EDGE_CURVE ( 'NONE', #31379, #6418, #39577, .T. ) ;
#77803 = CARTESIAN_POINT ( 'NONE',  ( 17.89153430032353143, 34.22757668435322387, -23.57710181514798009 ) ) ;
#77804 = CARTESIAN_POINT ( 'NONE',  ( -84.24460074213088490, -39.43037569060520298, 179.9152917709095050 ) ) ;
#77805 = CARTESIAN_POINT ( 'NONE',  ( 49.07844914649123069, 40.91359446734409744, -43.02828753854897315 ) ) ;
#77806 = ORIENTED_EDGE ( 'NONE', *, *, #2365, .T. ) ;
#77807 = CARTESIAN_POINT ( 'NONE',  ( -16.83213846691014126, 302.5742749712027262, 9.878299602143622238 ) ) ;
#77808 = CARTESIAN_POINT ( 'NONE',  ( 0.9999999999999997780, -26.91905550219523846, -6.087553237117470317 ) ) ;
#77809 = CARTESIAN_POINT ( 'NONE',  ( -86.38463748994981017, -60.13544983588694492, 4.008287378961288283 ) ) ;
#77810 = AXIS2_PLACEMENT_3D ( 'NONE', #1101, #19501, #9739 ) ;
#77811 = B_SPLINE_CURVE_WITH_KNOTS ( 'NONE', 3,
 ( #20089, #29758, #69137, #95520 ),
 .UNSPECIFIED., .F., .F.,
 ( 4, 4 ),
 ( 0.000000000000000000, 0.002118337988235547299 ),
 .UNSPECIFIED. ) ;
#77812 = CARTESIAN_POINT ( 'NONE',  ( -32.10528697966012857, 486.1671898930081852, 5.449875171704860577 ) ) ;
#77813 = CARTESIAN_POINT ( 'NONE',  ( -3.293703171889100112, 33.36073719191674058, -5.000000000000000000 ) ) ;
#77814 = AXIS2_PLACEMENT_3D ( 'NONE', #80084, #64457, #7254 ) ;
#77815 = CARTESIAN_POINT ( 'NONE',  ( 9.517802786884892896, 142.5467050669339528, -5.000000000000310862 ) ) ;
#77816 = DIRECTION ( 'NONE',  ( -1.000000000000000000, -0.000000000000000000, -0.000000000000000000 ) ) ;
#77817 = CARTESIAN_POINT ( 'NONE',  ( 37.36680950585426331, 18.64316884707256605, -10.04205104291870398 ) ) ;
#77818 = CARTESIAN_POINT ( 'NONE',  ( 67.17255777190595722, -60.00000000000001421, 138.9727001947898941 ) ) ;
#77819 = CARTESIAN_POINT ( 'NONE',  ( -9.993576133260314080E-16, 61.49999999999999289, 8.160374191332742555 ) ) ;
#77820 = CARTESIAN_POINT ( 'NONE',  ( -86.89976874444957389, -30.00000000000007105, -18.81729257278660583 ) ) ;
#77821 = MECHANICAL_DESIGN_GEOMETRIC_PRESENTATION_REPRESENTATION (  '', ( #24499 ), #317 ) ;
#77822 = CARTESIAN_POINT ( 'NONE',  ( -63.37298395216151192, -49.91547941956211787, 86.82718669228569297 ) ) ;
#77823 = VERTEX_POINT ( 'NONE', #47103 ) ;
#77824 = CARTESIAN_POINT ( 'NONE',  ( 94.89952817683000319, -60.00000000000002842, 205.0337064426678921 ) ) ;
#77825 = CARTESIAN_POINT ( 'NONE',  ( 56.10245818848532195, 40.83957962279791332, -33.37187160345136050 ) ) ;
#77826 = CARTESIAN_POINT ( 'NONE',  ( 57.00552557303263512, -57.67115621451332430, -38.41573049067468304 ) ) ;
#77827 = ORIENTED_EDGE ( 'NONE', *, *, #63856, .F. ) ;
#77828 = CARTESIAN_POINT ( 'NONE',  ( 13.38886880393120116, -54.52389483426509287, 31.09159242423791270 ) ) ;
#77829 = CARTESIAN_POINT ( 'NONE',  ( -5.082755093536325042, -24.96875000204838813, -5.082755093536325930 ) ) ;
#77830 = CARTESIAN_POINT ( 'NONE',  ( -0.7828025612222084817, 28.10837865791959800, -38.51177607868886810 ) ) ;
#77831 = ORIENTED_EDGE ( 'NONE', *, *, #70730, .F. ) ;
#77832 = FILL_AREA_STYLE_COLOUR ( '', #61374 ) ;
#77833 = ORIENTED_EDGE ( 'NONE', *, *, #34685, .T. ) ;
#77834 = CARTESIAN_POINT ( 'NONE',  ( 0.000000000000000000, -1.200000000000000030E-05, 18.75000000000000355 ) ) ;
#77835 = CARTESIAN_POINT ( 'NONE',  ( -71.42284278233368866, -60.00000000000001421, -32.04182544189346515 ) ) ;
#77836 = CARTESIAN_POINT ( 'NONE',  ( -11.52585092648323162, 43.45746737603746368, 13.79532806417373614 ) ) ;
#77837 = CARTESIAN_POINT ( 'NONE',  ( 2.977408999572650927, -31.25000000204838813, -7.188101187500001821 ) ) ;
#77838 = CARTESIAN_POINT ( 'NONE',  ( 61.85555555555556140, 3.309500000000014541, 0.000000000000000000 ) ) ;
#77839 = CARTESIAN_POINT ( 'NONE',  ( 24.41571844174603356, -4.285714285714296246, 6.539732759932823214 ) ) ;
#77840 = CARTESIAN_POINT ( 'NONE',  ( 1.570796324976846403, 50.00000000000000000, -73.00000000000001421 ) ) ;
#77841 = CARTESIAN_POINT ( 'NONE',  ( -7.550180524134848525, 108.0055924721318519, 2.651855549982493176 ) ) ;
#77842 = CARTESIAN_POINT ( 'NONE',  ( 41.81614247337357426, 436.2534677952791640, 7.171297734017413106 ) ) ;
#77843 = EDGE_CURVE ( 'NONE', #21702, #73045, #24080, .T. ) ;
#77844 = EDGE_LOOP ( 'NONE', ( #45184, #58701, #75604, #64887, #89346, #79560 ) ) ;
#77846 = CARTESIAN_POINT ( 'NONE',  ( 32.39821730551995671, -25.61740565494374167, 31.48411120452532330 ) ) ;
#77845 = CARTESIAN_POINT ( 'NONE',  ( 4.512137457764992199, 52.17996906692113157, -6.299107601609536644 ) ) ;
#77847 = CARTESIAN_POINT ( 'NONE',  ( 24.56594385547636605, -4.285714285715934047, 6.601913983210457637 ) ) ;
#77848 = ORIENTED_EDGE ( 'NONE', *, *, #34229, .T. ) ;
#77849 = EDGE_CURVE ( 'NONE', #102936, #8913, #51608, .T. ) ;
#77850 = CARTESIAN_POINT ( 'NONE',  ( -22.57862130244024002, 26.07716137114785226, -30.87848508644228929 ) ) ;
#77851 = EDGE_CURVE ( 'NONE', #12410, #17858, #15278, .T. ) ;
#77852 = CARTESIAN_POINT ( 'NONE',  ( 6.602753909532903975, 5.319290460493536266, -7.792447862505333056 ) ) ;
#77853 = CARTESIAN_POINT ( 'NONE',  ( 19.83349330513380693, 1.593028355512270962E-15, 0.000000000000000000 ) ) ;
#77854 = DIRECTION ( 'NONE',  ( -1.000000000000000000, -1.224606353822377258E-16, -0.000000000000000000 ) ) ;
#77855 = SURFACE_STYLE_USAGE ( .BOTH. , #87027 ) ;
#77856 = FILL_AREA_STYLE ('',( #63275 ) ) ;
#77857 = CARTESIAN_POINT ( 'NONE',  ( -16.14595037822608248, 20.23371447308014481, 4.922994507609256054 ) ) ;
#77858 = FACE_OUTER_BOUND ( 'NONE', #29197, .T. ) ;
#77859 = ORIENTED_EDGE ( 'NONE', *, *, #47430, .F. ) ;
#77860 = CARTESIAN_POINT ( 'NONE',  ( 91.87201142978150870, -60.00000000000000000, 10.31812443270822222 ) ) ;
#77861 = CYLINDRICAL_SURFACE ( 'NONE', #80818, 4.250000000000000000 ) ;
#77862 = B_SPLINE_CURVE_WITH_KNOTS ( 'NONE', 3,
 ( #9833, #92347, #41159, #60027, #74042, #67034 ),
 .UNSPECIFIED., .F., .F.,
 ( 4, 2, 4 ),
 ( 0.003841072314098320766, 0.005765657563962173389, 0.007690242813826025578 ),
 .UNSPECIFIED. ) ;
#77864 = CARTESIAN_POINT ( 'NONE',  ( 5.691929483231185749, -5.629165124598853431, 3.250000000000002220 ) ) ;
#77863 = AXIS2_PLACEMENT_3D ( 'NONE', #36286, #5463, #28716 ) ;
#77865 = EDGE_CURVE ( 'NONE', #2886, #70854, #23398, .T. ) ;
#77866 = CARTESIAN_POINT ( 'NONE',  ( -35.73766838807912904, 382.4801828565075539, 5.056470275602615416 ) ) ;
#77867 = EDGE_CURVE ( 'NONE', #65549, #90138, #34485, .T. ) ;
#77868 = CIRCLE ( 'NONE', #3794, 6.000000000000000888 ) ;
#77869 = CARTESIAN_POINT ( 'NONE',  ( -7.036764705886677795, 40.29466777512107001, -71.06385277390548083 ) ) ;
#77870 = DIRECTION ( 'NONE',  ( -0.5735764363510497121, 0.8191520442889892450, 1.003171929053521665E-16 ) ) ;
#77871 = ORIENTED_EDGE ( 'NONE', *, *, #98165, .F. ) ;
#77872 = CARTESIAN_POINT ( 'NONE',  ( -84.78418355050577304, -30.00000000000874678, 197.0029753287615222 ) ) ;
#77873 = ORIENTED_EDGE ( 'NONE', *, *, #42349, .F. ) ;
#77874 = CARTESIAN_POINT ( 'NONE',  ( -9.728434877168217199, -57.17846926216942194, 24.67462639010848946 ) ) ;
#77875 = FILL_AREA_STYLE ('',( #44990 ) ) ;
#77876 = CARTESIAN_POINT ( 'NONE',  ( 0.000000000000000000, 0.000000000000000000, -6.800000000000000711 ) ) ;
#77877 = CARTESIAN_POINT ( 'NONE',  ( 16.11139379967212548, 21.68073351270184546, -1.735103873172237465 ) ) ;
#77878 = CARTESIAN_POINT ( 'NONE',  ( 82.82716448943715193, -37.79852848148829025, -11.55289307985657210 ) ) ;
#77879 = CIRCLE ( 'NONE', #31391, 0.5000000000000004441 ) ;
#77880 = CARTESIAN_POINT ( 'NONE',  ( 4.401442555609581635E-16, -31.15625000204838813, -7.188101187500000044 ) ) ;
#77881 = CARTESIAN_POINT ( 'NONE',  ( -17.78094014186206095, 45.00000000000000000, 62.75731298173543848 ) ) ;
#77882 = CARTESIAN_POINT ( 'NONE',  ( 72.50181414422412729, -37.99999999999997868, -21.26202816386757277 ) ) ;
#77883 = VERTEX_POINT ( 'NONE', #56239 ) ;
#77884 = PRESENTATION_STYLE_ASSIGNMENT (( #62253 ) ) ;
#77885 = ORIENTED_EDGE ( 'NONE', *, *, #96973, .T. ) ;
#77886 = CARTESIAN_POINT ( 'NONE',  ( 49.02571528365142939, 7.903708718522375776, -16.36159347772493078 ) ) ;
#77887 = DIRECTION ( 'NONE',  ( 0.000000000000000000, 0.000000000000000000, 1.000000000000000000 ) ) ;
#77889 = ORIENTED_EDGE ( 'NONE', *, *, #4277, .F. ) ;
#77888 = FACE_OUTER_BOUND ( 'NONE', #44393, .T. ) ;
#77890 = CARTESIAN_POINT ( 'NONE',  ( 81.44888424073813837, -18.68565686739217924, 133.0755223295938663 ) ) ;
#77891 = ORIENTED_EDGE ( 'NONE', *, *, #35020, .F. ) ;
#77892 = CARTESIAN_POINT ( 'NONE',  ( 1.726903458799834867, -50.00449021765935953, 40.95332780868852041 ) ) ;
#77893 = CARTESIAN_POINT ( 'NONE',  ( -7.188101187500002709, -16.81250000204838813, 2.977408999572647819 ) ) ;
#77894 = CARTESIAN_POINT ( 'NONE',  ( -82.98668029349501296, -57.53378708018315280, 201.1759417985833238 ) ) ;
#77895 = ORIENTED_EDGE ( 'NONE', *, *, #102948, .F. ) ;
#77896 = VECTOR ( 'NONE', #14931, 1000.000000000000000 ) ;
#77897 =( GEOMETRIC_REPRESENTATION_CONTEXT ( 3 ) GLOBAL_UNCERTAINTY_ASSIGNED_CONTEXT ( ( #83698 ) ) GLOBAL_UNIT_ASSIGNED_CONTEXT ( ( #44970, #101599, #69764 ) ) REPRESENTATION_CONTEXT ( 'NONE', 'WORKASPACE' ) );
#77898 = CARTESIAN_POINT ( 'NONE',  ( 4.322615621094100469, 10.89057051264452625, 4.999999999999999112 ) ) ;
#77899 = CARTESIAN_POINT ( 'NONE',  ( -9.989113211954167681, 81.02700726451004698, 0.5334031035449062763 ) ) ;
#77900 = EDGE_CURVE ( 'NONE', #10075, #34113, #40844, .T. ) ;
#77901 = VECTOR ( 'NONE', #16771, 1000.000000000000000 ) ;
#77902 = CARTESIAN_POINT ( 'NONE',  ( 49.27995299967488307, 13.03636147101435050, -15.63012893017262250 ) ) ;
#77903 = CARTESIAN_POINT ( 'NONE',  ( 5.656854249492380582, -20.00000000409677270, -5.656854249492379694 ) ) ;
#77904 = CARTESIAN_POINT ( 'NONE',  ( -45.30276295077697313, -28.39995151607098478, 40.39584832702679762 ) ) ;
#77905 = CARTESIAN_POINT ( 'NONE',  ( -2.500000000000097256, -24.66556416602881896, -30.98418060188836876 ) ) ;
#77906 = VECTOR ( 'NONE', #47204, 1000.000000000000000 ) ;
#77907 = DIRECTION ( 'NONE',  ( 0.000000000000000000, 0.9349068334195446139, -0.3548932414479595843 ) ) ;
#77908 = B_SPLINE_CURVE_WITH_KNOTS ( 'NONE', 3,
 ( #99010, #66670, #23047, #3539, #27326, #67215, #100089, #51541, #50994, #10547, #44535, #52070 ),
 .UNSPECIFIED., .F., .F.,
 ( 4, 2, 2, 2, 2, 4 ),
 ( 0.000000000000000000, 0.2500336435762632314, 0.5000829980240025785, 0.7501323524717418145, 0.8751570296956115991, 1.000000000000000000 ),
 .UNSPECIFIED. ) ;
#77909 = CARTESIAN_POINT ( 'NONE',  ( 5.121894999926677627, -2.681690743133432697, -18.64842307824732970 ) ) ;
#77910 = CARTESIAN_POINT ( 'NONE',  ( 32.22503847990217452, 485.9064490506207790, 4.829857536092636572 ) ) ;
#77911 = APPLICATION_PROTOCOL_DEFINITION ( 'draft international standard', 'automotive_design', 1998, #69346 ) ;
#77912 = CARTESIAN_POINT ( 'NONE',  ( 5.154030868011758137, -30.00000000000000711, -5.413958715054342896 ) ) ;
#77913 = EDGE_LOOP ( 'NONE', ( #48045, #47411, #26156, #72545, #71043 ) ) ;
#77914 = CARTESIAN_POINT ( 'NONE',  ( 11.35794436181222089, -4.958956545026470764, -12.57307762860520661 ) ) ;
#77916 = CARTESIAN_POINT ( 'NONE',  ( 0.000000000000000000, 0.000000000000000000, -1.875285714285714445 ) ) ;
#77915 =( BOUNDED_SURFACE ( )  B_SPLINE_SURFACE ( 3, 2, ( 
 ( #33206, #15934, #90897 ),
 ( #89832, #91436, #81706 ),
 ( #57977, #17014, #99495 ),
 ( #7829, #41271, #66077 ),
 ( #8897, #74159, #7297 ),
 ( #97912, #24064, #73624 ),
 ( #41798, #106529, #40208 ),
 ( #24587, #17550, #32684 ),
 ( #8369, #73083, #98956 ),
 ( #80659, #105992, #25670 ),
 ( #48287, #81186, #89307 ),
 ( #58535, #49349, #32141 ),
 ( #65019, #66612, #40739 ),
 ( #6780, #15402, #64506 ),
 ( #49889, #31618, #48813 ),
 ( #98441, #82796, #74686 ) ),
 .UNSPECIFIED., .F., .F., .F. ) 
 B_SPLINE_SURFACE_WITH_KNOTS ( ( 4, 2, 2, 2, 2, 2, 2, 4 ),
 ( 3, 3 ),
 ( 0.000000000000000000, 0.001044086800741871740, 0.001566130201112807610, 0.002088173601483743480, 0.002610217001854679350, 0.003132260402225615220, 0.003654303802596551090, 0.004176347202967486960 ),
 ( 0.000000000000000000, 1.000000000000000000 ),
 .UNSPECIFIED. ) 
 GEOMETRIC_REPRESENTATION_ITEM ( )  RATIONAL_B_SPLINE_SURFACE ( (
 ( 1.000000000000000000, 0.8350736500408202367, 1.000000000000000000),
 ( 1.000000000000000000, 0.8489954227501540496, 1.000000000000000000),
 ( 1.000000000000000000, 0.8615675893696067567, 1.000000000000000000),
 ( 1.000000000000000000, 0.8776574663916940633, 1.000000000000000000),
 ( 1.000000000000000000, 0.8825492266237192629, 1.000000000000000000),
 ( 1.000000000000000000, 0.8909252284700192037, 1.000000000000000000),
 ( 1.000000000000000000, 0.8944578560793419175, 1.000000000000000000),
 ( 1.000000000000000000, 0.9000429021727629486, 1.000000000000000000),
 ( 1.000000000000000000, 0.9020681612884537959, 1.000000000000000000),
 ( 1.000000000000000000, 0.9043430709037243442, 1.000000000000000000),
 ( 1.000000000000000000, 0.9046293304020756043, 1.000000000000000000),
 ( 1.000000000000000000, 0.9034445554302654724, 1.000000000000000000),
 ( 1.000000000000000000, 0.9019515008116110177, 1.000000000000000000),
 ( 1.000000000000000000, 0.8973842636247786331, 1.000000000000000000),
 ( 1.000000000000000000, 0.8943059481781706621, 1.000000000000000000),
 ( 1.000000000000000000, 0.8904848454314516770, 1.000000000000000000) ) ) 
 REPRESENTATION_ITEM ( '' )  SURFACE ( )  );
#77917 = CARTESIAN_POINT ( 'NONE',  ( -17.02376466190710858, -20.13787694001170792, -37.76456291957570954 ) ) ;
#77918 = CARTESIAN_POINT ( 'NONE',  ( -59.62543477322416408, -30.00000000000001066, 66.02805493078550114 ) ) ;
#77919 = EDGE_CURVE ( 'NONE', #67329, #27550, #67174, .T. ) ;
#77920 = CARTESIAN_POINT ( 'NONE',  ( 22.10841373170462987, 28.16423242622106216, -31.35595207099958159 ) ) ;
#77921 = ORIENTED_EDGE ( 'NONE', *, *, #13306, .F. ) ;
#77922 = CARTESIAN_POINT ( 'NONE',  ( -12.49955057333833253, -4.332870170146376765, -12.71907580221295220 ) ) ;
#77923 = CARTESIAN_POINT ( 'NONE',  ( 77.62028495137472817, -57.51624882744770417, 196.0320499155326672 ) ) ;
#77924 = CARTESIAN_POINT ( 'NONE',  ( 5.036189803708992052, 48.00000000000000711, -76.26213611645744095 ) ) ;
#77925 = CARTESIAN_POINT ( 'NONE',  ( -2.241046694638763270, -6.576374040526363984, -6.171384342982626947 ) ) ;
#77926 = CARTESIAN_POINT ( 'NONE',  ( -15.64030048137735207, 21.26710225493047091, -5.626279437303003839 ) ) ;
#77927 = FACE_OUTER_BOUND ( 'NONE', #68820, .T. ) ;
#77928 = CARTESIAN_POINT ( 'NONE',  ( -65.76787259454413004, -60.00000000000000000, 121.4293818171927200 ) ) ;
#77929 = CARTESIAN_POINT ( 'NONE',  ( -6.781345014477444089, 3.590342129888842049, -6.122077150241849175 ) ) ;
#77930 = ADVANCED_FACE ( 'NONE', ( #34692 ), #42743, .T. ) ;
#77931 = PRESENTATION_STYLE_ASSIGNMENT (( #44507 ) ) ;
#77932 = CARTESIAN_POINT ( 'NONE',  ( -84.85514074054155742, -53.83695654295202360, 190.4612003849218240 ) ) ;
#77933 = VECTOR ( 'NONE', #104681, 1000.000000000000000 ) ;
#77934 = VERTEX_POINT ( 'NONE', #99360 ) ;
#77935 = CARTESIAN_POINT ( 'NONE',  ( -41.75349605900994021, 461.8279235811434660, 2.915883750441013333 ) ) ;
#77936 = CARTESIAN_POINT ( 'NONE',  ( -2.047037499957236051, -56.88421240858798456, 33.36767775095443511 ) ) ;
#77937 = CARTESIAN_POINT ( 'NONE',  ( -5.711455862418337581, 41.98245415718732687, -59.41190564724043099 ) ) ;
#77938 = PRESENTATION_LAYER_ASSIGNMENT (  '', '', ( #81364 ) ) ;
#77939 = ORIENTED_EDGE ( 'NONE', *, *, #83334, .F. ) ;
#77940 = CARTESIAN_POINT ( 'NONE',  ( -36.49890972612865880, 361.2193401986697836, 2.712660087864745329 ) ) ;
#77941 = CARTESIAN_POINT ( 'NONE',  ( 38.02420928480272977, 490.5701994133388553, 12.25121054170005941 ) ) ;
#77942 = CARTESIAN_POINT ( 'NONE',  ( -33.00000000000000000, 500.0000000000002274, 15.00000000000000711 ) ) ;
#77943 = EDGE_LOOP ( 'NONE', ( #47008, #81921, #104060, #98936 ) ) ;
#77944 = MECHANICAL_DESIGN_GEOMETRIC_PRESENTATION_REPRESENTATION (  '', ( #72702 ), #12405 ) ;
#77945 = CARTESIAN_POINT ( 'NONE',  ( 22.10266876167072425, 303.0855146123441273, -9.950096580394351520 ) ) ;
#77946 = CARTESIAN_POINT ( 'NONE',  ( 12.49205219477306095, 22.71772351425832781, 5.929143317787740841 ) ) ;
#77947 = CARTESIAN_POINT ( 'NONE',  ( 9.687386010480340204, 53.40046982867094982, -3.326548872099157172 ) ) ;
#77948 = CARTESIAN_POINT ( 'NONE',  ( 95.73610373016691710, -30.00000000000000355, 71.50072510963239836 ) ) ;
#77949 = CARTESIAN_POINT ( 'NONE',  ( -77.54683902299700549, -53.37720965911378812, 145.1088727403986525 ) ) ;
#77950 = VERTEX_POINT ( 'NONE', #82125 ) ;
#77951 = CARTESIAN_POINT ( 'NONE',  ( 6.243930039575695118E-05, -60.00000000000000000, 42.00000000000000711 ) ) ;
#77952 = DIRECTION ( 'NONE',  ( 1.000000000000000000, 0.000000000000000000, 0.000000000000000000 ) ) ;
#77953 = CARTESIAN_POINT ( 'NONE',  ( 15.51076798754675679, -57.67136409421777188, 41.78720178657271589 ) ) ;
#77954 = CARTESIAN_POINT ( 'NONE',  ( 19.50011280463133545, 50.00000000000000000, 59.90639435984937222 ) ) ;
#77955 = CARTESIAN_POINT ( 'NONE',  ( 36.36099827879255741, 334.2868656930699558, -2.351449576734861324 ) ) ;
#77956 = CARTESIAN_POINT ( 'NONE',  ( 28.58349330513380337, 1.593028355512270567E-15, 0.000000000000000000 ) ) ;
#77957 = ORIENTED_EDGE ( 'NONE', *, *, #40555, .T. ) ;
#77958 = CYLINDRICAL_SURFACE ( 'NONE', #97793, 5.000000000000000888 ) ;
#77959 = CARTESIAN_POINT ( 'NONE',  ( 31.94980155458579318, 439.7324857888989982, 23.88680823179080903 ) ) ;
#77960 = CARTESIAN_POINT ( 'NONE',  ( -2.977408999572650039, -24.68750000204838457, -7.188101187500001821 ) ) ;
#77961 = ORIENTED_EDGE ( 'NONE', *, *, #81, .F. ) ;
#77962 = CIRCLE ( 'NONE', #91743, 2.000000000000000000 ) ;
#77963 = FACE_OUTER_BOUND ( 'NONE', #106213, .T. ) ;
#77964 = CARTESIAN_POINT ( 'NONE',  ( 6.195804100829465533, 41.59435685053999521, -70.65487364791140124 ) ) ;
#77965 = DIRECTION ( 'NONE',  ( 1.000000000000000000, 0.000000000000000000, -1.224646799147353207E-16 ) ) ;
#77966 = CARTESIAN_POINT ( 'NONE',  ( 5.413502513818780670, -11.02777463356547472, -10.18306091005958791 ) ) ;
#77967 = CARTESIAN_POINT ( 'NONE',  ( -24.23713502960758603, 27.31419257049583038, -32.69873751732588119 ) ) ;
#77968 = ORIENTED_EDGE ( 'NONE', *, *, #39336, .F. ) ;
#77969 = CARTESIAN_POINT ( 'NONE',  ( 5.563457319916096822, -59.99999999999998579, -42.58005360022414720 ) ) ;
#77970 = AXIS2_PLACEMENT_3D ( 'NONE', #86128, #95790, #13255 ) ;
#77972 = CARTESIAN_POINT ( 'NONE',  ( 27.12275927623064220, -49.91024972011634020, 34.05263844785792315 ) ) ;
#77971 = CARTESIAN_POINT ( 'NONE',  ( -37.55014638933011639, -30.00000000000003553, 45.10809268468624111 ) ) ;
#77973 = CARTESIAN_POINT ( 'NONE',  ( -7.290763246116595115E-15, 7.666536031838887766, 59.53359981990485750 ) ) ;
#77974 = ORIENTED_EDGE ( 'NONE', *, *, #49203, .F. ) ;
#77975 = CARTESIAN_POINT ( 'NONE',  ( -38.96414789418697211, -56.81010691829630588, 41.53583478051260869 ) ) ;
#77976 = ADVANCED_FACE ( 'NONE', ( #74038 ), #101588, .T. ) ;
#77977 = ORIENTED_EDGE ( 'NONE', *, *, #73188, .T. ) ;
#77978 = CARTESIAN_POINT ( 'NONE',  ( -8.127057321558243785, -4.285714285714296246, -23.93420880016848784 ) ) ;
#77979 = FACE_OUTER_BOUND ( 'NONE', #65242, .T. ) ;
#77980 = CARTESIAN_POINT ( 'NONE',  ( -43.36987996248237209, 463.6266071970522376, 5.362859981238893070 ) ) ;
#77981 = CIRCLE ( 'NONE', #15989, 4.000000000000007105 ) ;
#77982 = CARTESIAN_POINT ( 'NONE',  ( -0.6428164758118281030, 52.11010785308932469, -7.915233080243755381 ) ) ;
#77983 = DIRECTION ( 'NONE',  ( -1.000000000000000000, -0.000000000000000000, -0.000000000000000000 ) ) ;
#77984 = CARTESIAN_POINT ( 'NONE',  ( 10.68122111649761052, -0.9711149147263152814, 20.28324505696595637 ) ) ;
#77985 = VERTEX_POINT ( 'NONE', #7702 ) ;
#77986 = CARTESIAN_POINT ( 'NONE',  ( -65.34381883650611655, -38.33780668462405572, 114.6597469430721219 ) ) ;
#77987 = CARTESIAN_POINT ( 'NONE',  ( 97.90175465450766978, -29.99999999999976907, 190.6242977259294094 ) ) ;
#77988 = CARTESIAN_POINT ( 'NONE',  ( 40.91302753174524298, 39.68470576882931056, -51.74909898369087813 ) ) ;
#77989 = CARTESIAN_POINT ( 'NONE',  ( 57.70539558375507738, 6.856755485862130937E-15, 0.000000000000000000 ) ) ;
#77990 = EDGE_CURVE ( 'NONE', #19064, #53956, #50296, .T. ) ;
#77991 = CARTESIAN_POINT ( 'NONE',  ( 81.59117427061555361, -29.99999999999999645, -6.241865967097711021 ) ) ;
#77992 = EDGE_CURVE ( 'NONE', #49001, #15279, #62638, .T. ) ;
#77993 = DIRECTION ( 'NONE',  ( 9.251858538543008510E-15, -0.9911985061125712093, 0.1323839925376438520 ) ) ;
#77994 = EDGE_LOOP ( 'NONE', ( #37242, #102511, #13890, #64449 ) ) ;
#77995 = EDGE_LOOP ( 'NONE', ( #48863, #19662, #90540, #87570 ) ) ;
#77996 = ORIENTED_EDGE ( 'NONE', *, *, #74300, .T. ) ;
#77997 = LINE ( 'NONE', #86647, #10739 ) ;
#77998 = CARTESIAN_POINT ( 'NONE',  ( 31.55411176397327466, 43.06427903709310812, -67.12026830634881946 ) ) ;
#77999 = CARTESIAN_POINT ( 'NONE',  ( -37.24792026525560118, 25.58915884325793044, -13.42514790916754919 ) ) ;
#78000 = CARTESIAN_POINT ( 'NONE',  ( 4.472135954999581386, -10.27329903512641884, -4.000000000000000000 ) ) ;
#78001 = SURFACE_STYLE_USAGE ( .BOTH. , #37046 ) ;
#78002 = CARTESIAN_POINT ( 'NONE',  ( -7.934883677559678716, -88.86839177937552847, 1.051380792122687202 ) ) ;
#78003 = ORIENTED_EDGE ( 'NONE', *, *, #49733, .T. ) ;
#78004 = CARTESIAN_POINT ( 'NONE',  ( 6.145467200820246667, 48.00000000000000000, -77.00333157708931253 ) ) ;
#78005 = B_SPLINE_CURVE_WITH_KNOTS ( 'NONE', 3,
 ( #80631, #1288, #10464, #74659, #744, #1833, #25090, #49863 ),
 .UNSPECIFIED., .F., .F.,
 ( 4, 2, 2, 4 ),
 ( 0.003797433802554452380, 0.004743183970586248299, 0.005688934138618042917, 0.007580434474681632152 ),
 .UNSPECIFIED. ) ;
#78006 = VERTEX_POINT ( 'NONE', #90232 ) ;
#78007 = CARTESIAN_POINT ( 'NONE',  ( -5.649205854336968535, -61.54645467188483821, -2.034449005107563657 ) ) ;
#78008 = CARTESIAN_POINT ( 'NONE',  ( 2.377971153322278042E-07, -60.00000000000000000, 39.63907915656436387 ) ) ;
#78009 = CARTESIAN_POINT ( 'NONE',  ( 3.313708498984724304, -11.46875000409677092, 8.000000000000039080 ) ) ;
#78010 = CARTESIAN_POINT ( 'NONE',  ( 25.00873914691374367, 295.6585831474191082, 2.110237673684152604 ) ) ;
#78011 = EDGE_CURVE ( 'NONE', #68266, #81772, #56752, .T. ) ;
#78012 = VECTOR ( 'NONE', #20980, 1000.000000000000000 ) ;
#78013 = CARTESIAN_POINT ( 'NONE',  ( 0.000000000000000000, 0.000000000000000000, 0.000000000000000000 ) ) ;
#78014 = CARTESIAN_POINT ( 'NONE',  ( 64.90979689770158245, -25.57766637826449241, 78.74366095350538330 ) ) ;
#78015 = PRESENTATION_LAYER_ASSIGNMENT (  '', '', ( #98616 ) ) ;
#78016 = EDGE_LOOP ( 'NONE', ( #87936, #42442, #72250, #81877 ) ) ;
#78017 = CARTESIAN_POINT ( 'NONE',  ( 0.000000000000000000, 0.000000000000000000, 5.000000000000000888 ) ) ;
#78018 = CARTESIAN_POINT ( 'NONE',  ( -74.39710941758080764, -38.35602968779575406, -29.42678671130902401 ) ) ;
#78019 = CIRCLE ( 'NONE', #31532, 6.499999999999999112 ) ;
#78020 = LINE ( 'NONE', #5714, #28259 ) ;
#78021 = DIRECTION ( 'NONE',  ( 0.000000000000000000, -0.6886991506762676352, 0.7250472259499980421 ) ) ;
#78022 = ORIENTED_EDGE ( 'NONE', *, *, #100420, .T. ) ;
#78023 = CARTESIAN_POINT ( 'NONE',  ( -4.970849588242775674, -3.447900702885855928, 102.2755693391596026 ) ) ;
#78024 =( NAMED_UNIT ( * ) SI_UNIT ( $, .STERADIAN. ) SOLID_ANGLE_UNIT ( ) );
#78025 = CARTESIAN_POINT ( 'NONE',  ( 0.2791032213812772445, -8.821394357840576461, -7.929128246061912577 ) ) ;
#78026 = AXIS2_PLACEMENT_3D ( 'NONE', #38480, #57808, #41644 ) ;
#78027 = CARTESIAN_POINT ( 'NONE',  ( -2.499999999999996891, -8.000000000000000000, -17.89626171146327493 ) ) ;
#78028 = EDGE_CURVE ( 'NONE', #3051, #71421, #17421, .T. ) ;
#78029 = CARTESIAN_POINT ( 'NONE',  ( -2.204364238465237794E-15, -20.00000000000001776, -9.000000000000007105 ) ) ;
#78030 = CARTESIAN_POINT ( 'NONE',  ( 26.11923076923076792, 4.172000000000003261, 5.109226446042759579E-16 ) ) ;
#78031 = CARTESIAN_POINT ( 'NONE',  ( 86.38940954400048611, -17.29237249855646397, 180.4464348139406979 ) ) ;
#78032 = CARTESIAN_POINT ( 'NONE',  ( -5.266678742591862417, 13.24337579848477375, -33.12418987319537678 ) ) ;
#78033 = CARTESIAN_POINT ( 'NONE',  ( -9.998846395930074848, 7.501654003239973889, 0.000000000000000000 ) ) ;
#78034 = EDGE_LOOP ( 'NONE', ( #32054, #66842, #77612 ) ) ;
#78035 = CARTESIAN_POINT ( 'NONE',  ( 14.03172653833942007, -57.67096042263639077, -44.20628230871724895 ) ) ;
#78036 = FILL_AREA_STYLE ('',( #102849 ) ) ;
#78037 = CARTESIAN_POINT ( 'NONE',  ( 36.08349330513379982, -4.000000000000000888, 4.898587196589416773E-16 ) ) ;
#78038 = VECTOR ( 'NONE', #51453, 999.9999999999998863 ) ;
#78039 = CARTESIAN_POINT ( 'NONE',  ( -97.43753319845056637, -29.99999999999999645, 133.6227268290389247 ) ) ;
#78040 = EDGE_CURVE ( 'NONE', #59320, #42837, #41155, .T. ) ;
#78041 = PRESENTATION_LAYER_ASSIGNMENT (  '', '', ( #33246 ) ) ;
#78042 = PRESENTATION_LAYER_ASSIGNMENT (  '', '', ( #17771 ) ) ;
#78043 = CARTESIAN_POINT ( 'NONE',  ( 0.000000000000000000, 80.00000000000000000, 0.000000000000000000 ) ) ;
#78044 = CARTESIAN_POINT ( 'NONE',  ( 10.20446870609379708, -57.67128174344939140, 41.61875012191181611 ) ) ;
#78046 = DIRECTION ( 'NONE',  ( -1.000000000000000000, -0.000000000000000000, -0.000000000000000000 ) ) ;
#78045 = CARTESIAN_POINT ( 'NONE',  ( 11.46409645960816626, 12.99999999999817923, -10.00000000000000178 ) ) ;
#78047 = SURFACE_STYLE_USAGE ( .BOTH. , #53248 ) ;
#78048 = CARTESIAN_POINT ( 'NONE',  ( 0.000000000000000000, 0.000000000000000000, 62.00000000000000000 ) ) ;
#78049 = FILL_AREA_STYLE ('',( #78567 ) ) ;
#78050 = FACE_OUTER_BOUND ( 'NONE', #95991, .T. ) ;
#78051 = DIRECTION ( 'NONE',  ( -1.000000000000000000, -0.000000000000000000, -0.000000000000000000 ) ) ;
#78052 = EDGE_CURVE ( 'NONE', #106311, #54954, #17211, .T. ) ;
#78053 = CARTESIAN_POINT ( 'NONE',  ( -86.71810255127751077, -53.77243697590854055, 192.6459912591498096 ) ) ;
#78054 = VERTEX_POINT ( 'NONE', #99912 ) ;
#78055 = FACE_OUTER_BOUND ( 'NONE', #8328, .T. ) ;
#78056 = CARTESIAN_POINT ( 'NONE',  ( -20.58320923621259624, -56.88195280983516255, 33.96619711972437017 ) ) ;
#78057 = EDGE_CURVE ( 'NONE', #70018, #24844, #22390, .T. ) ;
#78059 = CARTESIAN_POINT ( 'NONE',  ( 38.92819510383412762, 485.1409701397173535, -4.243468885292519310 ) ) ;
#78058 = PRESENTATION_STYLE_ASSIGNMENT (( #3650 ) ) ;
#78060 = EDGE_LOOP ( 'NONE', ( #59251, #48411, #44033, #103366, #54921 ) ) ;
#78061 = CARTESIAN_POINT ( 'NONE',  ( 16.14595037866564908, 6.775806037743102195, -6.185188124844921198 ) ) ;
#78062 = ORIENTED_EDGE ( 'NONE', *, *, #85200, .T. ) ;
#78063 = CARTESIAN_POINT ( 'NONE',  ( -32.28552837373656814, 464.7648866755938570, 15.30384310834764428 ) ) ;
#78064 = LINE ( 'NONE', #5762, #44263 ) ;
#78065 = CARTESIAN_POINT ( 'NONE',  ( -8.401895502683421668, -59.99999999999998579, -42.47750708342923787 ) ) ;
#78066 = VERTEX_POINT ( 'NONE', #78291 ) ;
#78067 = CARTESIAN_POINT ( 'NONE',  ( 0.000000000000000000, 115.0000000000000000, 0.000000000000000000 ) ) ;
#78068 = CARTESIAN_POINT ( 'NONE',  ( 0.000000000000000000, -14.49999999999999822, 8.000000000000000000 ) ) ;
#78069 = CARTESIAN_POINT ( 'NONE',  ( 99.57578696694601206, -37.83214993661866998, 191.2440777680208157 ) ) ;
#78070 = AXIS2_PLACEMENT_3D ( 'NONE', #72124, #105034, #6309 ) ;
#78072 = LINE ( 'NONE', #4187, #106227 ) ;
#78071 = FACE_OUTER_BOUND ( 'NONE', #28539, .T. ) ;
#78073 = ORIENTED_EDGE ( 'NONE', *, *, #65903, .T. ) ;
#78074 = CONICAL_SURFACE ( 'NONE', #95327, 8.000000000000000000, 0.9599310885968911355 ) ;
#78075 = ADVANCED_FACE ( 'NONE', ( #102036 ), #8562, .T. ) ;
#78076 = ORIENTED_EDGE ( 'NONE', *, *, #65291, .T. ) ;
#78077 = CIRCLE ( 'NONE', #23051, 4.000000000000000888 ) ;
#78078 = ORIENTED_EDGE ( 'NONE', *, *, #69088, .T. ) ;
#78079 = CARTESIAN_POINT ( 'NONE',  ( 25.89392128340153576, 307.0924142446438054, 10.67957798942343217 ) ) ;
#78080 = CARTESIAN_POINT ( 'NONE',  ( 0.000000000000000000, 0.000000000000000000, -8.500000000000000000 ) ) ;
#78081 = VERTEX_POINT ( 'NONE', #60545 ) ;
#78082 = CYLINDRICAL_SURFACE ( 'NONE', #65116, 6.499999999999999112 ) ;
#78083 = CARTESIAN_POINT ( 'NONE',  ( -5.652563880857838896, 41.79847487344755308, -70.46163212616390581 ) ) ;
#78084 = CARTESIAN_POINT ( 'NONE',  ( -92.02125586894585751, -59.99999999999631228, -20.08360105537134643 ) ) ;
#78085 = CARTESIAN_POINT ( 'NONE',  ( 7.046357527897571416, -66.30615650601004063, -3.789683693877209603 ) ) ;
#78086 = CARTESIAN_POINT ( 'NONE',  ( 55.71811758917225887, -60.00000000000965628, -39.11301512399793978 ) ) ;
#78087 = DIRECTION ( 'NONE',  ( 0.000000000000000000, -1.000000000000000000, 0.000000000000000000 ) ) ;
#78088 = CARTESIAN_POINT ( 'NONE',  ( -6.568714509987131578, 41.61374477456796939, -58.74117337121824534 ) ) ;
#78089 = VECTOR ( 'NONE', #64612, 1000.000000000000000 ) ;
#78091 = CARTESIAN_POINT ( 'NONE',  ( 4.981165396653468136, -22.06714069377673582, 27.55817400068765721 ) ) ;
#78090 = CARTESIAN_POINT ( 'NONE',  ( -106.4977058212534189, -30.00000000000001776, 137.1023255444873428 ) ) ;
#78092 = CARTESIAN_POINT ( 'NONE',  ( 28.58349330513380337, -4.000000000000000000, 4.898587196589415787E-16 ) ) ;
#78093 = CARTESIAN_POINT ( 'NONE',  ( -49.11024409948323211, -32.59653215272530957, 47.10069971812693268 ) ) ;
#78094 = VERTEX_POINT ( 'NONE', #20657 ) ;
#78095 = B_SPLINE_CURVE_WITH_KNOTS ( 'NONE', 3,
 ( #49505, #17165, #57581, #39844, #32292, #82413, #32825, #914 ),
 .UNSPECIFIED., .F., .F.,
 ( 4, 2, 2, 4 ),
 ( -1.406834188357377339E-05, 0.0004804345972576498734, 0.0007276860668282617408, 0.0009749375363988734998 ),
 .UNSPECIFIED. ) ;
#78096 = CARTESIAN_POINT ( 'NONE',  ( -3.893533249295163756, 18.77903270381816725, 5.817337832407639020 ) ) ;
#78097 = ORIENTED_EDGE ( 'NONE', *, *, #89452, .F. ) ;
#78098 = CARTESIAN_POINT ( 'NONE',  ( 13.09999999999999787, 1.533819458162526451E-15, 0.000000000000000000 ) ) ;
#78099 = CARTESIAN_POINT ( 'NONE',  ( 5.911778709945828325, -6.133381605834290262, 1.058844270818177336 ) ) ;
#78100 = ORIENTED_EDGE ( 'NONE', *, *, #57577, .T. ) ;
#78101 = CARTESIAN_POINT ( 'NONE',  ( -10.05401422878392204, -11.60173371080193050, 9.516791662972487131 ) ) ;
#78102 = ORIENTED_EDGE ( 'NONE', *, *, #106374, .T. ) ;
#78103 = CARTESIAN_POINT ( 'NONE',  ( 58.10017903397120875, -38.34421737741784852, 90.49762462764655879 ) ) ;
#78104 = PRESENTATION_LAYER_ASSIGNMENT (  '', '', ( #14569 ) ) ;
#78105 = CARTESIAN_POINT ( 'NONE',  ( 6.831363830528337289, 41.73171983268897378, -59.17722554277374059 ) ) ;
#78106 = CARTESIAN_POINT ( 'NONE',  ( -47.37019975542479955, 42.00000000008224532, -36.40416150956886554 ) ) ;
#78107 = CARTESIAN_POINT ( 'NONE',  ( 100.8967648887429789, -30.00000000000000711, 180.1179238002322336 ) ) ;
#78108 =( GEOMETRIC_REPRESENTATION_CONTEXT ( 3 ) GLOBAL_UNCERTAINTY_ASSIGNED_CONTEXT ( ( #68614 ) ) GLOBAL_UNIT_ASSIGNED_CONTEXT ( ( #56210, #24450, #31989 ) ) REPRESENTATION_CONTEXT ( 'NONE', 'WORKASPACE' ) );
#78109 = EDGE_CURVE ( 'NONE', #90738, #98861, #51357, .T. ) ;
#78110 = CARTESIAN_POINT ( 'NONE',  ( -1.005228751829300160, 36.47691725556884990, 29.24735311802084681 ) ) ;
#78111 = ORIENTED_EDGE ( 'NONE', *, *, #81982, .F. ) ;
#78112 = MECHANICAL_DESIGN_GEOMETRIC_PRESENTATION_REPRESENTATION (  '', ( #69502 ), #23014 ) ;
#78113 = ORIENTED_EDGE ( 'NONE', *, *, #25422, .F. ) ;
#78114 = EDGE_LOOP ( 'NONE', ( #97963, #29918 ) ) ;
#78115 = CARTESIAN_POINT ( 'NONE',  ( 54.70282561401326404, -18.68954287160401151, 51.55838953990642182 ) ) ;
#78116 = PRESENTATION_LAYER_ASSIGNMENT (  '', '', ( #14421 ) ) ;
#78117 = CARTESIAN_POINT ( 'NONE',  ( 43.03880698781972569, 435.3545807224048190, 16.83573131045119098 ) ) ;
#78118 = EDGE_CURVE ( 'NONE', #67342, #550, #99884, .T. ) ;
#78119 = CARTESIAN_POINT ( 'NONE',  ( -46.00000000000000711, 460.6827615371018965, 7.624057330649156583 ) ) ;
#78120 = ORIENTED_EDGE ( 'NONE', *, *, #63735, .F. ) ;
#78121 = CARTESIAN_POINT ( 'NONE',  ( -91.44391289275247914, -38.39053751225738864, -8.102761395347648943 ) ) ;
#78122 = ORIENTED_EDGE ( 'NONE', *, *, #510, .T. ) ;
#78123 = CARTESIAN_POINT ( 'NONE',  ( 105.5497290054224209, -38.38417664786370409, 196.8944578755671841 ) ) ;
#78124 = CARTESIAN_POINT ( 'NONE',  ( 11.12323130174675256, 19.59210383280182910, 8.689352701389447375 ) ) ;
#78125 = CARTESIAN_POINT ( 'NONE',  ( 85.28997562300351376, -52.71456239550101941, 1.971080634725701719 ) ) ;
#78126 = CARTESIAN_POINT ( 'NONE',  ( 42.72191162735155245, 427.3218109763436132, 19.12685808572960511 ) ) ;
#78127 = CARTESIAN_POINT ( 'NONE',  ( -43.02661387979790675, 465.7449615347597387, 11.43319743843397696 ) ) ;
#78128 = CYLINDRICAL_SURFACE ( 'NONE', #15427, 60.00000000000000000 ) ;
#78129 = CARTESIAN_POINT ( 'NONE',  ( -43.62838954006684844, 434.9736691849526551, 14.34345830637900576 ) ) ;
#78130 = DIRECTION ( 'NONE',  ( -1.000000000000000000, 0.000000000000000000, 0.000000000000000000 ) ) ;
#78131 = ORIENTED_EDGE ( 'NONE', *, *, #87389, .T. ) ;
#78132 = EDGE_CURVE ( 'NONE', #5164, #56216, #76164, .T. ) ;
#78133 = CARTESIAN_POINT ( 'NONE',  ( -10.00000000000000178, 15.11738935798242345, -0.3539438260497499433 ) ) ;
#78134 = CARTESIAN_POINT ( 'NONE',  ( 7.493949260784499522, 40.57568730855774675, -68.91429205858018747 ) ) ;
#78135 = PRESENTATION_LAYER_ASSIGNMENT (  '', '', ( #23114 ) ) ;
#78136 = CARTESIAN_POINT ( 'NONE',  ( -26.00996381060643969, 37.20445080285505668, 8.181011038402493440 ) ) ;
#78137 = ORIENTED_EDGE ( 'NONE', *, *, #58456, .T. ) ;
#78138 = DIRECTION ( 'NONE',  ( -0.7142857142857136354, -0.6998542122237659813, 0.000000000000000000 ) ) ;
#78139 = CARTESIAN_POINT ( 'NONE',  ( -29.70730338703692652, 314.7332412851916956, 12.83056961409002916 ) ) ;
#78140 = CARTESIAN_POINT ( 'NONE',  ( -11.17909359580129980, -4.978490734260999417, -77.11252404933959781 ) ) ;
#78141 = CARTESIAN_POINT ( 'NONE',  ( -5.656854249492379694, -20.93749999999999289, -5.656854249492380582 ) ) ;
#78142 = CARTESIAN_POINT ( 'NONE',  ( -34.70053457442661937, -26.34900356544920186, 41.82054189507673669 ) ) ;
#78143 = EDGE_CURVE ( 'NONE', #8789, #76065, #32699, .T. ) ;
#78144 = CARTESIAN_POINT ( 'NONE',  ( 42.33268550343510839, 436.4462712439766960, 6.764016893796107155 ) ) ;
#78145 = AXIS2_PLACEMENT_3D ( 'NONE', #78442, #14225, #102732 ) ;
#78146 = ORIENTED_EDGE ( 'NONE', *, *, #66782, .T. ) ;
#78147 = CARTESIAN_POINT ( 'NONE',  ( 83.76870840018638376, -50.13968266632630844, 186.2246346821466432 ) ) ;
#78148 = CARTESIAN_POINT ( 'NONE',  ( -38.74305977430618242, 27.39011302538496295, 11.77545443400052605 ) ) ;
#78149 = CARTESIAN_POINT ( 'NONE',  ( -15.54898481255693454, 46.20784644949144138, 4.780735607413708621 ) ) ;
#78150 = ORIENTED_EDGE ( 'NONE', *, *, #39875, .T. ) ;
#78151 = AXIS2_PLACEMENT_3D ( 'NONE', #60841, #29561, #85649 ) ;
#78152 = CARTESIAN_POINT ( 'NONE',  ( -91.05637678035618876, -45.26547174173002475, 77.50340589454103224 ) ) ;
#78153 = CARTESIAN_POINT ( 'NONE',  ( 6.683837171061803417, -3.955946848495962787, 6.851900933636989599 ) ) ;
#78154 = CARTESIAN_POINT ( 'NONE',  ( -5.499265899522562506, -4.999999999985523580, -99.22427370007513048 ) ) ;
#78155 = CARTESIAN_POINT ( 'NONE',  ( -30.25640691047282616, 12.05011699928720503, 39.73625916528160928 ) ) ;
#78156 = CARTESIAN_POINT ( 'NONE',  ( -9.478872174808550710, -22.49572152134529546, -38.54313998132425212 ) ) ;
#78157 = AXIS2_PLACEMENT_3D ( 'NONE', #16388, #89232, #32610 ) ;
#78158 = EDGE_CURVE ( 'NONE', #47612, #66358, #56906, .T. ) ;
#78159 = FILL_AREA_STYLE_COLOUR ( '', #26576 ) ;
#78160 = CARTESIAN_POINT ( 'NONE',  ( 7.563307719629934311, -19.30494957266906653, 35.21016297361445169 ) ) ;
#78161 = CARTESIAN_POINT ( 'NONE',  ( 3.035724950089473850, -0.5466957598722548273, 103.2067224559505831 ) ) ;
#78162 = CARTESIAN_POINT ( 'NONE',  ( 44.23667573787285789, -28.03029836076050429, 39.27938594101296843 ) ) ;
#78164 = CARTESIAN_POINT ( 'NONE',  ( -10.82859631130528655, 18.75128085564791292, 9.171573219068584137 ) ) ;
#78163 = FACE_OUTER_BOUND ( 'NONE', #7603, .T. ) ;
#78165 = CARTESIAN_POINT ( 'NONE',  ( 0.7515601774665998658, 295.1017350046088268, -10.00017833058526584 ) ) ;
#78166 = CARTESIAN_POINT ( 'NONE',  ( 40.75641113481592726, 360.0948485545300741, 24.37153223514695100 ) ) ;
#78167 = CARTESIAN_POINT ( 'NONE',  ( 36.78140055146844389, 305.3596551341470331, 0.4383668257698736803 ) ) ;
#78168 = DIRECTION ( 'NONE',  ( 1.000000000000000000, 1.224606353822377258E-16, 0.000000000000000000 ) ) ;
#78169 = DIRECTION ( 'NONE',  ( -1.000000000000000000, -1.224606353822377258E-16, -0.000000000000000000 ) ) ;
#78170 = ORIENTED_EDGE ( 'NONE', *, *, #62055, .F. ) ;
#78171 = CARTESIAN_POINT ( 'NONE',  ( -46.00000000000003553, 464.2883104330369974, 11.80345442596980199 ) ) ;
#78172 = CIRCLE ( 'NONE', #93675, 4.250000000000000000 ) ;
#78173 = EDGE_LOOP ( 'NONE', ( #49567, #61380, #66161, #54076, #41185 ) ) ;
#78174 = CARTESIAN_POINT ( 'NONE',  ( -9.346883474190137875, -3.134074240396935274, 14.76168387817866368 ) ) ;
#78175 = DIRECTION ( 'NONE',  ( 0.000000000000000000, 0.000000000000000000, 1.000000000000000000 ) ) ;
#78176 = DIRECTION ( 'NONE',  ( 0.000000000000000000, 0.000000000000000000, -1.000000000000000000 ) ) ;
#78177 = CONICAL_SURFACE ( 'NONE', #36882, 4.000000000000001776, 0.9599310885968774798 ) ;
#78178 = ADVANCED_FACE ( 'NONE', ( #2263 ), #61610, .T. ) ;
#78180 = CARTESIAN_POINT ( 'NONE',  ( 6.441795335963374391, -60.22817737698583329, -36.83328242771759164 ) ) ;
#78179 = PRESENTATION_STYLE_ASSIGNMENT (( #43686 ) ) ;
#78181 = STYLED_ITEM ( 'NONE', ( #81986 ), #67921 ) ;
#78182 = VERTEX_POINT ( 'NONE', #44890 ) ;
#78183 = AXIS2_PLACEMENT_3D ( 'NONE', #33456, #40462, #74410 ) ;
#78184 = DIRECTION ( 'NONE',  ( 0.000000000000000000, 1.000000000000000000, 0.000000000000000000 ) ) ;
#78185 = CARTESIAN_POINT ( 'NONE',  ( -43.49712701248153479, 471.1120579834711748, 8.168005033297315975 ) ) ;
#78186 = ORIENTED_EDGE ( 'NONE', *, *, #102106, .T. ) ;
#78187 = EDGE_CURVE ( 'NONE', #35426, #57692, #1771, .T. ) ;
#78188 = DIRECTION ( 'NONE',  ( 1.000000000000000000, -0.000000000000000000, -0.000000000000000000 ) ) ;
#78189 = DIRECTION ( 'NONE',  ( -1.000000000000000000, -0.000000000000000000, -0.000000000000000000 ) ) ;
#78190 = CARTESIAN_POINT ( 'NONE',  ( -92.03676806442638281, -59.99999999999999289, 19.23821862839820440 ) ) ;
#78191 = VERTEX_POINT ( 'NONE', #36819 ) ;
#78192 = CARTESIAN_POINT ( 'NONE',  ( -1.469576158976823947E-15, -28.06250000409677270, 8.000000000000000000 ) ) ;
#78193 = CARTESIAN_POINT ( 'NONE',  ( 63.81650669486618455, -4.000000000000000000, 0.000000000000000000 ) ) ;
#78194 = FILL_AREA_STYLE_COLOUR ( '', #105299 ) ;
#78195 = CARTESIAN_POINT ( 'NONE',  ( 6.499999999999999112, 3.752776749732559036, -6.064240316920397333 ) ) ;
#78197 = CARTESIAN_POINT ( 'NONE',  ( 10.28624191511840458, -1.200000000000000030E-05, 14.15779740156149025 ) ) ;
#78196 = CARTESIAN_POINT ( 'NONE',  ( 44.12589798587349321, 464.4133173135357424, 9.756011010161726560 ) ) ;
#78198 = CARTESIAN_POINT ( 'NONE',  ( -80.10560773978777149, -60.38361758132244006, 176.0919189731656900 ) ) ;
#78199 = ORIENTED_EDGE ( 'NONE', *, *, #38184, .F. ) ;
#78200 = CARTESIAN_POINT ( 'NONE',  ( -38.95242300085207177, 491.1731620564949026, 12.13306966136735099 ) ) ;
#78201 = EDGE_CURVE ( 'NONE', #87130, #11128, #43278, .T. ) ;
#78202 = ORIENTED_EDGE ( 'NONE', *, *, #62264, .F. ) ;
#78203 = ORIENTED_EDGE ( 'NONE', *, *, #70117, .F. ) ;
#78204 = CARTESIAN_POINT ( 'NONE',  ( 14.24124568368486088, -4.332661967059059371, -11.33228852115809637 ) ) ;
#78205 = CARTESIAN_POINT ( 'NONE',  ( -5.897959690130281096, -64.39611687089356451, 14.30281393798261114 ) ) ;
#78206 = PRESENTATION_STYLE_ASSIGNMENT (( #103026 ) ) ;
#78207 = VERTEX_POINT ( 'NONE', #44344 ) ;
#78208 = CIRCLE ( 'NONE', #40328, 5.000000000000001776 ) ;
#78209 = CARTESIAN_POINT ( 'NONE',  ( -1.600194386257963230E-15, 60.33964880548970200, 13.06657876680918662 ) ) ;
#78210 = FILL_AREA_STYLE_COLOUR ( '', #66815 ) ;
#78211 = CARTESIAN_POINT ( 'NONE',  ( -94.31942352638992588, -57.67240272246704791, 24.69011299903190704 ) ) ;
#78212 = CARTESIAN_POINT ( 'NONE',  ( 6.928203230275510549, -10.26883324508999173, -4.000000000000000888 ) ) ;
#78213 = CARTESIAN_POINT ( 'NONE',  ( 43.54570344706466756, 464.5919001250003930, 9.427857144828900360 ) ) ;
#78214 = CARTESIAN_POINT ( 'NONE',  ( -9.948181520647855436, 101.1310719723962137, 1.049088206181489014 ) ) ;
#78215 = CARTESIAN_POINT ( 'NONE',  ( 6.800000000000000711, 0.000000000000000000, 0.000000000000000000 ) ) ;
#78216 = CARTESIAN_POINT ( 'NONE',  ( 68.53628924694606894, -14.21045842199431597, -27.48009014525527860 ) ) ;
#78217 = CARTESIAN_POINT ( 'NONE',  ( -73.20747738243755975, -14.21045842199437992, 129.5005664428163641 ) ) ;
#78218 = CARTESIAN_POINT ( 'NONE',  ( -53.91561090801278056, -49.91042375249266883, 62.12222278454709112 ) ) ;
#78219 = VERTEX_POINT ( 'NONE', #52415 ) ;
#78220 = CARTESIAN_POINT ( 'NONE',  ( 44.11327388758692081, 464.4313852428372797, 9.822198357557351045 ) ) ;
#78221 = MECHANICAL_DESIGN_GEOMETRIC_PRESENTATION_REPRESENTATION (  '', ( #62995 ), #31742 ) ;
#78222 = EDGE_LOOP ( 'NONE', ( #84770, #104377 ) ) ;
#78223 = CARTESIAN_POINT ( 'NONE',  ( -100.1861007398734529, -37.81597759049645902, 190.2366006595198940 ) ) ;
#78224 = CARTESIAN_POINT ( 'NONE',  ( 97.86690513680532888, -37.99999999999998579, 125.1103042162925760 ) ) ;
#78225 = CARTESIAN_POINT ( 'NONE',  ( -30.59355846057999884, 12.96027739219344532, -41.71512601614534077 ) ) ;
#78226 = EDGE_LOOP ( 'NONE', ( #90580, #88870, #24377, #20147, #57085 ) ) ;
#78227 = CARTESIAN_POINT ( 'NONE',  ( 19.49770126386425773, 49.99985876156954134, 59.97225932440124296 ) ) ;
#78228 = CARTESIAN_POINT ( 'NONE',  ( 44.47534377888507606, -38.31160956920668070, 57.00192013341546016 ) ) ;
#78229 = CARTESIAN_POINT ( 'NONE',  ( 7.849088363683611291, 76.00000000000000000, 5.000000000000000000 ) ) ;
#78230 = CARTESIAN_POINT ( 'NONE',  ( 4.401442555609581635E-16, -16.15625000204838457, -7.188101187500000044 ) ) ;
#78231 = CARTESIAN_POINT ( 'NONE',  ( -3.840629472727446691E-14, -1.200000000000000030E-05, -28.50000000000000000 ) ) ;
#78232 = CARTESIAN_POINT ( 'NONE',  ( -7.000000000000000000, -80.00000000000000000, 12.61250543006184088 ) ) ;
#78233 = CARTESIAN_POINT ( 'NONE',  ( 7.896165657598944065, -81.21088868628027058, -1.307894402814545831 ) ) ;
#78234 = CARTESIAN_POINT ( 'NONE',  ( 67.76059040313977277, -29.99999999999999645, 88.32474484931194070 ) ) ;
#78235 =( BOUNDED_CURVE ( )  B_SPLINE_CURVE ( 2, ( #9918, #728, #41758 ),
 .UNSPECIFIED., .F., .F. ) 
 B_SPLINE_CURVE_WITH_KNOTS ( ( 3, 3 ),
 ( 0.000000000000000000, 1.000000000000000000 ),
 .UNSPECIFIED. ) 
 CURVE ( )  GEOMETRIC_REPRESENTATION_ITEM ( )  RATIONAL_B_SPLINE_CURVE ( ( 1.000000000000000000, 1.428571428571427271, 1.428571428571429269 ) ) 
 REPRESENTATION_ITEM ( '' )  );
#78236 = CARTESIAN_POINT ( 'NONE',  ( 84.15356149169568312, 6.123233995736582872E-16, -5.000000000000011546 ) ) ;
#78237 = LINE ( 'NONE', #52361, #32376 ) ;
#78238 = EDGE_CURVE ( 'NONE', #51764, #42859, #34556, .T. ) ;
#78239 = CARTESIAN_POINT ( 'NONE',  ( -7.500000000000001776, -4.015205788346293048, -20.09376801818934766 ) ) ;
#78240 = ADVANCED_BREP_SHAPE_REPRESENTATION ( '', ( #88291, #10728 ), #47146 ) ;
#78241 = CARTESIAN_POINT ( 'NONE',  ( -27.61573564706210249, -18.62757927915192369, 28.73073199747976503 ) ) ;
#78242 = ORIENTED_EDGE ( 'NONE', *, *, #8628, .T. ) ;
#78243 = CARTESIAN_POINT ( 'NONE',  ( 48.37073679748882427, -39.52005737407285579, 48.17779182794379977 ) ) ;
#78244 = CARTESIAN_POINT ( 'NONE',  ( 0.000000000000000000, 0.000000000000000000, -7.259124522925831435 ) ) ;
#78245 = EDGE_CURVE ( 'NONE', #89428, #4091, #35759, .T. ) ;
#78246 = CARTESIAN_POINT ( 'NONE',  ( -7.896571385775229324, 88.78997999345754977, 1.305932416347436176 ) ) ;
#78247 = CARTESIAN_POINT ( 'NONE',  ( -84.29785342784349211, -38.74543721064067370, 198.0007389996342795 ) ) ;
#78248 = ORIENTED_EDGE ( 'NONE', *, *, #37501, .F. ) ;
#78249 = CARTESIAN_POINT ( 'NONE',  ( 91.24894573165114764, -38.36097309605214178, -1.409743066707331627 ) ) ;
#78250 = CARTESIAN_POINT ( 'NONE',  ( 11.92367304074753598, 6.475998827537138958, -8.920379189304513901 ) ) ;
#78251 = CARTESIAN_POINT ( 'NONE',  ( -19.04051945834135040, 49.58720281916519212, 61.84160661372276024 ) ) ;
#78252 = FACE_OUTER_BOUND ( 'NONE', #91426, .T. ) ;
#78253 = CARTESIAN_POINT ( 'NONE',  ( 6.406311604196643472, 41.42610738297985762, -70.78720126776296695 ) ) ;
#78254 = CARTESIAN_POINT ( 'NONE',  ( -1.469576158976823947E-15, -26.56250000409677270, 8.000000000000000000 ) ) ;
#78255 = CARTESIAN_POINT ( 'NONE',  ( -33.84761347220317873, 488.7471039746334327, 11.01988148152523550 ) ) ;
#78256 = DIRECTION ( 'NONE',  ( 0.000000000000000000, 1.000000000000000000, 0.000000000000000000 ) ) ;
#78257 = CARTESIAN_POINT ( 'NONE',  ( 111.0077917343090235, -60.00000000000000000, 152.2127138817539844 ) ) ;
#78258 = PRESENTATION_LAYER_ASSIGNMENT (  '', '', ( #83417 ) ) ;
#78259 = CARTESIAN_POINT ( 'NONE',  ( -7.800703710507054467, -68.58595692657939935, 1.791736796405269283 ) ) ;
#78260 = ORIENTED_EDGE ( 'NONE', *, *, #49800, .T. ) ;
#78261 = ADVANCED_FACE ( 'NONE', ( #70210 ), #103112, .T. ) ;
#78262 = CARTESIAN_POINT ( 'NONE',  ( 7.002990960197236880, 31.05266818383456240, 3.868040364119522678 ) ) ;
#78263 = AXIS2_PLACEMENT_3D ( 'NONE', #67164, #101653, #91958 ) ;
#78264 = FACE_OUTER_BOUND ( 'NONE', #66265, .T. ) ;
#78265 = ORIENTED_EDGE ( 'NONE', *, *, #96576, .T. ) ;
#78267 = CARTESIAN_POINT ( 'NONE',  ( 5.221816652746770870, 7.032134607704920271, -27.49812609708854794 ) ) ;
#78266 = CARTESIAN_POINT ( 'NONE',  ( -44.47534256803313468, -38.31161230092084935, 57.00189278798902137 ) ) ;
#78268 = DIRECTION ( 'NONE',  ( 0.000000000000000000, -1.000000000000000000, 0.000000000000000000 ) ) ;
#78269 = CARTESIAN_POINT ( 'NONE',  ( -2.093983074874240291, -3.000000000000000444, -7.791781413346525298 ) ) ;
#78270 = CARTESIAN_POINT ( 'NONE',  ( 41.92281291883664096, 435.4200907145704491, 7.396891011706831165 ) ) ;
#78271 = CARTESIAN_POINT ( 'NONE',  ( 7.188101187500001821, -10.43750000204838457, -2.977408999572650483 ) ) ;
#78272 = CARTESIAN_POINT ( 'NONE',  ( -7.996668422917848851, -4.999999999991826094, -91.14546720082944375 ) ) ;
#78273 = CARTESIAN_POINT ( 'NONE',  ( -42.91610780537345704, 434.7038292309375720, 17.44089711044167856 ) ) ;
#78275 = ORIENTED_EDGE ( 'NONE', *, *, #48425, .F. ) ;
#78274 = CARTESIAN_POINT ( 'NONE',  ( -32.93513049338658760, 465.6726574193327224, 10.66039033145138504 ) ) ;
#78276 = CARTESIAN_POINT ( 'NONE',  ( 83.36672125823241686, -39.47416250888723965, 173.2576703317640465 ) ) ;
#78277 = CARTESIAN_POINT ( 'NONE',  ( 7.849088607700290154, 70.40480431129584815, 1.301042606982605321E-15 ) ) ;
#78278 = CARTESIAN_POINT ( 'NONE',  ( 9.646083234704169840, 88.01290609023480727, -2.643797197754290451 ) ) ;
#78279 = ORIENTED_EDGE ( 'NONE', *, *, #35634, .T. ) ;
#78280 = DIRECTION ( 'NONE',  ( -0.000000000000000000, -1.000000000000000000, -0.000000000000000000 ) ) ;
#78281 = FACE_OUTER_BOUND ( 'NONE', #45638, .T. ) ;
#78282 = FACE_OUTER_BOUND ( 'NONE', #96163, .T. ) ;
#78283 = CARTESIAN_POINT ( 'NONE',  ( 6.928203230275510549, 30.00000000000000355, -4.000000000000000000 ) ) ;
#78284 = CARTESIAN_POINT ( 'NONE',  ( 9.830769230769229594, 4.172000000000003261, 0.000000000000000000 ) ) ;
#78285 = CARTESIAN_POINT ( 'NONE',  ( 0.000000000000000000, 60.00000000000000000, 0.000000000000000000 ) ) ;
#78286 = EDGE_LOOP ( 'NONE', ( #104183, #65730, #89249, #104390, #102649 ) ) ;
#78287 = AXIS2_PLACEMENT_3D ( 'NONE', #45499, #20732, #85963 ) ;
#78288 = CARTESIAN_POINT ( 'NONE',  ( -80.50284847417118783, -29.99999999999999645, -13.02832369715059357 ) ) ;
#78289 = CARTESIAN_POINT ( 'NONE',  ( -5.000000000000000000, -38.85524261681796787, 2.940510229002995857 ) ) ;
#78290 = DIRECTION ( 'NONE',  ( 0.8660254037844389297, -0.000000000000000000, 0.4999999999999998890 ) ) ;
#78291 = CARTESIAN_POINT ( 'NONE',  ( 9.833493305133801599, -4.000000000000000888, 4.898587196589416773E-16 ) ) ;
#78292 = CARTESIAN_POINT ( 'NONE',  ( 2.977408999572650927, -23.37500000204838813, -7.188101187500001821 ) ) ;
#78293 = FACE_OUTER_BOUND ( 'NONE', #9112, .T. ) ;
#78294 = CIRCLE ( 'NONE', #16313, 1.000000000000020872 ) ;
#78295 = VECTOR ( 'NONE', #65591, 999.9999999999998863 ) ;
#78296 = DIRECTION ( 'NONE',  ( 0.000000000000000000, 0.000000000000000000, 1.000000000000000000 ) ) ;
#78297 =( NAMED_UNIT ( * ) SI_UNIT ( $, .STERADIAN. ) SOLID_ANGLE_UNIT ( ) );
#78298 =( GEOMETRIC_REPRESENTATION_CONTEXT ( 3 ) GLOBAL_UNCERTAINTY_ASSIGNED_CONTEXT ( ( #34760 ) ) GLOBAL_UNIT_ASSIGNED_CONTEXT ( ( #76236, #77313, #70288 ) ) REPRESENTATION_CONTEXT ( 'NONE', 'WORKASPACE' ) );
#78299 = ORIENTED_EDGE ( 'NONE', *, *, #82355, .T. ) ;
#78300 = DIRECTION ( 'NONE',  ( 0.000000000000000000, 0.000000000000000000, 1.000000000000000000 ) ) ;
#78301 = CARTESIAN_POINT ( 'NONE',  ( 6.249999999999998224, 4.618802153517001408, -8.000000000000000000 ) ) ;
#78302 = AXIS2_PLACEMENT_3D ( 'NONE', #10617, #68347, #53745 ) ;
#78303 = CARTESIAN_POINT ( 'NONE',  ( -4.088019673764939910, 13.67890778943449526, -5.000000000000000888 ) ) ;
#78304 = EDGE_CURVE ( 'NONE', #79234, #82760, #70629, .T. ) ;
#78305 = EDGE_LOOP ( 'NONE', ( #86822, #95252, #12296 ) ) ;
#78306 = EDGE_CURVE ( 'NONE', #34171, #35056, #92883, .T. ) ;
#78307 = DIRECTION ( 'NONE',  ( 0.000000000000000000, 0.000000000000000000, 1.000000000000000000 ) ) ;
#78308 = ORIENTED_EDGE ( 'NONE', *, *, #75107, .F. ) ;
#78309 = ADVANCED_FACE ( 'NONE', ( #84803 ), #51748, .F. ) ;
#78310 = FILL_AREA_STYLE ('',( #37367 ) ) ;
#78311 = CARTESIAN_POINT ( 'NONE',  ( -3.054195049253882743, -0.8450860964495454652, 104.0345731970086121 ) ) ;
#78312 = CARTESIAN_POINT ( 'NONE',  ( 93.97977184163765685, 5.000000000000021316, 0.000000000000000000 ) ) ;
#78313 = UNCERTAINTY_MEASURE_WITH_UNIT (LENGTH_MEASURE( 1.000000000000000082E-05 ), #35137, 'distance_accuracy_value', 'NONE');
#78314 = CARTESIAN_POINT ( 'NONE',  ( -98.63189375226259870, -59.99999999999999289, 202.2227958148920095 ) ) ;
#78315 = CARTESIAN_POINT ( 'NONE',  ( 0.000000000000000000, 0.000000000000000000, 0.000000000000000000 ) ) ;
#78316 = EDGE_CURVE ( 'NONE', #48464, #41735, #60338, .T. ) ;
#78317 =( LENGTH_UNIT ( ) NAMED_UNIT ( * ) SI_UNIT ( .MILLI., .METRE. ) );
#78318 = DIRECTION ( 'NONE',  ( -1.000000000000000000, 0.000000000000000000, 0.000000000000000000 ) ) ;
#78319 = DIRECTION ( 'NONE',  ( 1.000000000000000000, -0.000000000000000000, -0.000000000000000000 ) ) ;
#78320 = CARTESIAN_POINT ( 'NONE',  ( -84.47965975623978352, -35.89726040385875194, 177.6434332425895093 ) ) ;
#78321 = CARTESIAN_POINT ( 'NONE',  ( 39.10169391268793504, 42.03037277983941067, -56.74405835323407388 ) ) ;
#78322 = ADVANCED_FACE ( 'NONE', ( #54003, #56109 ), #21690, .F. ) ;
#78323 = AXIS2_PLACEMENT_3D ( 'NONE', #51745, #25942, #33469 ) ;
#78324 = ORIENTED_EDGE ( 'NONE', *, *, #53888, .F. ) ;
#78325 = CARTESIAN_POINT ( 'NONE',  ( 28.09999999999999787, -3.309499999999999886, 4.475777889183790779E-16 ) ) ;
#78326 = PRODUCT_DEFINITION_FORMATION_WITH_SPECIFIED_SOURCE ( 'ANY', '', #14054, .NOT_KNOWN. ) ;
#78327 = CARTESIAN_POINT ( 'NONE',  ( -85.24568900165127161, -52.70636524970269221, 2.598678943497877647 ) ) ;
#78328 = CARTESIAN_POINT ( 'NONE',  ( 33.77559172535807619, 464.7834715296606305, 7.192701217093271815 ) ) ;
#78329 = FILL_AREA_STYLE ('',( #4987 ) ) ;
#78330 = CARTESIAN_POINT ( 'NONE',  ( 2.849089834143495814, 70.33461465726148276, -5.000000000000000000 ) ) ;
#78331 = CARTESIAN_POINT ( 'NONE',  ( 7.000000000000000000, 0.000000000000000000, -11.82492182392400437 ) ) ;
#78332 = CARTESIAN_POINT ( 'NONE',  ( 36.40416150955762475, 42.00000000000001421, -47.37019975555940476 ) ) ;
#78333 = CARTESIAN_POINT ( 'NONE',  ( 91.09720049356627669, -14.21045842199416143, 197.8400994950010272 ) ) ;
#78334 = CARTESIAN_POINT ( 'NONE',  ( -33.83237027343564307, 58.72416816948007323, -16.91618513671782509 ) ) ;
#78335 = CARTESIAN_POINT ( 'NONE',  ( -88.56648999577124926, -14.21045842199433018, 40.40162738224969274 ) ) ;
#78336 = CARTESIAN_POINT ( 'NONE',  ( -65.80396453374501675, -42.96215446677902605, 90.41881760261397005 ) ) ;
#78337 = ORIENTED_EDGE ( 'NONE', *, *, #20768, .T. ) ;
#78338 = CARTESIAN_POINT ( 'NONE',  ( 96.06638400950703272, -14.21045842199450426, 198.0643409056117434 ) ) ;
#78339 = CARTESIAN_POINT ( 'NONE',  ( 58.89336504995121402, 39.42406911483853804, -28.14246176607905525 ) ) ;
#78340 = CARTESIAN_POINT ( 'NONE',  ( 45.81799851979177873, -59.99999999998037481, 67.88348539002272730 ) ) ;
#78341 = ORIENTED_EDGE ( 'NONE', *, *, #94786, .T. ) ;
#78342 = CARTESIAN_POINT ( 'NONE',  ( -30.00000000000000000, 450.0000000000002274, 18.20242257375371153 ) ) ;
#78343 = CARTESIAN_POINT ( 'NONE',  ( -5.082755093536326818, -21.59375000204838457, 5.082755093536325042 ) ) ;
#78344 = CARTESIAN_POINT ( 'NONE',  ( -5.382954851612916869, -7.000125085105551648, -2.657971597726727975 ) ) ;
#78345 = ORIENTED_EDGE ( 'NONE', *, *, #103254, .T. ) ;
#78346 = DIRECTION ( 'NONE',  ( -1.000000000000000000, -0.000000000000000000, -0.000000000000000000 ) ) ;
#78347 = EDGE_LOOP ( 'NONE', ( #56937, #77113, #89782, #47617, #10788 ) ) ;
#78348 = DIRECTION ( 'NONE',  ( -1.000000000000000000, -0.000000000000000000, -0.000000000000000000 ) ) ;
#78349 = CARTESIAN_POINT ( 'NONE',  ( 66.00571552735603120, 4.898587196589294500E-16, -4.000000000000007105 ) ) ;
#78350 = CARTESIAN_POINT ( 'NONE',  ( -5.591075928466159084, -60.00000000000000000, -42.57939663618462589 ) ) ;
#78351 = CARTESIAN_POINT ( 'NONE',  ( 36.49551160402948113, 361.0291929650597353, 2.682884907252832463 ) ) ;
#78352 = CARTESIAN_POINT ( 'NONE',  ( 5.082755093536324154, -33.21875000204838813, 5.082755093536326818 ) ) ;
#78353 = DIRECTION ( 'NONE',  ( -1.000000000000000000, -1.224606353822377258E-16, -0.000000000000000000 ) ) ;
#78354 = DIRECTION ( 'NONE',  ( 1.000000000000000000, -0.000000000000000000, -0.000000000000000000 ) ) ;
#78355 = CARTESIAN_POINT ( 'NONE',  ( -7.996668422912395435, 49.99999999999999289, -78.85453279917057046 ) ) ;
#78356 = CARTESIAN_POINT ( 'NONE',  ( 36.08349330513379982, 1.593028355512270567E-15, 0.000000000000000000 ) ) ;
#78357 = CARTESIAN_POINT ( 'NONE',  ( 38.39281685574057690, 437.9237591976291810, 4.303444208756668665 ) ) ;
#78358 = EDGE_CURVE ( 'NONE', #82223, #105779, #74072, .T. ) ;
#78359 = AXIS2_PLACEMENT_3D ( 'NONE', #56056, #54467, #79302 ) ;
#78360 = CARTESIAN_POINT ( 'NONE',  ( 44.78945892759311675, 6.123233995736770227E-16, -5.000000000000002665 ) ) ;
#78361 = B_SPLINE_CURVE_WITH_KNOTS ( 'NONE', 3,
 ( #41560, #99245, #84682, #59358, #9708, #33485, #67445, #92220, #100322, #1610, #35096, #49643, #50684, #42084 ),
 .UNSPECIFIED., .F., .F.,
 ( 4, 2, 2, 2, 2, 2, 4 ),
 ( 0.000000000000000000, 0.0008623664466435473864, 0.001724732893287094773, 0.003449465786574139672, 0.004311832233217661146, 0.005174198679861184355, 0.006898931573148161384 ),
 .UNSPECIFIED. ) ;
#78362 = VERTEX_POINT ( 'NONE', #89044 ) ;
#78363 = CARTESIAN_POINT ( 'NONE',  ( -9.538946952600159790, 53.58200059918309677, -1.988036826341423646 ) ) ;
#78364 = CARTESIAN_POINT ( 'NONE',  ( 5.437321008177463888, -2.342832151771340854, 104.0362115404844303 ) ) ;
#78366 = CARTESIAN_POINT ( 'NONE',  ( 34.86627658960016163, -42.96414815358550499, 35.91348275393595912 ) ) ;
#78365 = CARTESIAN_POINT ( 'NONE',  ( 4.650850488836845820, 52.17814524009082788, -6.203660599199528392 ) ) ;
#78367 = CARTESIAN_POINT ( 'NONE',  ( 3.088855081073062209E-15, -4.285714285714286476, 25.22241582816893413 ) ) ;
#78368 = VERTEX_POINT ( 'NONE', #4949 ) ;
#78369 = EDGE_CURVE ( 'NONE', #78737, #64826, #106345, .T. ) ;
#78370 = EDGE_CURVE ( 'NONE', #20128, #4337, #87880, .T. ) ;
#78371 = CARTESIAN_POINT ( 'NONE',  ( -22.43980529875399554, 26.07880074899891909, -30.97394950045124418 ) ) ;
#78373 = CARTESIAN_POINT ( 'NONE',  ( -5.500000000000007105, 42.00000000000000000, -65.90297133655424489 ) ) ;
#78372 = CARTESIAN_POINT ( 'NONE',  ( 32.46316046841738512, 488.6793347432256382, 9.801212136610072179 ) ) ;
#78374 = CARTESIAN_POINT ( 'NONE',  ( -12.50000000000000355, -3.000000000000001776, -76.70872284621019332 ) ) ;
#78375 = CARTESIAN_POINT ( 'NONE',  ( 9.999999999999996447, 15.00000000000000000, -10.00000000000000000 ) ) ;
#78376 = CIRCLE ( 'NONE', #50789, 15.00000000000000711 ) ;
#78377 = VECTOR ( 'NONE', #17330, 1000.000000000000000 ) ;
#78378 = CARTESIAN_POINT ( 'NONE',  ( -40.54863160047752046, 437.2386745228059794, 5.317148167338432430 ) ) ;
#78379 = VECTOR ( 'NONE', #61903, 1000.000000000000000 ) ;
#78380 = LINE ( 'NONE', #63810, #34554 ) ;
#78381 = CARTESIAN_POINT ( 'NONE',  ( -35.02700494599118031, 463.8298975055874962, 19.03023931479493314 ) ) ;
#78382 = EDGE_LOOP ( 'NONE', ( #75648, #62219, #35289, #71294 ) ) ;
#78383 = CARTESIAN_POINT ( 'NONE',  ( 92.64166564108928981, -60.00000000000000711, -3.519352460692061424 ) ) ;
#78384 = PRESENTATION_LAYER_ASSIGNMENT (  '', '', ( #33593 ) ) ;
#78385 = CARTESIAN_POINT ( 'NONE',  ( 21.08349330513380693, -3.851859888774471706E-31, 4.000000000000001776 ) ) ;
#78386 = AXIS2_PLACEMENT_3D ( 'NONE', #23259, #57180, #71771 ) ;
#78387 = CARTESIAN_POINT ( 'NONE',  ( -6.188824320863258954, 41.46400361745708807, -70.81766458224430494 ) ) ;
#78388 = DIRECTION ( 'NONE',  ( 1.000000000000000000, 0.000000000000000000, 0.000000000000000000 ) ) ;
#78389 = EDGE_LOOP ( 'NONE', ( #66654, #52242, #20863, #96007, #10135, #5780 ) ) ;
#78390 = ADVANCED_FACE ( 'NONE', ( #13546 ), #17290, .T. ) ;
#78391 = CARTESIAN_POINT ( 'NONE',  ( -81.04890366060243423, -29.99999999999316813, 192.7446792250348722 ) ) ;
#78392 = ORIENTED_EDGE ( 'NONE', *, *, #57181, .T. ) ;
#78393 = LINE ( 'NONE', #70841, #22798 ) ;
#78394 = CARTESIAN_POINT ( 'NONE',  ( 0.000000000000000000, 4.898587196589412829E-16, -4.000000000000000000 ) ) ;
#78395 = CARTESIAN_POINT ( 'NONE',  ( 14.66373388272351441, 22.41296547518495075, 3.537915336787654574 ) ) ;
#78396 = CARTESIAN_POINT ( 'NONE',  ( -6.500000000000000000, 3.453380256388198788, -0.6809028088495666653 ) ) ;
#78397 = CARTESIAN_POINT ( 'NONE',  ( -1.320432766682874540E-15, -30.40625000204838813, 7.188101187500000044 ) ) ;
#78398 = CARTESIAN_POINT ( 'NONE',  ( -16.75187969033532553, 34.99134772383131065, 21.80698433968612093 ) ) ;
#78399 = FILL_AREA_STYLE ('',( #45526 ) ) ;
#78400 =( BOUNDED_CURVE ( )  B_SPLINE_CURVE ( 2, ( #82247, #40731, #16454, #73618, #106521, #235, #66072, #80651, #98949, #25109, #31613, #57970, #90891, #17006, #49882, #6232, #72046, #63974, #64496, #23527, #96862, #22990, #34809, #1308, #2393, #27258, #50932, #43925, #9404, #67677, #19172, #9956, #68201, #83316, #74680, #76814, #41794, #100561, #60144, #93553, #35339, #26721, #17541, #51478, #59593, #92467, #91943, #1852, #27795, #42320, #35878, #18616, #33727, #50402, #84393, #84923, #26197, #42862, #93008, #100027, #101101, #11009, #10482, #52006, #2925, #99485, #68758, #101638, #75755, #75214, #60666, #59056, #58524, #34269, #19702, #83848, #82788, #760, #8890, #43402, #66607, #25662, #76284, #91429, #67146, #18073, #5064, #11541, #29892, #95147, #21806, #54646, #28309, #85455, #28859, #79472, #86542, #61185, #37998, #70861, #94627, #13668, #20772, #36414, #46058, #71374, #21280, #4004, #63311, #69799, #95666, #94072, #4525, #69284, #45538, #102159, #87058, #20240, #78411, #30417, #96207, #62778, #52535, #78942, #13130, #44465, #87580, #3472, #46576, #5583, #103752, #104275, #38508, #102696, #77360, #12078, #62262, #53086, #54117, #86008, #45009, #77893, #61732, #36934, #53607, #12601, #37471, #70332, #103230, #29373, #32006, #79996, #40603, #81051, #30962, #6105, #22863, #73486, #56775, #15798, #72442, #90220, #89164, #39031, #64370, #88109, #106384, #24466, #97243, #16324, #7165, #97766, #64881, #71912, #48152, #55700, #23933, #56226, #14190, #32546, #49215, #81563, #65418, #23388, #7692, #89698, #105345, #48679, #105864, #47620, #63838, #15269, #98313, #96731, #88631, #57301, #47094, #104813, #82113, #8233, #40077, #41144, #33079, #74028, #14721, #107, #65944, #22336, #55183, #31490, #80522, #72957, #6640, #39567, #34680, #66472, #58929, #67552, #630, #91824, #67020, #99900, #26073, #27123, #91301 ),
 .UNSPECIFIED., .F., .F. ) 
 B_SPLINE_CURVE_WITH_KNOTS ( ( 3, 2, 2, 2, 2, 2, 2, 2, 2, 2, 2, 2, 2, 2, 2, 2, 2, 2, 2, 2, 2, 2, 2, 2, 2, 2, 2, 2, 2, 2, 2, 2, 2, 2, 2, 2, 2, 2, 2, 2, 2, 2, 2, 2, 2, 2, 2, 2, 2, 2, 2, 2, 2, 2, 2, 2, 2, 2, 2, 2, 2, 2, 2, 2, 2, 2, 2, 2, 2, 2, 2, 2, 2, 2, 2, 2, 2, 2, 2, 2, 2, 2, 2, 2, 2, 2, 2, 2, 2, 2, 2, 2, 2, 2, 2, 2, 2, 2, 2, 2, 2, 2, 2, 2, 2, 2, 2, 2, 2, 2, 2, 2, 3 ),
 ( 0.1630438152594470835, 0.1691176470588235392, 0.1764705882352941291, 0.1838235294117647189, 0.1911764705882352811, 0.1985294117647058709, 0.2058823529411764608, 0.2132352941176470507, 0.2205882352941176405, 0.2279411764705882304, 0.2352941176470588203, 0.2426470588235294101, 0.2500000000000000000, 0.2573529411764705621, 0.2647058823529411797, 0.2720588235294117418, 0.2794117647058823595, 0.2867647058823529216, 0.2941176470588235392, 0.3014705882352941013, 0.3088235294117647189, 0.3161764705882352811, 0.3235294117647058987, 0.3308823529411764608, 0.3382352941176470784, 0.3455882352941176405, 0.3529411764705882582, 0.3602941176470588203, 0.3676470588235294379, 0.3750000000000000000, 0.3823529411764705621, 0.3897058823529411242, 0.3970588235294117418, 0.4044117647058823595, 0.4117647058823529216, 0.4191176470588235947, 0.4264705882352941568, 0.4338235294117647189, 0.4411764705882352811, 0.4485294117647059542, 0.4558823529411765163, 0.4632352941176470784, 0.4705882352941176405, 0.4779411764705883137, 0.4852941176470588758, 0.4926470588235294379, 0.5000000000000000000, 0.5073529411764705621, 0.5147058823529411242, 0.5220588235294117974, 0.5294117647058823595, 0.5367647058823529216, 0.5441176470588234837, 0.5514705882352941568, 0.5588235294117647189, 0.5661764705882352811, 0.5735294117647058432, 0.5808823529411765163, 0.5882352941176470784, 0.5955882352941176405, 0.6029411764705882026, 0.6102941176470588758, 0.6176470588235294379, 0.6250000000000000000, 0.6323529411764705621, 0.6397058823529410132, 0.6470588235294117974, 0.6544117647058823595, 0.6617647058823528106, 0.6691176470588234837, 0.6764705882352941568, 0.6838235294117647189, 0.6911764705882352811, 0.6985294117647058432, 0.7058823529411765163, 0.7132352941176470784, 0.7205882352941176405, 0.7279411764705882026, 0.7352941176470588758, 0.7426470588235294379, 0.7500000000000000000, 0.7573529411764705621, 0.7647058823529411242, 0.7720588235294117974, 0.7794117647058823595, 0.7867647058823529216, 0.7941176470588234837, 0.8014705882352941568, 0.8088235294117647189, 0.8161764705882352811, 0.8235294117647058432, 0.8308823529411765163, 0.8382352941176470784, 0.8455882352941176405, 0.8529411764705880916, 0.8602941176470588758, 0.8676470588235294379, 0.8750000000000000000, 0.8823529411764704511, 0.8897058823529411242, 0.8970588235294117974, 0.9044117647058823595, 0.9117647058823528106, 0.9191176470588234837, 0.9264705882352941568, 0.9338235294117647189, 0.9411764705882351700, 0.9485294117647058432, 0.9558823529411765163, 0.9632352941176470784, 0.9705882352941175295, 0.9779411764705882026, 0.9804062415945057340 ),
 .UNSPECIFIED. ) 
 CURVE ( )  GEOMETRIC_REPRESENTATION_ITEM ( )  RATIONAL_B_SPLINE_CURVE ( ( 0.9781234062028207887, 0.9371213634217766542, 1.000000000000000000, 0.9238795325112867385, 1.000000000000000000, 0.9238795325112867385, 1.000000000000000000, 0.9238795325112867385, 1.000000000000000000, 0.9238795325112867385, 1.000000000000000000, 0.9238795325112867385, 1.000000000000000000, 0.9238795325112867385, 1.000000000000000000, 0.9238795325112867385, 1.000000000000000000, 0.9238795325112867385, 1.000000000000000000, 0.9238795325112867385, 1.000000000000000000, 0.9238795325112867385, 1.000000000000000000, 0.9238795325112867385, 1.000000000000000000, 0.9238795325112867385, 1.000000000000000000, 0.9238795325112867385, 1.000000000000000000, 0.9238795325112867385, 1.000000000000000000, 0.9238795325112867385, 1.000000000000000000, 0.9238795325112867385, 1.000000000000000000, 0.9238795325112867385, 1.000000000000000000, 0.9238795325112867385, 1.000000000000000000, 0.9238795325112867385, 1.000000000000000000, 0.9238795325112867385, 1.000000000000000000, 0.9238795325112867385, 1.000000000000000000, 0.9238795325112867385, 1.000000000000000000, 0.9238795325112867385, 1.000000000000000000, 0.9238795325112867385, 1.000000000000000000, 0.9238795325112867385, 1.000000000000000000, 0.9238795325112867385, 1.000000000000000000, 0.9238795325112867385, 1.000000000000000000, 0.9238795325112867385, 1.000000000000000000, 0.9238795325112867385, 1.000000000000000000, 0.9238795325112867385, 1.000000000000000000, 0.9238795325112867385, 1.000000000000000000, 0.9238795325112867385, 1.000000000000000000, 0.9238795325112867385, 1.000000000000000000, 0.9238795325112867385, 1.000000000000000000, 0.9238795325112867385, 1.000000000000000000, 0.9238795325112867385, 1.000000000000000000, 0.9238795325112867385, 1.000000000000000000, 0.9238795325112867385, 1.000000000000000000, 0.9238795325112867385, 1.000000000000000000, 0.9238795325112867385, 1.000000000000000000, 0.9238795325112867385, 1.000000000000000000, 0.9238795325112867385, 1.000000000000000000, 0.9238795325112867385, 1.000000000000000000, 0.9238795325112867385, 1.000000000000000000, 0.9238795325112867385, 1.000000000000000000, 0.9238795325112867385, 1.000000000000000000, 0.9238795325112867385, 1.000000000000000000, 0.9238795325112867385, 1.000000000000000000, 0.9238795325112867385, 1.000000000000000000, 0.9238795325112867385, 1.000000000000000000, 0.9238795325112867385, 1.000000000000000000, 0.9238795325112867385, 1.000000000000000000, 0.9238795325112867385, 1.000000000000000000, 0.9238795325112867385, 1.000000000000000000, 0.9238795325112867385, 1.000000000000000000, 0.9238795325112867385, 1.000000000000000000, 0.9238795325112867385, 1.000000000000000000, 0.9238795325112867385, 1.000000000000000000, 0.9238795325112867385, 1.000000000000000000, 0.9238795325112867385, 1.000000000000000000, 0.9238795325112867385, 1.000000000000000000, 0.9238795325112867385, 1.000000000000000000, 0.9238795325112867385, 1.000000000000000000, 0.9238795325112867385, 1.000000000000000000, 0.9238795325112867385, 1.000000000000000000, 0.9238795325112867385, 1.000000000000000000, 0.9238795325112867385, 1.000000000000000000, 0.9238795325112867385, 1.000000000000000000, 0.9238795325112867385, 1.000000000000000000, 0.9238795325112867385, 1.000000000000000000, 0.9238795325112867385, 1.000000000000000000, 0.9238795325112867385, 1.000000000000000000, 0.9238795325112867385, 1.000000000000000000, 0.9238795325112867385, 1.000000000000000000, 0.9238795325112867385, 1.000000000000000000, 0.9238795325112867385, 1.000000000000000000, 0.9238795325112867385, 1.000000000000000000, 0.9238795325112867385, 1.000000000000000000, 0.9238795325112867385, 1.000000000000000000, 0.9238795325112867385, 1.000000000000000000, 0.9238795325112867385, 1.000000000000000000, 0.9238795325112867385, 1.000000000000000000, 0.9238795325112867385, 1.000000000000000000, 0.9238795325112867385, 1.000000000000000000, 0.9238795325112867385, 1.000000000000000000, 0.9238795325112867385, 1.000000000000000000, 0.9238795325112867385, 1.000000000000000000, 0.9238795325112867385, 1.000000000000000000, 0.9238795325112867385, 1.000000000000000000, 0.9238795325112867385, 1.000000000000000000, 0.9238795325112867385, 1.000000000000000000, 0.9238795325112867385, 1.000000000000000000, 0.9238795325112867385, 1.000000000000000000, 0.9238795325112867385, 1.000000000000000000, 0.9238795325112867385, 1.000000000000000000, 0.9238795325112867385, 1.000000000000000000, 0.9238795325112867385, 1.000000000000000000, 0.9238795325112867385, 1.000000000000000000, 0.9238795325112867385, 1.000000000000000000, 0.9238795325112867385, 1.000000000000000000, 0.9238795325112867385, 1.000000000000000000, 0.9238795325112867385, 1.000000000000000000, 0.9238795325112867385, 1.000000000000000000, 0.9238795325112867385, 1.000000000000000000, 0.9238795325112867385, 1.000000000000000000, 0.9238795325112867385, 1.000000000000000000, 0.9238795325112867385, 1.000000000000000000, 0.9238795325112867385, 1.000000000000000000, 0.9238795325112867385, 1.000000000000000000, 0.9238795325112867385, 1.000000000000000000, 0.9744807002913096206, 0.9660720326926630630 ) ) 
 REPRESENTATION_ITEM ( '' )  );
#78401 = EDGE_CURVE ( 'NONE', #45187, #96540, #5203, .T. ) ;
#78402 = CARTESIAN_POINT ( 'NONE',  ( 4.286263797015736595E-16, 0.5000000000000000000, 3.500000000000000000 ) ) ;
#78403 = ORIENTED_EDGE ( 'NONE', *, *, #78316, .T. ) ;
#78404 =( BOUNDED_CURVE ( )  B_SPLINE_CURVE ( 2, ( #24326, #1584, #9151, #82528, #49620, #83573, #15658, #9680, #81440 ),
 .UNSPECIFIED., .F., .F. ) 
 B_SPLINE_CURVE_WITH_KNOTS ( ( 3, 2, 2, 2, 3 ),
 ( 0.9558823529411764053, 0.9632352941176469674, 0.9705882352941176405, 0.9779411764705882026, 0.9804062224232821254 ),
 .UNSPECIFIED. ) 
 CURVE ( )  GEOMETRIC_REPRESENTATION_ITEM ( )  RATIONAL_B_SPLINE_CURVE ( ( 1.000000000000001110, 0.9238795325112856283, 1.000000000000000000, 0.9238795325112867385, 1.000000000000000000, 0.9238795325112867385, 1.000000000000000000, 0.9744808987591700999, 0.9660721634849256390 ) ) 
 REPRESENTATION_ITEM ( '' )  );
#78405 = EDGE_CURVE ( 'NONE', #34141, #26380, #18915, .T. ) ;
#78407 = ORIENTED_EDGE ( 'NONE', *, *, #43638, .F. ) ;
#78406 = DIRECTION ( 'NONE',  ( -0.000000000000000000, -0.000000000000000000, -1.000000000000000000 ) ) ;
#78408 = CARTESIAN_POINT ( 'NONE',  ( 78.59144040420308386, -39.49479029591388013, 137.4423273624143746 ) ) ;
#78409 = VERTEX_POINT ( 'NONE', #30300 ) ;
#78410 = CARTESIAN_POINT ( 'NONE',  ( -12.50000000000000533, 27.17581705516544233, -44.71521942845799202 ) ) ;
#78411 = CARTESIAN_POINT ( 'NONE',  ( 5.082755093536325930, -18.96875000204838457, -5.082755093536325042 ) ) ;
#78412 = AXIS2_PLACEMENT_3D ( 'NONE', #4013, #20249, #37482 ) ;
#78413 = CARTESIAN_POINT ( 'NONE',  ( -77.37445547080469055, -57.51897485848058977, 195.6910618928241092 ) ) ;
#78414 = ORIENTED_EDGE ( 'NONE', *, *, #24131, .T. ) ;
#78415 = CARTESIAN_POINT ( 'NONE',  ( -5.858881034796412202, -13.78586324002981733, 1.317748741875968355 ) ) ;
#78416 = CARTESIAN_POINT ( 'NONE',  ( -9.797936955406314041, 81.53328310229518650, -2.012343231877590899 ) ) ;
#78417 = CARTESIAN_POINT ( 'NONE',  ( 48.90230676976855051, 14.54998273526172170, -14.70096925929882659 ) ) ;
#78418 = CARTESIAN_POINT ( 'NONE',  ( 3.313708498984762496, -15.96875000409677270, 7.999999999999998224 ) ) ;
#78419 = DIRECTION ( 'NONE',  ( 0.000000000000000000, 1.000000000000000000, 0.000000000000000000 ) ) ;
#78420 = CARTESIAN_POINT ( 'NONE',  ( -2.500000000000011990, -30.00000000000000000, -31.87333704504306908 ) ) ;
#78421 = CARTESIAN_POINT ( 'NONE',  ( 5.000000000000000888, 6.123233995736767268E-16, 5.000000000000000000 ) ) ;
#78422 = CARTESIAN_POINT ( 'NONE',  ( 7.500000000000000000, -2.376982511157178735, -18.31627213068316351 ) ) ;
#78423 = CARTESIAN_POINT ( 'NONE',  ( 11.31153846153846132, 1.411358822780289120E-15, 0.000000000000000000 ) ) ;
#78424 = VECTOR ( 'NONE', #2815, 1000.000000000000000 ) ;
#78425 = DIRECTION ( 'NONE',  ( 0.000000000000000000, 0.000000000000000000, -1.000000000000000000 ) ) ;
#78426 = EDGE_LOOP ( 'NONE', ( #13057, #7250, #55743, #53566, #24508 ) ) ;
#78427 = CARTESIAN_POINT ( 'NONE',  ( -2.788175468594526141, -49.58758714223310449, 44.41557376465305396 ) ) ;
#78428 = CARTESIAN_POINT ( 'NONE',  ( 46.08349330513379982, 4.000000000000002665, 0.000000000000000000 ) ) ;
#78429 = CARTESIAN_POINT ( 'NONE',  ( -41.92281291883663386, 435.4200907145705060, 7.396891011706863139 ) ) ;
#78430 = CARTESIAN_POINT ( 'NONE',  ( -35.79466378710967689, -25.44173586393017672, -36.80375087642579501 ) ) ;
#78431 = CARTESIAN_POINT ( 'NONE',  ( -62.52618473358160855, -30.00000000000000355, 73.41945751082272409 ) ) ;
#78432 = DIRECTION ( 'NONE',  ( 0.000000000000000000, 1.000000000000000000, 0.000000000000000000 ) ) ;
#78433 = EDGE_CURVE ( 'NONE', #71046, #87574, #87468, .T. ) ;
#78434 = AXIS2_PLACEMENT_3D ( 'NONE', #6614, #39540, #17390 ) ;
#78435 = B_SPLINE_CURVE_WITH_KNOTS ( 'NONE', 3,
 ( #102150, #19693, #53600, #52528 ),
 .UNSPECIFIED., .F., .F.,
 ( 4, 4 ),
 ( 0.000000000000000000, 1.000000000000000000 ),
 .UNSPECIFIED. ) ;
#78436 = ORIENTED_EDGE ( 'NONE', *, *, #68784, .F. ) ;
#78437 = LINE ( 'NONE', #38026, #1386 ) ;
#78438 = CARTESIAN_POINT ( 'NONE',  ( 73.86952552712314457, -57.61841923349722094, 186.3992556594028542 ) ) ;
#78439 = CARTESIAN_POINT ( 'NONE',  ( 57.70227852311749217, -34.58945965303971093, -25.91729053135263072 ) ) ;
#78440 = EDGE_CURVE ( 'NONE', #27550, #67329, #19017, .T. ) ;
#78441 = EDGE_CURVE ( 'NONE', #61647, #31749, #6065, .T. ) ;
#78442 = CARTESIAN_POINT ( 'NONE',  ( 34.10284876471455817, 1.482358050883964840E-15, 0.000000000000000000 ) ) ;
#78443 = DIRECTION ( 'NONE',  ( 0.000000000000000000, -0.5000000000000008882, -0.8660254037844381525 ) ) ;
#78444 = COLOUR_RGB ( '', 0.09019608, 0.27058824, 0.51372549) ;
#78445 = CARTESIAN_POINT ( 'NONE',  ( 39.34999999999999432, 3.309500000000003439, 4.052968581778167743E-16 ) ) ;
#78446 = CARTESIAN_POINT ( 'NONE',  ( -69.13297650054198584, -60.00000000000000711, 136.7714041556835411 ) ) ;
#78447 = CIRCLE ( 'NONE', #49178, 3.309500000000001663 ) ;
#78448 = CONICAL_SURFACE ( 'NONE', #100846, 4.000000000000001776, 0.9599310885968774798 ) ;
#78449 = CARTESIAN_POINT ( 'NONE',  ( 93.39999999999999147, 1.023464760207051730E-14, 0.000000000000000000 ) ) ;
#78450 = CARTESIAN_POINT ( 'NONE',  ( 30.00000000000000000, 0.000000000000000000, 0.000000000000000000 ) ) ;
#78451 = EDGE_CURVE ( 'NONE', #60981, #67219, #63986, .T. ) ;
#78452 = CARTESIAN_POINT ( 'NONE',  ( 23.38163988262877879, 50.00000000002003731, 60.94087333794557537 ) ) ;
#78453 = CARTESIAN_POINT ( 'NONE',  ( -85.35106076031452460, -42.92912420381342287, 186.7164831997029353 ) ) ;
#78454 = ORIENTED_EDGE ( 'NONE', *, *, #94247, .F. ) ;
#78455 = CARTESIAN_POINT ( 'NONE',  ( 34.03884506130833643, 322.5454401300060567, -5.433161704552694538 ) ) ;
#78456 = LINE ( 'NONE', #87100, #16089 ) ;
#78457 = EDGE_CURVE ( 'NONE', #95757, #20727, #21578, .T. ) ;
#78458 = AXIS2_PLACEMENT_3D ( 'NONE', #31513, #90786, #105374 ) ;
#78459 = CARTESIAN_POINT ( 'NONE',  ( -5.441822498209519132, 41.96569345422851427, -59.31342656602353003 ) ) ;
#78460 = CARTESIAN_POINT ( 'NONE',  ( -2.352990130084491319E-16, 8.660254037844390851, -10.00000000000000000 ) ) ;
#78461 = LINE ( 'NONE', #27306, #33665 ) ;
#78462 = CARTESIAN_POINT ( 'NONE',  ( -24.08998881576893680, 304.6612033203863348, -9.825736866731734409 ) ) ;
#78463 = DIRECTION ( 'NONE',  ( 0.000000000000000000, 0.000000000000000000, 1.000000000000000000 ) ) ;
#78464 = DIRECTION ( 'NONE',  ( -1.000000000000000000, -1.224606353822377258E-16, -0.000000000000000000 ) ) ;
#78465 = CARTESIAN_POINT ( 'NONE',  ( -43.51084452654468748, 465.2903130129606666, 9.421687747985890482 ) ) ;
#78466 = ORIENTED_EDGE ( 'NONE', *, *, #79912, .F. ) ;
#78467 = CARTESIAN_POINT ( 'NONE',  ( 19.15405721169568309, 50.00000000000001421, 60.37683062052576588 ) ) ;
#78468 = CARTESIAN_POINT ( 'NONE',  ( 11.09614018901123345, 8.445801345000054638, 9.827501351701041443 ) ) ;
#78469 = CARTESIAN_POINT ( 'NONE',  ( -24.56594385547200687, -4.285714285715344296, -6.601913983219908744 ) ) ;
#78470 = CARTESIAN_POINT ( 'NONE',  ( 88.10210802036469602, -14.21045842199426090, 36.33415240954661840 ) ) ;
#78471 = CARTESIAN_POINT ( 'NONE',  ( -79.60561737478720090, -42.96939065557461390, 147.0952876792103723 ) ) ;
#78472 = EDGE_LOOP ( 'NONE', ( #60353, #18478, #64284 ) ) ;
#78473 = DIRECTION ( 'NONE',  ( 0.5735764363510470476, -0.8191520442889911324, 1.003171929053524007E-16 ) ) ;
#78474 = DIRECTION ( 'NONE',  ( -0.000000000000000000, -0.000000000000000000, -1.000000000000000000 ) ) ;
#78475 = CARTESIAN_POINT ( 'NONE',  ( 35.84708862202803914, -57.69601094548832521, 50.03348472163382610 ) ) ;
#78476 = CARTESIAN_POINT ( 'NONE',  ( 62.09765651784079665, 49.99999999999999289, -11.13245139057254107 ) ) ;
#78477 = CARTESIAN_POINT ( 'NONE',  ( 37.59065068584150282, 369.8620417756742995, 4.163880029477669886 ) ) ;
#78478 = CARTESIAN_POINT ( 'NONE',  ( 28.99999999999999645, 0.000000000000000000, 4.999999999999999112 ) ) ;
#78479 = ORIENTED_EDGE ( 'NONE', *, *, #97861, .T. ) ;
#78480 = FACE_OUTER_BOUND ( 'NONE', #29046, .T. ) ;
#78481 = CARTESIAN_POINT ( 'NONE',  ( -15.64282023038923697, 37.16738321503569864, 22.45670599646769006 ) ) ;
#78482 = CARTESIAN_POINT ( 'NONE',  ( 7.188101187500000044, -26.65625000204838813, 0.000000000000000000 ) ) ;
#78483 = CIRCLE ( 'NONE', #50906, 4.000000000000001776 ) ;
#78484 = CARTESIAN_POINT ( 'NONE',  ( -3.594033448928638297, -9.156975712238446974, 6.225088131883843801 ) ) ;
#78485 = CARTESIAN_POINT ( 'NONE',  ( 6.441910988235199476, 41.95837105961398095, -69.50559658456835166 ) ) ;
#78486 = CARTESIAN_POINT ( 'NONE',  ( 25.88368638486081252, 37.21352445278208165, 8.492507970579360688 ) ) ;
#78487 = CARTESIAN_POINT ( 'NONE',  ( 12.33349330513380337, -4.000000000000000000, 4.898587196589415787E-16 ) ) ;
#78488 = DIRECTION ( 'NONE',  ( -0.000000000000000000, 0.000000000000000000, -1.000000000000000000 ) ) ;
#78489 = ORIENTED_EDGE ( 'NONE', *, *, #26310, .T. ) ;
#78490 = CARTESIAN_POINT ( 'NONE',  ( 33.00000000000000000, 489.5971041675262541, 10.80646835458729349 ) ) ;
#78492 = CARTESIAN_POINT ( 'NONE',  ( 25.43823788892170512, -22.08888639596277059, 28.86576217263490918 ) ) ;
#78491 = CARTESIAN_POINT ( 'NONE',  ( -70.37903440132366484, -60.00000000000007816, 160.1141433014324207 ) ) ;
#78493 = CARTESIAN_POINT ( 'NONE',  ( 1.080918900219005715E-14, 34.25047185182970111, -44.13186320217320713 ) ) ;
#78494 = ORIENTED_EDGE ( 'NONE', *, *, #63071, .F. ) ;
#78495 = ADVANCED_FACE ( 'NONE', ( #3761 ), #79242, .T. ) ;
#78496 = UNCERTAINTY_MEASURE_WITH_UNIT (LENGTH_MEASURE( 1.000000000000000082E-05 ), #97084, 'distance_accuracy_value', 'NONE');
#78497 = ORIENTED_EDGE ( 'NONE', *, *, #7044, .T. ) ;
#78498 = CARTESIAN_POINT ( 'NONE',  ( 1.544427540536530710E-15, -4.285714285714290916, -25.22241582816893057 ) ) ;
#78499 = CARTESIAN_POINT ( 'NONE',  ( -7.347880794884118356E-15, 0.000000000000000000, 60.00000000000000000 ) ) ;
#78500 = CARTESIAN_POINT ( 'NONE',  ( -44.27172743694714541, 463.5980762766266707, 7.352902973895489858 ) ) ;
#78501 = CARTESIAN_POINT ( 'NONE',  ( 1.128238012697730275, 300.0000000000000000, 9.936150108905557943 ) ) ;
#78502 = CARTESIAN_POINT ( 'NONE',  ( -3.184843881676170261E-16, -5.788408252967908396, -2.974182810908594821 ) ) ;
#78503 = ORIENTED_EDGE ( 'NONE', *, *, #78457, .T. ) ;
#78504 = CARTESIAN_POINT ( 'NONE',  ( 0.000000000000000000, 6.928203230275506108, 4.000000000000007105 ) ) ;
#78505 =( GEOMETRIC_REPRESENTATION_CONTEXT ( 3 ) GLOBAL_UNCERTAINTY_ASSIGNED_CONTEXT ( ( #100093 ) ) GLOBAL_UNIT_ASSIGNED_CONTEXT ( ( #39456, #22224, #14079 ) ) REPRESENTATION_CONTEXT ( 'NONE', 'WORKASPACE' ) );
#78506 = CARTESIAN_POINT ( 'NONE',  ( 97.64160974789494674, -30.00000000000016698, 190.8108562078370767 ) ) ;
#78507 = CARTESIAN_POINT ( 'NONE',  ( -13.25913213669673674, 3.878272661654435183, 6.943805427999512503 ) ) ;
#78508 = CARTESIAN_POINT ( 'NONE',  ( -4.496882872040834478, -84.46211334510377355, 3.972797206970398509 ) ) ;
#78509 = CARTESIAN_POINT ( 'NONE',  ( 81.59429082848517112, -30.00000000000000000, -6.732068947242803247 ) ) ;
#78510 = CARTESIAN_POINT ( 'NONE',  ( 10.11650669486618881, 0.000000000000000000, 4.000000000000000888 ) ) ;
#78511 = VERTEX_POINT ( 'NONE', #61474 ) ;
#78512 = AXIS2_PLACEMENT_3D ( 'NONE', #6481, #79317, #5438 ) ;
#78513 = EDGE_LOOP ( 'NONE', ( #37909, #79250, #67898, #26798, #87243 ) ) ;
#78514 = ORIENTED_EDGE ( 'NONE', *, *, #43222, .F. ) ;
#78515 = FACE_OUTER_BOUND ( 'NONE', #11469, .T. ) ;
#78516 = DIRECTION ( 'NONE',  ( -1.000000000000000000, -1.224606353822377258E-16, -0.000000000000000000 ) ) ;
#78517 = CARTESIAN_POINT ( 'NONE',  ( -89.99999999999997158, -60.00000000000000000, 194.0238439516549818 ) ) ;
#78518 = CARTESIAN_POINT ( 'NONE',  ( -8.000000000000000000, -16.53125000409677270, -3.313708498984762496 ) ) ;
#78519 = CARTESIAN_POINT ( 'NONE',  ( -1.356500113650659367, -70.62225732679223711, 13.06381631859566816 ) ) ;
#78520 = CARTESIAN_POINT ( 'NONE',  ( -7.211357414135265209, -87.01146539934438806, 3.467230644691329466 ) ) ;
#78521 = PRESENTATION_STYLE_ASSIGNMENT (( #44044 ) ) ;
#78522 = ORIENTED_EDGE ( 'NONE', *, *, #69675, .F. ) ;
#78523 = EDGE_CURVE ( 'NONE', #37257, #104590, #30557, .T. ) ;
#78524 = CARTESIAN_POINT ( 'NONE',  ( 8.559508646656407649, -1.200000000000000030E-05, 4.031152949374444461 ) ) ;
#78525 = VERTEX_POINT ( 'NONE', #95414 ) ;
#78526 = CARTESIAN_POINT ( 'NONE',  ( -1.400734872026641709, 15.45478884909084272, -9.907647895771706459 ) ) ;
#78527 = LINE ( 'NONE', #12200, #62509 ) ;
#78528 = CARTESIAN_POINT ( 'NONE',  ( 31.17288985937226542, 438.0041457322897713, 21.19838952990721026 ) ) ;
#78529 = CIRCLE ( 'NONE', #106067, 4.000000000000007105 ) ;
#78530 = CARTESIAN_POINT ( 'NONE',  ( 24.23803912011595685, 304.0757452244806700, 10.20472470771674622 ) ) ;
#78531 = AXIS2_PLACEMENT_3D ( 'NONE', #51942, #76752, #84856 ) ;
#78532 = EDGE_CURVE ( 'NONE', #44978, #51593, #79752, .T. ) ;
#78533 = LINE ( 'NONE', #88235, #92349 ) ;
#78534 = CARTESIAN_POINT ( 'NONE',  ( 63.87320186146764911, -25.57903068207289010, 75.85531773732697047 ) ) ;
#78535 = CIRCLE ( 'NONE', #13151, 3.309500000000001663 ) ;
#78536 = EDGE_LOOP ( 'NONE', ( #31920, #19580, #61305, #8063 ) ) ;
#78537 = DIRECTION ( 'NONE',  ( 0.000000000000000000, 1.000000000000000000, 0.000000000000000000 ) ) ;
#78538 = CIRCLE ( 'NONE', #32053, 6.000000000000000888 ) ;
#78539 = CARTESIAN_POINT ( 'NONE',  ( -55.39206909923246513, -36.62708581283116160, -35.18495517365747105 ) ) ;
#78540 = CARTESIAN_POINT ( 'NONE',  ( 0.000000000000000000, 0.000000000000000000, -1.876475477074182940 ) ) ;
#78541 =( BOUNDED_CURVE ( )  B_SPLINE_CURVE ( 2, ( #49015, #97566, #23730, #48489, #81384, #43079, #91635, #58740, #99711 ),
 .UNSPECIFIED., .F., .F. ) 
 B_SPLINE_CURVE_WITH_KNOTS ( ( 3, 2, 2, 2, 3 ),
 ( 0.2794117647058823040, 0.2867647058823528661, 0.2941176470588234837, 0.3014705882352940458, 0.3088235294117646634 ),
 .UNSPECIFIED. ) 
 CURVE ( )  GEOMETRIC_REPRESENTATION_ITEM ( )  RATIONAL_B_SPLINE_CURVE ( ( 1.000000000000000666, 0.9238795325112861834, 1.000000000000000000, 0.9238795325112867385, 1.000000000000000000, 0.9238795325112867385, 1.000000000000000000, 0.9238795325112872936, 0.9999999999999994449 ) ) 
 REPRESENTATION_ITEM ( '' )  );
#78542 = CARTESIAN_POINT ( 'NONE',  ( 0.000000000000000000, 0.000000000000000000, 0.000000000000000000 ) ) ;
#78543 = ORIENTED_EDGE ( 'NONE', *, *, #91059, .F. ) ;
#78544 = DIRECTION ( 'NONE',  ( 1.000000000000000000, 0.000000000000000000, 0.000000000000000000 ) ) ;
#78545 = CYLINDRICAL_SURFACE ( 'NONE', #45078, 4.000000000000000000 ) ;
#78546 = DIRECTION ( 'NONE',  ( 0.000000000000000000, 1.000000000000000000, 0.000000000000000000 ) ) ;
#78547 = CARTESIAN_POINT ( 'NONE',  ( 43.75010090113893568, 464.8337800386751724, 11.75004750935173448 ) ) ;
#78548 = AXIS2_PLACEMENT_3D ( 'NONE', #9955, #93007, #26720 ) ;
#78549 = DIRECTION ( 'NONE',  ( 0.000000000000000000, 1.000000000000000000, -1.224646799147353207E-16 ) ) ;
#78550 = ADVANCED_FACE ( 'NONE', ( #64133 ), #73793, .T. ) ;
#78551 = CARTESIAN_POINT ( 'NONE',  ( -21.04247164025375483, 37.86482112153537116, 10.52123582012688274 ) ) ;
#78552 = DIRECTION ( 'NONE',  ( -0.5735764363510497121, 0.8191520442889892450, 1.003171929053521665E-16 ) ) ;
#78553 = CARTESIAN_POINT ( 'NONE',  ( 85.42961103274494405, -50.19169959065673225, 189.9708901157421508 ) ) ;
#78554 = CARTESIAN_POINT ( 'NONE',  ( -5.280320895393596281, 15.76435391921249263, -35.40122979677870063 ) ) ;
#78555 = CARTESIAN_POINT ( 'NONE',  ( -9.596328384832000680, 8.973060046492864927, 5.000000000000158984 ) ) ;
#78556 = CARTESIAN_POINT ( 'NONE',  ( 7.934883677559682269, -6.131608220624498173, 1.051380792122689423 ) ) ;
#78557 = CARTESIAN_POINT ( 'NONE',  ( -7.894787914004607998, -1.231000152045941975E-13, -7.591390474663426424 ) ) ;
#78558 = DIRECTION ( 'NONE',  ( 0.000000000000000000, -1.000000000000000000, 0.000000000000000000 ) ) ;
#78559 = CARTESIAN_POINT ( 'NONE',  ( -100.3697800338488690, -30.00000000000000355, 157.6853798804383757 ) ) ;
#78560 = CARTESIAN_POINT ( 'NONE',  ( 0.000000000000000000, 44.50000000000000711, 0.000000000000000000 ) ) ;
#78561 = CARTESIAN_POINT ( 'NONE',  ( 2.872543100939889182, -57.67120699056544453, 41.60709250352346089 ) ) ;
#78563 = FACE_BOUND ( 'NONE', #5889, .T. ) ;
#78562 = CARTESIAN_POINT ( 'NONE',  ( 9.058705124515451956, 43.97099215302630171, 13.86878051210034180 ) ) ;
#78564 = EDGE_CURVE ( 'NONE', #46974, #11179, #6939, .T. ) ;
#78565 = CARTESIAN_POINT ( 'NONE',  ( -38.81358894280271699, 485.1131561813180042, -4.191378885296423995 ) ) ;
#78566 = DIRECTION ( 'NONE',  ( 0.000000000000000000, 1.000000000000000000, 0.000000000000000000 ) ) ;
#78567 = FILL_AREA_STYLE_COLOUR ( '', #42534 ) ;
#78568 = CARTESIAN_POINT ( 'NONE',  ( 43.97892253342649127, 485.8746234538170938, 4.637105959624745033 ) ) ;
#78569 = B_SPLINE_CURVE_WITH_KNOTS ( 'NONE', 3,
 ( #96981, #78650, #30683, #103477, #63028, #55435, #5323, #13387, #55956, #13918, #63570, #61986, #5834, #78136, #103996, #94878, #87304, #12858, #46309, #79200 ),
 .UNSPECIFIED., .F., .F.,
 ( 4, 2, 2, 2, 2, 2, 2, 2, 2, 4 ),
 ( 0.003027256308175210915, 0.003532084672752785343, 0.004036913037330358903, 0.004541741401907933330, 0.005046569766485507758, 0.005298983948774298007, 0.005551398131063089124, 0.006056226495640661817, 0.006561054860218235377, 0.007065883224795808069 ),
 .UNSPECIFIED. ) ;
#78570 = SURFACE_SIDE_STYLE ('',( #14353 ) ) ;
#78571 = ORIENTED_EDGE ( 'NONE', *, *, #58100, .T. ) ;
#78572 = CARTESIAN_POINT ( 'NONE',  ( 36.84999999999999432, 3.309500000000003439, 0.000000000000000000 ) ) ;
#78573 = LINE ( 'NONE', #96896, #17727 ) ;
#78574 = CARTESIAN_POINT ( 'NONE',  ( -19.74050068906625910, -22.07241655641780298, 28.03316789096357908 ) ) ;
#78575 = EDGE_CURVE ( 'NONE', #106154, #6487, #29142, .T. ) ;
#78576 = EDGE_CURVE ( 'NONE', #76274, #5888, #23141, .T. ) ;
#78578 = CARTESIAN_POINT ( 'NONE',  ( 0.6444270201114900010, 37.14712638292468228, -27.41604988274115939 ) ) ;
#78577 = CARTESIAN_POINT ( 'NONE',  ( -97.58016201383395583, -60.00000000000002132, 100.9982337082133625 ) ) ;
#78579 = CIRCLE ( 'NONE', #1015, 8.500000000000000000 ) ;
#78580 = ORIENTED_EDGE ( 'NONE', *, *, #57222, .T. ) ;
#78581 =( NAMED_UNIT ( * ) SI_UNIT ( $, .STERADIAN. ) SOLID_ANGLE_UNIT ( ) );
#78582 = ORIENTED_EDGE ( 'NONE', *, *, #28311, .F. ) ;
#78583 = CARTESIAN_POINT ( 'NONE',  ( 34.10284876471455817, 1.482358050883964840E-15, 0.000000000000000000 ) ) ;
#78584 = COLOUR_RGB ( '', 0.40784314, 0.44705882, 0.49803922) ;
#78585 = FACE_OUTER_BOUND ( 'NONE', #94123, .T. ) ;
#78586 = DIRECTION ( 'NONE',  ( -1.000000000000000000, -1.224606353822377258E-16, -0.000000000000000000 ) ) ;
#78587 = VERTEX_POINT ( 'NONE', #70613 ) ;
#78588 = CARTESIAN_POINT ( 'NONE',  ( 7.360624614871775329, 50.00000000000001421, -75.38987561219505551 ) ) ;
#78589 = AXIS2_PLACEMENT_3D ( 'NONE', #36697, #78168, #5358 ) ;
#78590 = CARTESIAN_POINT ( 'NONE',  ( 101.6883679399455360, -45.28236933294770239, 189.9366059431119140 ) ) ;
#78591 = STYLED_ITEM ( 'NONE', ( #92800 ), #37161 ) ;
#78592 = CARTESIAN_POINT ( 'NONE',  ( 99.17777777777777715, 4.172000000000019249, 0.000000000000000000 ) ) ;
#78593 = ORIENTED_EDGE ( 'NONE', *, *, #69142, .T. ) ;
#78594 = ORIENTED_EDGE ( 'NONE', *, *, #23247, .F. ) ;
#78595 = AXIS2_PLACEMENT_3D ( 'NONE', #90518, #16631, #58696 ) ;
#78596 = ORIENTED_EDGE ( 'NONE', *, *, #56998, .T. ) ;
#78597 = CARTESIAN_POINT ( 'NONE',  ( 19.70764564238373495, 304.7954121406194190, 9.925013215726725235 ) ) ;
#78598 = CARTESIAN_POINT ( 'NONE',  ( 69.67238219402268840, 6.975173280561618775E-15, 0.000000000000000000 ) ) ;
#78599 = VERTEX_POINT ( 'NONE', #62528 ) ;
#78600 = DIRECTION ( 'NONE',  ( 0.000000000000000000, 0.000000000000000000, 1.000000000000000000 ) ) ;
#78601 = CARTESIAN_POINT ( 'NONE',  ( -7.009057377284643842, 5.325693897448008585, -4.838501632524188523 ) ) ;
#78602 = CARTESIAN_POINT ( 'NONE',  ( -95.11134242253905313, -60.00000000001936939, -8.936519196967090295 ) ) ;
#78603 = B_SPLINE_CURVE_WITH_KNOTS ( 'NONE', 3,
 ( #84245, #68055, #20635, #43781, #42721, #18470 ),
 .UNSPECIFIED., .F., .F.,
 ( 4, 2, 4 ),
 ( 0.004444412883774349725, 0.006655097293744438938, 0.008865781703714527284 ),
 .UNSPECIFIED. ) ;
#78604 = FACE_OUTER_BOUND ( 'NONE', #3127, .T. ) ;
#78605 = CARTESIAN_POINT ( 'NONE',  ( 36.83392883285972630, -60.00000000000000000, 48.18703564933022676 ) ) ;
#78606 = LINE ( 'NONE', #62977, #66669 ) ;
#78607 = CARTESIAN_POINT ( 'NONE',  ( -5.898965146263452475, 41.68848200487053646, -58.70906998136139521 ) ) ;
#78609 = CARTESIAN_POINT ( 'NONE',  ( 8.139917744429576274, -35.99157900641900198, 29.88135676800304807 ) ) ;
#78608 = CARTESIAN_POINT ( 'NONE',  ( -93.38368407206768040, -29.99999999999995026, 56.44986585522355682 ) ) ;
#78610 = EDGE_CURVE ( 'NONE', #37114, #91829, #67259, .T. ) ;
#78611 = CARTESIAN_POINT ( 'NONE',  ( -48.14002044170912598, -25.68398854815584187, 43.60758539631409292 ) ) ;
#78612 = CARTESIAN_POINT ( 'NONE',  ( 0.000000000000000000, 34.08768991669519721, -35.82893434829263413 ) ) ;
#78613 = VERTEX_POINT ( 'NONE', #22080 ) ;
#78614 = CARTESIAN_POINT ( 'NONE',  ( 4.733165431326070832E-26, 13.70447791526910919, -49.25000000000000000 ) ) ;
#78615 = CARTESIAN_POINT ( 'NONE',  ( 0.000000000000000000, 0.000000000000000000, 0.000000000000000000 ) ) ;
#78616 = DIRECTION ( 'NONE',  ( 0.000000000000000000, 0.000000000000000000, -1.000000000000000000 ) ) ;
#78617 = EDGE_LOOP ( 'NONE', ( #10589, #5186, #59007, #27602, #105075 ) ) ;
#78618 = CARTESIAN_POINT ( 'NONE',  ( -6.594435029803459969, -7.011724847875096422, 13.88183737994264177 ) ) ;
#78619 = EDGE_LOOP ( 'NONE', ( #54464, #96722, #106510, #78454 ) ) ;
#78620 = CARTESIAN_POINT ( 'NONE',  ( 93.77331375627365162, -29.99999999994636113, 59.18492225089448056 ) ) ;
#78621 = CARTESIAN_POINT ( 'NONE',  ( 3.358578016107375053, -49.02765317499759590, 104.2746939430699200 ) ) ;
#78622 = CARTESIAN_POINT ( 'NONE',  ( 33.00000000000000000, 500.0000000000002274, 12.00000000000000711 ) ) ;
#78623 = CARTESIAN_POINT ( 'NONE',  ( -10.04205104296119622, 18.64316884715858080, 37.36680950591986772 ) ) ;
#78624 = CARTESIAN_POINT ( 'NONE',  ( 95.61654509437354932, -30.00000000000000000, 191.3219847211079241 ) ) ;
#78625 = EDGE_CURVE ( 'NONE', #104368, #63843, #77563, .T. ) ;
#78626 = CARTESIAN_POINT ( 'NONE',  ( 0.08285530295198710593, 1.570896314769988811, 7.999999999999996447 ) ) ;
#78627 = ORIENTED_EDGE ( 'NONE', *, *, #20778, .T. ) ;
#78628 = ORIENTED_EDGE ( 'NONE', *, *, #89999, .F. ) ;
#78629 = VERTEX_POINT ( 'NONE', #54935 ) ;
#78630 = CARTESIAN_POINT ( 'NONE',  ( 54.17857857744175476, -18.69473100391316933, 50.60200713917969040 ) ) ;
#78631 = CARTESIAN_POINT ( 'NONE',  ( -46.00000000000001421, 436.1447960644705404, 9.230581956296642687 ) ) ;
#78632 = CARTESIAN_POINT ( 'NONE',  ( -80.00000000000000000, -52.00000000000000000, -21.09707704303352926 ) ) ;
#78633 = ORIENTED_EDGE ( 'NONE', *, *, #92768, .F. ) ;
#78634 = CARTESIAN_POINT ( 'NONE',  ( -16.02333492353049138, 4.076663811951506844, -2.240748598612071429 ) ) ;
#78635 = EDGE_LOOP ( 'NONE', ( #94395, #48987, #59288, #39795 ) ) ;
#78636 = SURFACE_STYLE_USAGE ( .BOTH. , #52783 ) ;
#78637 = CARTESIAN_POINT ( 'NONE',  ( 88.66533242839328466, -38.54123067826672155, 200.1820925585725206 ) ) ;
#78638 = CARTESIAN_POINT ( 'NONE',  ( 12.32576155738170520, 22.37954607397292150, 6.324133886429093465 ) ) ;
#78639 = CARTESIAN_POINT ( 'NONE',  ( 85.02584152012659047, -52.70748002918131192, 6.452569411773205310 ) ) ;
#78640 = CARTESIAN_POINT ( 'NONE',  ( 6.169949891408688991, -4.949864754179184700, 4.426582755167964400 ) ) ;
#78641 = CARTESIAN_POINT ( 'NONE',  ( 40.94500826520420134, 409.4144549123020056, 27.74959626577850713 ) ) ;
#78642 = CARTESIAN_POINT ( 'NONE',  ( 7.999999999999998224, -24.78125000409677270, 3.313708498984766049 ) ) ;
#78643 = EDGE_CURVE ( 'NONE', #24672, #12817, #36265, .T. ) ;
#78644 = DIRECTION ( 'NONE',  ( 0.000000000000000000, -1.000000000000000000, 0.000000000000000000 ) ) ;
#78645 = VECTOR ( 'NONE', #18610, 1000.000000000000000 ) ;
#78646 = ORIENTED_EDGE ( 'NONE', *, *, #59087, .T. ) ;
#78647 = ADVANCED_FACE ( 'NONE', ( #78163 ), #13413, .F. ) ;
#78648 = LINE ( 'NONE', #61983, #72052 ) ;
#78649 = CARTESIAN_POINT ( 'NONE',  ( -35.25431541795652635, 462.2816602437375764, 4.574345776432286570 ) ) ;
#78650 = CARTESIAN_POINT ( 'NONE',  ( -26.94510944316361645, 36.66031116801333667, 10.05698433968617245 ) ) ;
#78651 = ORIENTED_EDGE ( 'NONE', *, *, #70412, .F. ) ;
#78652 = CARTESIAN_POINT ( 'NONE',  ( -5.125978502509880741, 54.24780662741380866, 6.031152949374397387 ) ) ;
#78653 = CARTESIAN_POINT ( 'NONE',  ( -38.13184040399831787, 310.3448107234241888, 5.627667502867490512 ) ) ;
#78654 = CARTESIAN_POINT ( 'NONE',  ( -11.72777639069216526, -4.888764693000935857, -76.94183081657440937 ) ) ;
#78655 = DIRECTION ( 'NONE',  ( -1.000000000000000000, -1.224606353822377258E-16, -0.000000000000000000 ) ) ;
#78656 = CARTESIAN_POINT ( 'NONE',  ( -3.313708498984765161, -18.96875000000000000, 7.999999999999998224 ) ) ;
#78657 = CIRCLE ( 'NONE', #45954, 7.000000000000006217 ) ;
#78659 = CARTESIAN_POINT ( 'NONE',  ( -39.73807737788186500, -28.46602993620439648, 46.96015580672782619 ) ) ;
#78658 = AXIS2_PLACEMENT_3D ( 'NONE', #73536, #88684, #39087 ) ;
#78660 = MECHANICAL_DESIGN_GEOMETRIC_PRESENTATION_REPRESENTATION (  '', ( #21818 ), #80428 ) ;
#78661 = VECTOR ( 'NONE', #15424, 1000.000000000000000 ) ;
#78662 = CARTESIAN_POINT ( 'NONE',  ( 96.28888888888889142, -4.171999999999998820, 5.616230220889773285E-16 ) ) ;
#78663 = AXIS2_PLACEMENT_3D ( 'NONE', #55501, #74355, #64689 ) ;
#78664 = ORIENTED_EDGE ( 'NONE', *, *, #91818, .F. ) ;
#78665 = CARTESIAN_POINT ( 'NONE',  ( 82.47298783150054646, -60.81518142251732684, 189.3310907902461224 ) ) ;
#78666 = CARTESIAN_POINT ( 'NONE',  ( -49.24306615471302706, 8.188742177551265655, 15.29695692017770803 ) ) ;
#78667 =( NAMED_UNIT ( * ) PLANE_ANGLE_UNIT ( ) SI_UNIT ( $, .RADIAN. ) );
#78668 = ORIENTED_EDGE ( 'NONE', *, *, #27166, .F. ) ;
#78669 = ADVANCED_FACE ( 'NONE', ( #4282 ), #25948, .T. ) ;
#78670 = CARTESIAN_POINT ( 'NONE',  ( -83.97903783031063085, -37.82227734234454886, 36.92279524269413571 ) ) ;
#78671 = COLOUR_RGB ( '', 0.72549020, 0.75294118, 0.79215686) ;
#78672 = CARTESIAN_POINT ( 'NONE',  ( 29.34999999999999787, -3.309499999999999886, 4.475777889183790779E-16 ) ) ;
#78673 = DIRECTION ( 'NONE',  ( 1.000000000000000000, 1.224606353822377258E-16, 0.000000000000000000 ) ) ;
#78674 = CARTESIAN_POINT ( 'NONE',  ( -30.64348173561394617, 7.829960647508013238, 41.65811975367132902 ) ) ;
#78675 = PRESENTATION_LAYER_ASSIGNMENT (  '', '', ( #78749 ) ) ;
#78676 = SURFACE_SIDE_STYLE ('',( #62523 ) ) ;
#78677 = B_SPLINE_CURVE_WITH_KNOTS ( 'NONE', 3,
 ( #79442, #46028, #70830, #89136, #87552, #47593, #78910, #80490, #55668, #104783, #39000, #105317, #54087, #14160, #46548, #29866, #56197, #62745, #72924, #23361 ),
 .UNSPECIFIED., .F., .F.,
 ( 4, 2, 2, 2, 2, 2, 2, 2, 2, 4 ),
 ( 0.000000000000000000, 0.0008428829220942208418, 0.001685765844188442551, 0.002528648766282664152, 0.003371531688376885969, 0.004214414610471107353, 0.005057297532565329171, 0.005478738993612435743, 0.005900180454659542315, 0.006743063376753731172 ),
 .UNSPECIFIED. ) ;
#78678 = FILL_AREA_STYLE ('',( #36688 ) ) ;
#78679 = CARTESIAN_POINT ( 'NONE',  ( -30.00000000000000000, -54.00000000000000711, 31.11721482942554928 ) ) ;
#78680 = CARTESIAN_POINT ( 'NONE',  ( 2.519529083135021441, -0.4213828544525365372, 103.1541576364168122 ) ) ;
#78681 = CARTESIAN_POINT ( 'NONE',  ( 39.81984205663119525, -26.24841966675792193, 35.84685613074071142 ) ) ;
#78683 = CARTESIAN_POINT ( 'NONE',  ( -14.41717015766604604, 21.44666408806050129, 5.359973845151366767 ) ) ;
#78682 = CARTESIAN_POINT ( 'NONE',  ( -1.908195823574487804E-14, -8.660254037844390851, -0.9999999999999974465 ) ) ;
#78684 = CARTESIAN_POINT ( 'NONE',  ( 1.338640380261408858, 297.3185856422899178, -10.00123718159648689 ) ) ;
#78685 = CARTESIAN_POINT ( 'NONE',  ( 40.85254446136673323, 441.7500193615117610, 25.53625856138344474 ) ) ;
#78686 = CARTESIAN_POINT ( 'NONE',  ( 40.86653802755286335, 319.2575511279100056, 3.927576133266500680 ) ) ;
#78687 = CARTESIAN_POINT ( 'NONE',  ( -5.601730134768053482, 12.35429686688392970, -12.97150009825810280 ) ) ;
#78688 = CARTESIAN_POINT ( 'NONE',  ( -97.17403402573184223, -38.00000000000000711, 120.7837554639863384 ) ) ;
#78689 = AXIS2_PLACEMENT_3D ( 'NONE', #93491, #19638, #68137 ) ;
#78690 = ORIENTED_EDGE ( 'NONE', *, *, #95754, .T. ) ;
#78691 = CARTESIAN_POINT ( 'NONE',  ( -10.32127027360808569, -0.7831254332910545513, 20.16036387503780958 ) ) ;
#78692 = VECTOR ( 'NONE', #94615, 1000.000000000000114 ) ;
#78693 = EDGE_CURVE ( 'NONE', #97345, #4171, #78095, .T. ) ;
#78694 = DIRECTION ( 'NONE',  ( 0.000000000000000000, -1.000000000000000000, 0.000000000000000000 ) ) ;
#78695 = EDGE_CURVE ( 'NONE', #64476, #90846, #70475, .T. ) ;
#78697 = CARTESIAN_POINT ( 'NONE',  ( 4.826816438350578942, -60.22815652793605778, -36.87038698696663630 ) ) ;
#78696 = CARTESIAN_POINT ( 'NONE',  ( 0.000000000000000000, -0.1944580884125578779, -19.78098730681987405 ) ) ;
#78698 = ORIENTED_EDGE ( 'NONE', *, *, #15436, .F. ) ;
#78699 = CARTESIAN_POINT ( 'NONE',  ( 17.50000000000000711, -2.499999999999999556, 25.00000000000000000 ) ) ;
#78700 =( LENGTH_UNIT ( ) NAMED_UNIT ( * ) SI_UNIT ( .MILLI., .METRE. ) );
#78701 = VERTEX_POINT ( 'NONE', #47903 ) ;
#78702 = EDGE_CURVE ( 'NONE', #79305, #60384, #12107, .T. ) ;
#78703 = CARTESIAN_POINT ( 'NONE',  ( 30.59734358679082789, 7.793378852367167653, -41.71107540015051285 ) ) ;
#78704 = CARTESIAN_POINT ( 'NONE',  ( 0.000000000000000000, 0.000000000000000000, 0.000000000000000000 ) ) ;
#78705 = CARTESIAN_POINT ( 'NONE',  ( -92.73353799494898908, -60.00000000000002132, -5.996388734087326533 ) ) ;
#78706 = ORIENTED_EDGE ( 'NONE', *, *, #80372, .T. ) ;
#78707 = CARTESIAN_POINT ( 'NONE',  ( 8.000000000000000000, 9.797174393178825657E-16, -11.12471428571428689 ) ) ;
#78708 = FILL_AREA_STYLE ('',( #21070 ) ) ;
#78709 = CARTESIAN_POINT ( 'NONE',  ( -9.918512371096300129, 26.20717007729448511, -1.297150762882706143 ) ) ;
#78710 = TOROIDAL_SURFACE ( 'NONE', #6343, 12.00000000000000711, 3.000000000000000000 ) ;
#78711 = DIRECTION ( 'NONE',  ( -1.000000000000000000, -1.224606353822377258E-16, -0.000000000000000000 ) ) ;
#78712 = CARTESIAN_POINT ( 'NONE',  ( -84.57683538449640537, -25.55585145918435686, 162.3719968557960840 ) ) ;
#78713 = VECTOR ( 'NONE', #31481, 1000.000000000000000 ) ;
#78714 = ORIENTED_EDGE ( 'NONE', *, *, #46707, .F. ) ;
#78715 = CARTESIAN_POINT ( 'NONE',  ( 0.000000000000000000, 0.000000000000000000, -3.725171428571429022 ) ) ;
#78716 = EDGE_LOOP ( 'NONE', ( #22802, #60886, #16416, #936, #89695 ) ) ;
#78717 = VERTEX_POINT ( 'NONE', #98059 ) ;
#78718 = CARTESIAN_POINT ( 'NONE',  ( 16.28378713908861997, -4.332661967062005459, -8.128475758628217918 ) ) ;
#78719 = CARTESIAN_POINT ( 'NONE',  ( -5.608211814930418093, -65.93615317932940911, 14.17185745138047537 ) ) ;
#78720 = FILL_AREA_STYLE ('',( #70651 ) ) ;
#78721 = ORIENTED_EDGE ( 'NONE', *, *, #105959, .T. ) ;
#78722 = CARTESIAN_POINT ( 'NONE',  ( -31.84025840404170182, 489.2001951420293722, 8.970820463101537356 ) ) ;
#78723 = SURFACE_SIDE_STYLE ('',( #11327 ) ) ;
#78724 = CARTESIAN_POINT ( 'NONE',  ( -104.7047915100801987, -57.67116545479915857, 96.89679091199744221 ) ) ;
#78725 = CARTESIAN_POINT ( 'NONE',  ( 7.619753052866895970, -13.17451502807175068, -2.447276542590446802 ) ) ;
#78726 = DIRECTION ( 'NONE',  ( 1.000000000000000000, 1.224606353822377258E-16, 0.000000000000000000 ) ) ;
#78727 = CARTESIAN_POINT ( 'NONE',  ( -9.253800200985681457, 103.6998966891182761, -3.791983798715486298 ) ) ;
#78728 = CARTESIAN_POINT ( 'NONE',  ( -13.95281146043403098, -50.20507689203379442, 25.82616780902253950 ) ) ;
#78729 = AXIS2_PLACEMENT_3D ( 'NONE', #40003, #57221, #30335 ) ;
#78730 = CARTESIAN_POINT ( 'NONE',  ( 78.96299857857128757, -14.21045842199439946, -22.44940295094700033 ) ) ;
#78731 = CARTESIAN_POINT ( 'NONE',  ( -43.57786082180619047, -59.99999999999987921, 62.86006299602857439 ) ) ;
#78732 = EDGE_CURVE ( 'NONE', #15446, #38219, #41417, .T. ) ;
#78733 = CARTESIAN_POINT ( 'NONE',  ( -55.42316588243139108, -36.03017795024024394, 59.79689301410119384 ) ) ;
#78734 = EDGE_LOOP ( 'NONE', ( #29592, #73182, #43378, #54884 ) ) ;
#78735 = SURFACE_STYLE_FILL_AREA ( #37270 ) ;
#78736 = AXIS2_PLACEMENT_3D ( 'NONE', #36545, #77498, #96206 ) ;
#78737 = VERTEX_POINT ( 'NONE', #89975 ) ;
#78738 = CIRCLE ( 'NONE', #33984, 3.309500000000001663 ) ;
#78739 = CARTESIAN_POINT ( 'NONE',  ( -101.2069807466581750, -45.26418589157207606, 190.9419624999435996 ) ) ;
#78740 = AXIS2_PLACEMENT_3D ( 'NONE', #102102, #85402, #2870 ) ;
#78741 = CARTESIAN_POINT ( 'NONE',  ( 4.699999999999999289, -7.505553499465137612, 3.546421054897781431E-16 ) ) ;
#78742 = EDGE_CURVE ( 'NONE', #43261, #83753, #103426, .T. ) ;
#78743 = ORIENTED_EDGE ( 'NONE', *, *, #67384, .F. ) ;
#78744 = CARTESIAN_POINT ( 'NONE',  ( 19.31802113242206786, 49.87598122772962483, 61.28462200380675995 ) ) ;
#78745 = CARTESIAN_POINT ( 'NONE',  ( 68.70539558375507738, 4.000000000000015099, 4.898587196589422689E-16 ) ) ;
#78746 = CARTESIAN_POINT ( 'NONE',  ( 37.24599997783883509, 25.86608068541391958, -10.98719536802521368 ) ) ;
#78747 = CARTESIAN_POINT ( 'NONE',  ( -2.977408999572654480, -17.00000000204838457, 7.188101187499999156 ) ) ;
#78748 = FACE_OUTER_BOUND ( 'NONE', #10417, .T. ) ;
#78749 = STYLED_ITEM ( 'NONE', ( #27570 ), #15853 ) ;
#78750 = DIRECTION ( 'NONE',  ( -1.000000000000000000, -1.224606353822377258E-16, -0.000000000000000000 ) ) ;
#78751 = CARTESIAN_POINT ( 'NONE',  ( 6.943482370013978944, -84.47151629739272494, 3.973876482044368164 ) ) ;
#78752 = CARTESIAN_POINT ( 'NONE',  ( 69.76690891810729056, -30.00000000000001421, 94.57972461657990948 ) ) ;
#78753 = VECTOR ( 'NONE', #66824, 1000.000000000000000 ) ;
#78754 = CARTESIAN_POINT ( 'NONE',  ( 4.472135954999580498, -10.00000000000000888, 4.000000000000000000 ) ) ;
#78755 = ADVANCED_FACE ( 'NONE', ( #16079 ), #56523, .T. ) ;
#78756 = CARTESIAN_POINT ( 'NONE',  ( 4.302760725356077565, -48.89765558026142145, 104.4121068519184945 ) ) ;
#78757 = CARTESIAN_POINT ( 'NONE',  ( 4.898587196589412829E-16, -24.12499999999999289, -8.000000000000000000 ) ) ;
#78758 = CARTESIAN_POINT ( 'NONE',  ( -27.32632706500987751, -39.48308634739166934, 32.30687911778738908 ) ) ;
#78759 = B_SPLINE_CURVE_WITH_KNOTS ( 'NONE', 3,
 ( #72380, #15738, #48621, #39506, #57242, #31433 ),
 .UNSPECIFIED., .F., .F.,
 ( 4, 2, 4 ),
 ( 0.004615310220740755608, 0.006918661718823359771, 0.009222013216905963068 ),
 .UNSPECIFIED. ) ;
#78760 = ORIENTED_EDGE ( 'NONE', *, *, #12769, .T. ) ;
#78761 = ORIENTED_EDGE ( 'NONE', *, *, #19418, .F. ) ;
#78762 = CARTESIAN_POINT ( 'NONE',  ( 48.69037531413704301, -39.51851888690750769, 48.66629101439573191 ) ) ;
#78763 = CARTESIAN_POINT ( 'NONE',  ( -1.231536178911134094, 11.27772218784141423, 50.25311877652383430 ) ) ;
#78764 = CYLINDRICAL_SURFACE ( 'NONE', #61726, 7.500000000001509015 ) ;
#78765 = CARTESIAN_POINT ( 'NONE',  ( -105.2287569084031418, -38.38999224387904974, 197.2639937961484407 ) ) ;
#78766 = CIRCLE ( 'NONE', #59861, 4.000000000000000888 ) ;
#78767 = VERTEX_POINT ( 'NONE', #81856 ) ;
#78768 = CARTESIAN_POINT ( 'NONE',  ( 90.61125330831669089, -38.34432070828795958, 12.49403374418715273 ) ) ;
#78769 = CARTESIAN_POINT ( 'NONE',  ( 13.38407207131497501, 3.659884948878311839, -6.694498904168558973 ) ) ;
#78770 = CARTESIAN_POINT ( 'NONE',  ( -19.00015996940621932, 49.50625549542287018, 61.91457260680915198 ) ) ;
#78771 = CARTESIAN_POINT ( 'NONE',  ( 10.68704811846494351, 43.88291023799746426, 12.97108649491024579 ) ) ;
#78772 = CARTESIAN_POINT ( 'NONE',  ( 6.097211899678556257, 40.29241764280718030, -71.16079434776209212 ) ) ;
#78773 = CARTESIAN_POINT ( 'NONE',  ( -31.63765798398162588, 436.4483132331570800, 18.85061845559700444 ) ) ;
#78774 = CARTESIAN_POINT ( 'NONE',  ( -33.21459943997732722, 487.8270262908587256, 10.08789160144731056 ) ) ;
#78775 = CARTESIAN_POINT ( 'NONE',  ( 12.50000000000000711, -4.999999999999999112, -55.73109925765189843 ) ) ;
#78776 = CIRCLE ( 'NONE', #40902, 4.172000000000001485 ) ;
#78777 = CARTESIAN_POINT ( 'NONE',  ( 108.8393071453071315, -59.99999999999999289, 194.0395522074744576 ) ) ;
#78778 = AXIS2_PLACEMENT_3D ( 'NONE', #81553, #57289, #40593 ) ;
#78779 = CARTESIAN_POINT ( 'NONE',  ( -15.55430219785582935, 34.98758788652926910, 22.68934981201532963 ) ) ;
#78780 = EDGE_LOOP ( 'NONE', ( #49714, #59324, #92118, #22068, #83834 ) ) ;
#78781 = EDGE_CURVE ( 'NONE', #90588, #4091, #10399, .T. ) ;
#78782 = CARTESIAN_POINT ( 'NONE',  ( -28.94221336919291332, 306.6375891257424087, -9.149909065943708342 ) ) ;
#78783 = CARTESIAN_POINT ( 'NONE',  ( 94.26467260280679739, 1.016364837396684119E-14, 0.000000000000000000 ) ) ;
#78784 = CARTESIAN_POINT ( 'NONE',  ( 0.000000000000000000, 0.5000000000000000000, -4.000000000000000000 ) ) ;
#78785 = VERTEX_POINT ( 'NONE', #65704 ) ;
#78787 = DIRECTION ( 'NONE',  ( 0.000000000000000000, 0.000000000000000000, 1.000000000000000000 ) ) ;
#78786 = CARTESIAN_POINT ( 'NONE',  ( -90.68541565423112161, -38.35038405383468074, 17.37308604620570662 ) ) ;
#78788 = CARTESIAN_POINT ( 'NONE',  ( 5.656854249492378806, -21.68749999999999645, 5.656854249492381470 ) ) ;
#78789 = CARTESIAN_POINT ( 'NONE',  ( 43.48483803624226596, 478.3762783859503429, 6.210097532619577088 ) ) ;
#78790 = SURFACE_STYLE_FILL_AREA ( #22724 ) ;
#78791 = CARTESIAN_POINT ( 'NONE',  ( 7.188101187499999156, -15.12500000204838457, 2.977408999572654924 ) ) ;
#78792 = CARTESIAN_POINT ( 'NONE',  ( -6.043427762771337086, -5.000000000000002665, -74.51456333905269958 ) ) ;
#78793 = ADVANCED_FACE ( 'NONE', ( #98587 ), #22542, .T. ) ;
#78794 = EDGE_CURVE ( 'NONE', #36676, #4725, #67789, .T. ) ;
#78795 = CARTESIAN_POINT ( 'NONE',  ( -42.80674739067558221, 434.8200538645568827, 17.89665983759107704 ) ) ;
#78796 = CIRCLE ( 'NONE', #106356, 0.9999999999999987788 ) ;
#78798 = ORIENTED_EDGE ( 'NONE', *, *, #42849, .F. ) ;
#78797 = CARTESIAN_POINT ( 'NONE',  ( 67.96666666666666856, 3.309500000000014541, 4.052968581778174646E-16 ) ) ;
#78799 = CARTESIAN_POINT ( 'NONE',  ( 83.04247666559754748, -39.48343404634957210, 170.2731162165301555 ) ) ;
#78800 = CARTESIAN_POINT ( 'NONE',  ( 8.731350795034574119, 131.9383239543996922, 0.000000000000000000 ) ) ;
#78801 = AXIS2_PLACEMENT_3D ( 'NONE', #61869, #78549, #29517 ) ;
#78802 = CARTESIAN_POINT ( 'NONE',  ( -36.41468026840615124, 439.0114751707915843, 23.96625823804127720 ) ) ;
#78803 = EDGE_LOOP ( 'NONE', ( #38721, #88732, #53787, #105569, #9546, #17968 ) ) ;
#78804 = CARTESIAN_POINT ( 'NONE',  ( -37.01956797474046823, 345.4690947806042232, 0.09929204855550027853 ) ) ;
#78805 = EDGE_CURVE ( 'NONE', #12797, #41885, #9041, .T. ) ;
#78806 = CARTESIAN_POINT ( 'NONE',  ( -46.92395915124596684, 18.83177588379273004, 15.01493731818062294 ) ) ;
#78807 = CARTESIAN_POINT ( 'NONE',  ( 7.999999999999998224, -29.09374999999999289, 3.313708498984766049 ) ) ;
#78808 = CARTESIAN_POINT ( 'NONE',  ( -12.50000000000000355, 41.59226156894883530, -76.70843802411151557 ) ) ;
#78809 = CARTESIAN_POINT ( 'NONE',  ( 20.00000000000000000, 12.99999999999999289, 0.000000000000000000 ) ) ;
#78810 = CARTESIAN_POINT ( 'NONE',  ( 0.2959367164359796853, 12.99314498399917639, 51.71656300685955898 ) ) ;
#78811 = EDGE_LOOP ( 'NONE', ( #31319, #54357, #25069, #13253 ) ) ;
#78812 = SURFACE_STYLE_FILL_AREA ( #70202 ) ;
#78813 = AXIS2_PLACEMENT_3D ( 'NONE', #69601, #69074, #93343 ) ;
#78814 = CARTESIAN_POINT ( 'NONE',  ( -4.460876563139970941, -48.83448355510768835, 104.3906876480053256 ) ) ;
#78815 = CARTESIAN_POINT ( 'NONE',  ( -1.000000000000000000, -10.14983348571115229, -12.32139453386699657 ) ) ;
#78816 = CARTESIAN_POINT ( 'NONE',  ( 14.29190075645646907, 21.26710225494832329, -5.626279437268317807 ) ) ;
#78818 = CARTESIAN_POINT ( 'NONE',  ( -15.55348733900250124, 4.754504522411744816, -5.683216791855722150 ) ) ;
#78817 = CARTESIAN_POINT ( 'NONE',  ( 7.412969500702210723, 41.14559805159964156, -68.91429205978418793 ) ) ;
#78819 = CARTESIAN_POINT ( 'NONE',  ( 2.977408999572651815, -20.93750000204838457, 7.188101187500000933 ) ) ;
#78820 = CIRCLE ( 'NONE', #32350, 5.000000000000011546 ) ;
#78821 = CARTESIAN_POINT ( 'NONE',  ( -30.00000000000000000, 488.6481008951269587, 3.890293910847615333 ) ) ;
#78822 = AXIS2_PLACEMENT_3D ( 'NONE', #78197, #59917, #43703 ) ;
#78823 = CARTESIAN_POINT ( 'NONE',  ( 1.308371270545586329, -5.000000000000000888, -9.999872502480485537 ) ) ;
#78824 = CONTEXT_DEPENDENT_SHAPE_REPRESENTATION ( #79720, #31399 ) ;
#78825 = VERTEX_POINT ( 'NONE', #15009 ) ;
#78826 = CARTESIAN_POINT ( 'NONE',  ( 0.000000000000000000, -2.000000000000000000, 0.000000000000000000 ) ) ;
#78827 = DIRECTION ( 'NONE',  ( -1.000000000000000000, -1.224606353822377258E-16, -0.000000000000000000 ) ) ;
#78828 = CARTESIAN_POINT ( 'NONE',  ( -8.570032633477826067, 24.09669418278768660, -5.000000000001270095 ) ) ;
#78829 = STYLED_ITEM ( 'NONE', ( #320 ), #9022 ) ;
#78830 =( NAMED_UNIT ( * ) SI_UNIT ( $, .STERADIAN. ) SOLID_ANGLE_UNIT ( ) );
#78831 = ADVANCED_FACE ( 'NONE', ( #80808, #9568 ), #69437, .T. ) ;
#78832 = CARTESIAN_POINT ( 'NONE',  ( 22.33349330513380693, -4.000000000000000888, 4.898587196589416773E-16 ) ) ;
#78833 = ORIENTED_EDGE ( 'NONE', *, *, #48161, .F. ) ;
#78834 = AXIS2_PLACEMENT_3D ( 'NONE', #32962, #25411, #65832 ) ;
#78835 = LINE ( 'NONE', #38409, #51566 ) ;
#78836 = CARTESIAN_POINT ( 'NONE',  ( 12.13034742782428133, 49.99999999999999289, -93.82352941176471006 ) ) ;
#78837 = EDGE_LOOP ( 'NONE', ( #98116, #80794, #53972, #26139, #70690 ) ) ;
#78838 = EDGE_CURVE ( 'NONE', #17636, #26380, #93384, .T. ) ;
#78839 = DIRECTION ( 'NONE',  ( 0.000000000000000000, -1.000000000000000000, 0.000000000000000000 ) ) ;
#78840 = AXIS2_PLACEMENT_3D ( 'NONE', #4352, #84742, #10306 ) ;
#78841 = CARTESIAN_POINT ( 'NONE',  ( -42.32873853761031313, 39.51951600909762163, -49.85685020764661601 ) ) ;
#78842 = CARTESIAN_POINT ( 'NONE',  ( -17.37779721166338476, 36.93489020264717482, 21.96297318349773775 ) ) ;
#78843 = CARTESIAN_POINT ( 'NONE',  ( -105.7694337438876317, -59.99999999999999289, 198.5129163904271934 ) ) ;
#78844 = CARTESIAN_POINT ( 'NONE',  ( 6.744163421200966901, 304.7396475197473364, -9.023845328246613562 ) ) ;
#78845 = FACE_OUTER_BOUND ( 'NONE', #14543, .T. ) ;
#78846 = FACE_OUTER_BOUND ( 'NONE', #44358, .T. ) ;
#78847 = AXIS2_PLACEMENT_3D ( 'NONE', #3431, #43878, #60627 ) ;
#78848 = CARTESIAN_POINT ( 'NONE',  ( -84.73791746677021308, -32.38247958360803835, 175.3255226634325084 ) ) ;
#78849 = DIRECTION ( 'NONE',  ( 0.000000000000000000, 0.000000000000000000, 1.000000000000000000 ) ) ;
#78850 = EDGE_LOOP ( 'NONE', ( #26816, #46051, #26829, #57535 ) ) ;
#78851 = CARTESIAN_POINT ( 'NONE',  ( -0.01431428620034891179, -57.67120202577072519, -44.61186648040676772 ) ) ;
#78852 =( BOUNDED_SURFACE ( )  B_SPLINE_SURFACE ( 3, 2, ( 
 ( #58508, #35863, #11523 ),
 ( #42846, #101083, #76798 ),
 ( #91929, #75741, #67129 ),
 ( #67663, #27779, #43387 ),
 ( #76270, #68739, #66590 ),
 ( #9939, #50389, #2376 ),
 ( #26707, #101623, #83301 ),
 ( #34258, #1837, #748 ) ),
 .UNSPECIFIED., .F., .F., .F. ) 
 B_SPLINE_SURFACE_WITH_KNOTS ( ( 4, 2, 2, 4 ),
 ( 3, 3 ),
 ( 0.009810586775086673275, 0.01999416116298580876, 0.02508594835693537736, 0.03017773555088494597 ),
 ( 0.000000000000000000, 1.000000000000000000 ),
 .UNSPECIFIED. ) 
 GEOMETRIC_REPRESENTATION_ITEM ( )  RATIONAL_B_SPLINE_SURFACE ( (
 ( 1.000000000000000000, 0.7071067811865475727, 1.000000000000000000),
 ( 1.000000000000000000, 0.7071067811865475727, 1.000000000000000000),
 ( 1.000000000000000000, 0.7071080532031980281, 1.000000000000000000),
 ( 1.000000000000000000, 0.7071061932061152300, 1.000000000000000000),
 ( 1.000000000000000000, 0.7071074416953658792, 1.000000000000000000),
 ( 1.000000000000000000, 0.7071061820943852494, 1.000000000000000000),
 ( 1.000000000000000000, 0.7071482300333765680, 1.000000000000000000),
 ( 1.000000000000000000, 0.7071067811865450192, 1.000000000000000000) ) ) 
 REPRESENTATION_ITEM ( '' )  SURFACE ( )  );
#78853 = ADVANCED_FACE ( 'NONE', ( #43024 ), #87965, .F. ) ;
#78854 = CARTESIAN_POINT ( 'NONE',  ( 5.646888413699862497, -68.44974155970390939, 2.040714635159915247 ) ) ;
#78855 = CARTESIAN_POINT ( 'NONE',  ( -84.90780823601593852, -52.70144861668445913, 11.02726620768325638 ) ) ;
#78856 = FACE_BOUND ( 'NONE', #44456, .T. ) ;
#78857 = AXIS2_PLACEMENT_3D ( 'NONE', #96762, #88662, #31517 ) ;
#78858 = FACE_OUTER_BOUND ( 'NONE', #54031, .T. ) ;
#78859 = CARTESIAN_POINT ( 'NONE',  ( 3.443342638033509484, 124.1418742747060548, -5.000000000000000000 ) ) ;
#78860 = DIRECTION ( 'NONE',  ( -1.000000000000000000, -0.000000000000000000, -0.000000000000000000 ) ) ;
#78861 = CARTESIAN_POINT ( 'NONE',  ( 33.52312678242137167, 18.64316884714798306, 19.32152200346563120 ) ) ;
#78862 = PRESENTATION_LAYER_ASSIGNMENT (  '', '', ( #4815 ) ) ;
#78863 = CARTESIAN_POINT ( 'NONE',  ( 88.91505260351625850, -29.99999999999995381, 199.0551756924508879 ) ) ;
#78864 = CARTESIAN_POINT ( 'NONE',  ( 0.000000000000000000, 51.11204936430951307, -27.84083606136722366 ) ) ;
#78865 = CARTESIAN_POINT ( 'NONE',  ( -95.99503958615204624, -14.21045842199434794, 88.91558689677049188 ) ) ;
#78866 = EDGE_CURVE ( 'NONE', #32369, #83574, #103682, .T. ) ;
#78867 = CARTESIAN_POINT ( 'NONE',  ( -66.48194133918796922, -32.53344480627807656, 86.88017675495862591 ) ) ;
#78868 = ORIENTED_EDGE ( 'NONE', *, *, #97090, .F. ) ;
#78869 = CARTESIAN_POINT ( 'NONE',  ( 11.87333998996387230, 39.42593707198930986, 63.97654705930002450 ) ) ;
#78870 = CARTESIAN_POINT ( 'NONE',  ( 71.31866560408677458, -59.99999999996072830, 168.9897809639343791 ) ) ;
#78871 = EDGE_LOOP ( 'NONE', ( #29643, #61922, #92786, #30684 ) ) ;
#78872 = CARTESIAN_POINT ( 'NONE',  ( -7.188101187500000044, -17.28125000204838813, -8.802885111219163269E-16 ) ) ;
#78873 = CIRCLE ( 'NONE', #32405, 0.5000000000000004441 ) ;
#78874 = CARTESIAN_POINT ( 'NONE',  ( 18.00000000000000355, 12.99999999999999289, 0.000000000000000000 ) ) ;
#78875 = ORIENTED_EDGE ( 'NONE', *, *, #14425, .F. ) ;
#78877 = FACE_OUTER_BOUND ( 'NONE', #37954, .T. ) ;
#78876 = CONICAL_SURFACE ( 'NONE', #6570, 4.172000000000009479, 0.9599310885968813656 ) ;
#78878 = ORIENTED_EDGE ( 'NONE', *, *, #40929, .F. ) ;
#78879 = DIRECTION ( 'NONE',  ( -0.000000000000000000, 1.000000000000000000, -0.000000000000000000 ) ) ;
#78880 = CARTESIAN_POINT ( 'NONE',  ( 46.86052085224882546, 18.87480283624687161, -15.15319613412887279 ) ) ;
#78881 = CARTESIAN_POINT ( 'NONE',  ( -92.75956059744693505, -59.99999999999998579, -7.438970123485077579 ) ) ;
#78882 = FACE_OUTER_BOUND ( 'NONE', #99316, .T. ) ;
#78883 = CARTESIAN_POINT ( 'NONE',  ( -2.977408999572650039, -31.06250000204838813, -7.188101187500001821 ) ) ;
#78884 = DIRECTION ( 'NONE',  ( 1.000000000000000000, 0.000000000000000000, -0.000000000000000000 ) ) ;
#78885 = CARTESIAN_POINT ( 'NONE',  ( 22.67073868809949033, -4.285714285714296246, 11.17734400176826348 ) ) ;
#78886 = FACE_OUTER_BOUND ( 'NONE', #94273, .T. ) ;
#78887 = CARTESIAN_POINT ( 'NONE',  ( 31.84999999999999787, 1.533819458162526451E-15, 0.000000000000000000 ) ) ;
#78888 = CARTESIAN_POINT ( 'NONE',  ( -7.412906595240168706, 107.6418827285225603, 3.014362223629234006 ) ) ;
#78889 = EDGE_CURVE ( 'NONE', #32770, #70163, #75914, .T. ) ;
#78890 = FACE_OUTER_BOUND ( 'NONE', #103531, .T. ) ;
#78891 = CARTESIAN_POINT ( 'NONE',  ( 23.08332880300597978, 303.3267438324617160, -9.898176362637144621 ) ) ;
#78892 = VERTEX_POINT ( 'NONE', #2013 ) ;
#78893 = CARTESIAN_POINT ( 'NONE',  ( 21.36650669486618881, -3.999999999999998224, 0.000000000000000000 ) ) ;
#78894 = DIRECTION ( 'NONE',  ( 0.000000000000000000, -1.000000000000000000, 0.000000000000000000 ) ) ;
#78895 = AXIS2_PLACEMENT_3D ( 'NONE', #67348, #52740, #101307 ) ;
#78896 = VECTOR ( 'NONE', #68415, 1000.000000000000000 ) ;
#78897 = CARTESIAN_POINT ( 'NONE',  ( 36.97211274858098307, -39.50748652884733758, 36.52538937020025855 ) ) ;
#78899 = CIRCLE ( 'NONE', #103004, 3.000000000000006661 ) ;
#78898 = CARTESIAN_POINT ( 'NONE',  ( -17.78317311658302202, -3.469446951953614189E-15, -13.66642973270732142 ) ) ;
#78900 = ORIENTED_EDGE ( 'NONE', *, *, #26967, .F. ) ;
#78901 = DIRECTION ( 'NONE',  ( 0.000000000000000000, 0.000000000000000000, 1.000000000000000000 ) ) ;
#78903 = CARTESIAN_POINT ( 'NONE',  ( -34.94338628507543376, 342.5355909536760350, -0.9693026116843473927 ) ) ;
#78902 = FACE_OUTER_BOUND ( 'NONE', #64699, .T. ) ;
#78904 = CARTESIAN_POINT ( 'NONE',  ( 42.98746414932995208, 1.482358050883964840E-15, 0.000000000000000000 ) ) ;
#78905 = CARTESIAN_POINT ( 'NONE',  ( 5.000000000000000000, 6.123233995736766282E-16, -9.974599999999998801 ) ) ;
#78906 = CIRCLE ( 'NONE', #23816, 3.309500000000001663 ) ;
#78907 = SURFACE_STYLE_USAGE ( .BOTH. , #61700 ) ;
#78908 =( NAMED_UNIT ( * ) PLANE_ANGLE_UNIT ( ) SI_UNIT ( $, .RADIAN. ) );
#78909 = CARTESIAN_POINT ( 'NONE',  ( -3.400000000000000355, 4.163799117101001052E-16, -8.000000000000000000 ) ) ;
#78910 = CARTESIAN_POINT ( 'NONE',  ( -3.041362414359006117, -49.44898643135800143, 44.27295612633997024 ) ) ;
#78911 = ORIENTED_EDGE ( 'NONE', *, *, #46736, .F. ) ;
#78912 = CARTESIAN_POINT ( 'NONE',  ( 92.13009336766872082, -59.99999999999999289, 3.893291599061448061 ) ) ;
#78913 = CARTESIAN_POINT ( 'NONE',  ( 29.68315524076926337, -1.200000000000000030E-05, -40.85535821593530414 ) ) ;
#78914 = DIRECTION ( 'NONE',  ( 0.000000000000000000, 0.000000000000000000, 1.000000000000000000 ) ) ;
#78915 = CARTESIAN_POINT ( 'NONE',  ( -7.004291982367331748, 40.56179000230169862, -71.01843131766943884 ) ) ;
#78916 = FACE_BOUND ( 'NONE', #33799, .T. ) ;
#78917 = ORIENTED_EDGE ( 'NONE', *, *, #35018, .T. ) ;
#78918 = EDGE_CURVE ( 'NONE', #33663, #27751, #43226, .T. ) ;
#78919 = VECTOR ( 'NONE', #2026, 1000.000000000000000 ) ;
#78920 = CARTESIAN_POINT ( 'NONE',  ( -92.52610172686061674, -29.99999999989381649, 50.79198441316200530 ) ) ;
#78921 = ORIENTED_EDGE ( 'NONE', *, *, #48109, .T. ) ;
#78922 = CYLINDRICAL_SURFACE ( 'NONE', #2191, 1.250000000000001110 ) ;
#78923 = DIRECTION ( 'NONE',  ( -0.000000000000000000, 1.000000000000000000, -0.000000000000000000 ) ) ;
#78924 = CYLINDRICAL_SURFACE ( 'NONE', #41920, 8.000000000000000000 ) ;
#78925 =( NAMED_UNIT ( * ) PLANE_ANGLE_UNIT ( ) SI_UNIT ( $, .RADIAN. ) );
#78926 = CARTESIAN_POINT ( 'NONE',  ( 83.04580959076339752, -45.27726561227110125, -14.40480725557183206 ) ) ;
#78927 = CARTESIAN_POINT ( 'NONE',  ( -7.188101187500002709, -32.18750000204838813, 2.977408999572648707 ) ) ;
#78928 = CARTESIAN_POINT ( 'NONE',  ( -44.12472801210821416, 485.7238370326489871, 3.975897585127424527 ) ) ;
#78929 = CARTESIAN_POINT ( 'NONE',  ( 52.81650669486619165, 4.000000000000015099, 4.898587196589422689E-16 ) ) ;
#78931 = EDGE_CURVE ( 'NONE', #25325, #73667, #14844, .T. ) ;
#78930 = CARTESIAN_POINT ( 'NONE',  ( 34.87911814363040719, 490.1439009131577791, 11.96539503908413415 ) ) ;
#78932 = ORIENTED_EDGE ( 'NONE', *, *, #90578, .F. ) ;
#78933 = MECHANICAL_DESIGN_GEOMETRIC_PRESENTATION_REPRESENTATION (  '', ( #72070 ), #92706 ) ;
#78934 = AXIS2_PLACEMENT_3D ( 'NONE', #96033, #29734, #46417 ) ;
#78936 = VERTEX_POINT ( 'NONE', #47252 ) ;
#78935 = CARTESIAN_POINT ( 'NONE',  ( 32.84444940698777771, 439.0476299206099497, 24.86213004146451766 ) ) ;
#78937 = CARTESIAN_POINT ( 'NONE',  ( 79.72836144202692310, -18.67635071187021012, 125.0949995831272474 ) ) ;
#78938 =( NAMED_UNIT ( * ) PLANE_ANGLE_UNIT ( ) SI_UNIT ( $, .RADIAN. ) );
#78939 = ORIENTED_EDGE ( 'NONE', *, *, #68613, .F. ) ;
#78940 = EDGE_CURVE ( 'NONE', #105570, #104380, #56979, .T. ) ;
#78941 = CARTESIAN_POINT ( 'NONE',  ( -12.50000000000000888, 38.67421576088683821, -61.60810543285763430 ) ) ;
#78942 = CARTESIAN_POINT ( 'NONE',  ( -7.188101187500000933, -18.50000000204838457, -2.977408999572651371 ) ) ;
#78943 = CARTESIAN_POINT ( 'NONE',  ( -108.1850948662969216, -57.66112862901258751, 198.7856339303252753 ) ) ;
#78944 = ORIENTED_EDGE ( 'NONE', *, *, #25505, .F. ) ;
#78945 = SURFACE_SIDE_STYLE ('',( #46063 ) ) ;
#78946 = COLOUR_RGB ( '', 0.66274510, 0.83137255, 0.94901961) ;
#78947 = FACE_OUTER_BOUND ( 'NONE', #39275, .T. ) ;
#78948 = CARTESIAN_POINT ( 'NONE',  ( -5.911778709945830101, -13.86661839416573194, 1.058844270818175115 ) ) ;
#78949 = VECTOR ( 'NONE', #103332, 1000.000000000000000 ) ;
#78950 = CARTESIAN_POINT ( 'NONE',  ( 7.384655732054108412, 41.09429998108713988, -59.07190378971382927 ) ) ;
#78951 = DIRECTION ( 'NONE',  ( 0.000000000000000000, -1.000000000000000000, 0.000000000000000000 ) ) ;
#78952 = CARTESIAN_POINT ( 'NONE',  ( 8.000000000000000000, -9.593750004096769146, -3.313708498984761608 ) ) ;
#78953 = CARTESIAN_POINT ( 'NONE',  ( -40.22137457019058360, -26.42085694424761044, 36.10270639820529226 ) ) ;
#78954 = CARTESIAN_POINT ( 'NONE',  ( -37.24675868481172358, 25.86585418676965276, 10.98683038162339010 ) ) ;
#78955 = CIRCLE ( 'NONE', #92735, 4.172000000000001485 ) ;
#78956 = DIRECTION ( 'NONE',  ( 0.000000000000000000, 1.000000000000000000, 0.000000000000000000 ) ) ;
#78957 = CARTESIAN_POINT ( 'NONE',  ( 7.500000000000007105, 42.86855997971688481, -62.45407030448338048 ) ) ;
#78958 = CARTESIAN_POINT ( 'NONE',  ( 51.88291765283141643, 138.1183258647170362, 182.1969486012845607 ) ) ;
#78959 = CARTESIAN_POINT ( 'NONE',  ( 37.88459826976592382, 27.77132929239739312, 10.98695786631084914 ) ) ;
#78960 = ORIENTED_EDGE ( 'NONE', *, *, #90201, .T. ) ;
#78961 = CARTESIAN_POINT ( 'NONE',  ( -4.888678503699334321, -52.01088711094052286, 40.11975448313368275 ) ) ;
#78962 = LINE ( 'NONE', #70878, #30260 ) ;
#78963 = DIRECTION ( 'NONE',  ( -1.000000000000000000, -1.224606353822377258E-16, -0.000000000000000000 ) ) ;
#78964 = CARTESIAN_POINT ( 'NONE',  ( -63.12118703508443929, -30.05855728996417398, -32.04057825768840928 ) ) ;
#78965 = CARTESIAN_POINT ( 'NONE',  ( -66.41877331073435187, -30.00000000000001066, 84.34413472128925093 ) ) ;
#78966 = CARTESIAN_POINT ( 'NONE',  ( 7.500000000000007105, 42.00000000000000711, -70.16688272716297092 ) ) ;
#78967 = EDGE_CURVE ( 'NONE', #88573, #102768, #8719, .T. ) ;
#78968 = ORIENTED_EDGE ( 'NONE', *, *, #68341, .F. ) ;
#78969 = CONICAL_SURFACE ( 'NONE', #53112, 4.000000000000007105, 0.9599310885968835860 ) ;
#78970 = CARTESIAN_POINT ( 'NONE',  ( -16.50306599549761444, -4.333298119783954405, -6.982805419935155022 ) ) ;
#78971 = CARTESIAN_POINT ( 'NONE',  ( 96.56796194465512428, -57.62221250710192777, 204.4799581288910986 ) ) ;
#78972 = AXIS2_PLACEMENT_3D ( 'NONE', #90279, #99955, #81627 ) ;
#78973 = CARTESIAN_POINT ( 'NONE',  ( 69.51775844058592213, -21.77030775744987068, -19.67941227880303856 ) ) ;
#78974 = VECTOR ( 'NONE', #77495, 1000.000000000000000 ) ;
#78975 = EDGE_CURVE ( 'NONE', #11885, #3128, #1856, .T. ) ;
#78976 = CARTESIAN_POINT ( 'NONE',  ( 33.49615637169857507, 465.2403011571852289, 8.307633084691127934 ) ) ;
#78977 = CARTESIAN_POINT ( 'NONE',  ( -14.86018380392287241, 23.02630934695395126, 1.319261379087336206 ) ) ;
#78978 = DIRECTION ( 'NONE',  ( -0.000000000000000000, -0.000000000000000000, -1.000000000000000000 ) ) ;
#78979 = CARTESIAN_POINT ( 'NONE',  ( -51.75140944414650335, -60.00000000000002132, 76.27795920913510486 ) ) ;
#78980 = AXIS2_PLACEMENT_3D ( 'NONE', #37336, #45926, #37868 ) ;
#78981 = CARTESIAN_POINT ( 'NONE',  ( 0.000000000000000000, 0.000000000000000000, -6.418875477074183600 ) ) ;
#78982 = CARTESIAN_POINT ( 'NONE',  ( -63.03617022295203753, 48.00000000000000000, -16.93907820454660396 ) ) ;
#78983 = CARTESIAN_POINT ( 'NONE',  ( -84.31464934120297983, -57.44558481396982330, 191.1750344329549307 ) ) ;
#78984 = ORIENTED_EDGE ( 'NONE', *, *, #592, .F. ) ;
#78985 = CARTESIAN_POINT ( 'NONE',  ( 32.01721732537988885, 318.3378566774296701, -5.732130415166460047 ) ) ;
#78986 = DIRECTION ( 'NONE',  ( 0.000000000000000000, 1.000000000000000000, 0.000000000000000000 ) ) ;
#78987 = CARTESIAN_POINT ( 'NONE',  ( -6.847405770342755993, 41.77151253865379488, -59.31773377044793705 ) ) ;
#78988 = DIRECTION ( 'NONE',  ( 0.000000000000000000, 0.000000000000000000, -1.000000000000000000 ) ) ;
#78989 = CARTESIAN_POINT ( 'NONE',  ( 12.49723740359450730, -3.303264067465667697, -76.71011700628446306 ) ) ;
#78990 = EDGE_CURVE ( 'NONE', #17653, #12439, #83055, .T. ) ;
#78991 = CARTESIAN_POINT ( 'NONE',  ( -20.56310269357972587, 303.8628971230333491, -9.997642691052938346 ) ) ;
#78992 = CARTESIAN_POINT ( 'NONE',  ( -83.65529993258698482, -45.25817475319772143, -13.07161437908048462 ) ) ;
#78993 = AXIS2_PLACEMENT_3D ( 'NONE', #48056, #64277, #81474 ) ;
#78994 = LINE ( 'NONE', #77408, #63206 ) ;
#78995 = DIRECTION ( 'NONE',  ( 0.000000000000000000, -1.000000000000000000, 0.000000000000000000 ) ) ;
#78996 = STYLED_ITEM ( 'NONE', ( #73902 ), #5817 ) ;
#78997 = ORIENTED_EDGE ( 'NONE', *, *, #16736, .F. ) ;
#78998 = CARTESIAN_POINT ( 'NONE',  ( 31.36650669486618881, 4.898587196589413815E-16, -4.000000000000000888 ) ) ;
#78999 = CARTESIAN_POINT ( 'NONE',  ( 13.01536098179566281, 4.316280655867278604, 7.368423276989370940 ) ) ;
#79000 = EDGE_CURVE ( 'NONE', #40074, #95890, #44927, .T. ) ;
#79001 = CARTESIAN_POINT ( 'NONE',  ( 6.601913983210295100, -4.285714285714226079, 24.56594385547514747 ) ) ;
#79002 =( GEOMETRIC_REPRESENTATION_CONTEXT ( 3 ) GLOBAL_UNCERTAINTY_ASSIGNED_CONTEXT ( ( #42954 ) ) GLOBAL_UNIT_ASSIGNED_CONTEXT ( ( #82482, #18303, #9635 ) ) REPRESENTATION_CONTEXT ( 'NONE', 'WORKASPACE' ) );
#79003 = CARTESIAN_POINT ( 'NONE',  ( -33.47662383462841262, 484.3276029200706603, 3.198141044746298789 ) ) ;
#79004 = VECTOR ( 'NONE', #94096, 1000.000000000000000 ) ;
#79005 = CARTESIAN_POINT ( 'NONE',  ( 82.73925898424661796, -14.21045842199433373, -19.52984640694043250 ) ) ;
#79006 = CARTESIAN_POINT ( 'NONE',  ( -78.56154225647874512, -49.90730404993688296, 147.8671053437099374 ) ) ;
#79007 = ORIENTED_EDGE ( 'NONE', *, *, #27984, .T. ) ;
#79008 = DIRECTION ( 'NONE',  ( 0.000000000000000000, -1.000000000000000000, 0.000000000000000000 ) ) ;
#79009 = CARTESIAN_POINT ( 'NONE',  ( 0.000000000000000000, 0.000000000000000000, -4.147675477074182382 ) ) ;
#79010 = CARTESIAN_POINT ( 'NONE',  ( 83.32454909816027566, -57.53833991724482644, 201.3685442388917863 ) ) ;
#79011 =( NAMED_UNIT ( * ) SI_UNIT ( $, .STERADIAN. ) SOLID_ANGLE_UNIT ( ) );
#79012 = UNCERTAINTY_MEASURE_WITH_UNIT (LENGTH_MEASURE( 1.000000000000000082E-05 ), #24814, 'distance_accuracy_value', 'NONE');
#79014 = PRESENTATION_LAYER_ASSIGNMENT (  '', '', ( #101422 ) ) ;
#79013 = CARTESIAN_POINT ( 'NONE',  ( 30.98142344576083573, 309.3658521538144441, -8.497048073299385607 ) ) ;
#79015 = DIRECTION ( 'NONE',  ( 1.000000000000000000, 0.000000000000000000, 0.000000000000000000 ) ) ;
#79016 = EDGE_LOOP ( 'NONE', ( #38429, #99897, #23475, #82980 ) ) ;
#79017 = FILL_AREA_STYLE_COLOUR ( '', #9564 ) ;
#79018 = CARTESIAN_POINT ( 'NONE',  ( 31.32516044773268149, 438.3824493690776762, 22.69256374299771295 ) ) ;
#79019 = DIRECTION ( 'NONE',  ( -3.673940397442057649E-17, 0.000000000000000000, -1.000000000000000000 ) ) ;
#79020 = CARTESIAN_POINT ( 'NONE',  ( -2.977408999572654480, -22.62500000204838813, 7.188101187499999156 ) ) ;
#79021 = ORIENTED_EDGE ( 'NONE', *, *, #72024, .F. ) ;
#79022 = DIRECTION ( 'NONE',  ( 0.000000000000000000, 0.000000000000000000, 1.000000000000000000 ) ) ;
#79023 = CARTESIAN_POINT ( 'NONE',  ( -44.47534256803313468, -38.31161230092084224, 57.00189278798902137 ) ) ;
#79024 = CARTESIAN_POINT ( 'NONE',  ( -44.28929576524119227, 435.2229490444834141, 14.00215079178472166 ) ) ;
#79025 = CARTESIAN_POINT ( 'NONE',  ( -17.64329382111517575, 45.32481993297742662, -6.176472982800969902 ) ) ;
#79026 = CARTESIAN_POINT ( 'NONE',  ( 5.299999999999999822, 3.752776749732553263, -6.499999999999999112 ) ) ;
#79028 = CARTESIAN_POINT ( 'NONE',  ( -35.53321744913902336, 463.4104023594616706, 19.92304894059135023 ) ) ;
#79027 = CIRCLE ( 'NONE', #15346, 7.500000000000000888 ) ;
#79029 = EDGE_LOOP ( 'NONE', ( #26388, #95386, #38755, #29594, #60624 ) ) ;
#79030 = DIRECTION ( 'NONE',  ( 0.000000000000000000, -1.000000000000000000, 0.000000000000000000 ) ) ;
#79032 = CARTESIAN_POINT ( 'NONE',  ( 28.53304972825587527, -53.38433873617589143, 35.07953571996775111 ) ) ;
#79031 = CARTESIAN_POINT ( 'NONE',  ( -66.35297339498846725, -60.00000000000000000, 134.7723483620486888 ) ) ;
#79033 = CARTESIAN_POINT ( 'NONE',  ( -10.00000000000000355, 105.0000000000000000, 0.000000000000000000 ) ) ;
#79035 = ORIENTED_EDGE ( 'NONE', *, *, #39083, .F. ) ;
#79034 =( BOUNDED_SURFACE ( )  B_SPLINE_SURFACE ( 2, 3, ( 
 ( #18957, #66392, #51800, #58855, #8156, #99271, #41060, #25450, #27, #32997, #50209, #91746, #4325, #11328, #101950, #19495, #28639, #103550, #2720, #53415, #70655, #3267, #28108, #21086, #93344, #36739, #68545, #77691, #27584, #12399, #60465, #3800, #62572, #21603, #95457, #44260, #103030, #69075, #61522, #53923, #69602, #102495, #77152, #94951, #36208, #94415, #60984, #52332, #20576, #85245, #52871, #93871, #85801, #11874, #12930, #20030, #44802, #86334, #78211, #45330, #84711, #37260, #70122, #29184, #62062, #86854, #45850, #78724, #4862, #37794, #29700, #10798, #76606, #43716, #35667, #101432, #39363, #31798, #65210, #80851, #54434, #55498, #6964, #105662, #48481, #81373, #39882, #106177, #64686, #71692, #7484, #13989, #64171, #72755, #23182, #79269, #54975, #97558, #56029, #32340, #87381, #89495, #88960, #23718, #56571, #71175, #15590, #40400, #88437, #95998, #73282, #104600, #30212, #5897, #98104, #14511, #13458, #5392, #46379, #47422, #38313, #96529, #104069, #63097, #22123, #63641, #87906, #46894, #15056, #97041, #79799, #80313, #38828, #47945, #6424, #30755, #22661, #72240, #105142, #31285, #26397, #2057, #92135, #99157, #8023, #17737, #43070, #99701, #82457, #35005, #50597, #34484, #58174, #65747, #1517, #41462, #106721, #8560, #75959, #25315, #75424, #49006, #18283, #91101, #40933, #66270, #90017, #42524, #10157, #33399, #67872, #73827, #25871, #66811, #32870, #50084, #24777, #58728, #17209, #16122, #67352, #51138, #81907, #98627, #59262, #24255, #84054, #82990, #57626, #83513, #57103, #91627, #74352, #90551, #430, #100230, #16660, #9085, #49550, #41994 ),
 ( #74874, #962, #9612, #33942, #36610, #69998, #11737, #61390, #77021, #4734, #3138, #69475, #68416, #60858, #102360, #2591, #93748, #68954, #45721, #19900, #28507, #101826, #77562, #76483, #101309, #86732, #93212, #37672, #52742, #20969, #19376, #86207, #35541, #78084, #26923, #27458, #92673, #20444, #60337, #11204, #52207, #44676, #12807, #18831, #94280, #78602, #85120, #12280, #44137, #102899, #3678, #85665, #36084, #53287, #100755, #27991, #53803, #45210, #51674, #4203, #37132, #29063, #61933, #94822, #59797, #84596, #10678, #43594, #64565, #63512, #54853, #22541, #87255, #23594, #64048, #30624, #104478, #31679, #81250, #97433, #29575, #39239, #80723, #6299, #39764, #88313, #31162, #46779, #7365, #79674, #72113, #38195, #96410, #105022, #79142, #55384, #38706, #15464, #14388, #96923, #71570, #47299, #46256, #71054, #56442, #62974, #70534, #80195, #89375, #95875, #55898, #5268, #47819, #103425, #103945, #62447, #23059, #30091, #87782, #22000, #88833, #48357, #95338, #14927, #21474, #13865, #6841, #5784, #72640, #105541, #54309, #13331, #66144, #93498, #40804, #101577, #58047, #97981, #81775, #90970, #43864, #90429, #74229, #51946, #57506, #101037, #49423, #35817, #33274, #24654, #99026, #76756, #49956, #24135, #60082, #25189, #48881, #56978, #73697, #92946, #76224, #35272, #16532, #7898, #89893, #84861, #27736, #68698, #2330, #17080, #82864, #68143, #10943, #106054, #19108, #8961, #2864, #60607, #16005, #73153, #82326, #19645, #307, #106600, #27192, #52478, #8437, #85396, #40277, #41338, #32206, #43341, #65622, #32750, #65083, #98505, #53026, #85949, #87001, #3416 ),
 ( #86486, #63250, #78350, #13071, #12544, #95092, #94016, #12020, #104214, #3946, #22276, #4472, #38454, #36878, #103695, #44952, #95607, #44407, #77835, #36358, #37940, #69745, #28796, #102639, #62209, #30359, #69227, #46001, #96143, #61679, #29841, #94567, #87524, #21228, #103174, #20717, #37411, #55123, #53555, #71320, #29317, #102096, #45479, #54057, #13606, #70275, #78881, #21749, #5008, #70800, #62718, #5528, #54585, #46519, #79416, #11479, #77301, #28255, #61125, #20176, #96669, #71845, #88576, #32489, #15739, #81508, #31434, #22805, #104751, #24405, #73967, #82056, #48622, #7109, #97708, #7629, #57243, #47037, #65360, #23873, #90163, #16267, #63782, #14134, #64311, #8177, #15205, #55641, #40547, #106322, #23327, #73430, #98251, #97183, #49152, #64829, #6575, #14658, #56167, #41083, #47567, #80463, #56717, #79936, #30902, #47, #33020, #48093, #80992, #65886, #98768, #24921, #6046, #89638, #88053, #38972, #39507, #105808, #72381, #89109, #105287, #40025, #72898, #31948, #100900, #43737, #51817, #92273, #83647, #67495, #18426, #27068, #16812, #35144, #100374, #59951, #92817, #33540, #90702, #34092, #84733, #91767, #66413, #10298, #76096, #99843, #43211, #51281, #66965, #84202, #34624, #83133, #99296, #26015, #68014, #25470, #58326, #26537, #49699, #74499, #10816, #2197, #17889, #50741, #18974, #68566, #76625, #82603, #59409, #2736, #35691, #101451, #75572, #57775, #58875, #8707, #9758, #41615, #91250, #42673, #576, #17357, #1667, #50231, #9230, #42135, #75021, #1118, #4343, #3285, #28128, #13476, #20047, #38331, #20595, #54451, #52895, #12946, #69094, #4879 ) ),
 .UNSPECIFIED., .F., .F., .F. ) 
 B_SPLINE_SURFACE_WITH_KNOTS ( ( 3, 3 ),
 ( 4, 2, 2, 2, 2, 2, 2, 2, 2, 2, 2, 2, 2, 2, 2, 2, 2, 2, 2, 2, 2, 2, 2, 2, 2, 2, 2, 2, 2, 2, 2, 2, 2, 2, 2, 2, 2, 2, 2, 2, 2, 2, 2, 2, 2, 2, 2, 2, 2, 2, 2, 2, 2, 2, 2, 2, 2, 2, 2, 2, 2, 2, 2, 2, 2, 2, 2, 2, 2, 2, 2, 2, 2, 2, 2, 2, 2, 2, 2, 2, 2, 2, 2, 2, 2, 2, 2, 2, 2, 2, 2, 2, 2, 2, 2, 2, 2, 2, 2, 4 ),
 ( 0.000000000000000000, 1.000000000000000000 ),
 ( 0.000000000000000000, 0.008346361953628917210, 0.01669272390725783442, 0.03338544781451566884, 0.04173180976814458432, 0.05007817172177350673, 0.05425135269858796794, 0.05842453367540242221, 0.06677089562903133768, 0.07511725758266024622, 0.07929043855947470743, 0.08346361953628916863, 0.08555021002469639924, 0.08763680051310362984, 0.09180998148991809105, 0.09389657197832532165, 0.09493986722252893695, 0.09598316246673255225, 0.09806975295513978286, 0.1001563434435470135, 0.1011996386877506288, 0.1022429339319542441, 0.1043295244203614747, 0.1085027053971759359, 0.1126758863739903971, 0.1168490673508048444, 0.1210222483276192917, 0.1251954293044337529, 0.1335417912580626754, 0.1418881532116915700, 0.1502345151653204924, 0.1669272390725783373, 0.1836199629798361821, 0.2003126868870940269, 0.2336981347016096888, 0.2503908586088675059, 0.2670835825161253507, 0.2754299444697542176, 0.2837763064233831400, 0.2921226683770120625, 0.2962958493538265237, 0.3004690303306409849, 0.3025556208190481877, 0.3046422113074554461, 0.3088153922842699073, 0.3109019827726771101, 0.3119452780168807671, 0.3129885732610843685, 0.3150751637494916269, 0.3161184589936952283, 0.3171617542378988297, 0.3192483447263060325, 0.3202916399705096895, 0.3213349352147132909, 0.3255081161915277521, 0.3265514114357313535, 0.3275947066799349550, 0.3296812971683422133, 0.3317678876567494717, 0.3338544781451566745, 0.3359410686335638774, 0.3380276591219711357, 0.3390709543661747372, 0.3401142496103783941, 0.3422008400987855969, 0.3442874305871927998, 0.3453307258313964567, 0.3463740210756000582, 0.3505472020524145194, 0.3547203830292289806, 0.3588935640060434418, 0.3630667449828579030, 0.3672399259596723642, 0.3755862879133012866, 0.3839326498669302090, 0.3922790118205591314, 0.4006253737741880538, 0.4173180976814458987, 0.4340108215887037435, 0.4507035454959615883, 0.4590499074495905107, 0.4673962694032193776, 0.4757426313568482446, 0.4799158123336627058, 0.4840889933104771670, 0.4882621742872916282, 0.4924353552641060894, 0.4945219457525132922, 0.4966085362409205506, 0.5007817172177350118, 0.5028683077061422146, 0.5039116029503458716, 0.5049548981945495285, 0.5091280791713639342, 0.5112146696597711371, 0.5133012601481783399, 0.5174744411249928566, 0.5216476221018073733, 0.5258208030786217790, 0.5341671650322507015 ),
 .UNSPECIFIED. ) 
 GEOMETRIC_REPRESENTATION_ITEM ( )  RATIONAL_B_SPLINE_SURFACE ( (
 ( 1.000000000000000000, 1.000000000000000000, 1.000000000000000000, 1.000000000000000000, 1.000000000000000000, 1.000000000000000000, 1.000000000000000000, 1.000000000000000000, 1.000000000000000000, 1.000000000000000000, 1.000000000000000000, 1.000000000000000000, 1.000000000000000000, 1.000000000000000000, 1.000000000000000000, 1.000000000000000000, 1.000000000000000000, 1.000000000000000000, 1.000000000000000000, 1.000000000000000000, 1.000000000000000000, 1.000000000000000000, 1.000000000000000000, 1.000000000000000000, 1.000000000000000000, 1.000000000000000000, 1.000000000000000000, 1.000000000000000000, 1.000000000000000000, 1.000000000000000000, 1.000000000000000000, 1.000000000000000000, 1.000000000000000000, 1.000000000000000000, 1.000000000000000000, 1.000000000000000000, 1.000000000000000000, 1.000000000000000000, 1.000000000000000000, 1.000000000000000000, 1.000000000000000000, 1.000000000000000000, 1.000000000000000000, 1.000000000000000000, 1.000000000000000000, 1.000000000000000000, 1.000000000000000000, 1.000000000000000000, 1.000000000000000000, 1.000000000000000000, 1.000000000000000000, 1.000000000000000000, 1.000000000000000000, 1.000000000000000000, 1.000000000000000000, 1.000000000000000000, 1.000000000000000000, 1.000000000000000000, 1.000000000000000000, 1.000000000000000000, 1.000000000000000000, 1.000000000000000000, 1.000000000000000000, 1.000000000000000000, 1.000000000000000000, 1.000000000000000000, 1.000000000000000000, 1.000000000000000000, 1.000000000000000000, 1.000000000000000000, 1.000000000000000000, 1.000000000000000000, 1.000000000000000000, 1.000000000000000000, 1.000000000000000000, 1.000000000000000000, 1.000000000000000000, 1.000000000000000000, 1.000000000000000000, 1.000000000000000000, 1.000000000000000000, 1.000000000000000000, 1.000000000000000000, 1.000000000000000000, 1.000000000000000000, 1.000000000000000000, 1.000000000000000000, 1.000000000000000000, 1.000000000000000000, 1.000000000000000000, 1.000000000000000000, 1.000000000000000000, 1.000000000000000000, 1.000000000000000000, 1.000000000000000000, 1.000000000000000000, 1.000000000000000000, 1.000000000000000000, 1.000000000000000000, 1.000000000000000000, 1.000000000000000000, 1.000000000000000000, 1.000000000000000000, 1.000000000000000000, 1.000000000000000000, 1.000000000000000000, 1.000000000000000000, 1.000000000000000000, 1.000000000000000000, 1.000000000000000000, 1.000000000000000000, 1.000000000000000000, 1.000000000000000000, 1.000000000000000000, 1.000000000000000000, 1.000000000000000000, 1.000000000000000000, 1.000000000000000000, 1.000000000000000000, 1.000000000000000000, 1.000000000000000000, 1.000000000000000000, 1.000000000000000000, 1.000000000000000000, 1.000000000000000000, 1.000000000000000000, 1.000000000000000000, 1.000000000000000000, 1.000000000000000000, 1.000000000000000000, 1.000000000000000000, 1.000000000000000000, 1.000000000000000000, 1.000000000000000000, 1.000000000000000000, 1.000000000000000000, 1.000000000000000000, 1.000000000000000000, 1.000000000000000000, 1.000000000000000000, 1.000000000000000000, 1.000000000000000000, 1.000000000000000000, 1.000000000000000000, 1.000000000000000000, 1.000000000000000000, 1.000000000000000000, 1.000000000000000000, 1.000000000000000000, 1.000000000000000000, 1.000000000000000000, 1.000000000000000000, 1.000000000000000000, 1.000000000000000000, 1.000000000000000000, 1.000000000000000000, 1.000000000000000000, 1.000000000000000000, 1.000000000000000000, 1.000000000000000000, 1.000000000000000000, 1.000000000000000000, 1.000000000000000000, 1.000000000000000000, 1.000000000000000000, 1.000000000000000000, 1.000000000000000000, 1.000000000000000000, 1.000000000000000000, 1.000000000000000000, 1.000000000000000000, 1.000000000000000000, 1.000000000000000000, 1.000000000000000000, 1.000000000000000000, 1.000000000000000000, 1.000000000000000000, 1.000000000000000000, 1.000000000000000000, 1.000000000000000000, 1.000000000000000000, 1.000000000000000000, 1.000000000000000000, 1.000000000000000000, 1.000000000000000000, 1.000000000000000000, 1.000000000000000000, 1.000000000000000000, 1.000000000000000000, 1.000000000000000000, 1.000000000000000000, 1.000000000000000000, 1.000000000000000000, 1.000000000000000000, 1.000000000000000000, 1.000000000000000000, 1.000000000000000000, 1.000000000000000000, 1.000000000000000000, 1.000000000000000000),
 ( 1.857142857142858317, 1.857142857142858317, 1.857142857142858317, 1.857142857142858317, 1.857142857142858317, 1.857142857142858317, 1.857142857142858317, 1.857142857142858317, 1.857142857142858317, 1.857142857142858317, 1.857142857142858317, 1.857142857142858317, 1.857142857142858317, 1.857142857142858317, 1.857142857142858317, 1.857142857142858317, 1.857142857142858317, 1.857142857142858317, 1.857142857142858317, 1.857142857142858317, 1.857142857142858317, 1.857142857142858317, 1.857142857142858317, 1.857142857142858317, 1.857142857142858317, 1.857142857142858317, 1.857142857142858317, 1.857142857142858317, 1.857142857142858317, 1.857142857142858317, 1.857142857142858317, 1.857142857142858317, 1.857142857142858317, 1.857142857142858317, 1.857142857142858317, 1.857142857142858317, 1.857142857142858317, 1.857142857142858317, 1.857142857142858317, 1.857142857142858317, 1.857142857142858317, 1.857142857142858317, 1.857142857142858317, 1.857142857142858317, 1.857142857142858317, 1.857142857142858317, 1.857142857142858317, 1.857142857142858317, 1.857142857142858317, 1.857142857142858317, 1.857142857142858317, 1.857142857142858317, 1.857142857142858317, 1.857142857142858317, 1.857142857142858317, 1.857142857142858317, 1.857142857142858317, 1.857142857142858317, 1.857142857142858317, 1.857142857142858317, 1.857142857142858317, 1.857142857142858317, 1.857142857142858317, 1.857142857142858317, 1.857142857142858317, 1.857142857142858317, 1.857142857142858317, 1.857142857142858317, 1.857142857142858317, 1.857142857142858317, 1.857142857142858317, 1.857142857142858317, 1.857142857142858317, 1.857142857142858317, 1.857142857142858317, 1.857142857142858317, 1.857142857142858317, 1.857142857142858317, 1.857142857142858317, 1.857142857142858317, 1.857142857142858317, 1.857142857142858317, 1.857142857142858317, 1.857142857142858317, 1.857142857142858317, 1.857142857142858317, 1.857142857142858317, 1.857142857142858317, 1.857142857142858317, 1.857142857142858317, 1.857142857142858317, 1.857142857142858317, 1.857142857142858317, 1.857142857142858317, 1.857142857142858317, 1.857142857142858317, 1.857142857142858317, 1.857142857142858317, 1.857142857142858317, 1.857142857142858317, 1.857142857142858317, 1.857142857142858317, 1.857142857142858317, 1.857142857142858317, 1.857142857142858317, 1.857142857142858317, 1.857142857142858317, 1.857142857142858317, 1.857142857142858317, 1.857142857142858317, 1.857142857142858317, 1.857142857142858317, 1.857142857142858317, 1.857142857142858317, 1.857142857142858317, 1.857142857142858317, 1.857142857142858317, 1.857142857142858317, 1.857142857142858317, 1.857142857142858317, 1.857142857142858317, 1.857142857142858317, 1.857142857142858317, 1.857142857142858317, 1.857142857142858317, 1.857142857142858317, 1.857142857142858317, 1.857142857142858317, 1.857142857142858317, 1.857142857142858317, 1.857142857142858317, 1.857142857142858317, 1.857142857142858317, 1.857142857142858317, 1.857142857142858317, 1.857142857142858317, 1.857142857142858317, 1.857142857142858317, 1.857142857142858317, 1.857142857142858317, 1.857142857142858317, 1.857142857142858317, 1.857142857142858317, 1.857142857142858317, 1.857142857142858317, 1.857142857142858317, 1.857142857142858317, 1.857142857142858317, 1.857142857142858317, 1.857142857142858317, 1.857142857142858317, 1.857142857142858317, 1.857142857142858317, 1.857142857142858317, 1.857142857142858317, 1.857142857142858317, 1.857142857142858317, 1.857142857142858317, 1.857142857142858317, 1.857142857142858317, 1.857142857142858317, 1.857142857142858317, 1.857142857142858317, 1.857142857142858317, 1.857142857142858317, 1.857142857142858317, 1.857142857142858317, 1.857142857142858317, 1.857142857142858317, 1.857142857142858317, 1.857142857142858317, 1.857142857142858317, 1.857142857142860093, 1.857142857142860093, 1.857142857142858317, 1.857142857142858317, 1.857142857142858317, 1.857142857142858317, 1.857142857142858317, 1.857142857142858317, 1.857142857142858317, 1.857142857142858317, 1.857142857142858317, 1.857142857142858317, 1.857142857142858317, 1.857142857142858317, 1.857142857142858317, 1.857142857142858317, 1.857142857142858317, 1.857142857142858317, 1.857142857142858317, 1.857142857142858317, 1.857142857142858317, 1.857142857142858317, 1.857142857142858317, 1.857142857142858317, 1.857142857142860981, 1.857142857142860981, 1.857142857142858317, 1.857142857142858317),
 ( 1.000000000000000000, 1.000000000000000000, 1.000000000000000000, 1.000000000000000000, 1.000000000000000000, 1.000000000000000000, 1.000000000000000000, 1.000000000000000000, 1.000000000000000000, 1.000000000000000000, 1.000000000000000000, 1.000000000000000000, 1.000000000000000000, 1.000000000000000000, 1.000000000000000000, 1.000000000000000000, 1.000000000000000000, 1.000000000000000000, 1.000000000000000000, 1.000000000000000000, 1.000000000000000000, 1.000000000000000000, 1.000000000000000000, 1.000000000000000000, 1.000000000000000000, 1.000000000000000000, 1.000000000000000000, 1.000000000000000000, 1.000000000000000000, 1.000000000000000000, 1.000000000000000000, 1.000000000000000000, 1.000000000000000000, 1.000000000000000000, 1.000000000000000000, 1.000000000000000000, 1.000000000000000000, 1.000000000000000000, 1.000000000000000000, 1.000000000000000000, 1.000000000000000000, 1.000000000000000000, 1.000000000000000000, 1.000000000000000000, 1.000000000000000000, 1.000000000000000000, 1.000000000000000000, 1.000000000000000000, 1.000000000000000000, 1.000000000000000000, 1.000000000000000000, 1.000000000000000000, 1.000000000000000000, 1.000000000000000000, 1.000000000000000000, 1.000000000000000000, 1.000000000000000000, 1.000000000000000000, 1.000000000000000000, 1.000000000000000000, 1.000000000000000000, 1.000000000000000000, 1.000000000000000000, 1.000000000000000000, 1.000000000000000000, 1.000000000000000000, 1.000000000000000000, 1.000000000000000000, 1.000000000000000000, 1.000000000000000000, 1.000000000000000000, 1.000000000000000000, 1.000000000000000000, 1.000000000000000000, 1.000000000000000000, 1.000000000000000000, 1.000000000000000000, 1.000000000000000000, 1.000000000000000000, 1.000000000000000000, 1.000000000000000000, 1.000000000000000000, 1.000000000000000000, 1.000000000000000000, 1.000000000000000000, 1.000000000000000000, 1.000000000000000000, 1.000000000000000000, 1.000000000000000000, 1.000000000000000000, 1.000000000000000000, 1.000000000000000000, 1.000000000000000000, 1.000000000000000000, 1.000000000000000000, 1.000000000000000000, 1.000000000000000000, 1.000000000000000000, 1.000000000000000000, 1.000000000000000000, 1.000000000000000000, 1.000000000000000000, 1.000000000000000000, 1.000000000000000000, 1.000000000000000000, 1.000000000000000000, 1.000000000000000000, 1.000000000000000000, 1.000000000000000000, 1.000000000000000000, 1.000000000000000000, 1.000000000000000000, 1.000000000000000000, 1.000000000000000000, 1.000000000000000000, 1.000000000000000000, 1.000000000000000000, 1.000000000000000000, 1.000000000000000000, 1.000000000000000000, 1.000000000000000000, 1.000000000000000000, 1.000000000000000000, 1.000000000000000000, 1.000000000000000000, 1.000000000000000000, 1.000000000000000000, 1.000000000000000000, 1.000000000000000000, 1.000000000000000000, 1.000000000000000000, 1.000000000000000000, 1.000000000000000000, 1.000000000000000000, 1.000000000000000000, 1.000000000000000000, 1.000000000000000000, 1.000000000000000000, 1.000000000000000000, 1.000000000000000000, 1.000000000000000000, 1.000000000000000000, 1.000000000000000000, 1.000000000000000000, 1.000000000000000000, 1.000000000000000000, 1.000000000000000000, 1.000000000000000000, 1.000000000000000000, 1.000000000000000000, 1.000000000000000000, 1.000000000000000000, 1.000000000000000000, 1.000000000000000000, 1.000000000000000000, 1.000000000000000000, 1.000000000000000000, 1.000000000000000000, 1.000000000000000000, 1.000000000000000000, 1.000000000000000000, 1.000000000000000000, 1.000000000000000000, 1.000000000000000000, 1.000000000000000000, 1.000000000000000000, 1.000000000000000000, 1.000000000000000000, 1.000000000000000000, 1.000000000000000000, 1.000000000000000000, 1.000000000000000000, 1.000000000000000000, 1.000000000000000000, 1.000000000000000000, 1.000000000000000000, 1.000000000000000000, 1.000000000000000000, 1.000000000000000000, 1.000000000000000000, 1.000000000000000000, 1.000000000000000000, 1.000000000000000000, 1.000000000000000000, 1.000000000000000000, 1.000000000000000000, 1.000000000000000000, 1.000000000000000000, 1.000000000000000000, 1.000000000000000000, 1.000000000000000000, 1.000000000000000000, 1.000000000000000000, 1.000000000000000000, 1.000000000000000000, 1.000000000000000000, 1.000000000000000000, 1.000000000000000000, 1.000000000000000000, 1.000000000000000000) ) ) 
 REPRESENTATION_ITEM ( '' )  SURFACE ( )  );
#79036 = VERTEX_POINT ( 'NONE', #87210 ) ;
#79037 = CARTESIAN_POINT ( 'NONE',  ( -23.93420880016847008, -4.285714285714296246, 8.127057321558250891 ) ) ;
#79038 = CARTESIAN_POINT ( 'NONE',  ( 13.99999999999998046, 59.99999999999999289, 6.999999999999994671 ) ) ;
#79039 = CARTESIAN_POINT ( 'NONE',  ( 93.39999999999999147, 1.023464760207051730E-14, 0.000000000000000000 ) ) ;
#79040 = AXIS2_PLACEMENT_3D ( 'NONE', #38477, #62233, #45506 ) ;
#79041 = CARTESIAN_POINT ( 'NONE',  ( 0.000000000000000000, 195.0000000000000000, 2.000000000000011102 ) ) ;
#79042 = DIRECTION ( 'NONE',  ( -0.000000000000000000, -1.000000000000000000, -0.000000000000000000 ) ) ;
#79043 = FILL_AREA_STYLE_COLOUR ( '', #17672 ) ;
#79044 = VERTEX_POINT ( 'NONE', #13285 ) ;
#79045 = AXIS2_PLACEMENT_3D ( 'NONE', #102722, #28885, #95690 ) ;
#79046 = CARTESIAN_POINT ( 'NONE',  ( 5.000000000000000000, 6.123233995736766282E-16, -1.446714285714285841 ) ) ;
#79047 = CARTESIAN_POINT ( 'NONE',  ( 89.07481883248233601, -29.99999999999995737, 188.8186571231210564 ) ) ;
#79048 = CARTESIAN_POINT ( 'NONE',  ( -10.55482376525340094, 17.82747234158580696, -9.593668801698457926 ) ) ;
#79049 = DIRECTION ( 'NONE',  ( 0.000000000000000000, 0.000000000000000000, 1.000000000000000000 ) ) ;
#79050 = CARTESIAN_POINT ( 'NONE',  ( 81.13650333864865161, -30.00000000000000711, 1.865448809746575343 ) ) ;
#79051 = DIRECTION ( 'NONE',  ( 0.5735764363510554853, 0.8191520442889852482, 0.000000000000000000 ) ) ;
#79052 = ORIENTED_EDGE ( 'NONE', *, *, #98566, .T. ) ;
#79053 = EDGE_CURVE ( 'NONE', #43916, #47808, #63767, .T. ) ;
#79054 = EDGE_CURVE ( 'NONE', #31379, #78599, #102342, .T. ) ;
#79055 = ORIENTED_EDGE ( 'NONE', *, *, #50847, .T. ) ;
#79056 = VERTEX_POINT ( 'NONE', #73098 ) ;
#79057 = LINE ( 'NONE', #55293, #77906 ) ;
#79058 = FACE_OUTER_BOUND ( 'NONE', #58575, .T. ) ;
#79059 = CARTESIAN_POINT ( 'NONE',  ( -37.40770385488823280, 25.53062906199498983, -13.45617127781034839 ) ) ;
#79060 = CARTESIAN_POINT ( 'NONE',  ( -8.559508646656389885, -1.200000000000000030E-05, -1.531152949374502859 ) ) ;
#79061 = CARTESIAN_POINT ( 'NONE',  ( -1.000000000000770495, -69.59657292934927852, 12.76848391599230581 ) ) ;
#79062 = CARTESIAN_POINT ( 'NONE',  ( -6.928203230275509661, -85.26526156932588663, 4.000000000000001776 ) ) ;
#79063 = CARTESIAN_POINT ( 'NONE',  ( -33.50421398922254923, 488.2600042842250332, 10.59612602189812414 ) ) ;
#79064 = ORIENTED_EDGE ( 'NONE', *, *, #26899, .T. ) ;
#79066 = EDGE_CURVE ( 'NONE', #3905, #43590, #36862, .T. ) ;
#79065 = LINE ( 'NONE', #78524, #9860 ) ;
#79067 = ORIENTED_EDGE ( 'NONE', *, *, #60913, .T. ) ;
#79068 = DIRECTION ( 'NONE',  ( 0.000000000000000000, 0.000000000000000000, 1.000000000000000000 ) ) ;
#79069 = FILL_AREA_STYLE ('',( #69920 ) ) ;
#79070 = CARTESIAN_POINT ( 'NONE',  ( -41.13328595189528158, 484.9084785457653197, -3.795084846866993988 ) ) ;
#79071 = AXIS2_PLACEMENT_3D ( 'NONE', #103508, #86291, #21049 ) ;
#79072 = DIRECTION ( 'NONE',  ( 1.150791560227848297E-16, -0.3420201433256725987, 0.9396926207859068736 ) ) ;
#79073 = CARTESIAN_POINT ( 'NONE',  ( 63.13592217280013585, -42.95845782474785324, 82.55303697426595022 ) ) ;
#79074 = ORIENTED_EDGE ( 'NONE', *, *, #61242, .T. ) ;
#79075 = EDGE_CURVE ( 'NONE', #36, #52979, #58611, .T. ) ;
#79076 = CARTESIAN_POINT ( 'NONE',  ( 40.02527844605699414, 463.9419950688768495, 18.74737584574104332 ) ) ;
#79077 = CARTESIAN_POINT ( 'NONE',  ( -54.10267422029167506, -36.39685484491198508, -35.43891616374990861 ) ) ;
#79078 = CARTESIAN_POINT ( 'NONE',  ( -6.879789419156628227, 9.213335847798312273, -1.315101155215614881 ) ) ;
#79079 = CARTESIAN_POINT ( 'NONE',  ( -9.108279475058850494, 51.39276620778235838, 3.907239883328841312 ) ) ;
#79080 = VERTEX_POINT ( 'NONE', #55850 ) ;
#79081 = CARTESIAN_POINT ( 'NONE',  ( 101.2019940638598854, -2.002967142162725287E-29, 5.000000000000011546 ) ) ;
#79082 = FACE_OUTER_BOUND ( 'NONE', #21, .T. ) ;
#79083 = VECTOR ( 'NONE', #49725, 1000.000000000000114 ) ;
#79084 = CARTESIAN_POINT ( 'NONE',  ( 71.14984002819953446, 6.856755485862130937E-15, 0.000000000000000000 ) ) ;
#79085 = CARTESIAN_POINT ( 'NONE',  ( 8.000000000000000000, -27.68750000409677270, 0.000000000000000000 ) ) ;
#79086 = CARTESIAN_POINT ( 'NONE',  ( 2.055025722541617750, 6.319083845364131591, -5.720331885005371930 ) ) ;
#79087 = CARTESIAN_POINT ( 'NONE',  ( 87.02613672383397159, -35.40267602311793382, 188.2183129969156994 ) ) ;
#79088 = MECHANICAL_DESIGN_GEOMETRIC_PRESENTATION_REPRESENTATION (  '', ( #5036 ), #39454 ) ;
#79089 = CARTESIAN_POINT ( 'NONE',  ( 44.26781960101214963, 464.1284203585717592, 8.781346234564500364 ) ) ;
#79090 = CARTESIAN_POINT ( 'NONE',  ( -9.838569036983576765, 7.857203345569047315, 5.000000000000000888 ) ) ;
#79091 = CARTESIAN_POINT ( 'NONE',  ( 7.986539162393901492, -6.026728289425493656, -0.5321833565149887146 ) ) ;
#79092 = CARTESIAN_POINT ( 'NONE',  ( -43.51595707228967314, 485.1238408984097532, -1.707557185901023677 ) ) ;
#79093 = CARTESIAN_POINT ( 'NONE',  ( 13.76566278825922574, -50.82203498049078405, 29.56014984665260670 ) ) ;
#79094 = CARTESIAN_POINT ( 'NONE',  ( 35.11649460235492626, 436.5236565062589875, 6.589765443822644286 ) ) ;
#79095 = CARTESIAN_POINT ( 'NONE',  ( -97.53946591935846300, -30.00000000000000000, 134.3205009627786524 ) ) ;
#79096 = EDGE_CURVE ( 'NONE', #11751, #6495, #82276, .T. ) ;
#79097 = CIRCLE ( 'NONE', #68804, 4.000000000000000888 ) ;
#79098 = CARTESIAN_POINT ( 'NONE',  ( 0.000000000000000000, -1.000000000000000000, 0.000000000000000000 ) ) ;
#79099 = CARTESIAN_POINT ( 'NONE',  ( 4.499670101681318535, -57.67121445897252130, 41.60302808447698908 ) ) ;
#79101 = DIRECTION ( 'NONE',  ( 1.000000000000000000, 0.000000000000000000, -0.000000000000000000 ) ) ;
#79100 = CARTESIAN_POINT ( 'NONE',  ( 12.80748990434369716, 8.843371560882051341, -9.113774775587792476 ) ) ;
#79102 = EDGE_CURVE ( 'NONE', #55070, #103417, #40230, .T. ) ;
#79103 = ADVANCED_FACE ( 'NONE', ( #80676 ), #62183, .T. ) ;
#79105 = DIRECTION ( 'NONE',  ( -1.000000000000000000, 0.000000000000000000, 0.000000000000000000 ) ) ;
#79104 = VECTOR ( 'NONE', #29844, 1000.000000000000000 ) ;
#79106 = CARTESIAN_POINT ( 'NONE',  ( -17.49999999999997513, 50.00000000000000000, 63.82142195434425958 ) ) ;
#79107 = CARTESIAN_POINT ( 'NONE',  ( -10.00000000000000000, 15.00000000000000000, 1.544939622598903828 ) ) ;
#79108 = CARTESIAN_POINT ( 'NONE',  ( 93.97977184163765685, -2.002967142162725287E-29, 5.000000000000011546 ) ) ;
#79109 = DIRECTION ( 'NONE',  ( 0.000000000000000000, 0.000000000000000000, -1.000000000000000000 ) ) ;
#79110 = EDGE_CURVE ( 'NONE', #15319, #42431, #10488, .T. ) ;
#79111 = CARTESIAN_POINT ( 'NONE',  ( -87.26825944249861777, -50.07870994218606597, 192.1711060702807572 ) ) ;
#79112 = ORIENTED_EDGE ( 'NONE', *, *, #90788, .F. ) ;
#79113 = CARTESIAN_POINT ( 'NONE',  ( 40.98863139543689726, 485.5630605922963809, -4.100416933092245309 ) ) ;
#79114 = CARTESIAN_POINT ( 'NONE',  ( -1.569964449840315579, -49.94642998360953356, 101.7846783319226773 ) ) ;
#79115 = CARTESIAN_POINT ( 'NONE',  ( -11.52844523698097667, -56.88420388045057052, 33.40189270011925515 ) ) ;
#79117 = CARTESIAN_POINT ( 'NONE',  ( 46.84999999999999432, 1.533819458162526451E-15, 0.000000000000000000 ) ) ;
#79116 = CARTESIAN_POINT ( 'NONE',  ( -106.4182805671071606, -60.00000000000000000, 168.3060419393721929 ) ) ;
#79118 = ORIENTED_EDGE ( 'NONE', *, *, #74880, .T. ) ;
#79119 = EDGE_CURVE ( 'NONE', #7939, #94793, #95247, .T. ) ;
#79120 = DIRECTION ( 'NONE',  ( 0.000000000000000000, -1.000000000000000000, 0.000000000000000000 ) ) ;
#79121 = EDGE_CURVE ( 'NONE', #94380, #39211, #32702, .T. ) ;
#79122 = CARTESIAN_POINT ( 'NONE',  ( 15.31219705632019235, 3.104419271452464990, -3.118400172706347284 ) ) ;
#79123 = CARTESIAN_POINT ( 'NONE',  ( 1.489880555935390203E-15, 34.19642918197134662, 12.16579798332631945 ) ) ;
#79124 = ORIENTED_EDGE ( 'NONE', *, *, #93806, .T. ) ;
#79125 = FACE_OUTER_BOUND ( 'NONE', #63631, .T. ) ;
#79126 =( GEOMETRIC_REPRESENTATION_CONTEXT ( 3 ) GLOBAL_UNCERTAINTY_ASSIGNED_CONTEXT ( ( #31224 ) ) GLOBAL_UNIT_ASSIGNED_CONTEXT ( ( #21703, #72851, #103648 ) ) REPRESENTATION_CONTEXT ( 'NONE', 'WORKASPACE' ) );
#79128 = DIRECTION ( 'NONE',  ( 0.000000000000000000, 0.000000000000000000, -1.000000000000000000 ) ) ;
#79127 = FACE_OUTER_BOUND ( 'NONE', #91504, .T. ) ;
#79129 = ADVANCED_FACE ( 'NONE', ( #67708 ), #41438, .F. ) ;
#79130 = CARTESIAN_POINT ( 'NONE',  ( -10.50000000000000533, -5.000000000000000000, -55.73109922010478812 ) ) ;
#79131 = CARTESIAN_POINT ( 'NONE',  ( -4.399054598113282921, -1.887557197752925964, 102.7269706464928021 ) ) ;
#79132 = ORIENTED_EDGE ( 'NONE', *, *, #41150, .F. ) ;
#79133 = ORIENTED_EDGE ( 'NONE', *, *, #9345, .F. ) ;
#79134 = CARTESIAN_POINT ( 'NONE',  ( -29.49192533388955084, 326.6740820537864920, 15.30567695811878970 ) ) ;
#79135 = VERTEX_POINT ( 'NONE', #84949 ) ;
#79136 = CARTESIAN_POINT ( 'NONE',  ( 21.38648923915819466, 305.0940074287001380, 9.988878310497041113 ) ) ;
#79137 = DIRECTION ( 'NONE',  ( 0.000000000000000000, -1.000000000000000000, 0.000000000000000000 ) ) ;
#79138 = CARTESIAN_POINT ( 'NONE',  ( 37.61650669486618881, 1.474610560812782335E-15, 0.000000000000000000 ) ) ;
#79139 = ORIENTED_EDGE ( 'NONE', *, *, #37328, .T. ) ;
#79140 = CARTESIAN_POINT ( 'NONE',  ( -4.852941176470599416, -5.000000000000002665, -70.80672828634229177 ) ) ;
#79141 = CARTESIAN_POINT ( 'NONE',  ( -5.342383608296940700, 41.79455473986575242, -70.44171442173730213 ) ) ;
#79142 = CARTESIAN_POINT ( 'NONE',  ( -108.2304173386098114, -60.00000000000612488, 199.3584347283029956 ) ) ;
#79143 = B_SPLINE_CURVE_WITH_KNOTS ( 'NONE', 1,
 ( #45780, #85728, #27516 ),
 .UNSPECIFIED., .F., .F.,
 ( 2, 1, 2 ),
 ( 0.07762659915682808276, 1.000000000000000000, 1.399003598253852676 ),
 .UNSPECIFIED. ) ;
#79144 = CARTESIAN_POINT ( 'NONE',  ( 46.00000000000000000, 487.9838442367869220, -0.2095173675547508108 ) ) ;
#79145 = CARTESIAN_POINT ( 'NONE',  ( 61.20638430029620736, -59.99999999999997868, -37.77879205856383749 ) ) ;
#79146 = DIRECTION ( 'NONE',  ( -0.9605097441496667221, 0.000000000000000000, -0.2782463501890758972 ) ) ;
#79147 = CARTESIAN_POINT ( 'NONE',  ( -5.971402860190597295, 41.34845723532072270, -58.36201413431516727 ) ) ;
#79149 = CARTESIAN_POINT ( 'NONE',  ( 12.57823845030392995, -53.39675556580161242, 32.84955403993266998 ) ) ;
#79148 = CARTESIAN_POINT ( 'NONE',  ( -100.7780794135568954, -14.21045842199427156, 117.1455274902871366 ) ) ;
#79150 = CARTESIAN_POINT ( 'NONE',  ( -7.620083193376602892, 52.13705811446491367, 1.952270494569938952 ) ) ;
#79151 = AXIS2_PLACEMENT_3D ( 'NONE', #17915, #84760, #43761 ) ;
#79152 = CARTESIAN_POINT ( 'NONE',  ( -48.37106977321703738, -39.52344964594737320, 48.17924728568779358 ) ) ;
#79153 = DIRECTION ( 'NONE',  ( 0.000000000000000000, -1.000000000000000000, 0.000000000000000000 ) ) ;
#79154 = ORIENTED_EDGE ( 'NONE', *, *, #79320, .F. ) ;
#79155 = DIRECTION ( 'NONE',  ( 1.000000000000000000, 1.224606353822377258E-16, 0.000000000000000000 ) ) ;
#79156 = CARTESIAN_POINT ( 'NONE',  ( 0.000000000000000000, 0.000000000000000000, -5.283275477074182547 ) ) ;
#79157 =( GEOMETRIC_REPRESENTATION_CONTEXT ( 3 ) GLOBAL_UNCERTAINTY_ASSIGNED_CONTEXT ( ( #101191 ) ) GLOBAL_UNIT_ASSIGNED_CONTEXT ( ( #94021, #79941, #12549 ) ) REPRESENTATION_CONTEXT ( 'NONE', 'WORKASPACE' ) );
#79158 = SURFACE_STYLE_FILL_AREA ( #87268 ) ;
#79159 = ORIENTED_EDGE ( 'NONE', *, *, #2268, .T. ) ;
#79160 = FILL_AREA_STYLE_COLOUR ( '', #4578 ) ;
#79161 = ORIENTED_EDGE ( 'NONE', *, *, #29791, .F. ) ;
#79162 = CARTESIAN_POINT ( 'NONE',  ( 89.41588365431587704, -29.99999999999777245, 199.0983604411771068 ) ) ;
#79163 = CARTESIAN_POINT ( 'NONE',  ( 41.36650669486618881, 1.474610560812782335E-15, 0.000000000000000000 ) ) ;
#79164 = CARTESIAN_POINT ( 'NONE',  ( 57.69562748396144514, 41.99999999999999289, 15.50526908259264225 ) ) ;
#79165 = CARTESIAN_POINT ( 'NONE',  ( 94.55558776287254830, -30.00000000000000000, 191.3215855683534983 ) ) ;
#79166 =( BOUNDED_CURVE ( )  B_SPLINE_CURVE ( 2, ( #54728, #40152, #96811, #73029, #64961, #56855, #7774, #89775, #81647 ),
 .UNSPECIFIED., .F., .F. ) 
 B_SPLINE_CURVE_WITH_KNOTS ( ( 3, 2, 2, 2, 3 ),
 ( 0.7794117647058823595, 0.7867647058823529216, 0.7941176470588234837, 0.8014705882352941568, 0.8088235294117647189 ),
 .UNSPECIFIED. ) 
 CURVE ( )  GEOMETRIC_REPRESENTATION_ITEM ( )  RATIONAL_B_SPLINE_CURVE ( ( 1.000000000000000000, 0.9238795325112867385, 1.000000000000000000, 0.9238795325112867385, 1.000000000000000000, 0.9238795325112867385, 1.000000000000000000, 0.9238795325112867385, 1.000000000000000000 ) ) 
 REPRESENTATION_ITEM ( '' )  );
#79167 = B_SPLINE_SURFACE_WITH_KNOTS ( 'NONE', 3, 3, ( 
 ( #40573, #65386, #105831, #81017, #97730, #56740, #65912, #15764 ),
 ( #75, #57267, #16292, #49177, #98792, #8200, #48645, #41111 ),
 ( #26562, #75596, #36252, #27626, #2762, #60507, #58902, #59434 ),
 ( #100930, #85286, #18451, #17913, #76651, #99871, #26043, #91792 ),
 ( #51846, #67520, #69121, #50766, #10840, #83675, #19538, #1695 ),
 ( #9784, #42700, #92297, #11374, #35713, #93392, #51305, #34651 ),
 ( #84758, #2219, #43238, #100400, #84227, #52375, #44301, #68036 ),
 ( #35169, #10322, #43759, #77195, #59977, #92838, #76123, #27091 ) ),
 .UNSPECIFIED., .F., .F., .F.,
 ( 4, 2, 2, 4 ),
 ( 4, 2, 2, 4 ),
 ( 0.000000000000000000, 0.2500000000000000000, 0.5000000000000000000, 1.000000000000000000 ),
 ( 0.000000000000000000, 0.2500000000000000000, 0.5000000000000000000, 1.000000000000000000 ),
 .UNSPECIFIED. ) ;
#79168 = CARTESIAN_POINT ( 'NONE',  ( 0.3194001229790396357, 3.115132258388582098, 7.999999999999998224 ) ) ;
#79169 = ORIENTED_EDGE ( 'NONE', *, *, #10963, .T. ) ;
#79170 = ADVANCED_FACE ( 'NONE', ( #52037 ), #99517, .T. ) ;
#79171 = B_SPLINE_CURVE_WITH_KNOTS ( 'NONE', 3,
 ( #42481, #24733, #74313, #66224, #50039, #91585, #7441, #17694, #25271, #75377, #74835, #57583, #50554 ),
 .UNSPECIFIED., .F., .F.,
 ( 4, 1, 1, 1, 1, 1, 2, 2, 4 ),
 ( 0.000000000000000000, 0.2499999999999372724, 0.3749999999999085731, 0.4374999999998958611, 0.4687499999998881450, 0.4843749999998855360, 0.4921874999998830380, 0.4999999999998806510, 1.000000000000000000 ),
 .UNSPECIFIED. ) ;
#79172 = VECTOR ( 'NONE', #36299, 1000.000000000000000 ) ;
#79173 = ORIENTED_EDGE ( 'NONE', *, *, #86303, .T. ) ;
#79174 = EDGE_LOOP ( 'NONE', ( #95234, #25442, #103349, #96821 ) ) ;
#79175 = DIRECTION ( 'NONE',  ( 0.000000000000000000, 0.000000000000000000, -1.000000000000000000 ) ) ;
#79176 = CARTESIAN_POINT ( 'NONE',  ( -46.00000000000000000, 438.0166301925364110, 11.64259471675216950 ) ) ;
#79177 = DIRECTION ( 'NONE',  ( 0.000000000000000000, -1.000000000000000000, 0.000000000000000000 ) ) ;
#79178 = ADVANCED_FACE ( 'NONE', ( #11038 ), #11107, .F. ) ;
#79179 = ORIENTED_EDGE ( 'NONE', *, *, #100161, .T. ) ;
#79181 = EDGE_CURVE ( 'NONE', #15859, #70568, #34174, .T. ) ;
#79180 = DIRECTION ( 'NONE',  ( 0.000000000000000000, 0.000000000000000000, 1.000000000000000000 ) ) ;
#79182 = CIRCLE ( 'NONE', #5124, 62.00000000000000000 ) ;
#79183 = ORIENTED_EDGE ( 'NONE', *, *, #46973, .T. ) ;
#79184 = PRESENTATION_STYLE_ASSIGNMENT (( #78636 ) ) ;
#79185 = CARTESIAN_POINT ( 'NONE',  ( 88.55819102178084279, -38.54384100792545098, 200.1464042754968489 ) ) ;
#79186 = CARTESIAN_POINT ( 'NONE',  ( 14.04890433743131872, 4.428206803761019827, 5.208796089510552285 ) ) ;
#79187 = CARTESIAN_POINT ( 'NONE',  ( 84.90898523671995690, -52.70835617166946463, 11.02871142132924120 ) ) ;
#79189 = CARTESIAN_POINT ( 'NONE',  ( 6.222742520105477126, -7.673830019007173320, -0.2914634815676439561 ) ) ;
#79188 = B_SPLINE_CURVE_WITH_KNOTS ( 'NONE', 3,
 ( #82169, #81110, #105911, #23989, #56831, #1774, #51395, #17994, #44931, #43320, #35253, #68676, #76202, #67071, #20155, #76734, #26126, #43843, #11460, #3393 ),
 .UNSPECIFIED., .F., .F.,
 ( 4, 2, 2, 2, 2, 2, 2, 2, 2, 4 ),
 ( 0.003094771980465663586, 0.003598513203823375511, 0.004102254427181087001, 0.004605995650538798926, 0.005109736873896510850, 0.005361607485575363777, 0.005613478097254216703, 0.006117219320611923424, 0.006620960543969630144, 0.007124701767327335997 ),
 .UNSPECIFIED. ) ;
#79190 = CARTESIAN_POINT ( 'NONE',  ( 40.89635135780635977, 427.9313666579921573, 26.89375439067753959 ) ) ;
#79191 = LINE ( 'NONE', #38235, #31617 ) ;
#79192 = VECTOR ( 'NONE', #70040, 1000.000000000000000 ) ;
#79193 = CARTESIAN_POINT ( 'NONE',  ( 7.703928834700302986, 4.447865386531935528, -7.917997657324739258 ) ) ;
#79194 = B_SPLINE_CURVE_WITH_KNOTS ( 'NONE', 3,
 ( #91835, #42210, #8778, #84272, #33094, #42748, #34695, #24995, #43281, #41684, #51360, #99367, #58404, #65959, #67569, #10368, #100450, #17957, #75092, #25545 ),
 .UNSPECIFIED., .F., .F.,
 ( 4, 2, 2, 2, 2, 2, 2, 2, 2, 4 ),
 ( 0.007623009076049266745, 0.008128762804230848030, 0.008381639668321639106, 0.008634516532412430181, 0.009140270260594005394, 0.009646023988775582342, 0.01015177771695715755, 0.01065753144513873450, 0.01116328517332031145, 0.01166903890150188666 ),
 .UNSPECIFIED. ) ;
#79195 = EDGE_CURVE ( 'NONE', #7556, #88005, #15684, .T. ) ;
#79196 = CARTESIAN_POINT ( 'NONE',  ( 0.000000000000000000, 0.000000000000000000, -9.975036109638290682 ) ) ;
#79197 = ORIENTED_EDGE ( 'NONE', *, *, #92680, .F. ) ;
#79198 = DIRECTION ( 'NONE',  ( 0.8191520442889975717, 1.003171929053531773E-16, -0.5735764363510378328 ) ) ;
#79199 = CARTESIAN_POINT ( 'NONE',  ( -34.87421981230464496, 463.4384841829531183, 4.864009048391830348 ) ) ;
#79200 = CARTESIAN_POINT ( 'NONE',  ( -27.10511071441183262, 36.88665068479722464, 7.556984339686156460 ) ) ;
#79201 = VERTEX_POINT ( 'NONE', #23827 ) ;
#79202 = DIRECTION ( 'NONE',  ( -0.000000000000000000, 0.000000000000000000, -1.000000000000000000 ) ) ;
#79203 = CARTESIAN_POINT ( 'NONE',  ( -32.35864103015216386, 300.7401528847129271, 11.27243207037040484 ) ) ;
#79204 = FACE_OUTER_BOUND ( 'NONE', #106750, .T. ) ;
#79205 =( NAMED_UNIT ( * ) PLANE_ANGLE_UNIT ( ) SI_UNIT ( $, .RADIAN. ) );
#79206 = CARTESIAN_POINT ( 'NONE',  ( -8.000000000000001776, -13.15624999999999467, 3.313708498984758943 ) ) ;
#79207 = CARTESIAN_POINT ( 'NONE',  ( 5.895225616202836250, -15.33049738696555586, 34.54478832876725392 ) ) ;
#79208 = PRESENTATION_LAYER_ASSIGNMENT (  '', '', ( #5152 ) ) ;
#79209 = FACE_OUTER_BOUND ( 'NONE', #88161, .T. ) ;
#79210 = ORIENTED_EDGE ( 'NONE', *, *, #46775, .T. ) ;
#79211 = CARTESIAN_POINT ( 'NONE',  ( 84.83276708130827615, -39.37258369601807573, 182.9372201221722491 ) ) ;
#79212 = CARTESIAN_POINT ( 'NONE',  ( -48.15068916914997033, 11.33291430652583465, 14.35535821593516559 ) ) ;
#79213 = FACE_OUTER_BOUND ( 'NONE', #7269, .T. ) ;
#79214 = VERTEX_POINT ( 'NONE', #78832 ) ;
#79215 = CARTESIAN_POINT ( 'NONE',  ( 95.92657667454260206, -57.67157085294456209, 40.82693322936258795 ) ) ;
#79216 = CARTESIAN_POINT ( 'NONE',  ( 33.50185725305296103, 488.2566613463520184, 10.59321780396354029 ) ) ;
#79217 = DIRECTION ( 'NONE',  ( 0.000000000000000000, 1.000000000000000000, 0.000000000000000000 ) ) ;
#79218 = CARTESIAN_POINT ( 'NONE',  ( -30.55529413189687915, 11.20957620317258474, 39.95174307499986099 ) ) ;
#79219 = DIRECTION ( 'NONE',  ( 0.000000000000000000, 0.000000000000000000, 1.000000000000000000 ) ) ;
#79220 = CONICAL_SURFACE ( 'NONE', #74050, 3.309500000000007880, 0.9599310885968770357 ) ;
#79221 = CARTESIAN_POINT ( 'NONE',  ( 15.10968165226510784, -22.75080798962788720, 35.94916242595005684 ) ) ;
#79222 =( NAMED_UNIT ( * ) PLANE_ANGLE_UNIT ( ) SI_UNIT ( $, .RADIAN. ) );
#79223 = CARTESIAN_POINT ( 'NONE',  ( 33.65952191125959558, -23.43196893441297846, 33.04094279894314923 ) ) ;
#79226 = CARTESIAN_POINT ( 'NONE',  ( -14.35785620000130969, 3.948300967446466636, 4.282865182316123231 ) ) ;
#79225 = VECTOR ( 'NONE', #75375, 1000.000000000000000 ) ;
#79224 = CARTESIAN_POINT ( 'NONE',  ( 27.33349330513380693, 1.593028355512270962E-15, 0.000000000000000000 ) ) ;
#79227 = EDGE_CURVE ( 'NONE', #72526, #84586, #31163, .T. ) ;
#79228 = SURFACE_SIDE_STYLE ('',( #54937 ) ) ;
#79229 = CARTESIAN_POINT ( 'NONE',  ( 40.93292669599463096, 378.0706848361106722, 26.55786848468904537 ) ) ;
#79230 = ORIENTED_EDGE ( 'NONE', *, *, #63726, .T. ) ;
#79231 = CARTESIAN_POINT ( 'NONE',  ( 32.65228357897255052, 299.7864930558274068, -0.8975401584249106390 ) ) ;
#79232 = CARTESIAN_POINT ( 'NONE',  ( 27.61650669486618881, 0.000000000000000000, 4.000000000000000888 ) ) ;
#79233 = CARTESIAN_POINT ( 'NONE',  ( -99.81141058005968603, -37.99999999999998579, 138.1247188685539413 ) ) ;
#79234 = VERTEX_POINT ( 'NONE', #4961 ) ;
#79235 = CARTESIAN_POINT ( 'NONE',  ( -12.28040651794425386, -2.772380348077450041, 20.68240731548373645 ) ) ;
#79236 = LINE ( 'NONE', #30175, #90008 ) ;
#79237 = DIRECTION ( 'NONE',  ( 0.5735764363510557073, -0.8191520442889850262, 1.003171929053516612E-16 ) ) ;
#79238 = COLOUR_RGB ( '', 0.08235294, 0.09019608, 0.10196078) ;
#79239 = ADVANCED_FACE ( 'NONE', ( #64266, #89591 ), #21701, .T. ) ;
#79240 = CARTESIAN_POINT ( 'NONE',  ( -4.707071514954599856, -34.58962144921125770, -32.59876395530876891 ) ) ;
#79241 = ORIENTED_EDGE ( 'NONE', *, *, #98877, .F. ) ;
#79242 = CONICAL_SURFACE ( 'NONE', #22474, 5.000000000000001776, 0.9599310885968803664 ) ;
#79243 = CARTESIAN_POINT ( 'NONE',  ( 2.621328321947801854, 7.606199919103181273, -7.633618187056858240 ) ) ;
#79244 = CARTESIAN_POINT ( 'NONE',  ( 0.4033376246892507733, -4.059728990630811829, -5.968343123267133343 ) ) ;
#79245 = ORIENTED_EDGE ( 'NONE', *, *, #86010, .F. ) ;
#79246 = CARTESIAN_POINT ( 'NONE',  ( 30.10549840784159770, 7.858493733726954922, -42.03383688247146921 ) ) ;
#79247 = AXIS2_PLACEMENT_3D ( 'NONE', #9590, #42503, #34459 ) ;
#79248 = CARTESIAN_POINT ( 'NONE',  ( -44.11327388758650159, 464.4313852428384735, 9.822198357558047377 ) ) ;
#79249 = CARTESIAN_POINT ( 'NONE',  ( -92.26459300646831707, -60.00000000000002132, 2.000424519725360284 ) ) ;
#79250 = ORIENTED_EDGE ( 'NONE', *, *, #95841, .F. ) ;
#79251 = CARTESIAN_POINT ( 'NONE',  ( 3.313708498984771378, -27.96875000409677270, 7.999999999999988454 ) ) ;
#79252 = DIRECTION ( 'NONE',  ( 0.000000000000000000, 0.000000000000000000, -1.000000000000000000 ) ) ;
#79253 = CARTESIAN_POINT ( 'NONE',  ( -9.646032546913145822, 26.98719671525633501, 2.644051433538242790 ) ) ;
#79255 = CARTESIAN_POINT ( 'NONE',  ( 54.52222222222221859, 6.915964383211875250E-15, 0.000000000000000000 ) ) ;
#79254 = FILL_AREA_STYLE_COLOUR ( '', #4386 ) ;
#79256 = EDGE_CURVE ( 'NONE', #85984, #80639, #47131, .T. ) ;
#79257 = CIRCLE ( 'NONE', #20744, 4.000000000000001776 ) ;
#79258 = CARTESIAN_POINT ( 'NONE',  ( -85.65078221568934680, -18.54887076467624141, 161.4868767356897195 ) ) ;
#79259 = ORIENTED_EDGE ( 'NONE', *, *, #53898, .T. ) ;
#79260 = CARTESIAN_POINT ( 'NONE',  ( 6.837824896291514243, 3.947820044545422569, -6.564402953523715389 ) ) ;
#79261 = ORIENTED_EDGE ( 'NONE', *, *, #67207, .F. ) ;
#79262 = ORIENTED_EDGE ( 'NONE', *, *, #70545, .T. ) ;
#79263 = CARTESIAN_POINT ( 'NONE',  ( 32.10523163092994992, 436.9431439331139586, 23.91259324438140510 ) ) ;
#79264 = CARTESIAN_POINT ( 'NONE',  ( -2.179633855064840198, -70.50537186176407545, 13.16847616745739558 ) ) ;
#79266 = ORIENTED_EDGE ( 'NONE', *, *, #95429, .F. ) ;
#79265 = B_SPLINE_CURVE_WITH_KNOTS ( 'NONE', 3,
 ( #41249, #35723, #3315, #10853, #36262, #11926, #52928, #85854, #43249, #92311, #69130, #84237 ),
 .UNSPECIFIED., .F., .F.,
 ( 4, 2, 2, 2, 2, 4 ),
 ( 0.000000000000000000, 0.0004272229515409421198, 0.0008544459030818842395, 0.001708891806163794283, 0.002563337709245704001, 0.003417783612327614153 ),
 .UNSPECIFIED. ) ;
#79267 = CARTESIAN_POINT ( 'NONE',  ( 16.32418145836348700, 45.71594865110100869, -6.626690021756291848 ) ) ;
#79268 = DIRECTION ( 'NONE',  ( 0.7663137714224784736, 0.000000000000000000, 0.6424665000825005023 ) ) ;
#79269 = CARTESIAN_POINT ( 'NONE',  ( -107.1080015683288025, -57.65528894494657663, 199.9870551016494744 ) ) ;
#79270 = DIRECTION ( 'NONE',  ( -1.000000000000000000, -0.000000000000000000, -0.000000000000000000 ) ) ;
#79271 = CARTESIAN_POINT ( 'NONE',  ( -17.47333451427476447, 294.5877965850818327, -2.055689352271495629 ) ) ;
#79272 = FILL_AREA_STYLE ('',( #35671 ) ) ;
#79273 = PRESENTATION_STYLE_ASSIGNMENT (( #62066 ) ) ;
#79274 = CARTESIAN_POINT ( 'NONE',  ( -17.99621717127797993, 36.54019273113858191, -22.85642881224880796 ) ) ;
#79275 = AXIS2_PLACEMENT_3D ( 'NONE', #86425, #95040, #21177 ) ;
#79276 = CARTESIAN_POINT ( 'NONE',  ( 90.08848753752288019, -30.00000000000005684, -9.081672415796756326 ) ) ;
#79277 = CARTESIAN_POINT ( 'NONE',  ( -55.31183857750818333, -60.00000000000000000, 93.46795725556545165 ) ) ;
#79278 = EDGE_CURVE ( 'NONE', #34518, #866, #65550, .T. ) ;
#79279 = CARTESIAN_POINT ( 'NONE',  ( -56.58626023515411418, -39.49787623006356796, 63.80283036987835743 ) ) ;
#79280 = ORIENTED_EDGE ( 'NONE', *, *, #28581, .F. ) ;
#79281 = CARTESIAN_POINT ( 'NONE',  ( 6.321708934325914520, 15.64391652793080034, -3.012444762083619221 ) ) ;
#79282 = EDGE_LOOP ( 'NONE', ( #16829, #26970, #67768, #98736 ) ) ;
#79283 = CARTESIAN_POINT ( 'NONE',  ( -98.89625630335217465, -37.76835372157881210, 191.9674801915058140 ) ) ;
#79284 = CARTESIAN_POINT ( 'NONE',  ( -30.90097930193297415, 13.60840423680624589, -41.14831600716862425 ) ) ;
#79285 = ORIENTED_EDGE ( 'NONE', *, *, #79603, .F. ) ;
#79286 = CARTESIAN_POINT ( 'NONE',  ( 19.46591973412748189, 49.98735554868721920, 60.46518678595987950 ) ) ;
#79287 = SURFACE_STYLE_USAGE ( .BOTH. , #85818 ) ;
#79288 = FACE_OUTER_BOUND ( 'NONE', #38918, .T. ) ;
#79289 = CARTESIAN_POINT ( 'NONE',  ( 6.249999999999998224, -9.237604307034018802, 3.355146209984123968E-17 ) ) ;
#79290 =( NAMED_UNIT ( * ) PLANE_ANGLE_UNIT ( ) SI_UNIT ( $, .RADIAN. ) );
#79291 = CARTESIAN_POINT ( 'NONE',  ( 7.618844049274129837, -81.82764101070539198, 2.450177051822847840 ) ) ;
#79292 = CARTESIAN_POINT ( 'NONE',  ( 65.07902261671387123, -29.99999999999999645, 80.45956481633361079 ) ) ;
#79293 = DIRECTION ( 'NONE',  ( 0.000000000000000000, 0.000000000000000000, 1.000000000000000000 ) ) ;
#79294 = CARTESIAN_POINT ( 'NONE',  ( 25.11650669486618881, 4.000000000000003553, 4.898587196589414801E-16 ) ) ;
#79295 = CARTESIAN_POINT ( 'NONE',  ( -32.82691535583477815, 485.1045372766794799, 1.724905475514949771 ) ) ;
#79296 = UNCERTAINTY_MEASURE_WITH_UNIT (LENGTH_MEASURE( 1.000000000000000082E-05 ), #58061, 'distance_accuracy_value', 'NONE');
#79297 = CARTESIAN_POINT ( 'NONE',  ( -27.94118946956361427, -39.48418884341392499, 32.48209851497355061 ) ) ;
#79298 = AXIS2_PLACEMENT_3D ( 'NONE', #33551, #50752, #65897 ) ;
#79299 = ORIENTED_EDGE ( 'NONE', *, *, #61966, .F. ) ;
#79300 = ORIENTED_EDGE ( 'NONE', *, *, #80792, .T. ) ;
#79301 = CARTESIAN_POINT ( 'NONE',  ( 48.73357450832351390, -36.05786625502788212, 47.64037412505590652 ) ) ;
#79302 = DIRECTION ( 'NONE',  ( 1.000000000000000000, 0.000000000000000000, 0.000000000000000000 ) ) ;
#79303 = CARTESIAN_POINT ( 'NONE',  ( -6.925232610679096901, 16.86791138880112584, -1.053462737155420381 ) ) ;
#79304 = CARTESIAN_POINT ( 'NONE',  ( -110.9857816620232001, -38.35624345773422306, 171.1830732495621135 ) ) ;
#79305 = VERTEX_POINT ( 'NONE', #63201 ) ;
#79306 = CARTESIAN_POINT ( 'NONE',  ( 91.26056446089212670, -38.40160960025664849, -10.77111187304667617 ) ) ;
#79307 = CARTESIAN_POINT ( 'NONE',  ( 11.79976288999368528, 6.746418028092196373, -9.068817350359527296 ) ) ;
#79308 = CARTESIAN_POINT ( 'NONE',  ( 21.67692307692307452, 1.411358822780289120E-15, 0.000000000000000000 ) ) ;
#79309 = LINE ( 'NONE', #62613, #74064 ) ;
#79310 = SURFACE_SIDE_STYLE ('',( #14030 ) ) ;
#79311 = CARTESIAN_POINT ( 'NONE',  ( -31.35596682365697419, 438.0939828603714545, 22.55458131664454768 ) ) ;
#79312 = CARTESIAN_POINT ( 'NONE',  ( 5.656854249492378806, -17.37500000409676915, 5.656854249492381470 ) ) ;
#79313 = CARTESIAN_POINT ( 'NONE',  ( 5.000000000000000000, -60.71953810597794643, 12.61250543007074931 ) ) ;
#79314 = CARTESIAN_POINT ( 'NONE',  ( 95.49222815291510358, -60.00000000000000000, 202.5659028883012525 ) ) ;
#79315 = AXIS2_PLACEMENT_3D ( 'NONE', #1289, #67126, #33711 ) ;
#79316 = ADVANCED_FACE ( 'NONE', ( #71273 ), #100032, .T. ) ;
#79317 = DIRECTION ( 'NONE',  ( -0.000000000000000000, 1.000000000000000000, -0.000000000000000000 ) ) ;
#79318 = CONICAL_SURFACE ( 'NONE', #32840, 5.000000000000010658, 0.9599310885968697082 ) ;
#79319 = EDGE_LOOP ( 'NONE', ( #63632, #100737, #65737, #29790, #38801, #37291 ) ) ;
#79320 = EDGE_CURVE ( 'NONE', #83574, #9383, #71792, .T. ) ;
#79321 = CARTESIAN_POINT ( 'NONE',  ( -28.34102358861306570, 306.0549377924973555, -9.285773497043622982 ) ) ;
#79322 = CARTESIAN_POINT ( 'NONE',  ( 7.986468734911285949, 33.97313679723078650, 0.5341897780976184729 ) ) ;
#79323 = PRESENTATION_STYLE_ASSIGNMENT (( #103084 ) ) ;
#79324 = ORIENTED_EDGE ( 'NONE', *, *, #28654, .T. ) ;
#79325 = AXIS2_PLACEMENT_3D ( 'NONE', #60296, #44632, #91582 ) ;
#79327 = CARTESIAN_POINT ( 'NONE',  ( 5.221736196116609108, 7.022645827047127476, -27.48951043644760261 ) ) ;
#79326 = CARTESIAN_POINT ( 'NONE',  ( -110.4574577157169131, -38.35609589571208033, 182.8352804127118532 ) ) ;
#79328 = CARTESIAN_POINT ( 'NONE',  ( -2.499999999999998224, -8.000000000000000000, 14.79019945774904166 ) ) ;
#79329 = CARTESIAN_POINT ( 'NONE',  ( 31.42312417694817483, 414.9735925968759602, 24.35715672292620582 ) ) ;
#79330 = CARTESIAN_POINT ( 'NONE',  ( 7.188101187500001821, -14.93750000204838457, -2.977408999572650483 ) ) ;
#79331 = CARTESIAN_POINT ( 'NONE',  ( -8.737863884125482983, -4.999999999994546585, -90.03618980230058355 ) ) ;
#79332 = STYLED_ITEM ( 'NONE', ( #54502 ), #73129 ) ;
#79333 =( LENGTH_UNIT ( ) NAMED_UNIT ( * ) SI_UNIT ( .MILLI., .METRE. ) );
#79335 = VERTEX_POINT ( 'NONE', #14086 ) ;
#79334 = CARTESIAN_POINT ( 'NONE',  ( -33.49051768689264463, 464.3918346587479959, 8.532988796677324572 ) ) ;
#79336 = CARTESIAN_POINT ( 'NONE',  ( 83.68669337585905055, -35.98195733051991141, 170.8185300273958092 ) ) ;
#79337 = COLOUR_RGB ( '', 0.09019608, 0.27058824, 0.51372549) ;
#79338 = LINE ( 'NONE', #95528, #3269 ) ;
#79339 = CARTESIAN_POINT ( 'NONE',  ( 36.81804884527923605, 27.89004356318390876, 13.21991692395683771 ) ) ;
#79340 = ORIENTED_EDGE ( 'NONE', *, *, #100402, .F. ) ;
#79341 = CARTESIAN_POINT ( 'NONE',  ( 5.299999999999999822, 0.000000000000000000, 0.000000000000000000 ) ) ;
#79342 = CARTESIAN_POINT ( 'NONE',  ( 17.53698998713263890, 34.16838527846118723, 24.04404631791792823 ) ) ;
#79343 = FILL_AREA_STYLE_COLOUR ( '', #24926 ) ;
#79344 = DIRECTION ( 'NONE',  ( 0.000000000000000000, -1.000000000000000000, 0.000000000000000000 ) ) ;
#79345 = FILL_AREA_STYLE ('',( #101642 ) ) ;
#79346 = CYLINDRICAL_SURFACE ( 'NONE', #19927, 5.000000000000000888 ) ;
#79347 = ORIENTED_EDGE ( 'NONE', *, *, #70607, .T. ) ;
#79348 = CARTESIAN_POINT ( 'NONE',  ( -4.370066673350128106, -48.86972780289094942, 104.3945758574409837 ) ) ;
#79349 = PRESENTATION_LAYER_ASSIGNMENT (  '', '', ( #22498 ) ) ;
#79350 = CARTESIAN_POINT ( 'NONE',  ( -5.000000000000000000, -41.56343021050086861, 4.051462231091807809 ) ) ;
#79351 = DIRECTION ( 'NONE',  ( 0.000000000000000000, -1.000000000000000000, 0.000000000000000000 ) ) ;
#79353 = DIRECTION ( 'NONE',  ( -1.000000000000000000, -0.000000000000000000, -0.000000000000000000 ) ) ;
#79352 = DIRECTION ( 'NONE',  ( -0.02699252395738975518, 0.001721171576548164101, -0.9996341536876447442 ) ) ;
#79354 = EDGE_CURVE ( 'NONE', #43945, #23419, #46992, .T. ) ;
#79355 = VECTOR ( 'NONE', #19943, 999.9999999999998863 ) ;
#79356 = CARTESIAN_POINT ( 'NONE',  ( -1.320432766682874540E-15, -19.53125000204838457, 7.188101187500000044 ) ) ;
#79357 = CARTESIAN_POINT ( 'NONE',  ( 46.00000000000000000, 438.3878896346935790, 16.22878885428537998 ) ) ;
#79358 = DIRECTION ( 'NONE',  ( 0.000000000000000000, 1.000000000000000000, 0.000000000000000000 ) ) ;
#79359 = EDGE_LOOP ( 'NONE', ( #29461, #53906, #46246, #60662 ) ) ;
#79360 = CARTESIAN_POINT ( 'NONE',  ( 45.36923076923077502, 4.172000000000003261, 5.109226446042759579E-16 ) ) ;
#79361 = CARTESIAN_POINT ( 'NONE',  ( -1.797870618176258484, 41.33266196706050977, -58.72278032362692102 ) ) ;
#79362 = CARTESIAN_POINT ( 'NONE',  ( -8.066622878819057263, 44.48464632161675780, 0.000000000000000000 ) ) ;
#79363 = EDGE_CURVE ( 'NONE', #38992, #54340, #75934, .T. ) ;
#79364 = CARTESIAN_POINT ( 'NONE',  ( -7.500000000000003553, -2.999999999999999112, -68.91429205785459544 ) ) ;
#79365 = CARTESIAN_POINT ( 'NONE',  ( 23.86650669486618881, 1.474610560812782335E-15, 0.000000000000000000 ) ) ;
#79366 = VECTOR ( 'NONE', #12829, 1000.000000000000114 ) ;
#79367 = ORIENTED_EDGE ( 'NONE', *, *, #30121, .T. ) ;
#79368 = CARTESIAN_POINT ( 'NONE',  ( 29.83349330513380693, 1.593028355512270962E-15, 0.000000000000000000 ) ) ;
#79369 = CIRCLE ( 'NONE', #103482, 2.000000000000001776 ) ;
#79370 = CARTESIAN_POINT ( 'NONE',  ( 0.000000000000000000, 0.000000000000000000, -0.01270000000000090501 ) ) ;
#79371 = ORIENTED_EDGE ( 'NONE', *, *, #32936, .T. ) ;
#79372 = FACE_OUTER_BOUND ( 'NONE', #41350, .T. ) ;
#79373 = CARTESIAN_POINT ( 'NONE',  ( -1.468752096361644721, -0.02845455281367775119, 101.6458968146023096 ) ) ;
#79374 =( LENGTH_UNIT ( ) NAMED_UNIT ( * ) SI_UNIT ( .MILLI., .METRE. ) );
#79375 = DIRECTION ( 'NONE',  ( -0.000000000000000000, 1.000000000000000000, 0.000000000000000000 ) ) ;
#79376 = CARTESIAN_POINT ( 'NONE',  ( -110.2080847442849176, -59.99999999999998579, 145.1285909512942283 ) ) ;
#79377 =( NAMED_UNIT ( * ) PLANE_ANGLE_UNIT ( ) SI_UNIT ( $, .RADIAN. ) );
#79378 = CARTESIAN_POINT ( 'NONE',  ( 0.4969600502617488313, -8.860760056385739603, -0.6527133886630315240 ) ) ;
#79379 = CARTESIAN_POINT ( 'NONE',  ( 43.74985542820358830, 435.5770091380369422, 16.96136490515564788 ) ) ;
#79380 =( LENGTH_UNIT ( ) NAMED_UNIT ( * ) SI_UNIT ( .MILLI., .METRE. ) );
#79381 = EDGE_CURVE ( 'NONE', #5588, #53891, #6525, .T. ) ;
#79382 = CARTESIAN_POINT ( 'NONE',  ( -86.39811128889826364, -17.86889493908928017, 174.6576044378396944 ) ) ;
#79383 = CARTESIAN_POINT ( 'NONE',  ( 34.57001659430475371, 42.66264814753424872, -62.97408465421569446 ) ) ;
#79384 = AXIS2_PLACEMENT_3D ( 'NONE', #23424, #45569, #78443 ) ;
#79385 = AXIS2_PLACEMENT_3D ( 'NONE', #51192, #17797, #106778 ) ;
#79386 = EDGE_LOOP ( 'NONE', ( #6063, #19429, #10441, #77543 ) ) ;
#79387 = CARTESIAN_POINT ( 'NONE',  ( 5.500000000000641265, 42.00000000000000000, -59.88032989331720302 ) ) ;
#79388 = ADVANCED_FACE ( 'NONE', ( #97136 ), #89060, .F. ) ;
#79389 = CARTESIAN_POINT ( 'NONE',  ( 5.725989721596477011, -68.57677111256458602, 1.809923354557184894 ) ) ;
#79390 = CARTESIAN_POINT ( 'NONE',  ( -84.98226205003312828, -52.70557095620105770, 17.49892321904152226 ) ) ;
#79391 = TOROIDAL_SURFACE ( 'NONE', #138, 10.00000000000000000, 5.000000000000000000 ) ;
#79392 = CARTESIAN_POINT ( 'NONE',  ( 84.73333333333332007, 1.023464760207051730E-14, 0.000000000000000000 ) ) ;
#79393 = DIRECTION ( 'NONE',  ( 0.000000000000000000, 1.000000000000000000, 0.000000000000000000 ) ) ;
#79394 = CARTESIAN_POINT ( 'NONE',  ( 8.224453817191152538, 115.5406540063856085, -5.000000000001228351 ) ) ;
#79395 = DIRECTION ( 'NONE',  ( 0.000000000000000000, -1.000000000000000000, 0.000000000000000000 ) ) ;
#79396 = CARTESIAN_POINT ( 'NONE',  ( 29.83308852632731245, 41.99999999995888089, 51.76085035125569789 ) ) ;
#79397 = EDGE_CURVE ( 'NONE', #14406, #71627, #25414, .T. ) ;
#79398 = CARTESIAN_POINT ( 'NONE',  ( 78.18398495971976558, -30.00000000000001421, 185.0784753857526539 ) ) ;
#79399 = AXIS2_PLACEMENT_3D ( 'NONE', #19962, #29126, #85734 ) ;
#79400 = CARTESIAN_POINT ( 'NONE',  ( -107.0562774193554816, -30.00000000000000355, 141.2195909136805767 ) ) ;
#79401 = CARTESIAN_POINT ( 'NONE',  ( -65.12971609318923072, -22.10221659701648633, 77.59119750484730105 ) ) ;
#79402 = ORIENTED_EDGE ( 'NONE', *, *, #61643, .F. ) ;
#79403 = CARTESIAN_POINT ( 'NONE',  ( -65.06413854203213987, 39.42447728981473176, 0.8157412600678713988 ) ) ;
#79404 = CARTESIAN_POINT ( 'NONE',  ( 101.9590430895730861, -60.00000000001238476, 203.7674679764209031 ) ) ;
#79405 = EDGE_CURVE ( 'NONE', #30305, #87682, #67327, .T. ) ;
#79406 = VERTEX_POINT ( 'NONE', #1612 ) ;
#79407 = FACE_OUTER_BOUND ( 'NONE', #105676, .T. ) ;
#79408 = CARTESIAN_POINT ( 'NONE',  ( 5.082755093536324154, -16.71875000204838813, 5.082755093536326818 ) ) ;
#79409 = CARTESIAN_POINT ( 'NONE',  ( 32.84237740334681632, 485.2251842821273158, 5.746442123022902138 ) ) ;
#79410 = EDGE_LOOP ( 'NONE', ( #26038, #77339, #88385, #44522, #106347, #7397 ) ) ;
#79411 = PRODUCT ( '11. Strainer', '11. Strainer', '', ( #81586 ) ) ;
#79412 = CARTESIAN_POINT ( 'NONE',  ( 35.11650669486618170, 1.474610560812782335E-15, 0.000000000000000000 ) ) ;
#79413 = EDGE_LOOP ( 'NONE', ( #63633, #12187, #43785, #92943, #23249, #34912 ) ) ;
#79414 = CARTESIAN_POINT ( 'NONE',  ( -43.03185303983481447, 485.3613526602391062, 6.073233449168579767 ) ) ;
#79415 = FACE_OUTER_BOUND ( 'NONE', #28721, .T. ) ;
#79416 = CARTESIAN_POINT ( 'NONE',  ( -91.87920463863368070, -59.99999999999998579, 9.409623471143431672 ) ) ;
#79417 = CARTESIAN_POINT ( 'NONE',  ( -5.724587470723463412E-14, -15.58845726811991561, -1.205771365940065953 ) ) ;
#79418 = CARTESIAN_POINT ( 'NONE',  ( -5.082755093536325042, -30.96875000204838813, -5.082755093536325930 ) ) ;
#79419 = FACE_OUTER_BOUND ( 'NONE', #40435, .T. ) ;
#79420 = CARTESIAN_POINT ( 'NONE',  ( 7.996668422916345165, 49.99999999999455014, -91.14546720080639375 ) ) ;
#79421 = CARTESIAN_POINT ( 'NONE',  ( -46.00000000000000000, 438.4646224975039672, 9.895601460523739235 ) ) ;
#79422 = CARTESIAN_POINT ( 'NONE',  ( -43.59756234217317683, 434.3244621007142996, 14.55946156040369921 ) ) ;
#79423 = CARTESIAN_POINT ( 'NONE',  ( 102.8042200330476277, -59.99999999999999289, 193.0926654062890861 ) ) ;
#79424 = VECTOR ( 'NONE', #49934, 1000.000000000000000 ) ;
#79425 = ORIENTED_EDGE ( 'NONE', *, *, #10358, .F. ) ;
#79426 = DIRECTION ( 'NONE',  ( 0.000000000000000000, 1.000000000000000000, 1.224646799147353207E-16 ) ) ;
#79427 = SURFACE_STYLE_USAGE ( .BOTH. , #14671 ) ;
#79428 = CARTESIAN_POINT ( 'NONE',  ( 36.95859885022851898, -60.27851612577346430, 40.61549778638487851 ) ) ;
#79429 = AXIS2_PLACEMENT_3D ( 'NONE', #48224, #97847, #73559 ) ;
#79430 = CARTESIAN_POINT ( 'NONE',  ( -2.910977163135976653, -8.673617379884035472E-16, -22.23822744035697241 ) ) ;
#79431 = VERTEX_POINT ( 'NONE', #2565 ) ;
#79432 = DIRECTION ( 'NONE',  ( -0.000000000000000000, 0.8660254037844382635, 0.5000000000000006661 ) ) ;
#79433 = AXIS2_PLACEMENT_3D ( 'NONE', #28427, #3052, #45130 ) ;
#79434 = EDGE_LOOP ( 'NONE', ( #29054, #34261, #53818 ) ) ;
#79436 = CARTESIAN_POINT ( 'NONE',  ( 45.40507512465600115, 439.2794387026467575, 6.273370203490043373 ) ) ;
#79435 = CARTESIAN_POINT ( 'NONE',  ( 8.901296169213878784, -5.000000000000000000, -17.06178707270185058 ) ) ;
#79437 = CARTESIAN_POINT ( 'NONE',  ( 43.00000000000000000, 500.0000000000002274, 0.000000000000000000 ) ) ;
#79438 = CARTESIAN_POINT ( 'NONE',  ( 12.33349330513380693, -4.000000000000000000, 4.898587196589415787E-16 ) ) ;
#79439 = CARTESIAN_POINT ( 'NONE',  ( -7.500000000055414340, -4.999999999944586548, -36.97043916959988508 ) ) ;
#79440 = CARTESIAN_POINT ( 'NONE',  ( -42.37751841893198446, 435.9440627571723326, 7.948837343527305421 ) ) ;
#79441 = CARTESIAN_POINT ( 'NONE',  ( 4.496882872040834478, -85.53788665489625487, 3.972797206970398509 ) ) ;
#79442 = CARTESIAN_POINT ( 'NONE',  ( -1.000000000000000444, -50.00000000000000000, 44.97220075561142494 ) ) ;
#79443 = CARTESIAN_POINT ( 'NONE',  ( 97.58552689470138830, -59.99999999999999289, 66.34462866920253532 ) ) ;
#79444 = CARTESIAN_POINT ( 'NONE',  ( 27.26371139070421279, 34.70268990229791228, -7.556984339686200869 ) ) ;
#79445 = CARTESIAN_POINT ( 'NONE',  ( -43.48220711419978812, 485.4752262574868951, 4.033700225028757025 ) ) ;
#79446 = FACE_BOUND ( 'NONE', #19893, .T. ) ;
#79447 = CARTESIAN_POINT ( 'NONE',  ( -11.43540210466514218, 13.32389838193370579, -9.996488892513244906 ) ) ;
#79448 = ORIENTED_EDGE ( 'NONE', *, *, #94369, .F. ) ;
#79449 = EDGE_CURVE ( 'NONE', #23052, #2708, #34639, .T. ) ;
#79450 = AXIS2_PLACEMENT_3D ( 'NONE', #61286, #54755, #53711 ) ;
#79451 = CARTESIAN_POINT ( 'NONE',  ( -90.00142789408454291, -29.99999999997103828, -9.692338486264096886 ) ) ;
#79452 = ORIENTED_EDGE ( 'NONE', *, *, #90889, .T. ) ;
#79453 = PRESENTATION_STYLE_ASSIGNMENT (( #70315 ) ) ;
#79454 = DIRECTION ( 'NONE',  ( 0.000000000000000000, -1.000000000000000000, 0.000000000000000000 ) ) ;
#79455 = CARTESIAN_POINT ( 'NONE',  ( 4.561000490385944239, 8.778822500554452901, 5.000000000000000000 ) ) ;
#79456 = CARTESIAN_POINT ( 'NONE',  ( 15.76884112491604562, 22.48937974161447073, -2.489079047138151424 ) ) ;
#79457 = CARTESIAN_POINT ( 'NONE',  ( -7.188101187500000044, -33.78125000204838813, -8.802885111219163269E-16 ) ) ;
#79459 = EDGE_CURVE ( 'NONE', #7599, #14445, #25966, .T. ) ;
#79458 = DIRECTION ( 'NONE',  ( 0.1269898409407502204, -0.9919025243773941236, 0.001721171576547747550 ) ) ;
#79460 = PLANE ( 'NONE',  #43668 ) ;
#79461 = LINE ( 'NONE', #29364, #13263 ) ;
#79462 = EDGE_LOOP ( 'NONE', ( #71266, #76886, #22207, #15600, #78878, #35269 ) ) ;
#79464 = EDGE_LOOP ( 'NONE', ( #18486, #59788, #51901, #11012 ) ) ;
#79463 = DIRECTION ( 'NONE',  ( 0.000000000000000000, 1.000000000000000000, 0.000000000000000000 ) ) ;
#79465 = CARTESIAN_POINT ( 'NONE',  ( 77.19329776267699117, -60.30815103425013035, 150.0154352435695557 ) ) ;
#79466 = VECTOR ( 'NONE', #105766, 1000.000000000000000 ) ;
#79467 = CARTESIAN_POINT ( 'NONE',  ( 14.68864207889602724, 1.585199049501273105, -3.034365436886341971 ) ) ;
#79468 = EDGE_LOOP ( 'NONE', ( #104864, #105019, #76455, #34895 ) ) ;
#79469 = AXIS2_PLACEMENT_3D ( 'NONE', #61864, #12213, #34938 ) ;
#79470 = CARTESIAN_POINT ( 'NONE',  ( -12.50000000000000533, 34.72467956601219186, -53.96055213376253334 ) ) ;
#79471 = CARTESIAN_POINT ( 'NONE',  ( 8.099999999999999645, -7.505553499465148271, 0.000000000000000000 ) ) ;
#79472 = CARTESIAN_POINT ( 'NONE',  ( -2.977408999572654480, -21.12500000204838813, 7.188101187499999156 ) ) ;
#79473 = AXIS2_PLACEMENT_3D ( 'NONE', #103216, #39016, #30406 ) ;
#79474 = CARTESIAN_POINT ( 'NONE',  ( 10.28624191511840458, 45.38549880562042205, 15.40779740156149202 ) ) ;
#79475 = CARTESIAN_POINT ( 'NONE',  ( 19.22276103763711319, 302.7169779577087070, 9.908341515297090396 ) ) ;
#79476 = EDGE_CURVE ( 'NONE', #17856, #15530, #48358, .T. ) ;
#79477 = VERTEX_POINT ( 'NONE', #8654 ) ;
#79478 = VECTOR ( 'NONE', #29489, 1000.000000000000000 ) ;
#79479 = FACE_OUTER_BOUND ( 'NONE', #103047, .T. ) ;
#79481 = CARTESIAN_POINT ( 'NONE',  ( -4.472135954999581386, -10.13579204946556089, 4.000000000000001776 ) ) ;
#79480 = PRESENTATION_LAYER_ASSIGNMENT (  '', '', ( #45016 ) ) ;
#79482 = CARTESIAN_POINT ( 'NONE',  ( 7.311443158282724397, 40.96482056676212125, -58.73188698012794617 ) ) ;
#79483 = AXIS2_PLACEMENT_3D ( 'NONE', #104021, #30163, #63049 ) ;
#79484 = CARTESIAN_POINT ( 'NONE',  ( 0.000000000000000000, 0.000000000000000000, -0.5776712190230098853 ) ) ;
#79485 = EDGE_CURVE ( 'NONE', #52531, #81845, #57726, .T. ) ;
#79486 = CARTESIAN_POINT ( 'NONE',  ( 8.000000000000000000, -11.18750000409677092, 0.000000000000000000 ) ) ;
#79487 = CARTESIAN_POINT ( 'NONE',  ( -1.816965407639463237, -12.60722515422099121, 32.17792230897330796 ) ) ;
#79488 = CARTESIAN_POINT ( 'NONE',  ( -36.43961512855968010, 26.07474805434645049, 11.65918951012361582 ) ) ;
#79489 = CARTESIAN_POINT ( 'NONE',  ( 42.48192783572675779, 485.4100919824720677, -3.499593777788684523 ) ) ;
#79490 = CARTESIAN_POINT ( 'NONE',  ( 7.500000000000000000, -6.192646671729328922, -14.54134196042664229 ) ) ;
#79491 =( NAMED_UNIT ( * ) PLANE_ANGLE_UNIT ( ) SI_UNIT ( $, .RADIAN. ) );
#79492 = APPLICATION_PROTOCOL_DEFINITION ( 'draft international standard', 'automotive_design', 1998, #36304 ) ;
#79493 = CARTESIAN_POINT ( 'NONE',  ( -11.55614992315287637, -8.838057010478776121, 19.09125476800991450 ) ) ;
#79494 = EDGE_LOOP ( 'NONE', ( #97631, #83500, #98013 ) ) ;
#79495 = CARTESIAN_POINT ( 'NONE',  ( 11.30425253726989787, 43.19231108733225710, 14.90234394683685082 ) ) ;
#79496 = CARTESIAN_POINT ( 'NONE',  ( -3.572352985695287586, 15.21714514899109894, 9.341953373613243627 ) ) ;
#79497 = CARTESIAN_POINT ( 'NONE',  ( -4.000000000000000000, 17.58303990196341715, -5.744562646538042827 ) ) ;
#79498 = CARTESIAN_POINT ( 'NONE',  ( -41.74004629104351238, -25.39692756236595272, -29.94283237742294901 ) ) ;
#79499 = CARTESIAN_POINT ( 'NONE',  ( -84.24535704145247905, -30.00000000000000355, 163.2126184220585685 ) ) ;
#79500 = EDGE_CURVE ( 'NONE', #65882, #100006, #51902, .T. ) ;
#79501 = DIRECTION ( 'NONE',  ( 0.000000000000000000, 1.000000000000000000, 0.000000000000000000 ) ) ;
#79502 = VERTEX_POINT ( 'NONE', #83603 ) ;
#79503 = CARTESIAN_POINT ( 'NONE',  ( 5.086432848262074522E-16, 0.3912769055735421664, -8.000000000000001776 ) ) ;
#79504 = CARTESIAN_POINT ( 'NONE',  ( 106.6623973988415486, -57.65263066412270376, 200.3796240358551586 ) ) ;
#79505 = CIRCLE ( 'NONE', #77752, 4.000000000000003553 ) ;
#79506 = CARTESIAN_POINT ( 'NONE',  ( 68.19648835047706825, -21.77029766163251523, -20.22171886456733247 ) ) ;
#79507 = DIRECTION ( 'NONE',  ( -0.000000000000000000, 1.000000000000000000, 1.224646799147353207E-16 ) ) ;
#79508 = CIRCLE ( 'NONE', #81187, 4.000000000000000888 ) ;
#79509 = CARTESIAN_POINT ( 'NONE',  ( -16.12871211736532118, 21.28428926969061408, 2.982820907284539746 ) ) ;
#79510 = CARTESIAN_POINT ( 'NONE',  ( 63.03617022303986772, 40.83906611471739012, -16.93907820431003586 ) ) ;
#79511 = CARTESIAN_POINT ( 'NONE',  ( -74.13159945279534213, -59.99999999999999289, 173.5497442450795802 ) ) ;
#79512 = PRESENTATION_STYLE_ASSIGNMENT (( #46615 ) ) ;
#79513 = LINE ( 'NONE', #20811, #25285 ) ;
#79514 = CARTESIAN_POINT ( 'NONE',  ( -63.03617022294436367, 49.99999999995993250, -16.93907820454377244 ) ) ;
#79515 = CARTESIAN_POINT ( 'NONE',  ( -86.00256373658280040, -31.97000255027745297, 183.8091090326766732 ) ) ;
#79516 = ORIENTED_EDGE ( 'NONE', *, *, #36388, .T. ) ;
#79517 = CARTESIAN_POINT ( 'NONE',  ( 31.90221457330017785, 317.1353150898008266, -7.038899609007000180 ) ) ;
#79518 = DIRECTION ( 'NONE',  ( 0.4753313241820203983, -0.2469313775204406425, 0.8444436198155712558 ) ) ;
#79519 = EDGE_CURVE ( 'NONE', #79761, #20102, #11017, .T. ) ;
#79520 = CARTESIAN_POINT ( 'NONE',  ( -27.94623540071386003, 307.0441435012233455, -9.286149966824948976 ) ) ;
#79521 = CARTESIAN_POINT ( 'NONE',  ( -83.19058701941813183, -45.25941601734338349, -14.11641135335829844 ) ) ;
#79522 = LINE ( 'NONE', #29942, #64889 ) ;
#79523 = DIRECTION ( 'NONE',  ( 0.6505632072693968704, 0.6639782930160459395, -0.3686466326319198794 ) ) ;
#79524 = EDGE_LOOP ( 'NONE', ( #12780, #101182, #74664, #27791, #83305 ) ) ;
#79525 = DIRECTION ( 'NONE',  ( 0.000000000000000000, -1.000000000000000000, 0.000000000000000000 ) ) ;
#79526 = CARTESIAN_POINT ( 'NONE',  ( 11.27810499350236384, 20.00336526192103648, 8.427062764154296559 ) ) ;
#79527 = EDGE_CURVE ( 'NONE', #41900, #59127, #44476, .T. ) ;
#79528 = CARTESIAN_POINT ( 'NONE',  ( -25.22241582816893413, -4.285714285714285587, 3.301606509427073455 ) ) ;
#79529 = DIRECTION ( 'NONE',  ( -0.5735764363510494901, -0.8191520442889894671, 0.000000000000000000 ) ) ;
#79530 = CARTESIAN_POINT ( 'NONE',  ( 87.61417445234833679, -14.21045842199449716, -10.69449287335903342 ) ) ;
#79531 = CARTESIAN_POINT ( 'NONE',  ( -78.86360919887746945, -49.90773682881172846, 149.9494586803164680 ) ) ;
#79532 = ORIENTED_EDGE ( 'NONE', *, *, #71304, .F. ) ;
#79533 = CARTESIAN_POINT ( 'NONE',  ( 28.84074934710125859, -30.00000000000002842, 39.52209614246421410 ) ) ;
#79534 = CARTESIAN_POINT ( 'NONE',  ( 4.521127550501233827, 250.6761024052766516, 3.944701057164349933 ) ) ;
#79535 = CARTESIAN_POINT ( 'NONE',  ( 100.6487164681503970, -57.62854788423276631, 203.7452194625044228 ) ) ;
#79536 = SURFACE_SIDE_STYLE ('',( #94135 ) ) ;
#79537 = CARTESIAN_POINT ( 'NONE',  ( 40.66390020119442283, 311.9487095737082427, -5.937893087732901698 ) ) ;
#79538 = DIRECTION ( 'NONE',  ( 0.000000000000000000, 0.000000000000000000, -1.000000000000000000 ) ) ;
#79539 = ORIENTED_EDGE ( 'NONE', *, *, #8243, .T. ) ;
#79540 = CARTESIAN_POINT ( 'NONE',  ( 7.500000000000000000, 3.988838049906436201, -0.8529248949437627791 ) ) ;
#79541 = STYLED_ITEM ( 'NONE', ( #39343 ), #8466 ) ;
#79542 = EDGE_CURVE ( 'NONE', #48048, #92227, #17306, .T. ) ;
#79543 = CARTESIAN_POINT ( 'NONE',  ( 0.000000000000000000, 0.000000000000000000, 0.000000000000000000 ) ) ;
#79545 = CARTESIAN_POINT ( 'NONE',  ( -102.3387829128316184, -60.15503256459196280, 129.8700687430441292 ) ) ;
#79544 = CARTESIAN_POINT ( 'NONE',  ( -15.52419239919893101, 37.09839268680908475, 22.76866006007168863 ) ) ;
#79546 = CARTESIAN_POINT ( 'NONE',  ( -5.082755093536326818, -22.71875000204838457, 5.082755093536325042 ) ) ;
#79547 = CARTESIAN_POINT ( 'NONE',  ( 8.000000000000000000, -20.09375000409677270, -3.313708498984761164 ) ) ;
#79548 = STYLED_ITEM ( 'NONE', ( #76540 ), #51156 ) ;
#79549 = CARTESIAN_POINT ( 'NONE',  ( 0.000000000000000000, 0.000000000000000000, 0.000000000000000000 ) ) ;
#79550 = CARTESIAN_POINT ( 'NONE',  ( 6.645514545840788934, 41.91298724924220664, -59.84148600294046361 ) ) ;
#79551 = CARTESIAN_POINT ( 'NONE',  ( 26.12466916459994337, 36.99826655557325950, 9.598780014887051237 ) ) ;
#79552 = CARTESIAN_POINT ( 'NONE',  ( 17.50000000000002842, 50.00000000000000000, -500000.0000000000582 ) ) ;
#79553 = CARTESIAN_POINT ( 'NONE',  ( -23.84332598391540614, 27.93368204320126935, -30.86206213703136214 ) ) ;
#79554 = ORIENTED_EDGE ( 'NONE', *, *, #83951, .F. ) ;
#79555 = CARTESIAN_POINT ( 'NONE',  ( 31.08349330513380337, 1.593028355512270567E-15, 0.000000000000000000 ) ) ;
#79556 = COLOUR_RGB ( '', 0.31764706, 0.68627451, 0.89019608) ;
#79558 = CARTESIAN_POINT ( 'NONE',  ( 25.12474446974736608, -46.43382705368295404, 32.95440499086974739 ) ) ;
#79557 = CARTESIAN_POINT ( 'NONE',  ( -52.56680815376439853, -59.99999999999999289, 85.36473592189453541 ) ) ;
#79559 = CARTESIAN_POINT ( 'NONE',  ( -24.45749910306381025, 25.45711128933222867, 31.59697626135422865 ) ) ;
#79560 = ORIENTED_EDGE ( 'NONE', *, *, #14677, .F. ) ;
#79561 = VECTOR ( 'NONE', #25120, 1000.000000000000000 ) ;
#79562 = UNCERTAINTY_MEASURE_WITH_UNIT (LENGTH_MEASURE( 1.000000000000000082E-05 ), #51343, 'distance_accuracy_value', 'NONE');
#79563 = ORIENTED_EDGE ( 'NONE', *, *, #84386, .T. ) ;
#79564 = CARTESIAN_POINT ( 'NONE',  ( -24.41571844174604067, -4.285714285714295357, 6.539732759932823214 ) ) ;
#79565 = CARTESIAN_POINT ( 'NONE',  ( 7.461258573462377974, 40.57432690845221401, -59.19360968028617975 ) ) ;
#79566 = CARTESIAN_POINT ( 'NONE',  ( -0.3336719003891429058, 51.28288261117670288, -10.20757999058579379 ) ) ;
#79567 = CARTESIAN_POINT ( 'NONE',  ( 12.53023694619758466, 1.820302489804639157, 14.89061371906986864 ) ) ;
#79568 = SURFACE_STYLE_USAGE ( .BOTH. , #64465 ) ;
#79569 = ORIENTED_EDGE ( 'NONE', *, *, #97741, .F. ) ;
#79570 = CARTESIAN_POINT ( 'NONE',  ( 65.64504852076265706, -60.00000000000000711, -34.00365457729831320 ) ) ;
#79571 = LINE ( 'NONE', #5684, #58427 ) ;
#79572 = CARTESIAN_POINT ( 'NONE',  ( -10.03820104914963984, 14.09414544201339758, -10.49954271116794580 ) ) ;
#79573 = CARTESIAN_POINT ( 'NONE',  ( 62.33904886068935980, 4.000000000000013323, 0.000000000000000000 ) ) ;
#79574 = CARTESIAN_POINT ( 'NONE',  ( 81.59412642177187536, -30.00000000000000000, -6.882760467535725013 ) ) ;
#79575 = DIRECTION ( 'NONE',  ( -0.7071067811865390240, 0.000000000000000000, 0.7071067811865561215 ) ) ;
#79576 = ORIENTED_EDGE ( 'NONE', *, *, #4254, .T. ) ;
#79577 = EDGE_CURVE ( 'NONE', #47740, #102923, #41518, .T. ) ;
#79578 = B_SPLINE_CURVE_WITH_KNOTS ( 'NONE', 3,
 ( #44266, #59394, #25999, #27052, #51805, #75554, #68550, #34074, #92255, #43721, #34609, #92801, #99277, #99826, #58860, #35131, #18410, #84716 ),
 .UNSPECIFIED., .F., .F.,
 ( 4, 2, 2, 2, 2, 2, 2, 2, 4 ),
 ( 0.000000000000000000, 0.0005503281002746097895, 0.001100656200549219579, 0.001650984300823829260, 0.002201312401098439158, 0.002751640501373049056, 0.003301968601647658520, 0.003852296701922268418, 0.004402624802196878316 ),
 .UNSPECIFIED. ) ;
#79579 =( GEOMETRIC_REPRESENTATION_CONTEXT ( 3 ) GLOBAL_UNCERTAINTY_ASSIGNED_CONTEXT ( ( #67963 ) ) GLOBAL_UNIT_ASSIGNED_CONTEXT ( ( #23645, #19314, #60276 ) ) REPRESENTATION_CONTEXT ( 'NONE', 'WORKASPACE' ) );
#79580 = EDGE_LOOP ( 'NONE', ( #49540, #61982, #53074, #64389 ) ) ;
#79581 = VERTEX_POINT ( 'NONE', #92221 ) ;
#79582 = FACE_OUTER_BOUND ( 'NONE', #17703, .T. ) ;
#79583 = DIRECTION ( 'NONE',  ( -1.000000000000000000, -1.224606353822377258E-16, -0.000000000000000000 ) ) ;
#79584 = DIRECTION ( 'NONE',  ( 0.000000000000000000, 0.000000000000000000, -1.000000000000000000 ) ) ;
#79585 = CIRCLE ( 'NONE', #10655, 5.000000000000002665 ) ;
#79586 = DIRECTION ( 'NONE',  ( -0.5735764363510494901, -0.8191520442889894671, 0.000000000000000000 ) ) ;
#79587 = CARTESIAN_POINT ( 'NONE',  ( 91.09088295274877112, 1.030564683017419500E-14, 0.000000000000000000 ) ) ;
#79589 = EDGE_CURVE ( 'NONE', #4111, #54176, #90898, .T. ) ;
#79588 = CARTESIAN_POINT ( 'NONE',  ( 0.000000000000000000, 43.50000000000000711, 0.000000000000000000 ) ) ;
#79590 = ORIENTED_EDGE ( 'NONE', *, *, #43399, .T. ) ;
#79591 = CARTESIAN_POINT ( 'NONE',  ( 8.737863884120029567, 49.99999999999999289, -79.96381019768851672 ) ) ;
#79592 = VERTEX_POINT ( 'NONE', #69573 ) ;
#79593 = DIRECTION ( 'NONE',  ( -1.000000000000000000, -1.224606353822377258E-16, -0.000000000000000000 ) ) ;
#79594 = CARTESIAN_POINT ( 'NONE',  ( 45.89060600365420584, -38.31793543208539177, 59.54903041405342634 ) ) ;
#79595 = SURFACE_STYLE_FILL_AREA ( #6766 ) ;
#79596 = CARTESIAN_POINT ( 'NONE',  ( 19.34999999999999787, 3.309500000000003439, 0.000000000000000000 ) ) ;
#79597 = CARTESIAN_POINT ( 'NONE',  ( 63.51939168307682593, -25.58021191660321847, 74.89133063105313681 ) ) ;
#79598 = VERTEX_POINT ( 'NONE', #76045 ) ;
#79599 = CARTESIAN_POINT ( 'NONE',  ( 41.15051831715039299, 464.6037346866244775, 16.66306381442320372 ) ) ;
#79600 = DIRECTION ( 'NONE',  ( 0.000000000000000000, 0.000000000000000000, 1.000000000000000000 ) ) ;
#79601 = DIRECTION ( 'NONE',  ( -0.1659550938519105956, -0.9861333108787085910, 0.000000000000000000 ) ) ;
#79602 = CARTESIAN_POINT ( 'NONE',  ( -9.749599596588822692, 51.26841084474641974, 3.172565964336790056 ) ) ;
#79603 = EDGE_CURVE ( 'NONE', #104924, #48559, #58783, .T. ) ;
#79604 = EDGE_LOOP ( 'NONE', ( #89338, #14001 ) ) ;
#79605 =( NAMED_UNIT ( * ) PLANE_ANGLE_UNIT ( ) SI_UNIT ( $, .RADIAN. ) );
#79606 = CARTESIAN_POINT ( 'NONE',  ( 23.09999999999999432, -3.309499999999999886, 0.000000000000000000 ) ) ;
#79607 = DIRECTION ( 'NONE',  ( -0.000000000000000000, -0.000000000000000000, 1.000000000000000000 ) ) ;
#79608 = CARTESIAN_POINT ( 'NONE',  ( -1.469576158976823947E-15, -28.06250000409677270, 8.000000000000000000 ) ) ;
#79609 = CARTESIAN_POINT ( 'NONE',  ( 2.094395098902538610, -4.999999999999998224, -8.000000000000000000 ) ) ;
#79610 = CARTESIAN_POINT ( 'NONE',  ( 86.89624646361832561, -35.41998960442577982, 187.9270345319939395 ) ) ;
#79611 = CARTESIAN_POINT ( 'NONE',  ( -5.075741750048029743, -4.332638003024074536, -17.09621982684887698 ) ) ;
#79612 = CARTESIAN_POINT ( 'NONE',  ( -9.550648135838782693, 9.268430070245118557, 0.000000000000000000 ) ) ;
#79613 = B_SPLINE_CURVE_WITH_KNOTS ( 'NONE', 3,
 ( #45654, #28987, #38632, #39160, #63442, #103866, #86132, #4128, #30016, #61314 ),
 .UNSPECIFIED., .F., .F.,
 ( 4, 2, 2, 2, 4 ),
 ( 0.000000000000000000, 0.001993803085173303895, 0.003987606170346607790, 0.005981409255519911684, 0.007975212340693215579 ),
 .UNSPECIFIED. ) ;
#79614 = CIRCLE ( 'NONE', #70998, 4.000000000000001776 ) ;
#79615 =( NAMED_UNIT ( * ) SI_UNIT ( $, .STERADIAN. ) SOLID_ANGLE_UNIT ( ) );
#79616 = EDGE_LOOP ( 'NONE', ( #90137, #97512, #810, #89586, #62715 ) ) ;
#79617 = CARTESIAN_POINT ( 'NONE',  ( 13.80732344291479663, -50.82138033104836694, 24.67475631203899411 ) ) ;
#79618 = CARTESIAN_POINT ( 'NONE',  ( 0.1061556211655305393, 4.836380039389409191, -4.623144047065556705 ) ) ;
#79619 = CARTESIAN_POINT ( 'NONE',  ( 36.35123893432750464, -59.99999999999999289, 47.70089417776525664 ) ) ;
#79620 = CARTESIAN_POINT ( 'NONE',  ( -98.78384617981630811, -29.99999999999999645, 143.3060070716083203 ) ) ;
#79621 = CARTESIAN_POINT ( 'NONE',  ( -4.678819457397884740, 143.9212778189118467, 5.000000000000000000 ) ) ;
#79622 = MECHANICAL_DESIGN_GEOMETRIC_PRESENTATION_REPRESENTATION (  '', ( #22850 ), #19407 ) ;
#79623 = CARTESIAN_POINT ( 'NONE',  ( 52.81362779437819910, -57.67621448248372218, 84.99611232883394507 ) ) ;
#79625 = CARTESIAN_POINT ( 'NONE',  ( 43.34642793389308935, 464.8022470463094464, 10.25621957614987956 ) ) ;
#79624 = CARTESIAN_POINT ( 'NONE',  ( -0.6476328880971240487, 25.22743360806496682, -40.58242577266638307 ) ) ;
#79626 = CARTESIAN_POINT ( 'NONE',  ( -17.92908368763044891, 41.95109109384650736, -82.51357555118542564 ) ) ;
#79627 = B_SPLINE_CURVE_WITH_KNOTS ( 'NONE', 3,
 ( #21156, #38899, #30284, #5458, #86404, #62644, #22731, #38380, #79861, #103100, #88506, #12996, #96065, #105213, #45921, #37332, #78277, #4393, #6497, #96599, #12466, #45399, #22197, #55048, #87977, #72307, #78800, #54506, #21673, #14058, #70724, #71762, #4933, #30826 ),
 .UNSPECIFIED., .F., .F.,
 ( 4, 2, 2, 2, 2, 2, 2, 2, 2, 2, 2, 2, 2, 2, 2, 2, 4 ),
 ( 0.000000000000000000, 0.002098190355514029017, 0.004196380711028058035, 0.008392761422056110865, 0.01678552284411221826, 0.02517828426616832566, 0.03357104568822444346, 0.05035656853233669988, 0.06714209137644897019, 0.08392761422056123355, 0.1007131370646734969, 0.1091058984867296217, 0.1174986599087857603, 0.1258914213308418850, 0.1300878020418699821, 0.1321859923973840445, 0.1342841827528981069 ),
 .UNSPECIFIED. ) ;
#79628 = CARTESIAN_POINT ( 'NONE',  ( -19.17276608133135696, 49.99999999999999289, 60.35151560209396848 ) ) ;
#79629 = CARTESIAN_POINT ( 'NONE',  ( -9.403185743875129177, 15.24615751665902685, 3.409011323176729835 ) ) ;
#79630 = CARTESIAN_POINT ( 'NONE',  ( 43.84752573847596580, 486.0721194390229698, 5.282948175099586585 ) ) ;
#79631 = CARTESIAN_POINT ( 'NONE',  ( -17.49999999999998579, 50.79875088428568120, 63.37001662960430082 ) ) ;
#79632 = PRESENTATION_STYLE_ASSIGNMENT (( #69962 ) ) ;
#79633 = FACE_BOUND ( 'NONE', #18191, .T. ) ;
#79634 = CARTESIAN_POINT ( 'NONE',  ( -87.42610337103299400, -31.68231154847087794, 188.4209481024660420 ) ) ;
#79635 = ORIENTED_EDGE ( 'NONE', *, *, #59618, .T. ) ;
#79636 = CARTESIAN_POINT ( 'NONE',  ( 17.50000000000002842, 48.58944628578559133, 64.09148194233368656 ) ) ;
#79637 = DIRECTION ( 'NONE',  ( 0.000000000000000000, -1.000000000000000000, 0.000000000000000000 ) ) ;
#79638 = CARTESIAN_POINT ( 'NONE',  ( -11.12563101218981920, -22.06807209563270433, 27.59097960060775634 ) ) ;
#79639 = AXIS2_PLACEMENT_3D ( 'NONE', #91045, #50025, #106665 ) ;
#79641 = DIRECTION ( 'NONE',  ( -1.000000000000000000, -1.224606353822377258E-16, -0.000000000000000000 ) ) ;
#79640 = CARTESIAN_POINT ( 'NONE',  ( -86.47393794408476708, -60.00000000000003553, 2.142859354767555402 ) ) ;
#79642 = ADVANCED_FACE ( 'NONE', ( #2147 ), #20946, .T. ) ;
#79643 = ORIENTED_EDGE ( 'NONE', *, *, #32312, .F. ) ;
#79644 = DIRECTION ( 'NONE',  ( -1.000000000000000000, -1.224606353822377258E-16, -0.000000000000000000 ) ) ;
#79645 =( GEOMETRIC_REPRESENTATION_CONTEXT ( 3 ) GLOBAL_UNCERTAINTY_ASSIGNED_CONTEXT ( ( #80140 ) ) GLOBAL_UNIT_ASSIGNED_CONTEXT ( ( #103368, #12212, #13800 ) ) REPRESENTATION_CONTEXT ( 'NONE', 'WORKASPACE' ) );
#79646 = EDGE_CURVE ( 'NONE', #63451, #92028, #7089, .T. ) ;
#79647 = CARTESIAN_POINT ( 'NONE',  ( -1.469576158976823947E-15, -14.56250000409677092, 8.000000000000000000 ) ) ;
#79648 = CARTESIAN_POINT ( 'NONE',  ( -89.99999999999997158, -60.00000000000000000, 196.0238439516549818 ) ) ;
#79649 = AXIS2_PLACEMENT_3D ( 'NONE', #13626, #14681, #104234 ) ;
#79650 = EDGE_CURVE ( 'NONE', #84725, #57214, #22093, .T. ) ;
#79651 = CARTESIAN_POINT ( 'NONE',  ( 16.02800152098294717, 4.194749798097111793, -2.552193233489410407 ) ) ;
#79652 = CARTESIAN_POINT ( 'NONE',  ( 73.13425705143828282, -60.00000000000000000, 163.6887274309862619 ) ) ;
#79653 = CARTESIAN_POINT ( 'NONE',  ( -21.51569398614858031, 294.9107018935607130, -9.987480606144492512 ) ) ;
#79654 = ORIENTED_EDGE ( 'NONE', *, *, #94536, .F. ) ;
#79655 = FACE_OUTER_BOUND ( 'NONE', #82316, .T. ) ;
#79656 = CARTESIAN_POINT ( 'NONE',  ( -34.24139198049589794, 434.2621489448225134, 10.63631919729165887 ) ) ;
#79657 = EDGE_CURVE ( 'NONE', #55862, #7464, #3654, .T. ) ;
#79658 = AXIS2_PLACEMENT_3D ( 'NONE', #42840, #18596, #41774 ) ;
#79660 = DIRECTION ( 'NONE',  ( -1.000000000000000000, -1.224606353822377258E-16, -0.000000000000000000 ) ) ;
#79659 = CARTESIAN_POINT ( 'NONE',  ( 39.04758850296788353, -59.99999999999992184, 54.77506993285218329 ) ) ;
#79661 = CARTESIAN_POINT ( 'NONE',  ( 3.225573779814643771, 115.6473726989443520, -5.000000000000000000 ) ) ;
#79662 = CARTESIAN_POINT ( 'NONE',  ( -4.581218816254563286, -2.199133564524444306, 103.5404609598622301 ) ) ;
#79663 = EDGE_LOOP ( 'NONE', ( #96029, #61961, #28346, #16776, #36405 ) ) ;
#79664 = ADVANCED_FACE ( 'NONE', ( #97015 ), #54561, .T. ) ;
#79665 = ORIENTED_EDGE ( 'NONE', *, *, #52359, .T. ) ;
#79666 = CARTESIAN_POINT ( 'NONE',  ( -28.61750315445088333, 319.5788945160356320, 13.56838495107838760 ) ) ;
#79667 = ORIENTED_EDGE ( 'NONE', *, *, #14441, .T. ) ;
#79668 = DIRECTION ( 'NONE',  ( 0.000000000000000000, 0.000000000000000000, -1.000000000000000000 ) ) ;
#79669 = DIRECTION ( 'NONE',  ( 0.000000000000000000, -1.000000000000000000, 0.000000000000000000 ) ) ;
#79670 = CARTESIAN_POINT ( 'NONE',  ( 8.000000000000000000, -12.59375000409676915, -3.313708498984761164 ) ) ;
#79671 = EDGE_LOOP ( 'NONE', ( #43053, #80783, #68943, #53432, #4575, #19969 ) ) ;
#79672 =( NAMED_UNIT ( * ) SI_UNIT ( $, .STERADIAN. ) SOLID_ANGLE_UNIT ( ) );
#79673 = FACE_OUTER_BOUND ( 'NONE', #22533, .T. ) ;
#79674 = CARTESIAN_POINT ( 'NONE',  ( -110.3226427399711582, -60.00000000000000000, 196.3480137812436510 ) ) ;
#79675 = FACE_OUTER_BOUND ( 'NONE', #24402, .T. ) ;
#79676 = CARTESIAN_POINT ( 'NONE',  ( 46.81529435896409552, -59.99999999999998579, 64.36527784653102913 ) ) ;
#79677 = CARTESIAN_POINT ( 'NONE',  ( -10.73749782760683225, -5.000000000000000888, 12.43190307932432148 ) ) ;
#79678 = CARTESIAN_POINT ( 'NONE',  ( 24.83349330513380693, 1.593028355512270962E-15, 0.000000000000000000 ) ) ;
#79680 = CARTESIAN_POINT ( 'NONE',  ( 10.19381490664068401, -32.51059560698807616, 29.31869721906751991 ) ) ;
#79679 = CARTESIAN_POINT ( 'NONE',  ( -89.06819603267832974, -14.21045842199437637, 44.46121640280500031 ) ) ;
#79681 = DIRECTION ( 'NONE',  ( -1.000000000000000000, -1.224606353822377258E-16, -0.000000000000000000 ) ) ;
#79682 = CARTESIAN_POINT ( 'NONE',  ( -46.99000847530295033, -56.81688643933499350, 51.30717529515786168 ) ) ;
#79683 = CARTESIAN_POINT ( 'NONE',  ( 1.140727867604837575, -70.62093189267218918, 13.04401102971384141 ) ) ;
#79684 = ORIENTED_EDGE ( 'NONE', *, *, #40207, .T. ) ;
#79685 = CARTESIAN_POINT ( 'NONE',  ( 1.116109309485880940, 9.313441320552295011, -51.08022315653880696 ) ) ;
#79686 = CIRCLE ( 'NONE', #15939, 4.000000000000007105 ) ;
#79687 = CARTESIAN_POINT ( 'NONE',  ( 1.944839216437187431E-15, 45.30391365246044444, 18.75000000000001066 ) ) ;
#79688 = CARTESIAN_POINT ( 'NONE',  ( 5.650483388624516046, -6.544334031496181758, 2.031129859422145856 ) ) ;
#79689 = FACE_BOUND ( 'NONE', #54412, .T. ) ;
#79690 = ORIENTED_EDGE ( 'NONE', *, *, #46202, .F. ) ;
#79691 = CARTESIAN_POINT ( 'NONE',  ( -11.12687447062504376, -11.05336892415653161, 10.14262434277811487 ) ) ;
#79692 = EDGE_LOOP ( 'NONE', ( #60454, #30738, #91533, #63086, #1807 ) ) ;
#79693 = CARTESIAN_POINT ( 'NONE',  ( 80.42360447295121162, -30.00000000008963141, 191.4221980076535488 ) ) ;
#79694 = AXIS2_PLACEMENT_3D ( 'NONE', #62397, #35485, #19328 ) ;
#79695 = CARTESIAN_POINT ( 'NONE',  ( 0.3157512944461039472, -3.097794232780329171, -8.000000000000000000 ) ) ;
#79696 =( NAMED_UNIT ( * ) SI_UNIT ( $, .STERADIAN. ) SOLID_ANGLE_UNIT ( ) );
#79697 = CARTESIAN_POINT ( 'NONE',  ( 97.40260387833026812, -30.00000000000000000, 190.9330021436813354 ) ) ;
#79698 =( GEOMETRIC_REPRESENTATION_CONTEXT ( 3 ) GLOBAL_UNCERTAINTY_ASSIGNED_CONTEXT ( ( #88374 ) ) GLOBAL_UNIT_ASSIGNED_CONTEXT ( ( #92104, #40367, #7451 ) ) REPRESENTATION_CONTEXT ( 'NONE', 'WORKASPACE' ) );
#79699 = DIRECTION ( 'NONE',  ( 0.000000000000000000, 0.000000000000000000, 1.000000000000000000 ) ) ;
#79700 = VERTEX_POINT ( 'NONE', #47915 ) ;
#79701 = ADVANCED_FACE ( 'NONE', ( #54406 ), #82865, .T. ) ;
#79702 = ORIENTED_EDGE ( 'NONE', *, *, #86746, .F. ) ;
#79703 = ORIENTED_EDGE ( 'NONE', *, *, #72024, .T. ) ;
#79704 = CARTESIAN_POINT ( 'NONE',  ( -27.42282820131847743, 36.77223311657368043, 7.587759719706580697 ) ) ;
#79705 = CARTESIAN_POINT ( 'NONE',  ( 40.11650669486618881, 1.474610560812782335E-15, 0.000000000000000000 ) ) ;
#79706 = AXIS2_PLACEMENT_3D ( 'NONE', #8205, #98282, #50770 ) ;
#79707 = CARTESIAN_POINT ( 'NONE',  ( 38.58349330513380693, 1.593028355512270567E-15, 0.000000000000000000 ) ) ;
#79708 = ADVANCED_FACE ( 'NONE', ( #71148 ), #79391, .T. ) ;
#79709 = EDGE_CURVE ( 'NONE', #44516, #42513, #105632, .T. ) ;
#79710 = ORIENTED_EDGE ( 'NONE', *, *, #25287, .T. ) ;
#79711 = CARTESIAN_POINT ( 'NONE',  ( 9.165151389911683211, 105.2629551091633857, 4.000000000000002665 ) ) ;
#79712 = ORIENTED_EDGE ( 'NONE', *, *, #44488, .T. ) ;
#79713 = PLANE ( 'NONE',  #74181 ) ;
#79714 = CARTESIAN_POINT ( 'NONE',  ( 94.49521094355745277, -38.49073831966759940, 201.2139497919614541 ) ) ;
#79715 = CARTESIAN_POINT ( 'NONE',  ( 12.45811832932207608, 7.201502433278960780, 8.165472859347126189 ) ) ;
#79716 = CARTESIAN_POINT ( 'NONE',  ( 86.87161160163347517, -60.16194407056408977, -2.782513919925455603 ) ) ;
#79717 = CARTESIAN_POINT ( 'NONE',  ( 87.14793098496349444, -38.00000000001091394, 189.0872956505646414 ) ) ;
#79718 = CARTESIAN_POINT ( 'NONE',  ( 38.13456177595863750, 310.3538162346446825, 5.629934070714594618 ) ) ;
#79719 = DIRECTION ( 'NONE',  ( 0.5735764363510466035, -0.8191520442889914655, 1.003171929053524500E-16 ) ) ;
#79720 =( REPRESENTATION_RELATIONSHIP ('NONE','NONE', #69581, #25516 ) REPRESENTATION_RELATIONSHIP_WITH_TRANSFORMATION ( #85894 )SHAPE_REPRESENTATION_RELATIONSHIP( ) );
#79721 = CARTESIAN_POINT ( 'NONE',  ( -23.21751746555235840, 25.25267828308461304, -33.20617127781177658 ) ) ;
#79722 = CARTESIAN_POINT ( 'NONE',  ( -39.69476719266030074, 459.8381870091886867, 1.879428691193028467 ) ) ;
#79723 = SURFACE_SIDE_STYLE ('',( #45252 ) ) ;
#79724 = ORIENTED_EDGE ( 'NONE', *, *, #55769, .T. ) ;
#79725 = AXIS2_PLACEMENT_3D ( 'NONE', #83590, #51216, #84142 ) ;
#79726 = ADVANCED_FACE ( 'NONE', ( #104572 ), #46682, .T. ) ;
#79727 = LINE ( 'NONE', #46129, #44376 ) ;
#79728 = STYLED_ITEM ( 'NONE', ( #80655 ), #29376 ) ;
#79729 = CARTESIAN_POINT ( 'NONE',  ( -3.742273759344161732, 132.3176420647150451, 5.000000000000000000 ) ) ;
#79730 = ORIENTED_EDGE ( 'NONE', *, *, #71600, .F. ) ;
#79731 = DIRECTION ( 'NONE',  ( -1.000000000000000000, -1.224606353822377258E-16, -0.000000000000000000 ) ) ;
#79732 = CARTESIAN_POINT ( 'NONE',  ( -24.72181951469942973, 304.3809629507088630, 10.27362881536904382 ) ) ;
#79733 = CARTESIAN_POINT ( 'NONE',  ( 0.000000000000000000, 41.79151656018385097, 0.000000000000000000 ) ) ;
#79734 = UNCERTAINTY_MEASURE_WITH_UNIT (LENGTH_MEASURE( 1.000000000000000082E-05 ), #92927, 'distance_accuracy_value', 'NONE');
#79735 =( LENGTH_UNIT ( ) NAMED_UNIT ( * ) SI_UNIT ( .MILLI., .METRE. ) );
#79736 = CARTESIAN_POINT ( 'NONE',  ( 4.898587196589412829E-16, -15.12499999999999289, -8.000000000000000000 ) ) ;
#79737 = VECTOR ( 'NONE', #52371, 1000.000000000000000 ) ;
#79738 = CARTESIAN_POINT ( 'NONE',  ( -25.78771796013805329, -29.58065814986082032, 38.51179907014376624 ) ) ;
#79739 = PLANE ( 'NONE',  #76014 ) ;
#79740 = VERTEX_POINT ( 'NONE', #66240 ) ;
#79741 = CARTESIAN_POINT ( 'NONE',  ( 85.55570978684414740, -32.12474902453483594, 181.4378247361170224 ) ) ;
#79742 = EDGE_CURVE ( 'NONE', #2025, #47740, #57054, .T. ) ;
#79743 = DIRECTION ( 'NONE',  ( 0.000000000000000000, 1.000000000000000000, 0.000000000000000000 ) ) ;
#79744 = ORIENTED_EDGE ( 'NONE', *, *, #56761, .F. ) ;
#79745 = CARTESIAN_POINT ( 'NONE',  ( 94.34689964474569024, -57.67206129154387639, 0.5814794534858416242 ) ) ;
#79746 = CARTESIAN_POINT ( 'NONE',  ( 35.30457612794975120, 437.1674308734191072, 5.430039551426535382 ) ) ;
#79747 = CARTESIAN_POINT ( 'NONE',  ( 17.59386865953261392, -4.333298119783753677, 3.400962272007458598 ) ) ;
#79748 = CARTESIAN_POINT ( 'NONE',  ( -4.727711470032256003, -21.61685501870519843, -38.54800715255733223 ) ) ;
#79749 = CARTESIAN_POINT ( 'NONE',  ( 7.760496920029347656, -19.37151928998484607, 35.22200866297285415 ) ) ;
#79750 = CARTESIAN_POINT ( 'NONE',  ( -5.219866590715411370, -5.000000000000000000, -8.922269033013266792 ) ) ;
#79751 = CARTESIAN_POINT ( 'NONE',  ( 0.04606493828584038580, 9.175055303659558348, -8.057411785091792567 ) ) ;
#79753 = CARTESIAN_POINT ( 'NONE',  ( -13.12744080586892537, 8.268327554377737698, 8.825841405457195421 ) ) ;
#79752 = LINE ( 'NONE', #13946, #93036 ) ;
#79754 = CARTESIAN_POINT ( 'NONE',  ( 9.970195021754667764, 302.6460196488380916, -10.04373974541434045 ) ) ;
#79755 = CARTESIAN_POINT ( 'NONE',  ( 80.97977184163765685, 6.123233995736568081E-16, -5.000000000000011546 ) ) ;
#79756 = CARTESIAN_POINT ( 'NONE',  ( 9.999999999999998224, 15.00000000000000000, -1.544939622599252438 ) ) ;
#79757 = DIRECTION ( 'NONE',  ( 0.000000000000000000, 0.000000000000000000, -1.000000000000000000 ) ) ;
#79758 = AXIS2_PLACEMENT_3D ( 'NONE', #5908, #96008, #13997 ) ;
#79759 = CARTESIAN_POINT ( 'NONE',  ( -102.7253320651412594, -38.00000000000000000, 177.4151174456301590 ) ) ;
#79760 = CIRCLE ( 'NONE', #40197, 4.000000000000000888 ) ;
#79761 = VERTEX_POINT ( 'NONE', #57074 ) ;
#79762 = CARTESIAN_POINT ( 'NONE',  ( -8.661288751401347241, -0.2443065738830995925, 19.58558484236875330 ) ) ;
#79763 = DIRECTION ( 'NONE',  ( 0.000000000000000000, 1.000000000000000000, 0.000000000000000000 ) ) ;
#79764 = MECHANICAL_DESIGN_GEOMETRIC_PRESENTATION_REPRESENTATION (  '', ( #5713 ), #88407 ) ;
#79765 = CARTESIAN_POINT ( 'NONE',  ( -20.87337508428412747, -18.80453388489061339, -33.60507608888688935 ) ) ;
#79767 = CARTESIAN_POINT ( 'NONE',  ( -55.49686579569075917, -21.76997890922551449, -24.27064579473665873 ) ) ;
#79766 = CARTESIAN_POINT ( 'NONE',  ( 20.05074616892822448, 67.05096163904791240, 10.02537308446411224 ) ) ;
#79768 = EDGE_CURVE ( 'NONE', #3475, #30636, #33369, .T. ) ;
#79769 = EDGE_LOOP ( 'NONE', ( #40258, #101547, #57010 ) ) ;
#79770 = FACE_OUTER_BOUND ( 'NONE', #87837, .T. ) ;
#79772 = EDGE_LOOP ( 'NONE', ( #26051, #57447, #4335, #34613, #65925, #104915 ) ) ;
#79771 = STYLED_ITEM ( 'NONE', ( #48924 ), #21598 ) ;
#79773 = ADVANCED_FACE ( 'NONE', ( #40370 ), #32308, .T. ) ;
#79774 = EDGE_CURVE ( 'NONE', #105973, #39859, #81872, .T. ) ;
#79775 = FACE_BOUND ( 'NONE', #54926, .T. ) ;
#79776 = DIRECTION ( 'NONE',  ( 0.000000000000000000, -1.000000000000000000, 0.000000000000000000 ) ) ;
#79777 = CARTESIAN_POINT ( 'NONE',  ( -91.36484985775511802, -59.99999999999998579, -16.05759115015808192 ) ) ;
#79778 = EDGE_LOOP ( 'NONE', ( #31873, #24155, #46372, #87053 ) ) ;
#79779 = FACE_OUTER_BOUND ( 'NONE', #2599, .T. ) ;
#79780 = CARTESIAN_POINT ( 'NONE',  ( -8.400871283442178594, 54.02033344610075005, -1.531152949374503525 ) ) ;
#79781 = CARTESIAN_POINT ( 'NONE',  ( 0.000000000000000000, 0.000000000000000000, 0.000000000000000000 ) ) ;
#79783 = CARTESIAN_POINT ( 'NONE',  ( 20.77592568779148863, 5.000000000000003553, 0.000000000000000000 ) ) ;
#79782 = CARTESIAN_POINT ( 'NONE',  ( -5.000000000000000000, -60.71953810597282342, 12.61250543006821978 ) ) ;
#79784 = ADVANCED_FACE ( 'NONE', ( #42498 ), #57597, .F. ) ;
#79785 = CARTESIAN_POINT ( 'NONE',  ( -81.27817128073411368, -42.97173453030836754, 159.5003095331300926 ) ) ;
#79786 = EDGE_LOOP ( 'NONE', ( #94982, #48796, #26423, #80964, #78714 ) ) ;
#79787 = DIRECTION ( 'NONE',  ( 0.000000000000000000, -1.000000000000000000, 0.000000000000000000 ) ) ;
#79788 = VECTOR ( 'NONE', #15400, 1000.000000000000000 ) ;
#79789 = EDGE_CURVE ( 'NONE', #58364, #84222, #35517, .T. ) ;
#79790 = ORIENTED_EDGE ( 'NONE', *, *, #95077, .T. ) ;
#79791 = ORIENTED_EDGE ( 'NONE', *, *, #13692, .T. ) ;
#79793 =( BOUNDED_SURFACE ( )  B_SPLINE_SURFACE ( 3, 2, ( 
 ( #46777, #96408, #47297 ),
 ( #80722, #98503, #97980 ),
 ( #89892, #73696, #96922 ),
 ( #6839, #32749, #48356 ),
 ( #5783, #80194, #39238 ),
 ( #39763, #56441, #81248 ),
 ( #71569, #40276, #48880 ),
 ( #72112, #81774, #24653 ),
 ( #57505, #13864, #105021 ),
 ( #100636, #66684, #33273 ),
 ( #83924, #82863, #41336 ),
 ( #42397, #51007, #66143 ),
 ( #58046, #74228, #99025 ),
 ( #75292, #68284, #26796 ),
 ( #59666, #51553, #27340 ),
 ( #1385, #9486, #1929 ),
 ( #34353, #76353, #25188 ),
 ( #67227, #34880, #2466 ),
 ( #90969, #10559, #91501 ),
 ( #100104, #74755, #17078 ),
 ( #49954, #8959, #26270 ),
 ( #49422, #41867, #59133 ),
 ( #82325, #16531, #8436 ),
 ( #305, #92547, #92015 ),
 ( #18694, #43476, #84466 ),
 ( #25743, #835, #33806 ) ),
 .UNSPECIFIED., .F., .F., .F. ) 
 B_SPLINE_SURFACE_WITH_KNOTS ( ( 4, 2, 2, 2, 2, 2, 2, 2, 2, 2, 2, 2, 4 ),
 ( 3, 3 ),
 ( 0.000000000000000000, 0.0005478302971555681824, 0.001095660594311136365, 0.001643490891466704547, 0.001917406040044488530, 0.002191321188622272730, 0.002465236337200056929, 0.002739151485777841129, 0.003013066634355625328, 0.003286981782933409094, 0.003560896931511192860, 0.003834812080088977060, 0.004382642377244545459 ),
 ( 0.000000000000000000, 1.000000000000000000 ),
 .UNSPECIFIED. ) 
 GEOMETRIC_REPRESENTATION_ITEM ( )  RATIONAL_B_SPLINE_SURFACE ( (
 ( 1.000000000000000000, 0.7071067811865475727, 1.000000000000000000),
 ( 1.000000000000000000, 0.7205633224823966287, 1.000000000000000000),
 ( 1.000000000000000000, 0.7338046748641109396, 1.000000000000000000),
 ( 1.000000000000000000, 0.7598569482830193067, 1.000000000000000000),
 ( 1.000000000000000000, 0.7728059803406955863, 1.000000000000000000),
 ( 1.000000000000000000, 0.7970392697933029735, 1.000000000000000000),
 ( 1.000000000000000000, 0.8084357292879545964, 1.000000000000000000),
 ( 1.000000000000000000, 0.8242617997986435574, 1.000000000000000000),
 ( 1.000000000000000000, 0.8292815833602860121, 1.000000000000000000),
 ( 1.000000000000000000, 0.8385524799112056282, 1.000000000000000000),
 ( 1.000000000000000000, 0.8428399694378527762, 1.000000000000000000),
 ( 1.000000000000000000, 0.8506757475334101315, 1.000000000000000000),
 ( 1.000000000000000000, 0.8542245152659933005, 1.000000000000000000),
 ( 1.000000000000000000, 0.8604965487139695224, 1.000000000000000000),
 ( 1.000000000000000000, 0.8631692933856440764, 1.000000000000000000),
 ( 1.000000000000000000, 0.8674535388007971193, 1.000000000000000000),
 ( 1.000000000000000000, 0.8690878299427966525, 1.000000000000000000),
 ( 1.000000000000000000, 0.8713061800473307361, 1.000000000000000000),
 ( 1.000000000000000000, 0.8718871419634350861, 1.000000000000000000),
 ( 1.000000000000000000, 0.8719209662387901183, 1.000000000000000000),
 ( 1.000000000000000000, 0.8713887681177869826, 1.000000000000000000),
 ( 1.000000000000000000, 0.8692752663532745672, 1.000000000000000000),
 ( 1.000000000000000000, 0.8676790533738619748, 1.000000000000000000),
 ( 1.000000000000000000, 0.8614089247988900855, 1.000000000000000000),
 ( 1.000000000000000000, 0.8553884691243911487, 1.000000000000000000),
 ( 1.000000000000000000, 0.8477912478906596272, 1.000000000000000000) ) ) 
 REPRESENTATION_ITEM ( '' )  SURFACE ( )  );
#79792 = CARTESIAN_POINT ( 'NONE',  ( 28.58349330513380337, 1.593028355512270567E-15, 0.000000000000000000 ) ) ;
#79794 = CIRCLE ( 'NONE', #53917, 4.000000000000000888 ) ;
#79795 = ORIENTED_EDGE ( 'NONE', *, *, #64705, .F. ) ;
#79796 = CARTESIAN_POINT ( 'NONE',  ( -89.99999999999997158, -52.00000000000000000, 196.0238439516549818 ) ) ;
#79797 = CIRCLE ( 'NONE', #95367, 5.000000000000010658 ) ;
#79798 = DIRECTION ( 'NONE',  ( 0.000000000000000000, -1.000000000000000000, 0.000000000000000000 ) ) ;
#79799 = CARTESIAN_POINT ( 'NONE',  ( -77.37445547080469055, -57.51897485848058977, 195.6910618928241092 ) ) ;
#79800 = CARTESIAN_POINT ( 'NONE',  ( -4.478476647430157165, -65.27352079182048783, 3.992942460563209117 ) ) ;
#79801 = CARTESIAN_POINT ( 'NONE',  ( -65.02775738911799408, 48.00000000000000711, -4.794983377755789533 ) ) ;
#79802 = AXIS2_PLACEMENT_3D ( 'NONE', #11795, #1570, #85172 ) ;
#79803 = DIRECTION ( 'NONE',  ( 0.000000000000000000, 0.000000000000000000, -1.000000000000000000 ) ) ;
#79804 = CARTESIAN_POINT ( 'NONE',  ( 0.5678151344441708659, 27.34366627386414450, -40.61670413013122527 ) ) ;
#79805 = CARTESIAN_POINT ( 'NONE',  ( 89.90448154148772630, -29.99999999999993605, -11.15250327688899645 ) ) ;
#79806 = CARTESIAN_POINT ( 'NONE',  ( -42.11059216458311028, -14.21045842199439946, 45.52377215771286245 ) ) ;
#79807 = CARTESIAN_POINT ( 'NONE',  ( -53.66382358242866246, -32.56797292521762444, 54.84591734512859773 ) ) ;
#79808 = ORIENTED_EDGE ( 'NONE', *, *, #27480, .F. ) ;
#79809 = CARTESIAN_POINT ( 'NONE',  ( -12.34835181856066555, -4.332967528434497062, -12.86601580078907148 ) ) ;
#79810 = EDGE_LOOP ( 'NONE', ( #16835, #20299, #37538, #38969, #6544 ) ) ;
#79811 = CARTESIAN_POINT ( 'NONE',  ( -102.2165018913519674, -52.71483860031027291, 191.6989155236728664 ) ) ;
#79812 = CARTESIAN_POINT ( 'NONE',  ( -30.22667580650565711, 12.95764659710599709, -41.98307762325180192 ) ) ;
#79813 = EDGE_LOOP ( 'NONE', ( #1842, #42671, #85656, #70937 ) ) ;
#79814 = CARTESIAN_POINT ( 'NONE',  ( -16.75187969033531132, 34.25544727262101219, -24.30698433968676753 ) ) ;
#79815 = CARTESIAN_POINT ( 'NONE',  ( 90.90483875302744821, -38.34416586328904941, 3.443830408584400704 ) ) ;
#79816 = CARTESIAN_POINT ( 'NONE',  ( -7.188101187500002709, -11.18750000204838457, 2.977408999572648707 ) ) ;
#79817 = CARTESIAN_POINT ( 'NONE',  ( -10.01915592506624897, 302.6453132215667097, -2.043889601136170686 ) ) ;
#79819 = CARTESIAN_POINT ( 'NONE',  ( 32.64200203778431586, 464.2416672416183019, 8.403568186820924879 ) ) ;
#79818 = UNCERTAINTY_MEASURE_WITH_UNIT (LENGTH_MEASURE( 1.000000000000000082E-05 ), #31621, 'distance_accuracy_value', 'NONE');
#79820 = PLANE ( 'NONE',  #14524 ) ;
#79821 = DIRECTION ( 'NONE',  ( 0.000000000000000000, 0.000000000000000000, 1.000000000000000000 ) ) ;
#79822 = DIRECTION ( 'NONE',  ( -1.000000000000000000, -1.224606353822377258E-16, -0.000000000000000000 ) ) ;
#79823 = ORIENTED_EDGE ( 'NONE', *, *, #47254, .F. ) ;
#79824 = ORIENTED_EDGE ( 'NONE', *, *, #39084, .F. ) ;
#79825 = CARTESIAN_POINT ( 'NONE',  ( 50.70033520295613272, -42.97491282521573908, 53.11945173217547023 ) ) ;
#79826 = LINE ( 'NONE', #22695, #71417 ) ;
#79827 = CARTESIAN_POINT ( 'NONE',  ( -80.00000000000000000, -52.00000000000000000, -23.09707704303352926 ) ) ;
#79828 = EDGE_CURVE ( 'NONE', #92046, #21079, #106691, .T. ) ;
#79829 = CARTESIAN_POINT ( 'NONE',  ( -104.5126905089380074, -38.40291115105728181, 197.9553537318547853 ) ) ;
#79830 = ORIENTED_EDGE ( 'NONE', *, *, #86004, .T. ) ;
#79831 = CARTESIAN_POINT ( 'NONE',  ( 91.33644327358868509, -38.39903790272940398, -10.00103075991728829 ) ) ;
#79832 = CARTESIAN_POINT ( 'NONE',  ( 10.29730654639191378, 11.29257185708027755, -10.47295643394610209 ) ) ;
#79833 = CARTESIAN_POINT ( 'NONE',  ( -19.44215914665673495, 49.97163196006100350, 60.69499804416638966 ) ) ;
#79834 = CARTESIAN_POINT ( 'NONE',  ( 32.21797308369555424, 464.6987731533820352, 10.77720717743793344 ) ) ;
#79835 = CARTESIAN_POINT ( 'NONE',  ( -32.03156805414178621, 438.9467387518307646, 23.64778041155028276 ) ) ;
#79836 = CARTESIAN_POINT ( 'NONE',  ( 8.000000000000000000, -26.18750000409677270, 0.000000000000000000 ) ) ;
#79837 = CARTESIAN_POINT ( 'NONE',  ( 33.74271564777241394, 484.1802673187709729, 2.058285076122400081 ) ) ;
#79839 = CARTESIAN_POINT ( 'NONE',  ( -33.00540147334749008, 487.4196752801198613, 9.523982417603866324 ) ) ;
#79838 = AXIS2_PLACEMENT_3D ( 'NONE', #44769, #33624, #45822 ) ;
#79840 =( NAMED_UNIT ( * ) PLANE_ANGLE_UNIT ( ) SI_UNIT ( $, .RADIAN. ) );
#79841 = EDGE_CURVE ( 'NONE', #103962, #32281, #34705, .T. ) ;
#79842 = CARTESIAN_POINT ( 'NONE',  ( 91.63830261790323561, -60.00000000000000000, 202.2915991548087220 ) ) ;
#79843 = AXIS2_PLACEMENT_3D ( 'NONE', #81889, #56553, #47928 ) ;
#79844 = CARTESIAN_POINT ( 'NONE',  ( 82.42421628608209971, -5.000000000000000888, 6.123233995736779101E-16 ) ) ;
#79845 = VERTEX_POINT ( 'NONE', #15562 ) ;
#79846 = CARTESIAN_POINT ( 'NONE',  ( 57.95396635055557510, -29.07655056746734701, 62.48005105517134439 ) ) ;
#79847 = CARTESIAN_POINT ( 'NONE',  ( -31.38357374201002870, 298.3332731590748494, -9.233538704492573856 ) ) ;
#79848 = CARTESIAN_POINT ( 'NONE',  ( 7.413471587080155523, 32.64352159168327461, -3.013058070223547880 ) ) ;
#79849 = ORIENTED_EDGE ( 'NONE', *, *, #100752, .F. ) ;
#79851 = CARTESIAN_POINT ( 'NONE',  ( -9.771873710511815858, -50.53670347359850723, 29.13520411490522122 ) ) ;
#79850 = CARTESIAN_POINT ( 'NONE',  ( -110.9986318115168018, -38.35598781044485150, 173.1127387114688645 ) ) ;
#79852 = DIRECTION ( 'NONE',  ( 0.5735764363510466035, -0.8191520442889914655, 1.003171929053524500E-16 ) ) ;
#79853 = CARTESIAN_POINT ( 'NONE',  ( 9.999999999999998224, 15.00000000000000000, -4.582575694955843382 ) ) ;
#79854 = DIRECTION ( 'NONE',  ( 0.000000000000000000, 0.000000000000000000, 1.000000000000000000 ) ) ;
#79855 = CARTESIAN_POINT ( 'NONE',  ( -7.188101187500000044, -9.781250002048384573, -8.802885111219163269E-16 ) ) ;
#79856 = CARTESIAN_POINT ( 'NONE',  ( -9.999999999999996447, -5.000000000000002665, -86.30899693747676338 ) ) ;
#79857 = FACE_OUTER_BOUND ( 'NONE', #64784, .T. ) ;
#79858 = ORIENTED_EDGE ( 'NONE', *, *, #31916, .T. ) ;
#79859 = CARTESIAN_POINT ( 'NONE',  ( 84.12090616306510071, -35.94182022319192527, 174.7657314699721098 ) ) ;
#79860 = EDGE_CURVE ( 'NONE', #80889, #30981, #10561, .T. ) ;
#79861 = CARTESIAN_POINT ( 'NONE',  ( 8.619464431494504808, 22.85699679202996393, -9.629649721936179265E-31 ) ) ;
#79862 = CARTESIAN_POINT ( 'NONE',  ( -33.21102376836598324, 438.9613914113128317, 23.92328486949907074 ) ) ;
#79863 = ORIENTED_EDGE ( 'NONE', *, *, #104872, .T. ) ;
#79864 = CARTESIAN_POINT ( 'NONE',  ( -37.62251730745840916, 437.3427388312646258, 4.535622330043208805 ) ) ;
#79865 = CARTESIAN_POINT ( 'NONE',  ( 5.079306836895828070, -4.308466644845876381, -17.11871833148104471 ) ) ;
#79866 =( LENGTH_UNIT ( ) NAMED_UNIT ( * ) SI_UNIT ( .MILLI., .METRE. ) );
#79867 = CARTESIAN_POINT ( 'NONE',  ( -33.84683838397652522, 42.75782337701531333, -63.96829032114721514 ) ) ;
#79868 = PRESENTATION_STYLE_ASSIGNMENT (( #37871 ) ) ;
#79869 = VECTOR ( 'NONE', #28293, 999.9999999999998863 ) ;
#79870 = ORIENTED_EDGE ( 'NONE', *, *, #10691, .F. ) ;
#79871 =( GEOMETRIC_REPRESENTATION_CONTEXT ( 3 ) GLOBAL_UNCERTAINTY_ASSIGNED_CONTEXT ( ( #41344 ) ) GLOBAL_UNIT_ASSIGNED_CONTEXT ( ( #34687, #8770, #75085 ) ) REPRESENTATION_CONTEXT ( 'NONE', 'WORKASPACE' ) );
#79873 = CIRCLE ( 'NONE', #33397, 24.55262289886175964 ) ;
#79872 =( NAMED_UNIT ( * ) SI_UNIT ( $, .STERADIAN. ) SOLID_ANGLE_UNIT ( ) );
#79874 = CONICAL_SURFACE ( 'NONE', #102299, 4.000000000000001776, 0.9599310885968774798 ) ;
#79875 = CARTESIAN_POINT ( 'NONE',  ( -81.31126947214923462, -29.99999999999999645, 26.13564777162193309 ) ) ;
#79876 = CARTESIAN_POINT ( 'NONE',  ( -5.000000000005099920, -10.14983348571164434, -12.32139453386874450 ) ) ;
#79877 = DIRECTION ( 'NONE',  ( 0.000000000000000000, 1.000000000000000000, 0.000000000000000000 ) ) ;
#79879 = CARTESIAN_POINT ( 'NONE',  ( -13.12174090438720953, 8.291105618454766457, -8.825937222380286329 ) ) ;
#79878 = DIRECTION ( 'NONE',  ( 0.000000000000000000, -1.000000000000000000, 0.000000000000000000 ) ) ;
#79880 = CARTESIAN_POINT ( 'NONE',  ( -5.082755093536326818, -21.21875000204838457, 5.082755093536325042 ) ) ;
#79881 = CARTESIAN_POINT ( 'NONE',  ( -55.22048556067662162, 40.83906611472863801, 34.80214219330362369 ) ) ;
#79882 = LINE ( 'NONE', #80405, #86239 ) ;
#79883 = ORIENTED_EDGE ( 'NONE', *, *, #85485, .F. ) ;
#79884 = CARTESIAN_POINT ( 'NONE',  ( -18.91772294110159081, 48.25776538900139911, 62.18609455222676274 ) ) ;
#79885 = LINE ( 'NONE', #78301, #56414 ) ;
#79886 = CARTESIAN_POINT ( 'NONE',  ( -3.003085654062773280, 102.9757869438805642, -5.000000000000000000 ) ) ;
#79887 = CARTESIAN_POINT ( 'NONE',  ( -13.50000000000000000, -7.794228634059976457, -13.00000000000000000 ) ) ;
#79888 = CARTESIAN_POINT ( 'NONE',  ( -14.63960045772152263, 2.604522098982320344, 3.217332696247229062 ) ) ;
#79889 = MECHANICAL_DESIGN_GEOMETRIC_PRESENTATION_REPRESENTATION (  '', ( #29973 ), #83361 ) ;
#79890 = VERTEX_POINT ( 'NONE', #106152 ) ;
#79891 = SURFACE_STYLE_USAGE ( .BOTH. , #6529 ) ;
#79892 = EDGE_CURVE ( 'NONE', #31549, #58193, #16632, .T. ) ;
#79893 = FACE_OUTER_BOUND ( 'NONE', #32740, .T. ) ;
#79894 = VERTEX_POINT ( 'NONE', #58145 ) ;
#79895 = EDGE_CURVE ( 'NONE', #3716, #79761, #91074, .T. ) ;
#79896 = CARTESIAN_POINT ( 'NONE',  ( -28.20028738399506096, 34.17715485567774181, 9.432562058334550414 ) ) ;
#79897 = CARTESIAN_POINT ( 'NONE',  ( -0.9999999999999943379, -1.409462824231155764E-15, 101.0455488498966758 ) ) ;
#79898 = CARTESIAN_POINT ( 'NONE',  ( 9.797174393178825657E-16, 15.00000000000000000, 8.000000000000000000 ) ) ;
#79899 = B_SPLINE_CURVE_WITH_KNOTS ( 'NONE', 3,
 ( #58685, #84013, #19340, #75379, #77524, #18789, #52169, #91587, #76980, #10119, #43029, #66771, #1478, #75918, #51637, #36042 ),
 .UNSPECIFIED., .F., .F.,
 ( 4, 2, 2, 2, 2, 2, 2, 4 ),
 ( 7.152448122690996019E-18, 0.0005173708498437065446, 0.001034741699687405933, 0.001552112549531105322, 0.002069483399374804494, 0.002586854249218503883, 0.003104225099062203272, 0.004138966798749600315 ),
 .UNSPECIFIED. ) ;
#79900 = CARTESIAN_POINT ( 'NONE',  ( -111.0927031282581225, -59.99999999999998579, 153.0492826848410459 ) ) ;
#79901 = PRESENTATION_STYLE_ASSIGNMENT (( #4431 ) ) ;
#79902 = DIRECTION ( 'NONE',  ( -1.000000000000000000, -1.224606353822377258E-16, -0.000000000000000000 ) ) ;
#79903 = PLANE ( 'NONE',  #92464 ) ;
#79904 = B_SPLINE_CURVE_WITH_KNOTS ( 'NONE', 3,
 ( #63440, #22461, #96333, #45131 ),
 .UNSPECIFIED., .F., .F.,
 ( 4, 4 ),
 ( 0.000000000000000000, 0.0002629889189352557668 ),
 .UNSPECIFIED. ) ;
#79905 = CARTESIAN_POINT ( 'NONE',  ( -84.37166457177885093, -32.45306040212211940, 171.8685867912538185 ) ) ;
#79906 = VERTEX_POINT ( 'NONE', #74325 ) ;
#79907 = AXIS2_PLACEMENT_3D ( 'NONE', #39651, #104355, #56857 ) ;
#79908 = CARTESIAN_POINT ( 'NONE',  ( 34.55448620566968287, 42.66471839012794476, -62.99543540866341118 ) ) ;
#79909 = ADVANCED_FACE ( 'NONE', ( #75394 ), #84645, .T. ) ;
#79910 = ORIENTED_EDGE ( 'NONE', *, *, #91542, .T. ) ;
#79911 = DIRECTION ( 'NONE',  ( -0.000000000000000000, -0.000000000000000000, 1.000000000000000000 ) ) ;
#79912 = EDGE_CURVE ( 'NONE', #61174, #10145, #31240, .T. ) ;
#79913 = CARTESIAN_POINT ( 'NONE',  ( 0.9999999999999997780, -67.04094093997568393, 11.34959271885065135 ) ) ;
#79914 = CARTESIAN_POINT ( 'NONE',  ( -84.94869132047828941, -52.70034892481147182, 8.410862686292052359 ) ) ;
#79915 = FACE_BOUND ( 'NONE', #102881, .T. ) ;
#79916 = ADVANCED_FACE ( 'NONE', ( #25841 ), #53611, .T. ) ;
#79917 = CARTESIAN_POINT ( 'NONE',  ( -15.72218280906590593, 5.595371698621922185, -6.516822309426167692 ) ) ;
#79918 = CARTESIAN_POINT ( 'NONE',  ( 9.609486011791085858, 8.908497650349774588, 0.000000000000000000 ) ) ;
#79919 = DIRECTION ( 'NONE',  ( -1.000000000000000000, -1.224606353822377258E-16, -0.000000000000000000 ) ) ;
#79920 = CARTESIAN_POINT ( 'NONE',  ( 38.86638200451619696, 1.340359594676612611E-15, 0.000000000000000000 ) ) ;
#79921 = CARTESIAN_POINT ( 'NONE',  ( 107.9653405324804680, -30.00000000000002132, 188.7583403580863717 ) ) ;
#79922 = CARTESIAN_POINT ( 'NONE',  ( -92.03818768401583839, -29.99999999999997513, 46.84875813697714619 ) ) ;
#79923 = CARTESIAN_POINT ( 'NONE',  ( -63.25552657885100416, -46.43896528863776751, 84.68699370951671312 ) ) ;
#79924 = EDGE_LOOP ( 'NONE', ( #33305, #73399, #70263, #51691 ) ) ;
#79925 = CARTESIAN_POINT ( 'NONE',  ( -49.76159010805244520, 39.42507290984417523, 41.92561844419851980 ) ) ;
#79926 = CARTESIAN_POINT ( 'NONE',  ( 87.39880973402036091, -60.00000000001985967, 203.7820402037370684 ) ) ;
#79927 = VERTEX_POINT ( 'NONE', #98074 ) ;
#79928 = CARTESIAN_POINT ( 'NONE',  ( 1.994190048904284973, -29.02935297365003464, 28.72563985546674914 ) ) ;
#79929 = CARTESIAN_POINT ( 'NONE',  ( 7.188101187500000933, -19.43750000204838457, -2.977408999572650483 ) ) ;
#79930 = FACE_OUTER_BOUND ( 'NONE', #15000, .T. ) ;
#79931 = EDGE_LOOP ( 'NONE', ( #95908, #97038, #101125, #4753 ) ) ;
#79932 = DIRECTION ( 'NONE',  ( -1.000000000000000000, -1.224606353822377258E-16, -0.000000000000000000 ) ) ;
#79933 = ORIENTED_EDGE ( 'NONE', *, *, #35901, .F. ) ;
#79934 = LINE ( 'NONE', #103693, #76860 ) ;
#79935 = CARTESIAN_POINT ( 'NONE',  ( -5.082755093536325042, -29.46875000204838813, -5.082755093536325930 ) ) ;
#79936 = CARTESIAN_POINT ( 'NONE',  ( -100.6329257265545749, -59.99999999999997868, 201.6847065643074188 ) ) ;
#79937 = CARTESIAN_POINT ( 'NONE',  ( 16.07917213302808790, 5.118112109469848292, 4.258304778695062964 ) ) ;
#79938 = CARTESIAN_POINT ( 'NONE',  ( -7.188101187500001821, -27.87500000204838457, -2.977408999572651371 ) ) ;
#79939 = CYLINDRICAL_SURFACE ( 'NONE', #11961, 4.000000000000000888 ) ;
#79940 = AXIS2_PLACEMENT_3D ( 'NONE', #92064, #1443, #67799 ) ;
#79941 =( NAMED_UNIT ( * ) PLANE_ANGLE_UNIT ( ) SI_UNIT ( $, .RADIAN. ) );
#79942 = CARTESIAN_POINT ( 'NONE',  ( -9.999999999999996447, 48.00000000000000000, -83.69100306252323662 ) ) ;
#79943 = DIRECTION ( 'NONE',  ( 0.000000000000000000, -0.000000000000000000, 1.000000000000000000 ) ) ;
#79944 = CARTESIAN_POINT ( 'NONE',  ( -43.67631032990321671, 390.4612520042348365, 15.75310585023781407 ) ) ;
#79945 = CARTESIAN_POINT ( 'NONE',  ( 105.5351503390431844, -60.00000000000002132, 185.3579240910585497 ) ) ;
#79946 = AXIS2_PLACEMENT_3D ( 'NONE', #59316, #58787, #9668 ) ;
#79947 = CARTESIAN_POINT ( 'NONE',  ( -36.98928843693574464, -18.74377913183838729, 32.19268859513226033 ) ) ;
#79948 = ORIENTED_EDGE ( 'NONE', *, *, #73314, .T. ) ;
#79949 = CARTESIAN_POINT ( 'NONE',  ( -35.61930400255787532, 462.7723509827301314, 4.024879462734057611 ) ) ;
#79950 = CARTESIAN_POINT ( 'NONE',  ( 36.41154140541230078, -49.89264740158284184, 38.19905247078427379 ) ) ;
#79951 = CARTESIAN_POINT ( 'NONE',  ( -11.19959342722916951, 9.651029144387260302E-13, -19.43146043915260179 ) ) ;
#79952 = VERTEX_POINT ( 'NONE', #24226 ) ;
#79953 = DIRECTION ( 'NONE',  ( 0.000000000000000000, -0.5000000000000006661, 0.8660254037844382635 ) ) ;
#79954 = EDGE_CURVE ( 'NONE', #57189, #48471, #99657, .T. ) ;
#79955 = CARTESIAN_POINT ( 'NONE',  ( -74.48071276423321763, -38.33020298555444327, 164.6109856697501925 ) ) ;
#79956 = ORIENTED_EDGE ( 'NONE', *, *, #19731, .F. ) ;
#79958 = CARTESIAN_POINT ( 'NONE',  ( 45.43339346675878687, 430.7348383325900727, 7.234598910837349628 ) ) ;
#79957 = CARTESIAN_POINT ( 'NONE',  ( 4.651269564039822946, -4.999999999999991118, -15.66707428873065311 ) ) ;
#79959 = CARTESIAN_POINT ( 'NONE',  ( 15.97435091970916510, 37.21084721865046419, 22.07459719473141746 ) ) ;
#79960 = CARTESIAN_POINT ( 'NONE',  ( -33.88469969133009840, 464.6054137899091074, 6.797944932417651742 ) ) ;
#79961 = CARTESIAN_POINT ( 'NONE',  ( 62.59428447264396311, 4.000000000000015099, 4.898587196589422689E-16 ) ) ;
#79963 = B_SPLINE_CURVE_WITH_KNOTS ( 'NONE', 3,
 ( #59554, #92422, #723, #91906, #42283, #33691, #66034, #66565, #1268, #83803, #25071, #57929, #90849, #10446, #75718, #34234, #67106, #49843 ),
 .UNSPECIFIED., .F., .F.,
 ( 4, 2, 2, 2, 2, 2, 2, 2, 4 ),
 ( 0.5000000000000000000, 0.5625000000000000000, 0.6250000000000000000, 0.6875000000000000000, 0.7500000000000000000, 0.8125000000000000000, 0.8750000000000001110, 0.9375000000000000000, 1.000000000000000000 ),
 .UNSPECIFIED. ) ;
#79962 = LINE ( 'NONE', #4497, #27402 ) ;
#79964 = CARTESIAN_POINT ( 'NONE',  ( 10.11650669486618881, 4.000000000000003553, 4.898587196589414801E-16 ) ) ;
#79965 = CARTESIAN_POINT ( 'NONE',  ( 0.000000000000000000, 0.000000000000000000, 0.000000000000000000 ) ) ;
#79966 = CARTESIAN_POINT ( 'NONE',  ( 92.80923683822102532, -60.00000000000001421, 30.31541718318534606 ) ) ;
#79967 = CARTESIAN_POINT ( 'NONE',  ( 6.249999999999998224, 4.618802153517004960, 7.999999999999998224 ) ) ;
#79968 = FACE_BOUND ( 'NONE', #67248, .T. ) ;
#79969 = CARTESIAN_POINT ( 'NONE',  ( 59.41111111111111143, 3.309500000000014541, 0.000000000000000000 ) ) ;
#79970 = EDGE_CURVE ( 'NONE', #24510, #43850, #99779, .T. ) ;
#79971 = ORIENTED_EDGE ( 'NONE', *, *, #7846, .T. ) ;
#79972 = CIRCLE ( 'NONE', #67897, 1.000000000000001110 ) ;
#79973 = CARTESIAN_POINT ( 'NONE',  ( -87.59720537968154019, -30.00000000000068212, -17.71635471304703557 ) ) ;
#79974 = VERTEX_POINT ( 'NONE', #43567 ) ;
#79975 = CARTESIAN_POINT ( 'NONE',  ( 102.9313392694734688, 6.123233995736582872E-16, -5.000000000000011546 ) ) ;
#79976 = CARTESIAN_POINT ( 'NONE',  ( 8.642223818571391547, 22.39656424817261993, 0.000000000000000000 ) ) ;
#79977 = DIRECTION ( 'NONE',  ( -1.000000000000000000, 0.000000000000000000, 0.000000000000000000 ) ) ;
#79978 = CARTESIAN_POINT ( 'NONE',  ( 82.80415505393953879, -45.27777509290327629, -14.83251382924433237 ) ) ;
#79979 = CARTESIAN_POINT ( 'NONE',  ( -7.188101187500002709, -23.18750000204838813, 2.977408999572648707 ) ) ;
#79980 = DIRECTION ( 'NONE',  ( 0.000000000000000000, 0.000000000000000000, -1.000000000000000000 ) ) ;
#79981 =( LENGTH_UNIT ( ) NAMED_UNIT ( * ) SI_UNIT ( .MILLI., .METRE. ) );
#79982 = CARTESIAN_POINT ( 'NONE',  ( 5.799999999999999822, 4.618802153517003184, -8.000000000000000000 ) ) ;
#79983 = ORIENTED_EDGE ( 'NONE', *, *, #43711, .F. ) ;
#79984 = AXIS2_PLACEMENT_3D ( 'NONE', #28, #66393, #32998 ) ;
#79985 = AXIS2_PLACEMENT_3D ( 'NONE', #13612, #70283, #55131 ) ;
#79986 = AXIS2_PLACEMENT_3D ( 'NONE', #10258, #50694, #75525 ) ;
#79988 = EDGE_LOOP ( 'NONE', ( #48181, #29988 ) ) ;
#79987 = CYLINDRICAL_SURFACE ( 'NONE', #61592, 8.000000000000000000 ) ;
#79989 = CARTESIAN_POINT ( 'NONE',  ( 79.23531459263197974, -46.43389914412935582, 148.5210349803398344 ) ) ;
#79990 = EDGE_CURVE ( 'NONE', #58295, #53379, #94981, .T. ) ;
#79991 = MECHANICAL_DESIGN_GEOMETRIC_PRESENTATION_REPRESENTATION (  '', ( #85233 ), #78298 ) ;
#79992 = CARTESIAN_POINT ( 'NONE',  ( -38.81492354314366366, 27.33048476904497548, -12.09895268554974379 ) ) ;
#79993 = ORIENTED_EDGE ( 'NONE', *, *, #39491, .F. ) ;
#79994 = CARTESIAN_POINT ( 'NONE',  ( -12.50000000000000178, 39.23410961838661137, -63.25741677043061628 ) ) ;
#79995 = CARTESIAN_POINT ( 'NONE',  ( -0.9985759808268045434, 14.07160882109565314, -51.25515926415730661 ) ) ;
#79996 = CARTESIAN_POINT ( 'NONE',  ( 2.977408999572650927, -15.87500000204838635, -7.188101187500000933 ) ) ;
#79997 = CARTESIAN_POINT ( 'NONE',  ( 10.61948831387149461, 45.32774727476012799, 15.37414989828174861 ) ) ;
#79998 = ADVANCED_FACE ( 'NONE', ( #51647 ), #93028, .T. ) ;
#79999 = CARTESIAN_POINT ( 'NONE',  ( 15.86539410927191440, 294.5609640058206082, 9.875179453861520074 ) ) ;
#80000 = ORIENTED_EDGE ( 'NONE', *, *, #25553, .T. ) ;
#80001 = PRESENTATION_STYLE_ASSIGNMENT (( #81572 ) ) ;
#80002 = DIRECTION ( 'NONE',  ( 0.000000000000000000, 1.000000000000000000, 0.000000000000000000 ) ) ;
#80003 = LINE ( 'NONE', #32014, #52666 ) ;
#80004 = CARTESIAN_POINT ( 'NONE',  ( -9.918512371096301905, 81.20717007729450643, -1.297150762882695263 ) ) ;
#80005 = CARTESIAN_POINT ( 'NONE',  ( 48.02835407290414338, 14.94086294439859408, -16.85535821593631667 ) ) ;
#80006 = ORIENTED_EDGE ( 'NONE', *, *, #20879, .F. ) ;
#80007 = CARTESIAN_POINT ( 'NONE',  ( -8.000000000000000000, -8.937500004096769146, -9.797174393178825657E-16 ) ) ;
#80008 = CARTESIAN_POINT ( 'NONE',  ( -9.718871381506426488, -13.69778559267061802, 31.90811388817558480 ) ) ;
#80009 = CARTESIAN_POINT ( 'NONE',  ( 5.290067270632160756, 52.08006895350504806, -6.031152949374595451 ) ) ;
#80010 = CARTESIAN_POINT ( 'NONE',  ( 7.500000000000007105, 44.29449649216757479, -60.86453129175313137 ) ) ;
#80013 = ADVANCED_FACE ( 'NONE', ( #76453 ), #84027, .F. ) ;
#80012 = VECTOR ( 'NONE', #94229, 1000.000000000000227 ) ;
#80011 = APPLICATION_PROTOCOL_DEFINITION ( 'draft international standard', 'automotive_design', 1998, #5231 ) ;
#80014 = CARTESIAN_POINT ( 'NONE',  ( 37.72553331254036380, 27.55007976727166508, 13.45617127781008016 ) ) ;
#80015 = ORIENTED_EDGE ( 'NONE', *, *, #5983, .T. ) ;
#80016 = CARTESIAN_POINT ( 'NONE',  ( -6.593526337342319188, -48.85592895810358982, 39.35043480061310106 ) ) ;
#80017 = CARTESIAN_POINT ( 'NONE',  ( 0.000000000000000000, -6.505213034913025026E-15, 0.000000000000000000 ) ) ;
#80018 = CARTESIAN_POINT ( 'NONE',  ( -46.00000000000000000, 463.6369139993306021, 9.775485381098368620 ) ) ;
#80019 = CARTESIAN_POINT ( 'NONE',  ( -69.98795449185568884, -30.00000000000000000, 95.28635153949326764 ) ) ;
#80020 = DIRECTION ( 'NONE',  ( -0.000000000000000000, -0.000000000000000000, -1.000000000000000000 ) ) ;
#80021 = COLOUR_RGB ( '', 0.40784314, 0.44705882, 0.49803922) ;
#80022 = ORIENTED_EDGE ( 'NONE', *, *, #72002, .F. ) ;
#80023 = CARTESIAN_POINT ( 'NONE',  ( 19.34999999999999787, -3.309499999999999886, 0.000000000000000000 ) ) ;
#80024 = CARTESIAN_POINT ( 'NONE',  ( 103.1126816730884173, -57.63601659308862679, 202.8018784190458916 ) ) ;
#80025 = CARTESIAN_POINT ( 'NONE',  ( -3.312116827214752676E-14, 12.91535575336970965, 51.75000000000017764 ) ) ;
#80026 = CARTESIAN_POINT ( 'NONE',  ( 0.000000000000000000, -46.00000000000000000, 112.0000000000000000 ) ) ;
#80027 = CARTESIAN_POINT ( 'NONE',  ( -14.77180908113605362, 22.75028154196801822, 2.587654188242820563 ) ) ;
#80028 = CARTESIAN_POINT ( 'NONE',  ( -5.624108760328526913, 53.41997841376465317, 8.497405280055550847 ) ) ;
#80029 = CARTESIAN_POINT ( 'NONE',  ( -74.78472009158446099, -60.00000000000000711, 179.5816843754311094 ) ) ;
#80030 = DIRECTION ( 'NONE',  ( 1.000000000000000000, 0.000000000000000000, 0.000000000000000000 ) ) ;
#80031 = DIRECTION ( 'NONE',  ( 0.000000000000000000, -1.000000000000000000, 0.000000000000000000 ) ) ;
#80032 = CARTESIAN_POINT ( 'NONE',  ( -28.89099332391479535, 50.00000000002003731, 58.53034795348396813 ) ) ;
#80033 = CARTESIAN_POINT ( 'NONE',  ( -86.34127813042697142, -21.01238092349332831, 180.7339398568655042 ) ) ;
#80034 = ORIENTED_EDGE ( 'NONE', *, *, #3327, .T. ) ;
#80035 = CARTESIAN_POINT ( 'NONE',  ( 34.99329892478774440, 329.7144367575227193, -3.662448773238903055 ) ) ;
#80036 = EDGE_CURVE ( 'NONE', #88651, #78362, #65612, .T. ) ;
#80037 = DIRECTION ( 'NONE',  ( 0.5735764363510440500, 0.8191520442889932418, 0.000000000000000000 ) ) ;
#80038 = ADVANCED_FACE ( 'NONE', ( #2030 ), #100732, .T. ) ;
#80040 = CARTESIAN_POINT ( 'NONE',  ( -1.714505518806292863E-15, 60.00000000000000000, 6.999999999999992895 ) ) ;
#80039 = CIRCLE ( 'NONE', #86937, 4.000000000000007105 ) ;
#80041 = CARTESIAN_POINT ( 'NONE',  ( -81.59149017617403388, -37.80312470321176477, -14.43359743736064971 ) ) ;
#80042 = LINE ( 'NONE', #6690, #101151 ) ;
#80043 = DIRECTION ( 'NONE',  ( 0.000000000000000000, -1.000000000000000000, 0.000000000000000000 ) ) ;
#80044 = ORIENTED_EDGE ( 'NONE', *, *, #97411, .T. ) ;
#80045 = LINE ( 'NONE', #6694, #85472 ) ;
#80046 = EDGE_CURVE ( 'NONE', #56846, #87110, #93266, .T. ) ;
#80047 = CARTESIAN_POINT ( 'NONE',  ( 11.68384993704314567, 21.00149377200780165, 7.699446549790801342 ) ) ;
#80049 = CARTESIAN_POINT ( 'NONE',  ( 9.999999999999996447, 0.000000000000000000, -10.00000000000000000 ) ) ;
#80048 = B_SPLINE_CURVE_WITH_KNOTS ( 'NONE', 3,
 ( #93888, #18973, #52350, #78227, #34623, #67493, #76624, #52894, #101450, #85262, #3818, #11345, #44278, #100373, #20045, #44821, #94434, #20594, #86352, #92271, #53938, #79286, #56042, #71191, #5916, #5408, #87923, #86871, #4878, #97056, #103565, #15076, #104086, #31300, #29716, #96545, #45866, #88454, #37277, #78744, #103048, #22677, #29204, #62590, #95474, #38843, #96014, #14529, #47961, #30771, #4342, #38330, #63657, #55514, #105158, #64187, #47438, #88976, #80329, #21619, #23201, #62078, #30226, #70144, #94966, #21105, #70673, #6443, #54449, #54992, #39379, #63112, #22141, #12945, #71706, #37814, #14002, #87402 ),
 .UNSPECIFIED., .F., .F.,
 ( 4, 1, 1, 1, 2, 2, 2, 2, 1, 2, 2, 2, 2, 1, 1, 1, 2, 2, 2, 2, 1, 1, 2, 2, 2, 2, 1, 2, 2, 2, 2, 1, 2, 2, 2, 2, 2, 2, 2, 1, 2, 2, 2, 2, 4 ),
 ( 0.000000000000000000, 0.007812500000051594146, 0.01171875000007735826, 0.01367187500009205137, 0.01464843750009946731, 0.01562500000010688325, 0.02343750000011152884, 0.02734375000011205620, 0.02929687500011102230, 0.03027343750010927023, 0.03125000000010751816, 0.06250000000006696033, 0.09375000000002639555, 0.1093750000000080352, 0.1171874999999988620, 0.1210937499999942824, 0.1230468749999939632, 0.1249999999999936301, 0.1875000000000501543, 0.2187500000000764111, 0.2343750000000898726, 0.2421875000000949796, 0.2460937500000979217, 0.2500000000001008083, 0.3125000000001723066, 0.3437500000002080558, 0.3593750000002235434, 0.3671875000002313150, 0.3750000000002390310, 0.4375000000002702838, 0.4687500000002808309, 0.4843750000002861045, 0.4921875000002899347, 0.5000000000002936540, 0.5625000000002762235, 0.5937500000002652323, 0.6250000000002541301, 0.6875000000002211564, 0.7187500000002028377, 0.7343750000001891820, 0.7421875000001824096, 0.7500000000001757483, 0.8750000000000874856, 0.9375000000000437428, 1.000000000000000000 ),
 .UNSPECIFIED. ) ;
#80050 = CARTESIAN_POINT ( 'NONE',  ( -33.74271564777242105, 484.1802673187710297, 2.058285076122328139 ) ) ;
#80051 = CARTESIAN_POINT ( 'NONE',  ( 89.98361085880227961, -30.00000000000001776, -2.850603255620693055 ) ) ;
#80052 = CARTESIAN_POINT ( 'NONE',  ( -81.08683376277613775, -29.09337554716583796, 141.3844950506220925 ) ) ;
#80053 = AXIS2_PLACEMENT_3D ( 'NONE', #17867, #59390, #50720 ) ;
#80054 = EDGE_LOOP ( 'NONE', ( #72110, #89626, #63409, #46412, #25688, #59365 ) ) ;
#80055 = CARTESIAN_POINT ( 'NONE',  ( 1.363418823244991529, -14.21045842199435150, 34.36840973699906954 ) ) ;
#80056 = CARTESIAN_POINT ( 'NONE',  ( 4.503026011213026258, 250.5434186228332010, 3.965236350746919047 ) ) ;
#80057 = CARTESIAN_POINT ( 'NONE',  ( 107.5465923744455665, -57.65770870721873109, 199.5374833259203342 ) ) ;
#80058 = COLOUR_RGB ( '', 0.40784314, 0.44705882, 0.49803922) ;
#80059 = CARTESIAN_POINT ( 'NONE',  ( 16.75187969033571989, 37.11970326878314097, 21.80698433968582961 ) ) ;
#80060 = VECTOR ( 'NONE', #37547, 1000.000000000000000 ) ;
#80061 = CARTESIAN_POINT ( 'NONE',  ( 32.45330468351755826, 312.3793289830200592, -7.753281021820742858 ) ) ;
#80062 = DIRECTION ( 'NONE',  ( -1.000000000000000000, -0.000000000000000000, -0.000000000000000000 ) ) ;
#80063 = ORIENTED_EDGE ( 'NONE', *, *, #102731, .F. ) ;
#80064 = AXIS2_PLACEMENT_3D ( 'NONE', #95894, #54875, #5292 ) ;
#80065 = PLANE ( 'NONE',  #38921 ) ;
#80066 = CARTESIAN_POINT ( 'NONE',  ( 20.59999999999999787, 1.533819458162526451E-15, 0.000000000000000000 ) ) ;
#80068 = CARTESIAN_POINT ( 'NONE',  ( -105.2601448406410327, -52.71030778888786728, 170.4775048412932961 ) ) ;
#80067 = LINE ( 'NONE', #88180, #77669 ) ;
#80069 = CARTESIAN_POINT ( 'NONE',  ( 7.188101187500000044, -20.65625000204838813, 0.000000000000000000 ) ) ;
#80070 = CARTESIAN_POINT ( 'NONE',  ( 11.08349330513380515, 1.593028355512270962E-15, 0.000000000000000000 ) ) ;
#80071 = AXIS2_PLACEMENT_3D ( 'NONE', #59043, #9390, #52524 ) ;
#80072 = CARTESIAN_POINT ( 'NONE',  ( -8.000000000000000000, -23.84374999999999645, -3.313708498984762496 ) ) ;
#80073 = FACE_OUTER_BOUND ( 'NONE', #84091, .T. ) ;
#80074 = DIRECTION ( 'NONE',  ( 0.000000000000000000, -1.000000000000000000, 0.000000000000000000 ) ) ;
#80075 = FILL_AREA_STYLE ('',( #88188 ) ) ;
#80076 = ORIENTED_EDGE ( 'NONE', *, *, #64377, .F. ) ;
#80077 = CARTESIAN_POINT ( 'NONE',  ( 43.03987588564147160, 486.0760633267551611, 5.817066388975991487 ) ) ;
#80079 = CARTESIAN_POINT ( 'NONE',  ( 25.30379516431261067, -18.61089036987345224, 28.23902632360290355 ) ) ;
#80078 = DIRECTION ( 'NONE',  ( 0.000000000000000000, -1.000000000000000000, 0.000000000000000000 ) ) ;
#80080 = CARTESIAN_POINT ( 'NONE',  ( 23.29983671023130398, 28.09898118347550877, -30.70617127781076405 ) ) ;
#80081 = ORIENTED_EDGE ( 'NONE', *, *, #99080, .F. ) ;
#80082 = EDGE_CURVE ( 'NONE', #63169, #72949, #13837, .T. ) ;
#80083 = VERTEX_POINT ( 'NONE', #29036 ) ;
#80085 = CARTESIAN_POINT ( 'NONE',  ( -0.1697841580037205145, 43.17852052592515832, -18.74127414289921845 ) ) ;
#80084 = CARTESIAN_POINT ( 'NONE',  ( 16.84999999999999787, 1.533819458162526451E-15, 0.000000000000000000 ) ) ;
#80086 = DIRECTION ( 'NONE',  ( 0.000000000000000000, 1.000000000000000000, 0.000000000000000000 ) ) ;
#80087 = DIRECTION ( 'NONE',  ( 0.000000000000000000, 1.000000000000000000, 0.000000000000000000 ) ) ;
#80088 = CARTESIAN_POINT ( 'NONE',  ( 6.645597273868374621, 41.91296976309556044, -68.91429206532015428 ) ) ;
#80089 = CARTESIAN_POINT ( 'NONE',  ( 6.249999999999998224, 4.618802153517001408, -8.000000000000000000 ) ) ;
#80090 = CARTESIAN_POINT ( 'NONE',  ( 6.692326732991420724E-21, 18.87382441218278828, -49.25000000000000000 ) ) ;
#80091 = ORIENTED_EDGE ( 'NONE', *, *, #103398, .T. ) ;
#80092 = EDGE_CURVE ( 'NONE', #96238, #20513, #13307, .T. ) ;
#80093 = DIRECTION ( 'NONE',  ( 0.000000000000000000, -0.8363101477004211137, 0.5482566341169980983 ) ) ;
#80094 = CARTESIAN_POINT ( 'NONE',  ( 21.96352229986338145, 25.92428843650098358, -31.83062960408818753 ) ) ;
#80095 = CARTESIAN_POINT ( 'NONE',  ( -11.27547330588923913, 20.00714579501138246, 8.438865621785792470 ) ) ;
#80096 = CARTESIAN_POINT ( 'NONE',  ( 7.500000000000001776, -4.330127018922199866, -0.9999999999999974465 ) ) ;
#80097 = CARTESIAN_POINT ( 'NONE',  ( -6.062025480882868855, -5.000000000000000000, -74.52240934977429276 ) ) ;
#80098 =( BOUNDED_SURFACE ( )  B_SPLINE_SURFACE ( 3, 2, ( 
 ( #63919, #71989, #45610 ),
 ( #31039, #96806, #22937 ),
 ( #88710, #80597, #6718 ),
 ( #72514, #105420, #94700 ),
 ( #53679, #86613, #12678 ),
 ( #33147, #106463, #24533 ),
 ( #40674, #64443, #182 ),
 ( #89773, #24007, #15875 ),
 ( #7770, #42263, #32621 ),
 ( #82733, #8835, #50348 ) ),
 .UNSPECIFIED., .F., .F., .F. ) 
 B_SPLINE_SURFACE_WITH_KNOTS ( ( 4, 2, 2, 2, 4 ),
 ( 3, 3 ),
 ( 9.697104230710351658E-16, 0.002793818337083670434, 0.003492272921354345507, 0.004190727505625021013, 0.005587636674166371158 ),
 ( 0.000000000000000000, 1.000000000000000000 ),
 .UNSPECIFIED. ) 
 GEOMETRIC_REPRESENTATION_ITEM ( )  RATIONAL_B_SPLINE_SURFACE ( (
 ( 1.000000000000000000, 0.8239349643288951253, 1.000000000000000000),
 ( 1.000000000000000000, 0.8395566633234762266, 1.000000000000000000),
 ( 1.000000000000000000, 0.8448327636285400954, 1.000000000000000000),
 ( 1.000000000000000000, 0.8449253468988903171, 1.000000000000000000),
 ( 1.000000000000000000, 0.8445754865264456512, 1.000000000000000000),
 ( 1.000000000000000000, 0.8431693930248722602, 1.000000000000000000),
 ( 1.000000000000000000, 0.8421154100732993752, 1.000000000000000000),
 ( 1.000000000000000000, 0.8378581409665019075, 1.000000000000000000),
 ( 1.000000000000000000, 0.8335888548700695067, 1.000000000000000000),
 ( 1.000000000000000000, 0.8273155905870500648, 1.000000000000000000) ) ) 
 REPRESENTATION_ITEM ( '' )  SURFACE ( )  );
#80099 = CARTESIAN_POINT ( 'NONE',  ( -43.00000000000000000, 437.9690125970932399, 14.09127711025710639 ) ) ;
#80100 = EDGE_CURVE ( 'NONE', #71336, #65536, #36672, .T. ) ;
#80101 = ORIENTED_EDGE ( 'NONE', *, *, #33515, .F. ) ;
#80102 = CARTESIAN_POINT ( 'NONE',  ( -52.56483885390523625, 40.83906611473335602, -38.23529411764706509 ) ) ;
#80103 = VERTEX_POINT ( 'NONE', #48850 ) ;
#80104 = ORIENTED_EDGE ( 'NONE', *, *, #39428, .T. ) ;
#80105 = CARTESIAN_POINT ( 'NONE',  ( 0.3378883892481922002, 54.29263816026539047, 7.785150801134277820 ) ) ;
#80106 = DIRECTION ( 'NONE',  ( 1.000000000000000000, 0.000000000000000000, 0.000000000000000000 ) ) ;
#80107 = CARTESIAN_POINT ( 'NONE',  ( 41.08349330513380693, 1.593028355512270567E-15, 0.000000000000000000 ) ) ;
#80108 = CARTESIAN_POINT ( 'NONE',  ( 26.15315386302562928, 305.7446874650615882, 10.59157493570054775 ) ) ;
#80109 = CARTESIAN_POINT ( 'NONE',  ( -3.313708498984765161, -16.15625000409677270, 7.999999999999998224 ) ) ;
#80110 = DIRECTION ( 'NONE',  ( 0.2266275398148295539, 0.09415776302337237891, 0.9694195551255979648 ) ) ;
#80111 = CARTESIAN_POINT ( 'NONE',  ( -46.00000000000000000, 488.0336798547362491, -0.8984331811837963366 ) ) ;
#80112 = CARTESIAN_POINT ( 'NONE',  ( 0.05613245601036612881, 1.278525034529252924, -6.499999999999999112 ) ) ;
#80113 = ORIENTED_EDGE ( 'NONE', *, *, #45887, .F. ) ;
#80114 = CARTESIAN_POINT ( 'NONE',  ( 1.224646799147352073E-15, 49.99999999999999289, -75.00000000000001421 ) ) ;
#80115 = ORIENTED_EDGE ( 'NONE', *, *, #73346, .F. ) ;
#80116 = DIRECTION ( 'NONE',  ( 0.000000000000000000, 0.000000000000000000, 1.000000000000000000 ) ) ;
#80117 = CARTESIAN_POINT ( 'NONE',  ( 0.000000000000000000, 294.8518027762758038, 9.936999415352289589 ) ) ;
#80118 = CARTESIAN_POINT ( 'NONE',  ( -40.38854417759198157, 485.1419806746749828, -4.245955111568370022 ) ) ;
#80119 = CARTESIAN_POINT ( 'NONE',  ( 0.000000000000000000, 294.8518027762758038, -10.00000000000000178 ) ) ;
#80120 = CARTESIAN_POINT ( 'NONE',  ( 62.87606824768278102, -36.00767307724900945, 78.31049006666825107 ) ) ;
#80121 = CIRCLE ( 'NONE', #100990, 3.309500000000001663 ) ;
#80122 = ORIENTED_EDGE ( 'NONE', *, *, #17425, .F. ) ;
#80123 = CARTESIAN_POINT ( 'NONE',  ( 40.62716977365077042, 464.4319289640043849, 17.32222667058900001 ) ) ;
#80124 = CARTESIAN_POINT ( 'NONE',  ( -33.00000000000000000, 450.0000000000002274, 28.20242257375372219 ) ) ;
#80125 = DIRECTION ( 'NONE',  ( 0.8191520442889974607, 1.003171929053531649E-16, -0.5735764363510379438 ) ) ;
#80126 = ADVANCED_FACE ( 'NONE', ( #49385 ), #41308, .T. ) ;
#80127 = VECTOR ( 'NONE', #95647, 1000.000000000000000 ) ;
#80128 = EDGE_LOOP ( 'NONE', ( #33916, #15398, #7020, #69905 ) ) ;
#80129 = CARTESIAN_POINT ( 'NONE',  ( 46.78679791479564898, 18.82552674760553657, 15.44534812371287913 ) ) ;
#80130 = CIRCLE ( 'NONE', #99060, 3.309500000000007880 ) ;
#80131 = ADVANCED_FACE ( 'NONE', ( #73664 ), #61547, .F. ) ;
#80132 = DIRECTION ( 'NONE',  ( 1.000000000000000000, 1.224606353822377258E-16, 0.000000000000000000 ) ) ;
#80133 = CARTESIAN_POINT ( 'NONE',  ( 3.313708498984762496, -30.96875000409677980, 7.999999999999998224 ) ) ;
#80134 = AXIS2_PLACEMENT_3D ( 'NONE', #89788, #81661, #63412 ) ;
#80135 = CARTESIAN_POINT ( 'NONE',  ( 2.094395098902661623, -3.000000000000000000, 8.000000000000000000 ) ) ;
#80136 = VECTOR ( 'NONE', #106301, 1000.000000000000114 ) ;
#80137 = CARTESIAN_POINT ( 'NONE',  ( 86.58291375612756724, -50.12654805533016855, 191.4789541590376984 ) ) ;
#80138 = CIRCLE ( 'NONE', #30195, 4.000000000000000000 ) ;
#80139 = CARTESIAN_POINT ( 'NONE',  ( 85.31310517497098544, -5.000000000000000000, 6.123233995736778115E-16 ) ) ;
#80140 = UNCERTAINTY_MEASURE_WITH_UNIT (LENGTH_MEASURE( 1.000000000000000082E-05 ), #103368, 'distance_accuracy_value', 'NONE');
#80141 = CARTESIAN_POINT ( 'NONE',  ( -9.946294137122949408, 7.586021176442817371, 0.000000000000000000 ) ) ;
#80142 = FILL_AREA_STYLE ('',( #62925 ) ) ;
#80143 = ADVANCED_FACE ( 'NONE', ( #39731 ), #56942, .T. ) ;
#80144 = CARTESIAN_POINT ( 'NONE',  ( 15.72108712621133186, 304.5560400716026379, 9.874133111316416134 ) ) ;
#80145 = ORIENTED_EDGE ( 'NONE', *, *, #98938, .F. ) ;
#80146 = LINE ( 'NONE', #50423, #28194 ) ;
#80147 = CARTESIAN_POINT ( 'NONE',  ( -4.912112805545315375, -10.03270266009703526, 6.401595693439444901 ) ) ;
#80148 = AXIS2_PLACEMENT_3D ( 'NONE', #98697, #15665, #81448 ) ;
#80149 = CARTESIAN_POINT ( 'NONE',  ( 26.06770421271730953, -59.99999999999999289, 41.47426653923610473 ) ) ;
#80150 = CARTESIAN_POINT ( 'NONE',  ( -97.62704972254648794, -30.00000000000000711, 134.9237959675543550 ) ) ;
#80151 = CARTESIAN_POINT ( 'NONE',  ( 0.000000000000000000, 273.9999999999999432, 0.000000000000000000 ) ) ;
#80152 = CARTESIAN_POINT ( 'NONE',  ( 41.16726445008557533, -57.68949799089449471, 57.63647873290717172 ) ) ;
#80154 = CARTESIAN_POINT ( 'NONE',  ( 43.35041983546129529, 465.4837887079268057, 10.07799631932362239 ) ) ;
#80153 = CARTESIAN_POINT ( 'NONE',  ( 13.69035467268384032, 7.353514859321120589, -8.258215124936253204 ) ) ;
#80155 = CARTESIAN_POINT ( 'NONE',  ( -17.51806903888139644, 50.00000000000000711, 63.24379045937951815 ) ) ;
#80156 = CYLINDRICAL_SURFACE ( 'NONE', #53018, 1.250000000000001110 ) ;
#80157 = FILL_AREA_STYLE ('',( #40761 ) ) ;
#80158 = CARTESIAN_POINT ( 'NONE',  ( -17.68517609946639979, -60.00000000000001421, 39.97351463475433064 ) ) ;
#80159 = B_SPLINE_CURVE_WITH_KNOTS ( 'NONE', 3,
 ( #2408, #45025, #101652, #85475, #18087, #50948 ),
 .UNSPECIFIED., .F., .F.,
 ( 4, 2, 4 ),
 ( 0.02053414304140307317, 0.03170133459815401011, 0.04286852615490495400 ),
 .UNSPECIFIED. ) ;
#80160 = CARTESIAN_POINT ( 'NONE',  ( 3.807551310283626034, -15.50932548558135693, -35.16743972384818306 ) ) ;
#80161 = DIRECTION ( 'NONE',  ( 0.000000000000000000, 0.000000000000000000, 1.000000000000000000 ) ) ;
#80162 = VERTEX_POINT ( 'NONE', #56409 ) ;
#80163 = CARTESIAN_POINT ( 'NONE',  ( 35.05202888951401263, 439.1669932502342135, 24.09215602862335004 ) ) ;
#80164 = CARTESIAN_POINT ( 'NONE',  ( -15.36525660533068205, -22.06900397672482939, 27.72757744622246534 ) ) ;
#80166 = SURFACE_STYLE_USAGE ( .BOTH. , #105513 ) ;
#80165 = CARTESIAN_POINT ( 'NONE',  ( -105.0449526092814665, -60.00000000000002842, 150.2760437015073478 ) ) ;
#80167 = EDGE_CURVE ( 'NONE', #51961, #35975, #33201, .T. ) ;
#80168 = ORIENTED_EDGE ( 'NONE', *, *, #13698, .T. ) ;
#80169 = CARTESIAN_POINT ( 'NONE',  ( 26.78389989157783191, 34.86784115625223990, 7.588158416758067126 ) ) ;
#80170 = CARTESIAN_POINT ( 'NONE',  ( 16.05785784214673129, 4.775831776474257495, -3.710403933782447261 ) ) ;
#80171 = DIRECTION ( 'NONE',  ( 0.000000000000000000, 1.000000000000000000, 0.000000000000000000 ) ) ;
#80172 = EDGE_CURVE ( 'NONE', #24268, #55179, #65463, .T. ) ;
#80173 = CARTESIAN_POINT ( 'NONE',  ( 8.061685236282825271E-09, -15.39512265162600535, -35.22781471665102515 ) ) ;
#80174 = CARTESIAN_POINT ( 'NONE',  ( 16.05785784214651812, 4.775831776474217527, -3.710403933782383756 ) ) ;
#80175 = CARTESIAN_POINT ( 'NONE',  ( 57.96890702122141192, -60.00000000000000000, 94.09620601737630352 ) ) ;
#80176 = CARTESIAN_POINT ( 'NONE',  ( 0.000000000000000000, 10.71892156097790583, 14.93965356295127478 ) ) ;
#80177 = ORIENTED_EDGE ( 'NONE', *, *, #65157, .T. ) ;
#80178 = FACE_OUTER_BOUND ( 'NONE', #74196, .T. ) ;
#80179 = DIRECTION ( 'NONE',  ( 1.000000000000000000, 0.000000000000000000, 0.000000000000000000 ) ) ;
#80181 = CARTESIAN_POINT ( 'NONE',  ( 7.150000000000005684, 41.64999999999999147, -68.91429206202190016 ) ) ;
#80180 = CARTESIAN_POINT ( 'NONE',  ( 1.295095875561511761E-05, -30.00000000000000000, 37.00000000000000711 ) ) ;
#80182 = CARTESIAN_POINT ( 'NONE',  ( 4.225138137263999560, -1.061190178712521082, 104.4756818702664134 ) ) ;
#80183 =( NAMED_UNIT ( * ) SI_UNIT ( $, .STERADIAN. ) SOLID_ANGLE_UNIT ( ) );
#80184 = ORIENTED_EDGE ( 'NONE', *, *, #14417, .T. ) ;
#80185 = VECTOR ( 'NONE', #54137, 1000.000000000000000 ) ;
#80186 = CARTESIAN_POINT ( 'NONE',  ( -25.89661693312760349, 307.0966920204201642, 10.68061420533875250 ) ) ;
#80187 = ORIENTED_EDGE ( 'NONE', *, *, #74999, .T. ) ;
#80188 = CARTESIAN_POINT ( 'NONE',  ( 20.08142311587312179, 304.8415473682318861, 8.934819560836576358 ) ) ;
#80189 = FACE_BOUND ( 'NONE', #31448, .T. ) ;
#80190 = FILL_AREA_STYLE_COLOUR ( '', #22696 ) ;
#80191 = ORIENTED_EDGE ( 'NONE', *, *, #73202, .T. ) ;
#80192 = EDGE_CURVE ( 'NONE', #77294, #77299, #8633, .T. ) ;
#80193 = CARTESIAN_POINT ( 'NONE',  ( -1.724765290377670013, -5.000000000000002665, -69.73714729960835257 ) ) ;
#80194 = CARTESIAN_POINT ( 'NONE',  ( 5.000000000000000888, -12.24669057839810371, 9.804025467456250809 ) ) ;
#80195 = CARTESIAN_POINT ( 'NONE',  ( -97.86455770250910291, -60.00000000002447820, 204.8732123382124826 ) ) ;
#80196 = CARTESIAN_POINT ( 'NONE',  ( 5.980073869852059687, 2.767359234582687844, -6.500000000000000888 ) ) ;
#80197 = CARTESIAN_POINT ( 'NONE',  ( 80.95387373043369905, -60.00000000000000000, 197.0855688607617822 ) ) ;
#80198 = CARTESIAN_POINT ( 'NONE',  ( 0.6420822604574439874, 26.01275107339925086, -38.42434469679283637 ) ) ;
#80199 = PRESENTATION_LAYER_ASSIGNMENT (  '', '', ( #42327 ) ) ;
#80201 = CARTESIAN_POINT ( 'NONE',  ( 10.12131235883916958, -25.54850865871655330, 28.15731131281348709 ) ) ;
#80200 = CARTESIAN_POINT ( 'NONE',  ( -109.5811972119284690, -29.99999999999999289, 174.3366342583755113 ) ) ;
#80202 = CARTESIAN_POINT ( 'NONE',  ( 82.50885711773439368, -37.99999999999995737, 16.62692665718585516 ) ) ;
#80203 = CARTESIAN_POINT ( 'NONE',  ( -45.04059857025013969, -60.25991841825150175, 49.29949777491053453 ) ) ;
#80204 = CARTESIAN_POINT ( 'NONE',  ( 6.124999999999403144, -61.77251097506463395, 14.41094225130382078 ) ) ;
#80205 = VECTOR ( 'NONE', #27747, 999.9999999999998863 ) ;
#80206 = VERTEX_POINT ( 'NONE', #105512 ) ;
#80207 = CIRCLE ( 'NONE', #49249, 4.172000000000001485 ) ;
#80208 = FACE_OUTER_BOUND ( 'NONE', #52927, .T. ) ;
#80209 = AXIS2_PLACEMENT_3D ( 'NONE', #24378, #49125, #82576 ) ;
#80210 =( NAMED_UNIT ( * ) PLANE_ANGLE_UNIT ( ) SI_UNIT ( $, .RADIAN. ) );
#80211 = CARTESIAN_POINT ( 'NONE',  ( 1.262177448353618889E-25, 303.8518027762758038, -10.00000000000000533 ) ) ;
#80212 = CARTESIAN_POINT ( 'NONE',  ( 37.56673239365870387, -1.200000000000000030E-05, 13.45617127780999134 ) ) ;
#80213 = ORIENTED_EDGE ( 'NONE', *, *, #44161, .F. ) ;
#80214 = CARTESIAN_POINT ( 'NONE',  ( -7.369570678962171328, -14.99279962711093361, 15.08387202298855811 ) ) ;
#80215 = ORIENTED_EDGE ( 'NONE', *, *, #74483, .F. ) ;
#80216 = CARTESIAN_POINT ( 'NONE',  ( 107.8908516830521336, -30.00000000000169820, 188.9791561279670873 ) ) ;
#80217 = SURFACE_SIDE_STYLE ('',( #29596 ) ) ;
#80218 = CARTESIAN_POINT ( 'NONE',  ( 6.583804726435484866, 41.87230891639573116, -59.35876464016742915 ) ) ;
#80219 =( LENGTH_UNIT ( ) NAMED_UNIT ( * ) SI_UNIT ( .MILLI., .METRE. ) );
#80220 = CARTESIAN_POINT ( 'NONE',  ( 90.49494987202336915, -30.00000000000000355, 91.38635056579792604 ) ) ;
#80221 = CARTESIAN_POINT ( 'NONE',  ( 38.47428897412612514, 484.8307741943459632, -5.088672563358043632 ) ) ;
#80222 = ADVANCED_FACE ( 'NONE', ( #40244 ), #31653, .T. ) ;
#80223 = VERTEX_POINT ( 'NONE', #15435 ) ;
#80224 = ORIENTED_EDGE ( 'NONE', *, *, #50497, .F. ) ;
#80225 = ORIENTED_EDGE ( 'NONE', *, *, #78451, .T. ) ;
#80226 = CARTESIAN_POINT ( 'NONE',  ( 41.08349330513380693, 1.593028355512270567E-15, 0.000000000000000000 ) ) ;
#80227 = LINE ( 'NONE', #54887, #98971 ) ;
#80228 = DIRECTION ( 'NONE',  ( -1.000000000000000000, 0.000000000000000000, 0.000000000000000000 ) ) ;
#80229 = ORIENTED_EDGE ( 'NONE', *, *, #97831, .T. ) ;
#80230 = DIRECTION ( 'NONE',  ( 0.000000000000000000, -1.000000000000000000, 0.000000000000000000 ) ) ;
#80231 = ORIENTED_EDGE ( 'NONE', *, *, #67786, .F. ) ;
#80232 = CARTESIAN_POINT ( 'NONE',  ( 19.83349330513379982, -4.000000000000000000, 4.898587196589415787E-16 ) ) ;
#80233 = CARTESIAN_POINT ( 'NONE',  ( 94.14369787774502640, -38.49202524632631395, 201.1992593668043412 ) ) ;
#80234 = DIRECTION ( 'NONE',  ( 0.000000000000000000, -1.000000000000000000, 0.000000000000000000 ) ) ;
#80235 = CARTESIAN_POINT ( 'NONE',  ( 84.47908901077074972, -45.28586178760942005, -7.723303808647219881 ) ) ;
#80236 = CARTESIAN_POINT ( 'NONE',  ( 84.84573287372256800, -38.00000000000007816, 182.0739377323602071 ) ) ;
#80237 = CARTESIAN_POINT ( 'NONE',  ( 37.52740353635520165, 308.4545598930066035, 5.153891583661067699 ) ) ;
#80238 = CARTESIAN_POINT ( 'NONE',  ( 23.73746414932995208, 1.482358050883964840E-15, 0.000000000000000000 ) ) ;
#80239 =( GEOMETRIC_REPRESENTATION_CONTEXT ( 3 ) GLOBAL_UNCERTAINTY_ASSIGNED_CONTEXT ( ( #2750 ) ) GLOBAL_UNIT_ASSIGNED_CONTEXT ( ( #102451, #86817, #52831 ) ) REPRESENTATION_CONTEXT ( 'NONE', 'WORKASPACE' ) );
#80240 = CYLINDRICAL_SURFACE ( 'NONE', #52383, 3.400000000000000355 ) ;
#80241 = ORIENTED_EDGE ( 'NONE', *, *, #75151, .T. ) ;
#80242 = CARTESIAN_POINT ( 'NONE',  ( 32.62396605173337605, 486.1273723460453766, 7.520682129464227650 ) ) ;
#80243 = EDGE_CURVE ( 'NONE', #101726, #1493, #53451, .T. ) ;
#80244 = CARTESIAN_POINT ( 'NONE',  ( -33.21566647566201880, 463.2601667903500129, 6.161217084504481356 ) ) ;
#80245 = CARTESIAN_POINT ( 'NONE',  ( -3.548074437533462078, 24.62734600915379701, 4.999999999999998224 ) ) ;
#80246 = EDGE_LOOP ( 'NONE', ( #9375, #75824, #76383, #34471, #48810, #85681 ) ) ;
#80247 = CARTESIAN_POINT ( 'NONE',  ( -42.10086803841213765, 435.6552064019012960, 19.95582312411055881 ) ) ;
#80248 = CARTESIAN_POINT ( 'NONE',  ( -31.40680613098830420, 299.6578337794886124, 11.01686700637052674 ) ) ;
#80249 = CARTESIAN_POINT ( 'NONE',  ( 7.482513037750662122, 54.13169591394895974, -3.436679040787894657 ) ) ;
#80250 = CARTESIAN_POINT ( 'NONE',  ( -14.91858118607497019, 1.255821567010171884E-17, 15.00000000000000000 ) ) ;
#80251 = CARTESIAN_POINT ( 'NONE',  ( -5.656854249492381470, -16.06249999999999289, 5.656854249492379694 ) ) ;
#80252 = CARTESIAN_POINT ( 'NONE',  ( -20.45424608527195787, -19.94684262238009254, 35.83346515895529905 ) ) ;
#80253 = EDGE_CURVE ( 'NONE', #86116, #75985, #5194, .T. ) ;
#80254 = CARTESIAN_POINT ( 'NONE',  ( 13.22944098689769632, 303.5546580367862930, 9.873837682497947910 ) ) ;
#80255 = EDGE_LOOP ( 'NONE', ( #88277, #68981, #7268, #83408, #68745 ) ) ;
#80256 = CARTESIAN_POINT ( 'NONE',  ( 84.39531239231617121, -50.17912663769864423, 187.9369569292725544 ) ) ;
#80257 = CARTESIAN_POINT ( 'NONE',  ( 6.643884894376899553, -7.802125718944354027, -9.232358214956412824E-13 ) ) ;
#80258 = AXIS2_PLACEMENT_3D ( 'NONE', #46741, #13829, #94379 ) ;
#80259 = CARTESIAN_POINT ( 'NONE',  ( 3.801077171203084859, -1.110903940591797756, 104.1059035333591112 ) ) ;
#80260 = VERTEX_POINT ( 'NONE', #76325 ) ;
#80261 = CARTESIAN_POINT ( 'NONE',  ( 93.89123455727428791, -57.67342034595336742, 16.20923714071724575 ) ) ;
#80262 = EDGE_CURVE ( 'NONE', #71046, #78613, #48270, .T. ) ;
#80263 = CARTESIAN_POINT ( 'NONE',  ( 35.52295374289817431, 436.6489517640840177, 4.915275271775414012 ) ) ;
#80264 = CARTESIAN_POINT ( 'NONE',  ( 30.00000000000000000, 0.000000000000000000, 0.000000000000000000 ) ) ;
#80265 = CARTESIAN_POINT ( 'NONE',  ( 28.88581594204435632, 13.70410095367685877, 39.88976374582048834 ) ) ;
#80266 = AXIS2_PLACEMENT_3D ( 'NONE', #18753, #59185, #92063 ) ;
#80267 = CONICAL_SURFACE ( 'NONE', #64805, 3.309500000000001663, 0.9599310885968770357 ) ;
#80268 = CARTESIAN_POINT ( 'NONE',  ( 29.09632818934771947, 14.54213905807124441, 41.96777332363164703 ) ) ;
#80269 = CARTESIAN_POINT ( 'NONE',  ( 2.094395098902661623, -3.000000000000000000, 8.000000000000000000 ) ) ;
#80270 = DIRECTION ( 'NONE',  ( -1.000000000000000000, 0.000000000000000000, 0.000000000000000000 ) ) ;
#80272 = DIRECTION ( 'NONE',  ( 0.5735764363510440500, 0.8191520442889932418, 0.000000000000000000 ) ) ;
#80271 = DIRECTION ( 'NONE',  ( -1.000000000000000000, -1.224606353822377258E-16, -0.000000000000000000 ) ) ;
#80273 = CARTESIAN_POINT ( 'NONE',  ( 9.297673743008640912, 295.3592874400322899, -10.03978397955114588 ) ) ;
#80274 = AXIS2_PLACEMENT_3D ( 'NONE', #82824, #42362, #8923 ) ;
#80275 = CARTESIAN_POINT ( 'NONE',  ( -15.82358155159817947, 44.01628288912645814, -4.460636615200937349 ) ) ;
#80276 = LINE ( 'NONE', #69692, #99339 ) ;
#80277 = CARTESIAN_POINT ( 'NONE',  ( 9.926810856659445292, 15.46725112412266512, -1.404490565848973027 ) ) ;
#80278 = FACE_OUTER_BOUND ( 'NONE', #26838, .T. ) ;
#80279 = AXIS2_PLACEMENT_3D ( 'NONE', #75869, #870, #100671 ) ;
#80280 = COLOUR_RGB ( '', 0.72549020, 0.75294118, 0.79215686) ;
#80281 = CARTESIAN_POINT ( 'NONE',  ( -82.46010706263061252, -37.99999999999999289, -12.85786253404099000 ) ) ;
#80282 = VERTEX_POINT ( 'NONE', #56064 ) ;
#80283 = SURFACE_STYLE_FILL_AREA ( #88405 ) ;
#80284 = LINE ( 'NONE', #5869, #14237 ) ;
#80285 = CARTESIAN_POINT ( 'NONE',  ( -3.762156792001841055, -15.48433094664021503, -35.17833216663523643 ) ) ;
#80287 = CARTESIAN_POINT ( 'NONE',  ( -44.04665276855927658, -34.58949255706212966, -28.87972264604723094 ) ) ;
#80286 = CARTESIAN_POINT ( 'NONE',  ( 0.000000000000000000, -19.99999999999998934, 0.000000000000000000 ) ) ;
#80288 = ADVANCED_FACE ( 'NONE', ( #14029 ), #46522, .F. ) ;
#80289 = ORIENTED_EDGE ( 'NONE', *, *, #37992, .F. ) ;
#80290 = CARTESIAN_POINT ( 'NONE',  ( 2.411464220262822256, 7.267994521134540697, -7.491772860716854332 ) ) ;
#80291 = ORIENTED_EDGE ( 'NONE', *, *, #86004, .F. ) ;
#80292 = ADVANCED_FACE ( 'NONE', ( #73321 ), #48521, .T. ) ;
#80293 = EDGE_CURVE ( 'NONE', #15625, #86664, #88115, .T. ) ;
#80294 = CARTESIAN_POINT ( 'NONE',  ( 0.2578475836320693881, 4.367703157927328661, -5.434916218090833695 ) ) ;
#80295 = DIRECTION ( 'NONE',  ( 0.000000000000000000, 0.000000000000000000, -1.000000000000000000 ) ) ;
#80296 = CARTESIAN_POINT ( 'NONE',  ( -92.66085178039205061, -59.99999999999997868, -3.913123054519065391 ) ) ;
#80297 = ORIENTED_EDGE ( 'NONE', *, *, #61492, .T. ) ;
#80298 = CARTESIAN_POINT ( 'NONE',  ( 22.67522056483525006, -27.32510663572569598, -30.38798232809733690 ) ) ;
#80299 = CARTESIAN_POINT ( 'NONE',  ( -9.701736001019305888, 15.75130202679985914, 2.450449656239128693 ) ) ;
#80300 = CARTESIAN_POINT ( 'NONE',  ( 97.87950285349613466, -37.74667525479749486, 192.5555229186351767 ) ) ;
#80301 = CARTESIAN_POINT ( 'NONE',  ( 15.17407431220850533, 6.123233995736770227E-16, -5.000000000000002665 ) ) ;
#80302 = CARTESIAN_POINT ( 'NONE',  ( -80.66628790925550163, -53.40400959498802536, 170.0955033780085444 ) ) ;
#80303 = ORIENTED_EDGE ( 'NONE', *, *, #28525, .F. ) ;
#80304 = ORIENTED_EDGE ( 'NONE', *, *, #67138, .F. ) ;
#80305 = AXIS2_PLACEMENT_3D ( 'NONE', #63248, #78879, #88574 ) ;
#80306 = EDGE_LOOP ( 'NONE', ( #39412, #68078, #18462, #20120 ) ) ;
#80307 = CARTESIAN_POINT ( 'NONE',  ( 34.15310232806822910, 465.0579147271382681, 17.72315479633545010 ) ) ;
#80308 = CARTESIAN_POINT ( 'NONE',  ( -5.000000000000079936, -12.24669057839772535, 9.804025467455284470 ) ) ;
#80309 = DIRECTION ( 'NONE',  ( -0.5735764363510497121, 0.8191520442889892450, 1.003171929053521665E-16 ) ) ;
#80310 = ORIENTED_EDGE ( 'NONE', *, *, #76070, .F. ) ;
#80311 = EDGE_CURVE ( 'NONE', #85998, #92028, #79309, .T. ) ;
#80312 = CYLINDRICAL_SURFACE ( 'NONE', #83986, 4.000000000000000000 ) ;
#80313 = CARTESIAN_POINT ( 'NONE',  ( -76.77372030740811226, -57.52889592737719227, 194.6762175334667972 ) ) ;
#80314 = CARTESIAN_POINT ( 'NONE',  ( 3.105145020734076500, -49.42984310587327457, 103.2828773998820395 ) ) ;
#80315 = CARTESIAN_POINT ( 'NONE',  ( 0.5619217318086660029, 7.564468822943315018, -6.443866470201766283 ) ) ;
#80316 = CARTESIAN_POINT ( 'NONE',  ( -1.100444924853492656, 25.84109709204356520, 38.88573747810594483 ) ) ;
#80317 = CARTESIAN_POINT ( 'NONE',  ( 11.08349330513380160, -4.000000000000000888, 4.898587196589416773E-16 ) ) ;
#80318 = CARTESIAN_POINT ( 'NONE',  ( -53.63968661800659277, -29.99999999999997158, -34.46705067659466692 ) ) ;
#80319 = ADVANCED_FACE ( 'NONE', ( #63681 ), #46403, .T. ) ;
#80320 = CARTESIAN_POINT ( 'NONE',  ( -57.26243271903199172, -29.99999999999990763, 83.64903429017334702 ) ) ;
#80321 = CARTESIAN_POINT ( 'NONE',  ( -52.16595314293665098, -46.44255072620141789, 57.11458137737905361 ) ) ;
#80322 = ORIENTED_EDGE ( 'NONE', *, *, #40628, .F. ) ;
#80323 = CARTESIAN_POINT ( 'NONE',  ( 4.699999999999999289, -5.629165124598843661, 3.250000000000010658 ) ) ;
#80324 = ORIENTED_EDGE ( 'NONE', *, *, #26573, .T. ) ;
#80325 = CARTESIAN_POINT ( 'NONE',  ( -99.99287224920719552, -45.25595435666994604, 192.6068234404419570 ) ) ;
#80326 =( REPRESENTATION_RELATIONSHIP ('NONE','NONE', #69581, #63931 ) REPRESENTATION_RELATIONSHIP_WITH_TRANSFORMATION ( #91318 )SHAPE_REPRESENTATION_RELATIONSHIP( ) );
#80327 = CARTESIAN_POINT ( 'NONE',  ( -30.55657801806768603, 16.37492758275029914, -39.95287151819763238 ) ) ;
#80328 = EDGE_LOOP ( 'NONE', ( #25549, #25991, #97203, #38882, #43462 ) ) ;
#80329 = CARTESIAN_POINT ( 'NONE',  ( 19.02338435704004027, 49.55559105460935854, 61.87204836851903167 ) ) ;
#80331 = STYLED_ITEM ( 'NONE', ( #71920 ), #65823 ) ;
#80330 = B_SPLINE_CURVE_WITH_KNOTS ( 'NONE', 3,
 ( #4278, #55596, #88532, #14611 ),
 .UNSPECIFIED., .F., .F.,
 ( 4, 4 ),
 ( 3.469446951953614189E-18, 0.001900242520396275888 ),
 .UNSPECIFIED. ) ;
#80332 = CARTESIAN_POINT ( 'NONE',  ( 90.65073698084890452, -38.34357974882981779, 8.850807137404535396 ) ) ;
#80333 = DIRECTION ( 'NONE',  ( 0.000000000000000000, -1.000000000000000000, 0.000000000000000000 ) ) ;
#80334 = CARTESIAN_POINT ( 'NONE',  ( 63.07777777777777573, 6.915964383211875250E-15, 0.000000000000000000 ) ) ;
#80335 = CARTESIAN_POINT ( 'NONE',  ( -9.047684060188633026, 302.6745968392543205, 9.899357598522687596 ) ) ;
#80336 = DIRECTION ( 'NONE',  ( -1.000000000000000000, -0.000000000000000000, -0.000000000000000000 ) ) ;
#80337 = CARTESIAN_POINT ( 'NONE',  ( 66.21888218963562167, -30.00000000000000000, 83.75810960045656373 ) ) ;
#80338 = CARTESIAN_POINT ( 'NONE',  ( 32.94330508143927716, 1.340359594676612611E-15, 0.000000000000000000 ) ) ;
#80339 = CARTESIAN_POINT ( 'NONE',  ( 4.447904436602727607, 52.17731337436469374, -6.353523366743629275 ) ) ;
#80340 = DIRECTION ( 'NONE',  ( 1.000000000000000000, 1.224606353822377258E-16, 0.000000000000000000 ) ) ;
#80341 = TOROIDAL_SURFACE ( 'NONE', #94149, 65.50000000000000000, 0.5000000000000000000 ) ;
#80342 = CARTESIAN_POINT ( 'NONE',  ( -33.80014854764822019, 484.1533675815112474, 1.810747741428984314 ) ) ;
#80343 = UNCERTAINTY_MEASURE_WITH_UNIT (LENGTH_MEASURE( 1.000000000000000082E-05 ), #92908, 'distance_accuracy_value', 'NONE');
#80344 = VERTEX_POINT ( 'NONE', #71215 ) ;
#80345 = ORIENTED_EDGE ( 'NONE', *, *, #65477, .T. ) ;
#80346 = CARTESIAN_POINT ( 'NONE',  ( 49.62059425776106281, -39.51416815500159174, 50.13166883492932868 ) ) ;
#80347 = CONICAL_SURFACE ( 'NONE', #101079, 6.500000000000000000, 1.047197551196600296 ) ;
#80348 = CARTESIAN_POINT ( 'NONE',  ( -0.4977218462097728335, 295.8604035916879980, -9.999999999979417353 ) ) ;
#80349 = DIRECTION ( 'NONE',  ( -0.9861333108788029600, -0.1659550938513498497, 8.881784197001250351E-16 ) ) ;
#80350 = CARTESIAN_POINT ( 'NONE',  ( -108.8790446731752724, -38.35654071153614098, 190.5160550575546381 ) ) ;
#80351 = EDGE_LOOP ( 'NONE', ( #7931, #89213, #7473 ) ) ;
#80352 = CARTESIAN_POINT ( 'NONE',  ( 90.76152638017529739, -38.34260793734441108, 6.174342487980118754 ) ) ;
#80353 = CARTESIAN_POINT ( 'NONE',  ( 12.06665022449565150, 19.81138878756394917, -7.337788469117366930 ) ) ;
#80354 = CARTESIAN_POINT ( 'NONE',  ( -7.048357505843686255, 41.75164249415629314, -68.91429205804081448 ) ) ;
#80355 = CARTESIAN_POINT ( 'NONE',  ( 30.00000000000000355, 461.8423776372148950, 11.25810401088899759 ) ) ;
#80356 = CARTESIAN_POINT ( 'NONE',  ( 96.39769212010490662, -37.84852860063914903, 116.1806559511277044 ) ) ;
#80357 =( GEOMETRIC_REPRESENTATION_CONTEXT ( 3 ) GLOBAL_UNCERTAINTY_ASSIGNED_CONTEXT ( ( #61090 ) ) GLOBAL_UNIT_ASSIGNED_CONTEXT ( ( #24212, #33896, #15549 ) ) REPRESENTATION_CONTEXT ( 'NONE', 'WORKASPACE' ) );
#80358 = CARTESIAN_POINT ( 'NONE',  ( 13.45079846400083312, -54.00000000000000711, 23.11721482942554928 ) ) ;
#80359 = AXIS2_PLACEMENT_3D ( 'NONE', #49924, #67195, #100072 ) ;
#80361 = AXIS2_PLACEMENT_3D ( 'NONE', #31414, #32469, #65339 ) ;
#80360 = FACE_OUTER_BOUND ( 'NONE', #84960, .T. ) ;
#80362 = FILL_AREA_STYLE_COLOUR ( '', #103420 ) ;
#80363 = CARTESIAN_POINT ( 'NONE',  ( -32.12566262182737375, 486.1613120233242284, 5.452106427430423174 ) ) ;
#80364 = CARTESIAN_POINT ( 'NONE',  ( 83.25757091423945155, -60.00000000000000711, 199.0109655462719900 ) ) ;
#80365 = CONICAL_SURFACE ( 'NONE', #16709, 4.000000000000000000, 0.9599310885968912466 ) ;
#80366 = VECTOR ( 'NONE', #56536, 1000.000000000000000 ) ;
#80367 = FILL_AREA_STYLE ('',( #21650 ) ) ;
#80368 = ORIENTED_EDGE ( 'NONE', *, *, #899, .F. ) ;
#80369 = CARTESIAN_POINT ( 'NONE',  ( 55.86761055447268376, -36.02599416152285983, 60.76863504461332610 ) ) ;
#80370 = CARTESIAN_POINT ( 'NONE',  ( -33.30612659720004132, 300.4521844812165341, -0.7417152064293228708 ) ) ;
#80371 = CARTESIAN_POINT ( 'NONE',  ( 26.08349330513380693, -3.851859888774471706E-31, 4.000000000000001776 ) ) ;
#80372 = EDGE_CURVE ( 'NONE', #100438, #31665, #9672, .T. ) ;
#80373 = CARTESIAN_POINT ( 'NONE',  ( -7.934996450857311423, 26.13137543527469830, -1.050865690281772569 ) ) ;
#80374 = ORIENTED_EDGE ( 'NONE', *, *, #76773, .T. ) ;
#80375 = EDGE_CURVE ( 'NONE', #3854, #64475, #27632, .T. ) ;
#80377 = CARTESIAN_POINT ( 'NONE',  ( -9.215420734788352775, -53.73283515818290823, 23.11721482942554928 ) ) ;
#80376 = CARTESIAN_POINT ( 'NONE',  ( -104.4634795451426186, -38.40382459815164395, 198.0021900029066444 ) ) ;
#80378 = DIRECTION ( 'NONE',  ( 0.000000000000000000, -1.000000000000000000, 0.000000000000000000 ) ) ;
#80379 = CARTESIAN_POINT ( 'NONE',  ( 22.22078930644830308, 305.3250122787871987, 9.038968116793329344 ) ) ;
#80380 = DIRECTION ( 'NONE',  ( -0.000000000000000000, -0.5482566341170008739, -0.8363101477004192263 ) ) ;
#80381 = CARTESIAN_POINT ( 'NONE',  ( 2.977408999572650927, -10.25000000204838813, -7.188101187500001821 ) ) ;
#80382 = CARTESIAN_POINT ( 'NONE',  ( -5.036189802309444907, -5.000000000000002665, -76.26213611588271135 ) ) ;
#80383 = ADVANCED_FACE ( 'NONE', ( #42435 ), #8866, .T. ) ;
#80384 = EDGE_CURVE ( 'NONE', #30765, #7449, #16142, .T. ) ;
#80385 = CARTESIAN_POINT ( 'NONE',  ( 7.894787914004607998, 1.238680740843649375E-13, -7.591390474663426424 ) ) ;
#80386 = ORIENTED_EDGE ( 'NONE', *, *, #67181, .F. ) ;
#80387 = CARTESIAN_POINT ( 'NONE',  ( 81.16830495754287256, -60.54032804279978563, 184.2195180690823406 ) ) ;
#80388 = CARTESIAN_POINT ( 'NONE',  ( -46.00000000001166711, 463.3768225339526907, 8.978553580135045564 ) ) ;
#80389 = CARTESIAN_POINT ( 'NONE',  ( -35.05548986855151838, 439.9462388155539543, 24.33445361994856526 ) ) ;
#80390 = VERTEX_POINT ( 'NONE', #81945 ) ;
#80391 = CARTESIAN_POINT ( 'NONE',  ( -26.21429215707765792, 304.5182411030272078, -9.636487232772985578 ) ) ;
#80392 = EDGE_CURVE ( 'NONE', #17876, #73295, #85549, .T. ) ;
#80393 = CARTESIAN_POINT ( 'NONE',  ( 6.793650603637590990, -4.999999999999984901, -15.34177241507032896 ) ) ;
#80394 = CARTESIAN_POINT ( 'NONE',  ( 36.08349330513379982, 4.000000000000002665, 0.000000000000000000 ) ) ;
#80395 = DIRECTION ( 'NONE',  ( 0.06744659395731769647, -0.6445107564549842349, 0.7616146281272312413 ) ) ;
#80396 = STYLED_ITEM ( 'NONE', ( #64586 ), #100988 ) ;
#80397 = CARTESIAN_POINT ( 'NONE',  ( -28.61324058441433849, 13.48935699407721245, -40.19649855359993040 ) ) ;
#80398 = ORIENTED_EDGE ( 'NONE', *, *, #93956, .T. ) ;
#80399 = CARTESIAN_POINT ( 'NONE',  ( 6.838249506730348592, 3.995160516047493893, -6.573190279698081007 ) ) ;
#80400 = FILL_AREA_STYLE_COLOUR ( '', #65213 ) ;
#80402 = CARTESIAN_POINT ( 'NONE',  ( -11.93081618615098449, 6.460648502060225340, -8.911612056469465415 ) ) ;
#80401 = CARTESIAN_POINT ( 'NONE',  ( -4.447288604842995596, -18.47525482061914204, 35.07162955131727955 ) ) ;
#80403 = CARTESIAN_POINT ( 'NONE',  ( -7.188101187500002709, -21.31250000204838813, 2.977408999572648707 ) ) ;
#80404 = CARTESIAN_POINT ( 'NONE',  ( -29.50183317260367488, 13.72085623994617798, -42.10535821593475703 ) ) ;
#80405 = CARTESIAN_POINT ( 'NONE',  ( 7.715274834628325378E-15, 0.000000000000000000, -63.00000000000000000 ) ) ;
#80406 = VECTOR ( 'NONE', #88756, 1000.000000000000114 ) ;
#80407 = ORIENTED_EDGE ( 'NONE', *, *, #45975, .T. ) ;
#80408 = DIRECTION ( 'NONE',  ( 0.000000000000000000, 0.000000000000000000, 1.000000000000000000 ) ) ;
#80409 = CARTESIAN_POINT ( 'NONE',  ( -4.999999999999993783, -46.00000000000000000, 102.2532056551910387 ) ) ;
#80410 = CARTESIAN_POINT ( 'NONE',  ( -8.002730990579065562, 102.9130261956584746, -4.999999999992380317 ) ) ;
#80411 =( BOUNDED_SURFACE ( )  B_SPLINE_SURFACE ( 2, 3, ( 
 ( #79865, #87982, #41010, #72829, #39438, #40472, #14587, #6501, #81444, #48554, #14062, #15136 ),
 ( #98177, #104679, #96070, #39955, #24329, #72313, #73354, #22201, #90090, #31875, #16194, #7039 ),
 ( #64758, #57176, #30830, #97114, #63715, #96604, #73897, #83487, #47497, #97633, #23797, #105218 ),
 ( #63176, #64241, #89565, #23255, #55052, #15661, #80928, #56099, #22735, #46967, #5972, #55574 ),
 ( #106253, #32414, #88511, #80393, #89034, #48018, #51204, #83576, #83063, #58800, #100299, #74424 ) ),
 .UNSPECIFIED., .F., .F., .T. ) 
 B_SPLINE_SURFACE_WITH_KNOTS ( ( 3, 2, 3 ),
 ( 4, 2, 2, 2, 2, 4 ),
 ( -0.01000000000000000021, 0.000000000000000000, 1.000000000000000000 ),
 ( 0.000000000000000000, 0.0009008737055280950992, 0.001801747411056190198, 0.003603494822112380397, 0.005405242233168570595, 0.007206989644224760794 ),
 .UNSPECIFIED. ) 
 GEOMETRIC_REPRESENTATION_ITEM ( )  RATIONAL_B_SPLINE_SURFACE ( (
 ( 1.000000000000000000, 1.000000000000000000, 1.000000000000000000, 1.000000000000000000, 1.000000000000000000, 1.000000000000000000, 1.000000000000000000, 1.000000000000000000, 1.000000000000000000, 1.000000000000000000, 1.000000000000000000, 1.000000000000000000),
 ( 1.000000000000000000, 1.000000000000000000, 1.000000000000000000, 1.000000000000000000, 1.000000000000000000, 1.000000000000000000, 1.000000000000000000, 1.000000000000000000, 1.000000000000000000, 1.000000000000000000, 1.000000000000000000, 1.000000000000000000),
 ( 1.000000000000000000, 1.000000000000000000, 1.000000000000000000, 1.000000000000000000, 1.000000000000000000, 1.000000000000000000, 1.000000000000000000, 1.000000000000000000, 1.000000000000000000, 1.000000000000000000, 1.000000000000000000, 1.000000000000000000),
 ( 1.857142857142858317, 1.857142857142858317, 1.857142857142858317, 1.857142857142858317, 1.857142857142858317, 1.857142857142858317, 1.857142857142858317, 1.857142857142858317, 1.857142857142858317, 1.857142857142858317, 1.857142857142858317, 1.857142857142858317),
 ( 1.000000000000000000, 1.000000000000000000, 1.000000000000000000, 1.000000000000000000, 1.000000000000000000, 1.000000000000000000, 1.000000000000000000, 1.000000000000000000, 1.000000000000000000, 1.000000000000000000, 1.000000000000000000, 1.000000000000000000) ) ) 
 REPRESENTATION_ITEM ( '' )  SURFACE ( )  );
#80412 = DIRECTION ( 'NONE',  ( 0.000000000000000000, -1.000000000000000000, 0.000000000000000000 ) ) ;
#80413 = DIRECTION ( 'NONE',  ( -1.000000000000000000, -1.224606353822377258E-16, -0.000000000000000000 ) ) ;
#80414 = EDGE_CURVE ( 'NONE', #25485, #5108, #51586, .T. ) ;
#80415 = VERTEX_POINT ( 'NONE', #90057 ) ;
#80416 = CARTESIAN_POINT ( 'NONE',  ( 31.08349330513380693, 4.898587196589411843E-16, -4.000000000000001776 ) ) ;
#80417 = DIRECTION ( 'NONE',  ( -1.000000000000000000, 0.000000000000000000, 0.000000000000000000 ) ) ;
#80418 = AXIS2_PLACEMENT_3D ( 'NONE', #71549, #54288, #31142 ) ;
#80419 = CIRCLE ( 'NONE', #78658, 4.000000000000001776 ) ;
#80420 = ORIENTED_EDGE ( 'NONE', *, *, #80375, .F. ) ;
#80421 = EDGE_CURVE ( 'NONE', #17199, #91513, #16161, .T. ) ;
#80422 = CARTESIAN_POINT ( 'NONE',  ( 93.39999999999999147, 4.172000000000019249, 0.000000000000000000 ) ) ;
#80423 = ADVANCED_FACE ( 'NONE', ( #35991 ), #63785, .F. ) ;
#80424 = CARTESIAN_POINT ( 'NONE',  ( -1.276674890354437375, -1.417245842567761834E-15, 101.3108517956189161 ) ) ;
#80425 = UNCERTAINTY_MEASURE_WITH_UNIT (LENGTH_MEASURE( 1.000000000000000082E-05 ), #32744, 'distance_accuracy_value', 'NONE');
#80426 = CARTESIAN_POINT ( 'NONE',  ( -106.5012798387082142, -59.99999999999999289, 119.5216608596331298 ) ) ;
#80427 = PRODUCT_DEFINITION_SHAPE ( 'NONE', 'NONE',  #106815 ) ;
#80428 =( GEOMETRIC_REPRESENTATION_CONTEXT ( 3 ) GLOBAL_UNCERTAINTY_ASSIGNED_CONTEXT ( ( #53696 ) ) GLOBAL_UNIT_ASSIGNED_CONTEXT ( ( #57945, #18055, #75736 ) ) REPRESENTATION_CONTEXT ( 'NONE', 'WORKASPACE' ) );
#80429 = CIRCLE ( 'NONE', #106220, 0.5000000000000004441 ) ;
#80430 = VECTOR ( 'NONE', #59377, 1000.000000000000000 ) ;
#80431 = DIRECTION ( 'NONE',  ( -1.000000000000000000, -1.224606353822377258E-16, -0.000000000000000000 ) ) ;
#80432 = CARTESIAN_POINT ( 'NONE',  ( -8.737863884124131175, -5.000000000000002665, -79.96381019768853093 ) ) ;
#80433 = CARTESIAN_POINT ( 'NONE',  ( -83.43473808630078281, -42.98247295588366512, 178.5312127204583419 ) ) ;
#80434 = ORIENTED_EDGE ( 'NONE', *, *, #9943, .T. ) ;
#80435 = CARTESIAN_POINT ( 'NONE',  ( 7.500000000000005329, -5.250000000000004441, -68.91429205785459544 ) ) ;
#80436 = MECHANICAL_DESIGN_GEOMETRIC_PRESENTATION_REPRESENTATION (  '', ( #76988 ), #6374 ) ;
#80437 = AXIS2_PLACEMENT_3D ( 'NONE', #76718, #35786, #58968 ) ;
#80438 = ORIENTED_EDGE ( 'NONE', *, *, #9403, .F. ) ;
#80439 = CARTESIAN_POINT ( 'NONE',  ( 0.000000000000000000, 0.000000000000000000, 27.00000000000000000 ) ) ;
#80440 = CARTESIAN_POINT ( 'NONE',  ( 4.567209634097048720, -65.93599786085512449, -3.891254717191803714 ) ) ;
#80441 = CARTESIAN_POINT ( 'NONE',  ( -86.16836316469820645, -60.13563296699030047, 8.610485354239809652 ) ) ;
#80442 = CARTESIAN_POINT ( 'NONE',  ( -15.72336466908044095, 304.5560426036738022, 8.874135081214639342 ) ) ;
#80443 = CARTESIAN_POINT ( 'NONE',  ( -15.85122647056153156, 4.114663126756377132, -4.288211754877429449 ) ) ;
#80444 = CARTESIAN_POINT ( 'NONE',  ( 30.00000000000000000, 462.0217650461267453, 12.66663979486846081 ) ) ;
#80445 = CARTESIAN_POINT ( 'NONE',  ( -1.191759989000076070, -5.000000000000000000, -97.99990947982458067 ) ) ;
#80446 = CARTESIAN_POINT ( 'NONE',  ( -43.03987588564145028, 486.0760633267551611, 5.817066388976097180 ) ) ;
#80447 = CARTESIAN_POINT ( 'NONE',  ( 112.8608516834554649, -60.00000000000000000, 189.7942083920301855 ) ) ;
#80448 = CARTESIAN_POINT ( 'NONE',  ( -88.10255448128359035, -14.21045842199438347, 36.33746784607973268 ) ) ;
#80449 = CARTESIAN_POINT ( 'NONE',  ( -63.87384138004166800, -25.58014744444937705, 75.85766445878087438 ) ) ;
#80450 = ORIENTED_EDGE ( 'NONE', *, *, #11431, .F. ) ;
#80451 = CARTESIAN_POINT ( 'NONE',  ( -31.42871867836007027, 39.42550727674528588, 56.97524511970465255 ) ) ;
#80452 = CARTESIAN_POINT ( 'NONE',  ( 73.31980294431531320, -59.99999999999508304, 186.0766219959947705 ) ) ;
#80453 = ORIENTED_EDGE ( 'NONE', *, *, #46857, .T. ) ;
#80454 = CARTESIAN_POINT ( 'NONE',  ( 1.000716238102184574, -35.99156567037908871, 29.88824423799887953 ) ) ;
#80455 = CARTESIAN_POINT ( 'NONE',  ( 2.977408999572650927, -17.75000000204838457, -7.188101187500000933 ) ) ;
#80456 = EDGE_CURVE ( 'NONE', #30441, #79214, #41589, .T. ) ;
#80457 = ORIENTED_EDGE ( 'NONE', *, *, #51918, .T. ) ;
#80458 = COLOUR_RGB ( '', 0.09019608, 0.27058824, 0.51372549) ;
#80459 = CARTESIAN_POINT ( 'NONE',  ( 3.375199637455089441, -49.11004099528027922, 104.1123102281673170 ) ) ;
#80460 = ORIENTED_EDGE ( 'NONE', *, *, #24838, .F. ) ;
#80461 = CARTESIAN_POINT ( 'NONE',  ( 18.58349330513380337, 1.593028355512270567E-15, 0.000000000000000000 ) ) ;
#80462 = CARTESIAN_POINT ( 'NONE',  ( 36.84999999999999432, 1.533819458162526451E-15, 0.000000000000000000 ) ) ;
#80463 = CARTESIAN_POINT ( 'NONE',  ( -102.2674112109930888, -59.99999999999998579, 201.0223749624553307 ) ) ;
#80464 = CARTESIAN_POINT ( 'NONE',  ( 16.14595037822608603, 6.785770140112262538, 6.193810554583017769 ) ) ;
#80465 = CARTESIAN_POINT ( 'NONE',  ( 7.188101187500000044, -25.53125000204838813, 0.000000000000000000 ) ) ;
#80466 = CARTESIAN_POINT ( 'NONE',  ( 43.77599596716764552, 462.5271020414195391, 5.125623680081139888 ) ) ;
#80467 = MECHANICAL_DESIGN_GEOMETRIC_PRESENTATION_REPRESENTATION (  '', ( #75319 ), #63255 ) ;
#80468 = CARTESIAN_POINT ( 'NONE',  ( -13.63548989270066158, 20.28416372052714323, 6.862577965993339468 ) ) ;
#80469 = CARTESIAN_POINT ( 'NONE',  ( 5.000000000000000000, -65.46413530816580817, 15.04248154712246688 ) ) ;
#80470 = CARTESIAN_POINT ( 'NONE',  ( 5.036189802310016006, 50.00000000000001421, -93.73786388411662074 ) ) ;
#80471 = CARTESIAN_POINT ( 'NONE',  ( 21.67692307692307452, 1.411358822780289120E-15, 0.000000000000000000 ) ) ;
#80472 = CARTESIAN_POINT ( 'NONE',  ( 37.02012750797187124, 345.4824561708261399, 0.1020140138803038443 ) ) ;
#80473 = CARTESIAN_POINT ( 'NONE',  ( -36.78691999813820956, -36.04881776531558302, 35.70211516714942235 ) ) ;
#80474 = EDGE_LOOP ( 'NONE', ( #32109, #65600, #7703, #7033 ) ) ;
#80475 = CARTESIAN_POINT ( 'NONE',  ( 39.97211509376299432, -56.79955896029697016, 42.45315631278550228 ) ) ;
#80476 = CARTESIAN_POINT ( 'NONE',  ( 17.01589776168603407, -1.734723475976807094E-15, -2.227375807149030162 ) ) ;
#80477 = ORIENTED_EDGE ( 'NONE', *, *, #48345, .F. ) ;
#80479 = AXIS2_PLACEMENT_3D ( 'NONE', #68285, #94153, #75834 ) ;
#80478 = CARTESIAN_POINT ( 'NONE',  ( 6.585468679846625761, -7.640532685286896886, -0.2337908078075601470 ) ) ;
#80480 = CARTESIAN_POINT ( 'NONE',  ( -73.93043056857301565, -38.32664425143800457, 159.7661319727351383 ) ) ;
#80481 = ORIENTED_EDGE ( 'NONE', *, *, #99537, .T. ) ;
#80483 = CARTESIAN_POINT ( 'NONE',  ( -26.54817876223620488, 310.6276912632132507, 11.31208242866018132 ) ) ;
#80482 = CARTESIAN_POINT ( 'NONE',  ( 8.733056179379989459, -5.000000000000000000, -16.76938723918380703 ) ) ;
#80484 = DIRECTION ( 'NONE',  ( 0.000000000000000000, -1.000000000000000000, 0.000000000000000000 ) ) ;
#80485 = LINE ( 'NONE', #78375, #32787 ) ;
#80486 = FACE_OUTER_BOUND ( 'NONE', #41769, .T. ) ;
#80487 = DIRECTION ( 'NONE',  ( 1.000000000000000000, 0.000000000000000000, 0.000000000000000000 ) ) ;
#80489 = MECHANICAL_DESIGN_GEOMETRIC_PRESENTATION_REPRESENTATION (  '', ( #65022 ), #104671 ) ;
#80488 = LINE ( 'NONE', #13099, #101659 ) ;
#80490 = CARTESIAN_POINT ( 'NONE',  ( -3.455451579656851013, -49.16755827892872333, 44.00736102010382922 ) ) ;
#80491 = CARTESIAN_POINT ( 'NONE',  ( 93.34040896384792063, -60.00000000000002842, 35.57582133924940138 ) ) ;
#80492 = CARTESIAN_POINT ( 'NONE',  ( -44.10116655607205871, 485.7577240482563070, 4.111541829922503943 ) ) ;
#80493 = CARTESIAN_POINT ( 'NONE',  ( 13.58349330513380515, 1.593028355512270962E-15, 0.000000000000000000 ) ) ;
#80494 = CARTESIAN_POINT ( 'NONE',  ( 93.97977184163765685, 1.030564683017419500E-14, 0.000000000000000000 ) ) ;
#80495 = EDGE_LOOP ( 'NONE', ( #91452, #90829, #81675, #48737, #61430 ) ) ;
#80496 = EDGE_CURVE ( 'NONE', #37464, #80344, #19811, .T. ) ;
#80497 = CARTESIAN_POINT ( 'NONE',  ( -89.60745021536853017, -30.00000000000670397, -12.65992882304214895 ) ) ;
#80498 = VERTEX_POINT ( 'NONE', #27906 ) ;
#80499 = CARTESIAN_POINT ( 'NONE',  ( 4.582575694955843382, 15.00000000000000000, -10.00000000000000000 ) ) ;
#80500 = CARTESIAN_POINT ( 'NONE',  ( -15.88105853605327766, 3.776612129045478827, -3.593753328288301407 ) ) ;
#80501 = CARTESIAN_POINT ( 'NONE',  ( 9.517802786874057119, 9.453294933053111748, 5.000000000000309086 ) ) ;
#80502 = CARTESIAN_POINT ( 'NONE',  ( -3.454253436624922458, -49.15858197120396511, 103.7259032015043090 ) ) ;
#80503 = CARTESIAN_POINT ( 'NONE',  ( 0.000000000000000000, 6.123233995736770227E-16, -5.000000000000002665 ) ) ;
#80504 = AXIS2_PLACEMENT_3D ( 'NONE', #55100, #81488, #56143 ) ;
#80505 = CARTESIAN_POINT ( 'NONE',  ( 5.082755093536324154, -22.71875000204838457, 5.082755093536326818 ) ) ;
#80506 = DIRECTION ( 'NONE',  ( 0.5735764363510440500, 0.8191520442889932418, 0.000000000000000000 ) ) ;
#80507 = CARTESIAN_POINT ( 'NONE',  ( 7.029557119109635543, 41.29102226339720261, -70.49405813111694385 ) ) ;
#80508 = EDGE_CURVE ( 'NONE', #28791, #13515, #17281, .T. ) ;
#80509 = ORIENTED_EDGE ( 'NONE', *, *, #73191, .T. ) ;
#80510 = EDGE_CURVE ( 'NONE', #86218, #93736, #67585, .T. ) ;
#80511 = AXIS2_PLACEMENT_3D ( 'NONE', #44067, #11674, #13667 ) ;
#80512 = CIRCLE ( 'NONE', #1269, 4.000000000000007105 ) ;
#80513 = PRESENTATION_LAYER_ASSIGNMENT (  '', '', ( #85713 ) ) ;
#80515 = ORIENTED_EDGE ( 'NONE', *, *, #19193, .F. ) ;
#80514 = CARTESIAN_POINT ( 'NONE',  ( 4.970849588242775674, -3.447900702885856816, 102.2755693391596594 ) ) ;
#80516 = CARTESIAN_POINT ( 'NONE',  ( 82.07463894558122774, -29.09153447962462025, 147.4962313882754756 ) ) ;
#80517 = CARTESIAN_POINT ( 'NONE',  ( 15.22818746203033591, 3.929489829918852983, -4.609438620807785547 ) ) ;
#80518 = ORIENTED_EDGE ( 'NONE', *, *, #24112, .T. ) ;
#80519 = DIRECTION ( 'NONE',  ( 1.000000000000000000, 0.000000000000000000, 0.000000000000000000 ) ) ;
#80520 = EDGE_CURVE ( 'NONE', #97138, #44023, #46170, .T. ) ;
#80521 = CARTESIAN_POINT ( 'NONE',  ( -1.251098771870337023, 15.60329354122197110, -50.60675712933594639 ) ) ;
#80522 = CARTESIAN_POINT ( 'NONE',  ( 5.082755093536324154, -10.34375000204838457, 5.082755093536326818 ) ) ;
#80523 = CARTESIAN_POINT ( 'NONE',  ( 6.928203230275509661, 29.73069070304461192, -4.000000000000000000 ) ) ;
#80524 = CONICAL_SURFACE ( 'NONE', #32287, 5.000000000000001776, 0.9599310885968803664 ) ;
#80525 = CARTESIAN_POINT ( 'NONE',  ( -29.04643245788701122, -57.68166065953202093, 44.76603692081018693 ) ) ;
#80526 = CARTESIAN_POINT ( 'NONE',  ( 6.326445470157512574, -5.253846677262524523, -4.563138989068577622 ) ) ;
#80527 = ORIENTED_EDGE ( 'NONE', *, *, #29003, .T. ) ;
#80528 = SURFACE_STYLE_FILL_AREA ( #47099 ) ;
#80529 = CONICAL_SURFACE ( 'NONE', #34067, 4.000000000000001776, 0.9599310885968808105 ) ;
#80530 = CARTESIAN_POINT ( 'NONE',  ( 0.000000000000000000, 0.000000000000000000, 0.000000000000000000 ) ) ;
#80531 = CARTESIAN_POINT ( 'NONE',  ( 30.50942973405924974, 18.64284798592565195, -23.36871039509505721 ) ) ;
#80532 = CIRCLE ( 'NONE', #47741, 8.750000000000023093 ) ;
#80533 = ORIENTED_EDGE ( 'NONE', *, *, #31946, .T. ) ;
#80534 = CARTESIAN_POINT ( 'NONE',  ( -5.656854249492381470, -13.25000000409676915, 5.656854249492379694 ) ) ;
#80535 = LINE ( 'NONE', #11281, #51996 ) ;
#80536 = CARTESIAN_POINT ( 'NONE',  ( 9.999999999999998224, 15.00000000000000000, -1.734723475976806306E-15 ) ) ;
#80537 = CARTESIAN_POINT ( 'NONE',  ( 0.7834125968129763695, 52.06998597394611750, -8.012555785356894944 ) ) ;
#80538 = AXIS2_PLACEMENT_3D ( 'NONE', #103958, #46794, #87267 ) ;
#80539 = CARTESIAN_POINT ( 'NONE',  ( -9.176645556628256983, 85.52739032406731212, 3.973966573947710135 ) ) ;
#80540 = CARTESIAN_POINT ( 'NONE',  ( 5.656854249492378806, -20.18749999999999289, 5.656854249492381470 ) ) ;
#80541 = PRODUCT_CONTEXT ( 'NONE', #69346, 'mechanical' ) ;
#80542 = CARTESIAN_POINT ( 'NONE',  ( -6.125000000000002665, -15.62228920881133654, 14.41094225130411211 ) ) ;
#80543 = VERTEX_POINT ( 'NONE', #61296 ) ;
#80544 = CARTESIAN_POINT ( 'NONE',  ( 10.36965645692189142, 43.24028602702204438, 15.40779740156149913 ) ) ;
#80545 = CARTESIAN_POINT ( 'NONE',  ( -3.997425403567957503, 15.99999999372935022, 9.168149550321043506 ) ) ;
#80546 = CARTESIAN_POINT ( 'NONE',  ( -3.013127284365967107, 15.20956086706489963, -6.321382838634907131 ) ) ;
#80547 = CARTESIAN_POINT ( 'NONE',  ( 49.93561212394431692, -35.59291040412786344, -36.20314293518854498 ) ) ;
#80548 = DIRECTION ( 'NONE',  ( 0.000000000000000000, -1.000000000000000000, 0.000000000000000000 ) ) ;
#80549 = ORIENTED_EDGE ( 'NONE', *, *, #84641, .T. ) ;
#80550 = CARTESIAN_POINT ( 'NONE',  ( 8.000000000000000000, -9.593750004096769146, -3.313708498984761164 ) ) ;
#80551 = CARTESIAN_POINT ( 'NONE',  ( 100.9016562759859426, -57.62918874011371173, 203.6651917875242930 ) ) ;
#80552 = DIRECTION ( 'NONE',  ( 0.000000000000000000, 0.000000000000000000, 1.000000000000000000 ) ) ;
#80553 = AXIS2_PLACEMENT_3D ( 'NONE', #71195, #45870, #104091 ) ;
#80554 = EDGE_CURVE ( 'NONE', #105782, #64513, #20885, .T. ) ;
#80555 = CARTESIAN_POINT ( 'NONE',  ( -16.10099483391875808, 21.87267635329494198, 0.2108314046237644568 ) ) ;
#80556 = FACE_OUTER_BOUND ( 'NONE', #55488, .T. ) ;
#80557 = CARTESIAN_POINT ( 'NONE',  ( -74.34387358700993786, -59.99999999999999289, 175.6333023556407227 ) ) ;
#80558 = CARTESIAN_POINT ( 'NONE',  ( -40.93435977689158989, 414.3154843149413296, 27.72243992809649527 ) ) ;
#80559 = CARTESIAN_POINT ( 'NONE',  ( 6.400000000000000355, -9.237604307034013473, 7.924929828396943928E-16 ) ) ;
#80560 = CARTESIAN_POINT ( 'NONE',  ( 39.04923757937011430, 50.00000000002003731, 52.30342408740191473 ) ) ;
#80561 = AXIS2_PLACEMENT_3D ( 'NONE', #29004, #96349, #86676 ) ;
#80562 = CARTESIAN_POINT ( 'NONE',  ( -83.59396215382736273, -61.00678146017968118, 191.7067536044777398 ) ) ;
#80563 = ORIENTED_EDGE ( 'NONE', *, *, #94536, .T. ) ;
#80564 = CARTESIAN_POINT ( 'NONE',  ( 33.72097909745567534, 327.0062835497062110, -4.563092033313610685 ) ) ;
#80565 = ORIENTED_EDGE ( 'NONE', *, *, #30719, .T. ) ;
#80567 = ADVANCED_FACE ( 'NONE', ( #102812 ), #72462, .F. ) ;
#80566 = CARTESIAN_POINT ( 'NONE',  ( 12.15075205251924828, -4.649444361049084762, -76.81485639520219877 ) ) ;
#80568 = CARTESIAN_POINT ( 'NONE',  ( -22.25702730880545843, 304.1569973802309619, -9.934833947929556430 ) ) ;
#80569 = CARTESIAN_POINT ( 'NONE',  ( -84.10008721281353417, -60.17582440984561742, -17.33015767790280037 ) ) ;
#80570 = CARTESIAN_POINT ( 'NONE',  ( -43.18591170618147146, 464.9496799542819190, 14.54256400180418218 ) ) ;
#80571 = DIRECTION ( 'NONE',  ( 0.000000000000000000, 0.000000000000000000, 1.000000000000000000 ) ) ;
#80572 = CIRCLE ( 'NONE', #106440, 8.000000000000000000 ) ;
#80573 = ORIENTED_EDGE ( 'NONE', *, *, #103617, .T. ) ;
#80574 = CIRCLE ( 'NONE', #37522, 6.500000000000000888 ) ;
#80575 = CARTESIAN_POINT ( 'NONE',  ( 40.02592568779148507, 1.482358050883964840E-15, 0.000000000000000000 ) ) ;
#80576 = CARTESIAN_POINT ( 'NONE',  ( 13.00302362776394816, 4.344380092746527922, -7.377937999068717723 ) ) ;
#80577 = CARTESIAN_POINT ( 'NONE',  ( 11.19959342721965179, -3.864748466433897305E-12, 19.43146043915186993 ) ) ;
#80578 = CARTESIAN_POINT ( 'NONE',  ( -35.03620922308809327, 464.5070590296365367, 18.87187099903851717 ) ) ;
#80579 = CARTESIAN_POINT ( 'NONE',  ( 88.92118937161633596, -29.99999999999996092, -15.18954496189254755 ) ) ;
#80580 = CARTESIAN_POINT ( 'NONE',  ( -77.26988927366080873, -25.60911552037473626, 119.8400127943013018 ) ) ;
#80581 = EDGE_LOOP ( 'NONE', ( #17840, #54756, #66252, #54428, #97657 ) ) ;
#80582 = CARTESIAN_POINT ( 'NONE',  ( 21.36200998601213641, -60.00000000000005684, 42.72826288236584702 ) ) ;
#80583 =( NAMED_UNIT ( * ) PLANE_ANGLE_UNIT ( ) SI_UNIT ( $, .RADIAN. ) );
#80584 = CARTESIAN_POINT ( 'NONE',  ( 89.80416004794994933, -57.60826090897426610, 203.9417383441736149 ) ) ;
#80585 = AXIS2_PLACEMENT_3D ( 'NONE', #60834, #19879, #67328 ) ;
#80586 = AXIS2_PLACEMENT_3D ( 'NONE', #20902, #53737, #86665 ) ;
#80587 = CARTESIAN_POINT ( 'NONE',  ( 27.72817644236535983, 34.28350906085407956, 9.902989610335730220 ) ) ;
#80588 = CARTESIAN_POINT ( 'NONE',  ( 37.02242109889342458, 304.0242369042755968, -7.899015950623281768 ) ) ;
#80589 = ADVANCED_FACE ( 'NONE', ( #94737 ), #103856, .F. ) ;
#80590 = CARTESIAN_POINT ( 'NONE',  ( 26.84999999999999787, 3.309500000000003439, 4.052968581778167743E-16 ) ) ;
#80591 = EDGE_LOOP ( 'NONE', ( #35325, #78932, #13083 ) ) ;
#80592 = CARTESIAN_POINT ( 'NONE',  ( 7.500000000000000888, 0.000000000000000000, 1.734723475976807094E-15 ) ) ;
#80593 = CARTESIAN_POINT ( 'NONE',  ( -12.50000000000000000, 3.927497713838737692, -21.92086582174311005 ) ) ;
#80595 = CARTESIAN_POINT ( 'NONE',  ( -101.2390777639338637, -45.26542400508802189, 139.7538116451968051 ) ) ;
#80594 = DIRECTION ( 'NONE',  ( 1.000000000000000000, -0.000000000000000000, -0.000000000000000000 ) ) ;
#80596 = CARTESIAN_POINT ( 'NONE',  ( 7.188101187500001821, -20.56250000204838457, -2.977408999572650483 ) ) ;
#80597 = CARTESIAN_POINT ( 'NONE',  ( 43.58530483652910448, 484.9293427334628177, 0.7222135195755269299 ) ) ;
#80598 = CARTESIAN_POINT ( 'NONE',  ( 9.699016383038308931, 81.82361828551655947, 2.444973590251036999 ) ) ;
#80599 = CARTESIAN_POINT ( 'NONE',  ( 6.645597273868374621, 41.91296976309556044, -68.91429206532015428 ) ) ;
#80600 = CARTESIAN_POINT ( 'NONE',  ( -7.499999999999998224, -1.545780083833950380, -7.491787297939224821 ) ) ;
#80601 = FILL_AREA_STYLE ('',( #30497 ) ) ;
#80602 =( GEOMETRIC_REPRESENTATION_CONTEXT ( 3 ) GLOBAL_UNCERTAINTY_ASSIGNED_CONTEXT ( ( #72177 ) ) GLOBAL_UNIT_ASSIGNED_CONTEXT ( ( #23153, #72726, #31770 ) ) REPRESENTATION_CONTEXT ( 'NONE', 'WORKASPACE' ) );
#80603 = VERTEX_POINT ( 'NONE', #78517 ) ;
#80604 = FACE_OUTER_BOUND ( 'NONE', #59123, .T. ) ;
#80606 = CARTESIAN_POINT ( 'NONE',  ( 30.13134821053596113, -22.12450956031193883, 30.04249343119618132 ) ) ;
#80605 = CARTESIAN_POINT ( 'NONE',  ( 10.28624191511809371, 45.38549880562041494, -15.40779740156171762 ) ) ;
#80607 = CARTESIAN_POINT ( 'NONE',  ( -23.21751746555247919, 25.98869614573810694, 30.70617127781050471 ) ) ;
#80608 = EDGE_LOOP ( 'NONE', ( #39558, #51279, #19919, #84917, #31004, #52401 ) ) ;
#80609 = MECHANICAL_DESIGN_GEOMETRIC_PRESENTATION_REPRESENTATION (  '', ( #16888 ), #23760 ) ;
#80610 = EDGE_LOOP ( 'NONE', ( #6882, #69361 ) ) ;
#80612 = CARTESIAN_POINT ( 'NONE',  ( -1.218675684878021359, 43.73169810651692302, -17.17891848071411687 ) ) ;
#80611 = PRESENTATION_STYLE_ASSIGNMENT (( #47712 ) ) ;
#80613 = CARTESIAN_POINT ( 'NONE',  ( 37.38561277374697056, 0.000000000000000000, 5.000000000000002665 ) ) ;
#80614 = CARTESIAN_POINT ( 'NONE',  ( -44.28408485723331722, 463.6816916292610813, 7.557853517639972374 ) ) ;
#80615 = CARTESIAN_POINT ( 'NONE',  ( 43.00000000000000000, 461.4080316921935605, 3.462976341553817949 ) ) ;
#80616 =( NAMED_UNIT ( * ) SI_UNIT ( $, .STERADIAN. ) SOLID_ANGLE_UNIT ( ) );
#80617 = CARTESIAN_POINT ( 'NONE',  ( 0.000000000000000000, 27.68727484027578356, 0.000000000000000000 ) ) ;
#80619 = ORIENTED_EDGE ( 'NONE', *, *, #106052, .F. ) ;
#80618 = CONICAL_SURFACE ( 'NONE', #65227, 4.000000000000001776, 0.9599310885968774798 ) ;
#80620 = DIRECTION ( 'NONE',  ( -0.000000000000000000, -1.000000000000000000, -0.000000000000000000 ) ) ;
#80621 = CARTESIAN_POINT ( 'NONE',  ( 86.25826092630657627, -30.00000000000007461, 180.2437358770224307 ) ) ;
#80622 = CARTESIAN_POINT ( 'NONE',  ( -84.20864119875632525, -52.67321261282354072, -14.85889068594910256 ) ) ;
#80623 = DIRECTION ( 'NONE',  ( -1.000000000000000000, 0.000000000000000000, 0.000000000000000000 ) ) ;
#80624 = CARTESIAN_POINT ( 'NONE',  ( 46.96202111036839710, 13.62308641270886156, -14.94990935055657033 ) ) ;
#80625 = ORIENTED_EDGE ( 'NONE', *, *, #101768, .F. ) ;
#80626 = ORIENTED_EDGE ( 'NONE', *, *, #105076, .T. ) ;
#80627 = VECTOR ( 'NONE', #54676, 1000.000000000000000 ) ;
#80628 = EDGE_LOOP ( 'NONE', ( #105965, #54338, #60201, #39948, #7283 ) ) ;
#80629 = CARTESIAN_POINT ( 'NONE',  ( -10.00000000000000355, 30.00000000000000000, 0.000000000000000000 ) ) ;
#80630 =( NAMED_UNIT ( * ) PLANE_ANGLE_UNIT ( ) SI_UNIT ( $, .RADIAN. ) );
#80631 = CARTESIAN_POINT ( 'NONE',  ( 0.000000000000000000, 5.629165124598847214, -3.250000000000007550 ) ) ;
#80632 = FACE_OUTER_BOUND ( 'NONE', #92396, .T. ) ;
#80633 = CARTESIAN_POINT ( 'NONE',  ( -44.47935674825744456, 338.5055569983761643, 0.4977047367126199995 ) ) ;
#80634 = CARTESIAN_POINT ( 'NONE',  ( -4.176044994242080755, -67.08026818686849424, 13.14625702355704640 ) ) ;
#80635 = EDGE_CURVE ( 'NONE', #12958, #596, #13775, .T. ) ;
#80636 = CARTESIAN_POINT ( 'NONE',  ( -44.22863636901156070, 485.2832843285482909, 1.778997975940832310 ) ) ;
#80637 = CARTESIAN_POINT ( 'NONE',  ( -33.84761347220299399, 488.7471039746336032, 11.01988148152527103 ) ) ;
#80638 = CIRCLE ( 'NONE', #13228, 5.000000000000001776 ) ;
#80639 = VERTEX_POINT ( 'NONE', #70966 ) ;
#80640 = DIRECTION ( 'NONE',  ( 0.000000000000000000, 0.000000000000000000, -1.000000000000000000 ) ) ;
#80641 = EDGE_LOOP ( 'NONE', ( #82180, #16258, #71505 ) ) ;
#80642 = CARTESIAN_POINT ( 'NONE',  ( 0.000000000000000000, 0.000000000000000000, -7.131971428571428184 ) ) ;
#80643 = CARTESIAN_POINT ( 'NONE',  ( 3.364021409948656505, 294.8518027753228807, 9.936999415087239385 ) ) ;
#80644 =( GEOMETRIC_REPRESENTATION_CONTEXT ( 3 ) GLOBAL_UNCERTAINTY_ASSIGNED_CONTEXT ( ( #103116 ) ) GLOBAL_UNIT_ASSIGNED_CONTEXT ( ( #36334, #62185, #93473 ) ) REPRESENTATION_CONTEXT ( 'NONE', 'WORKASPACE' ) );
#80645 = DIRECTION ( 'NONE',  ( -1.000000000000000000, -1.224606353822377258E-16, -0.000000000000000000 ) ) ;
#80646 = CARTESIAN_POINT ( 'NONE',  ( 69.71140032424059996, -22.11089216996448314, 91.05876745230327174 ) ) ;
#80647 = AXIS2_PLACEMENT_3D ( 'NONE', #29781, #103630, #69680 ) ;
#80648 = ORIENTED_EDGE ( 'NONE', *, *, #79256, .F. ) ;
#80649 = CARTESIAN_POINT ( 'NONE',  ( 40.97311670756442226, 465.3163554148249546, 16.72191547249029853 ) ) ;
#80650 = EDGE_CURVE ( 'NONE', #98662, #48969, #30003, .T. ) ;
#80651 = CARTESIAN_POINT ( 'NONE',  ( 2.977408999572650927, -29.37500000204838457, -7.188101187500000933 ) ) ;
#80652 = EDGE_CURVE ( 'NONE', #61487, #93158, #91427, .T. ) ;
#80653 =( LENGTH_UNIT ( ) NAMED_UNIT ( * ) SI_UNIT ( .MILLI., .METRE. ) );
#80654 = VERTEX_POINT ( 'NONE', #95781 ) ;
#80655 = PRESENTATION_STYLE_ASSIGNMENT (( #40204 ) ) ;
#80656 = CARTESIAN_POINT ( 'NONE',  ( 67.96666666666666856, -3.309500000000000774, 0.000000000000000000 ) ) ;
#80657 = VECTOR ( 'NONE', #22942, 1000.000000000000114 ) ;
#80658 =( GEOMETRIC_REPRESENTATION_CONTEXT ( 3 ) GLOBAL_UNCERTAINTY_ASSIGNED_CONTEXT ( ( #38419 ) ) GLOBAL_UNIT_ASSIGNED_CONTEXT ( ( #31035, #7767, #39640 ) ) REPRESENTATION_CONTEXT ( 'NONE', 'WORKASPACE' ) );
#80659 = CARTESIAN_POINT ( 'NONE',  ( -36.52797673978124493, 490.9928046865521196, 12.47113835538635129 ) ) ;
#80660 = CARTESIAN_POINT ( 'NONE',  ( 3.313708498984762496, -32.46875000409677625, 7.999999999999998224 ) ) ;
#80661 = CARTESIAN_POINT ( 'NONE',  ( -2.094395098902536390, -3.000000000000000000, -8.000000000000000000 ) ) ;
#80662 = CIRCLE ( 'NONE', #84145, 3.309500000000001663 ) ;
#80663 = CARTESIAN_POINT ( 'NONE',  ( 86.45523760431080973, -17.05172403587358687, 183.4746797687946014 ) ) ;
#80664 =( NAMED_UNIT ( * ) SI_UNIT ( $, .STERADIAN. ) SOLID_ANGLE_UNIT ( ) );
#80665 = B_SPLINE_CURVE_WITH_KNOTS ( 'NONE', 3,
 ( #51952, #59005, #91891, #76765, #100509, #3424 ),
 .UNSPECIFIED., .F., .F.,
 ( 4, 2, 4 ),
 ( 2.475503369175507341E-07, 0.002222330217055621098, 0.004444412883774324571 ),
 .UNSPECIFIED. ) ;
#80666 = CARTESIAN_POINT ( 'NONE',  ( 9.999952458099484076, 33.99988114523864624, 0.2653554233229051817 ) ) ;
#80667 = DIRECTION ( 'NONE',  ( 0.000000000000000000, -1.000000000000000000, 0.000000000000000000 ) ) ;
#80668 = CARTESIAN_POINT ( 'NONE',  ( 3.339334701221695401, 304.8518027741603191, 9.936999414964258648 ) ) ;
#80669 = ORIENTED_EDGE ( 'NONE', *, *, #39336, .T. ) ;
#80670 = DIRECTION ( 'NONE',  ( 1.000000000000000000, 0.000000000000000000, 0.000000000000000000 ) ) ;
#80671 = CARTESIAN_POINT ( 'NONE',  ( 29.51551548483486798, -60.00000000000000000, 42.80185321029230039 ) ) ;
#80672 = CARTESIAN_POINT ( 'NONE',  ( -96.33434547725939012, -30.00000000000000000, 191.2481680440488958 ) ) ;
#80673 = STYLED_ITEM ( 'NONE', ( #76587 ), #44780 ) ;
#80674 = DIRECTION ( 'NONE',  ( -0.5735764363510510444, -0.8191520442889883569, 0.000000000000000000 ) ) ;
#80675 = CARTESIAN_POINT ( 'NONE',  ( 40.82139093095994298, -57.69032097903409806, 57.04468382372385094 ) ) ;
#80677 = DIRECTION ( 'NONE',  ( 0.5735764363510466035, -0.8191520442889914655, 1.003171929053524500E-16 ) ) ;
#80676 = FACE_OUTER_BOUND ( 'NONE', #851, .T. ) ;
#80678 = PRESENTATION_LAYER_ASSIGNMENT (  '', '', ( #97933 ) ) ;
#80679 = EDGE_CURVE ( 'NONE', #49541, #54088, #69388, .T. ) ;
#80680 = PRESENTATION_LAYER_ASSIGNMENT (  '', '', ( #44528 ) ) ;
#80681 =( NAMED_UNIT ( * ) SI_UNIT ( $, .STERADIAN. ) SOLID_ANGLE_UNIT ( ) );
#80682 =( NAMED_UNIT ( * ) SI_UNIT ( $, .STERADIAN. ) SOLID_ANGLE_UNIT ( ) );
#80683 = DIRECTION ( 'NONE',  ( 0.000000000000000000, 0.000000000000000000, -1.000000000000000000 ) ) ;
#80684 = CARTESIAN_POINT ( 'NONE',  ( -16.85308237588828106, -59.99999999999999289, 39.91134413746445375 ) ) ;
#80685 = CARTESIAN_POINT ( 'NONE',  ( 11.48763805786517800, 14.98694146577114950, 9.807607930316668998 ) ) ;
#80686 = CIRCLE ( 'NONE', #103119, 5.000000000000011546 ) ;
#80687 = CARTESIAN_POINT ( 'NONE',  ( -86.84973327953595401, -28.04380161740479949, 186.3552575792517416 ) ) ;
#80688 = EDGE_LOOP ( 'NONE', ( #10370, #57475, #29777, #101635 ) ) ;
#80689 = CARTESIAN_POINT ( 'NONE',  ( 17.50000000000256506, 49.16280683614454716, 62.52714020843568221 ) ) ;
#80690 = CARTESIAN_POINT ( 'NONE',  ( 36.88942319598261577, 438.8974264175596431, 23.87252030258318669 ) ) ;
#80691 = CARTESIAN_POINT ( 'NONE',  ( -14.82749242237660425, -56.88391391158748434, 33.50551569215675585 ) ) ;
#80694 = EDGE_CURVE ( 'NONE', #18717, #10704, #8710, .T. ) ;
#80693 = CARTESIAN_POINT ( 'NONE',  ( 40.21603221112102489, 460.7694907478772848, 2.143794914364641535 ) ) ;
#80692 = CARTESIAN_POINT ( 'NONE',  ( 2.241046694639375669, -6.576374040525785780, -6.171384342982555893 ) ) ;
#80695 = B_SPLINE_CURVE_WITH_KNOTS ( 'NONE', 3,
 ( #66397, #17339, #50214, #75005 ),
 .UNSPECIFIED., .F., .F.,
 ( 4, 4 ),
 ( 0.000000000000000000, 0.001346487449956073213 ),
 .UNSPECIFIED. ) ;
#80696 = VERTEX_POINT ( 'NONE', #96324 ) ;
#80697 = DIRECTION ( 'NONE',  ( -1.000000000000000000, -0.000000000000000000, -0.000000000000000000 ) ) ;
#80698 = AXIS2_PLACEMENT_3D ( 'NONE', #103649, #21704, #106278 ) ;
#80699 = CARTESIAN_POINT ( 'NONE',  ( -5.692357205181195035, -4.313020517848788593, -16.93296622887996961 ) ) ;
#80700 = CARTESIAN_POINT ( 'NONE',  ( 0.000000000000000000, -4.000000000000003553, 27.00000000000000000 ) ) ;
#80701 = DIRECTION ( 'NONE',  ( 1.000000000000000000, 1.224606353822377258E-16, 0.000000000000000000 ) ) ;
#80702 = CARTESIAN_POINT ( 'NONE',  ( -7.896254658894418021, -81.21070817245801265, 1.307282859663298158 ) ) ;
#80703 = CARTESIAN_POINT ( 'NONE',  ( 73.32284281756166422, -59.99999999999999289, 165.4600895165735039 ) ) ;
#80704 = CARTESIAN_POINT ( 'NONE',  ( 53.78349330513380266, -1.232595164407830946E-29, 4.000000000000007105 ) ) ;
#80705 = ORIENTED_EDGE ( 'NONE', *, *, #3134, .F. ) ;
#80706 = CARTESIAN_POINT ( 'NONE',  ( -42.80417301746779657, 434.8807528697725502, 8.723038671918009967 ) ) ;
#80707 = B_SPLINE_CURVE_WITH_KNOTS ( 'NONE', 3,
 ( #26226, #83876, #33226, #56926, #73099, #82277, #42355, #15956, #106012, #17033, #75242, #8389, #17571, #32158, #90376, #25693, #16489, #65572, #66101, #90920, #34303, #74179 ),
 .UNSPECIFIED., .F., .F.,
 ( 4, 2, 2, 2, 2, 2, 2, 2, 2, 2, 4 ),
 ( 0.006818712227115011036, 0.007321396069163314813, 0.007824079911211617722, 0.008326763753259920631, 0.008829447595308225274, 0.009080789516332376729, 0.009332131437356529918, 0.009583473358380681373, 0.009834815279404836297, 0.01033749912145313921, 0.01084018296350144211 ),
 .UNSPECIFIED. ) ;
#80709 = CARTESIAN_POINT ( 'NONE',  ( -38.47428897412184767, 485.7788508071988645, -4.770630528146724281 ) ) ;
#80708 = CARTESIAN_POINT ( 'NONE',  ( 37.39695856105412730, -59.99999999999995737, 52.44754946039245880 ) ) ;
#80710 = CARTESIAN_POINT ( 'NONE',  ( 4.284822031654965890, -1.092833614412281218, 104.4267991316945086 ) ) ;
#80711 = EDGE_CURVE ( 'NONE', #87062, #16434, #69911, .T. ) ;
#80712 = COLOUR_RGB ( '', 0.08235294, 0.09019608, 0.10196078) ;
#80713 = CARTESIAN_POINT ( 'NONE',  ( -4.999999999999993783, -3.737948356800065319, 102.2532056550983128 ) ) ;
#80714 = ORIENTED_EDGE ( 'NONE', *, *, #84416, .T. ) ;
#80715 = CARTESIAN_POINT ( 'NONE',  ( -30.15664824853507398, 323.6649206493684687, 14.81758955126313637 ) ) ;
#80716 = EDGE_LOOP ( 'NONE', ( #22154, #35866, #104993, #60711, #197, #81610 ) ) ;
#80718 = FACE_OUTER_BOUND ( 'NONE', #76003, .T. ) ;
#80717 =( BOUNDED_CURVE ( )  B_SPLINE_CURVE ( 2, ( #51737, #42056, #74942 ),
 .UNSPECIFIED., .F., .F. ) 
 B_SPLINE_CURVE_WITH_KNOTS ( ( 3, 3 ),
 ( 0.000000000000000000, 1.000000000000000000 ),
 .UNSPECIFIED. ) 
 CURVE ( )  GEOMETRIC_REPRESENTATION_ITEM ( )  RATIONAL_B_SPLINE_CURVE ( ( 1.000000000000000000, 1.857142857142858317, 1.000000000000000000 ) ) 
 REPRESENTATION_ITEM ( '' )  );
#80719 = EDGE_CURVE ( 'NONE', #32552, #38588, #3586, .T. ) ;
#80720 = DIRECTION ( 'NONE',  ( 0.5735764363510462704, 0.8191520442889915765, 0.000000000000000000 ) ) ;
#80721 = EDGE_LOOP ( 'NONE', ( #8656, #11914, #65611, #44799, #30225 ) ) ;
#80722 = CARTESIAN_POINT ( 'NONE',  ( 5.000000000000000000, -14.11573700085330074, 9.475244962104019564 ) ) ;
#80723 = CARTESIAN_POINT ( 'NONE',  ( -113.7384774196253971, -60.00000000001956835, 185.5332954700592438 ) ) ;
#80724 = CARTESIAN_POINT ( 'NONE',  ( 44.08482021419140295, 485.1618240760802792, 0.4493778471356573712 ) ) ;
#80725 = CARTESIAN_POINT ( 'NONE',  ( 38.69880557139828881, -59.99999999999998579, 50.34886149390489152 ) ) ;
#80726 = DIRECTION ( 'NONE',  ( -1.000000000000000000, -0.000000000000000000, -0.000000000000000000 ) ) ;
#80727 = CARTESIAN_POINT ( 'NONE',  ( 41.08349330513380693, 1.593028355512270567E-15, 0.000000000000000000 ) ) ;
#80729 = CARTESIAN_POINT ( 'NONE',  ( 9.346812867641324019, -53.39685740252094348, 32.79285266721333159 ) ) ;
#80728 = CARTESIAN_POINT ( 'NONE',  ( -105.8556346142475064, -14.21045842199439946, 186.2197870760574290 ) ) ;
#80730 = EDGE_CURVE ( 'NONE', #2579, #87282, #87694, .T. ) ;
#80731 = AXIS2_PLACEMENT_3D ( 'NONE', #44062, #68340, #18209 ) ;
#80732 = CARTESIAN_POINT ( 'NONE',  ( 82.45662180681927111, -37.99999999999996447, 14.43516799643988868 ) ) ;
#80733 = CARTESIAN_POINT ( 'NONE',  ( 0.3332995494436070127, 54.28974409543867097, -7.792324729589695131 ) ) ;
#80734 = CARTESIAN_POINT ( 'NONE',  ( -47.73610249163328945, -32.60741693219772230, 45.16641798069752411 ) ) ;
#80735 = CARTESIAN_POINT ( 'NONE',  ( -1.012641722624960217, 34.34730419169671478, -29.25075072817579169 ) ) ;
#80736 = VERTEX_POINT ( 'NONE', #95256 ) ;
#80737 = EDGE_CURVE ( 'NONE', #100740, #5108, #54761, .T. ) ;
#80738 = DIRECTION ( 'NONE',  ( -1.000000000000000000, -1.224606353822377258E-16, -0.000000000000000000 ) ) ;
#80739 = VECTOR ( 'NONE', #34546, 1000.000000000000000 ) ;
#80740 = CARTESIAN_POINT ( 'NONE',  ( 61.11682663846713837, -1.232595164407830946E-29, 4.000000000000007105 ) ) ;
#80741 = CARTESIAN_POINT ( 'NONE',  ( -4.971301086608930220, -62.51774646881273867, 12.85295273510877934 ) ) ;
#80742 = CYLINDRICAL_SURFACE ( 'NONE', #35279, 15.00000000000000711 ) ;
#80743 = CARTESIAN_POINT ( 'NONE',  ( 11.86977464456163922, 303.5920060571866088, -10.05522031238126424 ) ) ;
#80744 = CARTESIAN_POINT ( 'NONE',  ( 30.12932728364529922, 334.4140447340107585, 17.11298374841474867 ) ) ;
#80745 = ORIENTED_EDGE ( 'NONE', *, *, #72906, .F. ) ;
#80746 = ORIENTED_EDGE ( 'NONE', *, *, #37711, .T. ) ;
#80747 = B_SPLINE_CURVE_WITH_KNOTS ( 'NONE', 3,
 ( #36276, #102560, #61588, #89437 ),
 .UNSPECIFIED., .F., .F.,
 ( 4, 4 ),
 ( 0.000000000000000000, 1.000000000000000000 ),
 .UNSPECIFIED. ) ;
#80748 = CARTESIAN_POINT ( 'NONE',  ( 83.22744612763000305, -29.99999999997350741, 195.7235398707221634 ) ) ;
#80749 = DIRECTION ( 'NONE',  ( -1.000000000000000000, -1.224606353822377258E-16, -0.000000000000000000 ) ) ;
#80750 = EDGE_CURVE ( 'NONE', #8828, #88306, #100025, .T. ) ;
#80751 = CARTESIAN_POINT ( 'NONE',  ( 6.434574498933689490, 41.95046769211187865, -59.72043363588650067 ) ) ;
#80752 = CARTESIAN_POINT ( 'NONE',  ( -29.99397490504469133, 1.005902684993158047, -14.99698745252234033 ) ) ;
#80753 = CARTESIAN_POINT ( 'NONE',  ( 100.5470196648521153, -29.99999999999999645, 159.8114828581198026 ) ) ;
#80754 = CARTESIAN_POINT ( 'NONE',  ( -21.64906249285503392, 304.1279031160725026, 9.996121053679246415 ) ) ;
#80755 = ORIENTED_EDGE ( 'NONE', *, *, #37106, .F. ) ;
#80756 =( GEOMETRIC_REPRESENTATION_CONTEXT ( 3 ) GLOBAL_UNCERTAINTY_ASSIGNED_CONTEXT ( ( #100166 ) ) GLOBAL_UNIT_ASSIGNED_CONTEXT ( ( #51119, #3120, #36064 ) ) REPRESENTATION_CONTEXT ( 'NONE', 'WORKASPACE' ) );
#80757 = ORIENTED_EDGE ( 'NONE', *, *, #46650, .T. ) ;
#80758 = B_SPLINE_CURVE_WITH_KNOTS ( 'NONE', 3,
 ( #39989, #41045, #105770, #24881, #23292, #49113, #57735, #66375, #15169, #97670, #23836, #91211, #10, #8136, #82013, #32450, #56681, #97145, #49657, #15697, #65322, #98210, #90659, #24363, #80958, #89603, #48586, #72862, #7592, #7073 ),
 .UNSPECIFIED., .F., .F.,
 ( 4, 2, 2, 2, 2, 2, 2, 2, 2, 2, 2, 2, 2, 2, 4 ),
 ( 0.0006904739626665574049, 0.001153765004792713707, 0.001617056046918869793, 0.002543638131171178061, 0.003470220215423487631, 0.004396802299675795465, 0.005323384383928104167, 0.005786675426054258518, 0.006249966468180413737, 0.006713257510306568088, 0.006944903031369652202, 0.007176548552432735449, 0.007408194073495819564, 0.007639839594558903678, 0.008103130636685064100 ),
 .UNSPECIFIED. ) ;
#80759 = VERTEX_POINT ( 'NONE', #103342 ) ;
#80761 = VECTOR ( 'NONE', #32824, 1000.000000000000000 ) ;
#80760 = DIRECTION ( 'NONE',  ( -1.000000000000000000, 0.000000000000000000, 0.000000000000000000 ) ) ;
#80762 = CARTESIAN_POINT ( 'NONE',  ( 21.96335440039715436, 25.92421299530558798, 31.83099838201997756 ) ) ;
#80764 = EDGE_LOOP ( 'NONE', ( #22011, #66010, #5867, #85215, #41959 ) ) ;
#80763 = AXIS2_PLACEMENT_3D ( 'NONE', #77, #65914, #97209 ) ;
#80765 = DIRECTION ( 'NONE',  ( -0.000000000000000000, 0.000000000000000000, -1.000000000000000000 ) ) ;
#80766 = PRESENTATION_LAYER_ASSIGNMENT (  '', '', ( #101414 ) ) ;
#80767 = VERTEX_POINT ( 'NONE', #21388 ) ;
#80768 = DIRECTION ( 'NONE',  ( 0.000000000000000000, 0.000000000000000000, 1.000000000000000000 ) ) ;
#80769 = CARTESIAN_POINT ( 'NONE',  ( 79.90910546643618773, -38.77530854556393791, 192.8225656864368034 ) ) ;
#80770 = CARTESIAN_POINT ( 'NONE',  ( 12.80519380915450078, 6.532562108030647074, 7.664627944857000053 ) ) ;
#80771 = CARTESIAN_POINT ( 'NONE',  ( 85.42134923721152973, -52.71934788913637959, 0.1208844820147615962 ) ) ;
#80772 = CARTESIAN_POINT ( 'NONE',  ( 86.96752660269400792, -37.99999999999972999, 188.7629342415843610 ) ) ;
#80773 = CARTESIAN_POINT ( 'NONE',  ( 38.82779737621938665, 321.9597977506067537, 16.55577433839140156 ) ) ;
#80774 = VECTOR ( 'NONE', #84334, 1000.000000000000000 ) ;
#80775 = B_SPLINE_CURVE_WITH_KNOTS ( 'NONE', 3,
 ( #67774, #99050, #25768, #91526, #100660, #16025, #33298, #25216, #26821, #33837, #74781, #34379, #106623, #7925, #59693, #49982, #67252, #40830, #100130, #24677, #73720, #98531 ),
 .UNSPECIFIED., .F., .F.,
 ( 4, 2, 2, 2, 2, 2, 2, 2, 2, 2, 4 ),
 ( 0.003156676467191279339, 0.003660387902065995007, 0.004164099336940710674, 0.004667810771815426342, 0.005171522206690142009, 0.005423377924127489869, 0.005675233641564837728, 0.005927089359002185587, 0.006178945076439534313, 0.006682656511314223093, 0.007186367946188911872 ),
 .UNSPECIFIED. ) ;
#80776 = SURFACE_STYLE_USAGE ( .BOTH. , #105586 ) ;
#80777 = AXIS2_PLACEMENT_3D ( 'NONE', #17384, #82630, #59435 ) ;
#80778 = SURFACE_STYLE_USAGE ( .BOTH. , #103471 ) ;
#80779 = CARTESIAN_POINT ( 'NONE',  ( -4.581218816254734705, -47.80086643547572578, 103.5404609598622443 ) ) ;
#80780 = ADVANCED_FACE ( 'NONE', ( #36523 ), #65545, .T. ) ;
#80781 = DIRECTION ( 'NONE',  ( -0.8191520442889975717, 0.000000000000000000, -0.5735764363510378328 ) ) ;
#80782 = DIRECTION ( 'NONE',  ( 0.000000000000000000, 0.000000000000000000, 1.000000000000000000 ) ) ;
#80783 = ORIENTED_EDGE ( 'NONE', *, *, #10147, .T. ) ;
#80784 = CARTESIAN_POINT ( 'NONE',  ( -43.21649601278601693, 436.3330504929538165, 19.41248623753216407 ) ) ;
#80785 = CIRCLE ( 'NONE', #72174, 13.50000000000000000 ) ;
#80786 = CARTESIAN_POINT ( 'NONE',  ( -31.43357885710805633, 299.6859785502570048, 11.02347074399675186 ) ) ;
#80787 = CARTESIAN_POINT ( 'NONE',  ( -12.42907082493785076, -4.067133856147437498, -76.73301493501935511 ) ) ;
#80788 = UNCERTAINTY_MEASURE_WITH_UNIT (LENGTH_MEASURE( 1.000000000000000082E-05 ), #50578, 'distance_accuracy_value', 'NONE');
#80789 = DIRECTION ( 'NONE',  ( 0.000000000000000000, 0.000000000000000000, 1.000000000000000000 ) ) ;
#80790 = CARTESIAN_POINT ( 'NONE',  ( 3.313708498984762052, -16.71874999999999289, -8.000000000000000000 ) ) ;
#80791 = CARTESIAN_POINT ( 'NONE',  ( 10.39775555965807285, -20.26676808020434706, 35.38161163148800625 ) ) ;
#80792 = EDGE_CURVE ( 'NONE', #68971, #78587, #58691, .T. ) ;
#80793 =( GEOMETRIC_REPRESENTATION_CONTEXT ( 3 ) GLOBAL_UNCERTAINTY_ASSIGNED_CONTEXT ( ( #46923 ) ) GLOBAL_UNIT_ASSIGNED_CONTEXT ( ( #70827, #62742, #54607 ) ) REPRESENTATION_CONTEXT ( 'NONE', 'WORKASPACE' ) );
#80794 = ORIENTED_EDGE ( 'NONE', *, *, #80650, .T. ) ;
#80795 = CARTESIAN_POINT ( 'NONE',  ( 83.43892566183167503, -60.98069388147631287, 191.4419204983608438 ) ) ;
#80796 =( NAMED_UNIT ( * ) PLANE_ANGLE_UNIT ( ) SI_UNIT ( $, .RADIAN. ) );
#80797 = DIRECTION ( 'NONE',  ( 0.000000000000000000, -1.000000000000000000, 0.000000000000000000 ) ) ;
#80798 = ORIENTED_EDGE ( 'NONE', *, *, #52759, .F. ) ;
#80799 = CARTESIAN_POINT ( 'NONE',  ( 94.19775022482500049, -57.67256254209210908, 22.65169980652741799 ) ) ;
#80800 = DIRECTION ( 'NONE',  ( -1.000000000000000000, -1.224606353822377258E-16, -0.000000000000000000 ) ) ;
#80801 = DIRECTION ( 'NONE',  ( 0.000000000000000000, 1.000000000000000000, 0.000000000000000000 ) ) ;
#80802 = DIRECTION ( 'NONE',  ( -0.000000000000000000, -1.000000000000000000, -0.000000000000000000 ) ) ;
#80803 = ADVANCED_FACE ( 'NONE', ( #41246 ), #72029, .T. ) ;
#80804 = CARTESIAN_POINT ( 'NONE',  ( -84.85721030251472996, -37.99999999999993605, 182.1326420535735906 ) ) ;
#80805 = CARTESIAN_POINT ( 'NONE',  ( -8.000000000000000000, -4.999999999999998224, 2.094395098902548824 ) ) ;
#80806 = DIRECTION ( 'NONE',  ( -1.000000000000000000, -1.224606353822377258E-16, -0.000000000000000000 ) ) ;
#80807 = AXIS2_PLACEMENT_3D ( 'NONE', #66211, #7964, #81844 ) ;
#80809 = CARTESIAN_POINT ( 'NONE',  ( -10.52472853799489094, 10.25003985121227856, 10.32210089392438412 ) ) ;
#80808 = FACE_BOUND ( 'NONE', #56796, .T. ) ;
#80810 = EDGE_LOOP ( 'NONE', ( #57638, #4298, #21811 ) ) ;
#80811 = EDGE_CURVE ( 'NONE', #56333, #97465, #8351, .T. ) ;
#80812 = FILL_AREA_STYLE ('',( #15550 ) ) ;
#80813 = CARTESIAN_POINT ( 'NONE',  ( -15.66240720622342053, 43.86916268644461070, -6.198733367779965420 ) ) ;
#80814 = CARTESIAN_POINT ( 'NONE',  ( -27.26388916004784235, 36.55153124001466836, -10.05698433968606054 ) ) ;
#80815 = CARTESIAN_POINT ( 'NONE',  ( 9.571198553003402054, 15.30040232763730756, -2.918503601030738359 ) ) ;
#80816 = FACE_OUTER_BOUND ( 'NONE', #75322, .T. ) ;
#80817 = VECTOR ( 'NONE', #57862, 1000.000000000000000 ) ;
#80818 = AXIS2_PLACEMENT_3D ( 'NONE', #86515, #28829, #43892 ) ;
#80819 = LINE ( 'NONE', #6930, #41550 ) ;
#80820 = ORIENTED_EDGE ( 'NONE', *, *, #27054, .T. ) ;
#80821 = DIRECTION ( 'NONE',  ( 0.000000000000000000, 0.000000000000000000, -1.000000000000000000 ) ) ;
#80822 = CARTESIAN_POINT ( 'NONE',  ( 4.478476647430158941, -64.72647920817954059, 3.992942460563209117 ) ) ;
#80825 = EDGE_CURVE ( 'NONE', #34834, #39269, #86275, .T. ) ;
#80824 = CARTESIAN_POINT ( 'NONE',  ( -49.54934986436142452, -21.77002013510745115, -25.65681709438414160 ) ) ;
#80823 = FILL_AREA_STYLE ('',( #21565 ) ) ;
#80826 = ORIENTED_EDGE ( 'NONE', *, *, #34188, .T. ) ;
#80827 = AXIS2_PLACEMENT_3D ( 'NONE', #289, #6823, #73134 ) ;
#80828 = ORIENTED_EDGE ( 'NONE', *, *, #74349, .T. ) ;
#80829 =( GEOMETRIC_REPRESENTATION_CONTEXT ( 3 ) GLOBAL_UNCERTAINTY_ASSIGNED_CONTEXT ( ( #12692 ) ) GLOBAL_UNIT_ASSIGNED_CONTEXT ( ( #65789, #24298, #57147 ) ) REPRESENTATION_CONTEXT ( 'NONE', 'WORKASPACE' ) );
#80830 = CARTESIAN_POINT ( 'NONE',  ( 11.07247204453428147, 43.17212549673661925, -15.14411814079721452 ) ) ;
#80831 = CARTESIAN_POINT ( 'NONE',  ( -3.528928113779644438, 5.468125903023618228, 1.934623251528821186E-15 ) ) ;
#80832 = CARTESIAN_POINT ( 'NONE',  ( -92.38785827711156173, -59.99999999999999289, 0.3159652731796530611 ) ) ;
#80833 = EDGE_LOOP ( 'NONE', ( #62474, #78100, #81319, #63240 ) ) ;
#80834 = CARTESIAN_POINT ( 'NONE',  ( -2.414679174385195903E-15, -5.469921996229795802, 3.525817189091422055 ) ) ;
#80835 = CARTESIAN_POINT ( 'NONE',  ( -76.12537862032631608, -38.35598417008158378, -28.58435412235099804 ) ) ;
#80836 = CARTESIAN_POINT ( 'NONE',  ( -3.352941176470600304, -1.200583151104954283, 104.5794940929807524 ) ) ;
#80838 = DIRECTION ( 'NONE',  ( -0.000000000000000000, 1.000000000000000000, -0.000000000000000000 ) ) ;
#80837 = CARTESIAN_POINT ( 'NONE',  ( -16.75187969033554936, -1.200000000000000030E-05, -24.30698433968596106 ) ) ;
#80839 = AXIS2_PLACEMENT_3D ( 'NONE', #94974, #3825, #70679 ) ;
#80840 = ADVANCED_FACE ( 'NONE', ( #80632 ), #81163, .T. ) ;
#80841 = CARTESIAN_POINT ( 'NONE',  ( -81.31780443015183835, -46.44658433287104060, 165.0995960706320034 ) ) ;
#80842 = VERTEX_POINT ( 'NONE', #42305 ) ;
#80843 = VERTEX_POINT ( 'NONE', #100540 ) ;
#80844 = ORIENTED_EDGE ( 'NONE', *, *, #62503, .F. ) ;
#80845 = DIRECTION ( 'NONE',  ( 0.5735764363510490460, 0.8191520442889896891, 0.000000000000000000 ) ) ;
#80846 = EDGE_CURVE ( 'NONE', #52343, #88800, #75191, .T. ) ;
#80847 = CARTESIAN_POINT ( 'NONE',  ( -5.000000000000161648, -12.33523449218733958, 10.71643274012945568 ) ) ;
#80848 = ORIENTED_EDGE ( 'NONE', *, *, #46795, .F. ) ;
#80849 = DIRECTION ( 'NONE',  ( -0.000000000000000000, 1.000000000000000000, 0.000000000000000000 ) ) ;
#80850 = CARTESIAN_POINT ( 'NONE',  ( -50.10796912846466000, 53.37899725327127953, 25.05398456423233000 ) ) ;
#80851 = CARTESIAN_POINT ( 'NONE',  ( -113.9839795500101332, -57.67115229137139210, 179.6907882865009185 ) ) ;
#80852 = CARTESIAN_POINT ( 'NONE',  ( -4.503026011213025370, -65.54341862283317255, 3.965236350746919047 ) ) ;
#80853 = CIRCLE ( 'NONE', #32626, 5.000000000000000888 ) ;
#80854 = DIRECTION ( 'NONE',  ( -0.000000000000000000, -0.000000000000000000, 1.000000000000000000 ) ) ;
#80855 = LINE ( 'NONE', #32873, #102863 ) ;
#80856 = CARTESIAN_POINT ( 'NONE',  ( 0.000000000000000000, -99.99999999999997158, 0.000000000000000000 ) ) ;
#80857 = CARTESIAN_POINT ( 'NONE',  ( -47.47011933289886088, -14.21045842199439946, -33.05967481147064291 ) ) ;
#80858 = ADVANCED_FACE ( 'NONE', ( #18057 ), #53526, .F. ) ;
#80859 = CARTESIAN_POINT ( 'NONE',  ( -20.43766876253514653, -14.21045842199441012, 34.90391904204521012 ) ) ;
#80860 = CARTESIAN_POINT ( 'NONE',  ( -53.92306173273154002, -25.63130525233928481, 52.72527914939674787 ) ) ;
#80861 = VECTOR ( 'NONE', #38975, 1000.000000000000000 ) ;
#80862 = CARTESIAN_POINT ( 'NONE',  ( 3.866921754057069283, 18.90974295178000730, -5.835322522795916456 ) ) ;
#80863 = ORIENTED_EDGE ( 'NONE', *, *, #62948, .F. ) ;
#80864 = CARTESIAN_POINT ( 'NONE',  ( -100.4547888263544024, -60.28510889581524879, 195.5192978447599614 ) ) ;
#80865 = CARTESIAN_POINT ( 'NONE',  ( -3.010187908185308903, 299.5653876365528845, -10.00571708631421686 ) ) ;
#80866 = CIRCLE ( 'NONE', #98119, 5.000000000000001776 ) ;
#80867 = ORIENTED_EDGE ( 'NONE', *, *, #80046, .F. ) ;
#80869 = B_SPLINE_CURVE_WITH_KNOTS ( 'NONE', 3,
 ( #79248, #64150, #4839, #95976 ),
 .UNSPECIFIED., .F., .F.,
 ( 4, 4 ),
 ( 0.000000000000000000, 0.0002092826938412524983 ),
 .UNSPECIFIED. ) ;
#80868 = CARTESIAN_POINT ( 'NONE',  ( -17.25401547865008212, 43.52747190215453088, 4.305687115457426550 ) ) ;
#80870 = CARTESIAN_POINT ( 'NONE',  ( 108.2055158922219817, -38.35604994730526585, 139.2463622293343519 ) ) ;
#80871 = DIRECTION ( 'NONE',  ( -1.000000000000000000, -1.224606353822377258E-16, -0.000000000000000000 ) ) ;
#80872 = CARTESIAN_POINT ( 'NONE',  ( 9.113097280746996987, -54.00000000000000711, 31.11721482942554928 ) ) ;
#80873 = ADVANCED_FACE ( 'NONE', ( #60125, #51987 ), #9387, .F. ) ;
#80874 = CARTESIAN_POINT ( 'NONE',  ( -11.99473552897978124, 294.5867349183714623, 1.880683768558506719 ) ) ;
#80875 = CARTESIAN_POINT ( 'NONE',  ( 10.39117206796836257, 1.272551561242683764E-15, -8.500000000000000000 ) ) ;
#80876 = CARTESIAN_POINT ( 'NONE',  ( 80.78126285191066813, -30.00000000000000355, 138.7691592692428912 ) ) ;
#80877 = CARTESIAN_POINT ( 'NONE',  ( 20.37278541768183615, 303.8378246129572631, -10.00297115033342266 ) ) ;
#80878 = CARTESIAN_POINT ( 'NONE',  ( 37.83989825151484609, 491.6297408768497803, 12.44743998625087933 ) ) ;
#80879 = DIRECTION ( 'NONE',  ( 0.000000000000000000, -1.000000000000000000, 0.000000000000000000 ) ) ;
#80880 = CARTESIAN_POINT ( 'NONE',  ( 98.31310517497099966, 1.030564683017419500E-14, 0.000000000000000000 ) ) ;
#80881 = ORIENTED_EDGE ( 'NONE', *, *, #78532, .T. ) ;
#80882 = VERTEX_POINT ( 'NONE', #16986 ) ;
#80883 = CARTESIAN_POINT ( 'NONE',  ( 50.29923733747742887, -36.04821958570228446, 50.07162713147780408 ) ) ;
#80884 = CARTESIAN_POINT ( 'NONE',  ( 5.660419746013990228, 41.80469037513988440, -58.87109516261954667 ) ) ;
#80885 = CIRCLE ( 'NONE', #82586, 8.000000000000000000 ) ;
#80886 = CARTESIAN_POINT ( 'NONE',  ( -6.996281870428058269, 16.99350475219344148, -0.2643931112039912268 ) ) ;
#80887 = ORIENTED_EDGE ( 'NONE', *, *, #56013, .T. ) ;
#80888 = CARTESIAN_POINT ( 'NONE',  ( -104.8255383870086632, -38.39704354203259840, 197.6632266025270894 ) ) ;
#80889 = VERTEX_POINT ( 'NONE', #59039 ) ;
#80890 = CARTESIAN_POINT ( 'NONE',  ( 90.79437873324295083, -38.35012829369840404, 19.27249926157240978 ) ) ;
#80891 = CARTESIAN_POINT ( 'NONE',  ( 10.36448145403546839, 10.96207040866273630, -10.43058775967166873 ) ) ;
#80892 = DIRECTION ( 'NONE',  ( 1.000000000000000000, -0.000000000000000000, 1.224646799147353207E-16 ) ) ;
#80893 = DIRECTION ( 'NONE',  ( -0.000000000000000000, -0.000000000000000000, -1.000000000000000000 ) ) ;
#80894 = CARTESIAN_POINT ( 'NONE',  ( 104.8029988399297423, -52.71705893269023591, 161.0984590988129526 ) ) ;
#80895 = CARTESIAN_POINT ( 'NONE',  ( -32.17889379758943846, 439.3695696554026426, 23.63219374846804044 ) ) ;
#80896 = STYLED_ITEM ( 'NONE', ( #71105 ), #89529 ) ;
#80897 = CARTESIAN_POINT ( 'NONE',  ( 0.000000000000000000, 195.0000000000000000, 0.000000000000000000 ) ) ;
#80898 = CARTESIAN_POINT ( 'NONE',  ( -30.72294868208370744, 313.4051624346869289, -7.977499477794275151 ) ) ;
#80899 = DIRECTION ( 'NONE',  ( -0.000000000000000000, 1.000000000000000000, -0.000000000000000000 ) ) ;
#80900 = CARTESIAN_POINT ( 'NONE',  ( -29.99999999999997158, 486.7667864837128491, 5.222266633581357453 ) ) ;
#80901 = CARTESIAN_POINT ( 'NONE',  ( 82.53461625975002391, -60.00000000000002132, 198.4989634257764237 ) ) ;
#80902 = CARTESIAN_POINT ( 'NONE',  ( -15.96643448957893874, 35.08561881503606372, 22.07017619469237246 ) ) ;
#80903 = ORIENTED_EDGE ( 'NONE', *, *, #23770, .F. ) ;
#80904 = CARTESIAN_POINT ( 'NONE',  ( 57.59701642329373072, -36.02025670668500368, 64.66622269765490216 ) ) ;
#80905 = CARTESIAN_POINT ( 'NONE',  ( -33.52989424313292233, 300.6882358251922369, -0.6863093620646967263 ) ) ;
#80906 = EDGE_CURVE ( 'NONE', #88610, #82973, #81077, .T. ) ;
#80907 = CARTESIAN_POINT ( 'NONE',  ( 9.677525045153895888, -50.98682064026158400, 24.47381311117452185 ) ) ;
#80908 = AXIS2_PLACEMENT_3D ( 'NONE', #73288, #32347, #42001 ) ;
#80909 = CARTESIAN_POINT ( 'NONE',  ( 23.86650669486618881, 0.000000000000000000, 4.000000000000000888 ) ) ;
#80910 = EDGE_LOOP ( 'NONE', ( #7471, #49346, #51572, #22104, #20541 ) ) ;
#80912 = DIRECTION ( 'NONE',  ( -1.000000000000000000, 0.000000000000000000, 0.000000000000000000 ) ) ;
#80911 = CARTESIAN_POINT ( 'NONE',  ( -90.66174681505526678, -38.34313144972409759, 8.451963012734573510 ) ) ;
#80913 = DIRECTION ( 'NONE',  ( 0.1270361284032104077, 0.9918980905719715357, 0.000000000000000000 ) ) ;
#80914 = CARTESIAN_POINT ( 'NONE',  ( 30.13443748760208862, 331.7808586020135522, 15.50310796814377845 ) ) ;
#80915 = DIRECTION ( 'NONE',  ( 0.000000000000000000, 1.000000000000000000, 0.000000000000000000 ) ) ;
#80916 = AXIS2_PLACEMENT_3D ( 'NONE', #41278, #73633, #89840 ) ;
#80917 = CARTESIAN_POINT ( 'NONE',  ( 5.656854249492380582, -34.81249999999999289, -5.656854249492379694 ) ) ;
#80918 = PRESENTATION_STYLE_ASSIGNMENT (( #16723 ) ) ;
#80919 = EDGE_CURVE ( 'NONE', #101499, #97355, #60406, .T. ) ;
#80920 =( NAMED_UNIT ( * ) SI_UNIT ( $, .STERADIAN. ) SOLID_ANGLE_UNIT ( ) );
#80921 = STYLED_ITEM ( 'NONE', ( #64074 ), #32799 ) ;
#80922 = VERTEX_POINT ( 'NONE', #91926 ) ;
#80923 = CARTESIAN_POINT ( 'NONE',  ( 85.99887890796605916, -18.43241006622161748, 165.6326649775408839 ) ) ;
#80924 = CARTESIAN_POINT ( 'NONE',  ( 3.158718764008467961, -10.09043921932089205, -11.69018217342268251 ) ) ;
#80925 = CARTESIAN_POINT ( 'NONE',  ( -34.07401144359369738, 439.5803311721820705, 24.00237084771177010 ) ) ;
#80926 = ORIENTED_EDGE ( 'NONE', *, *, #88501, .T. ) ;
#80927 = CARTESIAN_POINT ( 'NONE',  ( 12.21253585067004543, 6.123233995736770227E-16, -5.000000000000002665 ) ) ;
#80928 = CARTESIAN_POINT ( 'NONE',  ( 7.579218993349996936, -5.000000000006481038, -17.00320663867185900 ) ) ;
#80929 = DIRECTION ( 'NONE',  ( 1.000000000000000000, 1.224606353822377258E-16, 0.000000000000000000 ) ) ;
#80930 = CARTESIAN_POINT ( 'NONE',  ( 14.68532172035349959, 1.589195250043442087, -3.050719247005512003 ) ) ;
#80931 = DIRECTION ( 'NONE',  ( 0.7071067811865521247, 0.000000000000000000, -0.7071067811865430208 ) ) ;
#80932 = CARTESIAN_POINT ( 'NONE',  ( -33.00000000000000000, 450.0000000000002274, -1.797577426246302013 ) ) ;
#80933 = EDGE_CURVE ( 'NONE', #37996, #79894, #63864, .T. ) ;
#80934 = ORIENTED_EDGE ( 'NONE', *, *, #55419, .T. ) ;
#80935 = STYLED_ITEM ( 'NONE', ( #23945 ), #77775 ) ;
#80936 = CARTESIAN_POINT ( 'NONE',  ( 6.499999999999999112, -4.076778466486165264, -6.121917890101378212 ) ) ;
#80937 = CARTESIAN_POINT ( 'NONE',  ( 0.3380568183126133053, 26.06491301246339987, 38.28514637226837891 ) ) ;
#80939 = CARTESIAN_POINT ( 'NONE',  ( -11.10308954262782599, 8.426119584744682811, -9.821132823669547207 ) ) ;
#80938 = DIRECTION ( 'NONE',  ( 0.000000000000000000, 0.000000000000000000, 1.000000000000000000 ) ) ;
#80940 = CIRCLE ( 'NONE', #8569, 7.499999999992679633 ) ;
#80941 = CARTESIAN_POINT ( 'NONE',  ( -7.188101187500000044, -10.90625000204838457, -8.802885111219163269E-16 ) ) ;
#80942 = CARTESIAN_POINT ( 'NONE',  ( -28.98628617572742527, 14.82338180310327225, -41.90038909576689008 ) ) ;
#80943 = CARTESIAN_POINT ( 'NONE',  ( 57.45015997180046696, -1.232595164407830946E-29, 4.000000000000007105 ) ) ;
#80944 = AXIS2_PLACEMENT_3D ( 'NONE', #47674, #14778, #6691 ) ;
#80946 = VERTEX_POINT ( 'NONE', #43907 ) ;
#80945 = B_SPLINE_CURVE_WITH_KNOTS ( 'NONE', 3,
 ( #8784, #49233, #82138, #25000, #67573, #99918, #9837, #49777, #32568, #74046, #1194, #66491 ),
 .UNSPECIFIED., .F., .F.,
 ( 4, 2, 2, 2, 2, 4 ),
 ( 0.000000000000000000, 0.0008601990320054680138, 0.001720398064010936028, 0.002580597096016404041, 0.003010696612019150842, 0.003440796128021898076 ),
 .UNSPECIFIED. ) ;
#80947 = LINE ( 'NONE', #7056, #101264 ) ;
#80948 = CARTESIAN_POINT ( 'NONE',  ( -8.734619362698921918, 132.0311980842794526, -2.602085213900631332E-15 ) ) ;
#80949 = CARTESIAN_POINT ( 'NONE',  ( 0.000000000000000000, 6.123233995736770227E-16, -5.000000000000002665 ) ) ;
#80950 = DIRECTION ( 'NONE',  ( 1.000000000000000000, 0.000000000000000000, 0.000000000000000000 ) ) ;
#80951 = ORIENTED_EDGE ( 'NONE', *, *, #58298, .F. ) ;
#80952 = CARTESIAN_POINT ( 'NONE',  ( -28.99999999999998934, 1.102182119232617714E-15, -9.000000000000000000 ) ) ;
#80953 = VERTEX_POINT ( 'NONE', #76266 ) ;
#80954 = SURFACE_STYLE_USAGE ( .BOTH. , #7587 ) ;
#80955 = CARTESIAN_POINT ( 'NONE',  ( 39.08667504521158520, 48.00000000000000000, -56.76470588235294912 ) ) ;
#80956 = PRESENTATION_STYLE_ASSIGNMENT (( #88013 ) ) ;
#80957 = CARTESIAN_POINT ( 'NONE',  ( -106.4884117741187595, -60.00000000000000000, 119.4417209971499290 ) ) ;
#80958 = CARTESIAN_POINT ( 'NONE',  ( 29.14598918812165351, 18.82621124954753000, -39.72463063980563902 ) ) ;
#80959 = CARTESIAN_POINT ( 'NONE',  ( 2.641326394094752755E-05, -39.47608681191096736, 30.46899776158753426 ) ) ;
#80960 = CARTESIAN_POINT ( 'NONE',  ( -7.117280438721564906, 3.124991324735574061, 14.67116533570241188 ) ) ;
#80962 = CARTESIAN_POINT ( 'NONE',  ( 35.48628994100678824, 491.6413678155948332, 12.45547902532423379 ) ) ;
#80961 = CARTESIAN_POINT ( 'NONE',  ( -6.043427762771337086, -5.000000000000002665, -74.51456333905269958 ) ) ;
#80963 = CARTESIAN_POINT ( 'NONE',  ( -86.10701541242173107, -18.36965636274899083, 167.2037440504452661 ) ) ;
#80964 = ORIENTED_EDGE ( 'NONE', *, *, #19163, .F. ) ;
#80965 =( LENGTH_UNIT ( ) NAMED_UNIT ( * ) SI_UNIT ( .MILLI., .METRE. ) );
#80966 = EDGE_LOOP ( 'NONE', ( #48805, #58909, #100363, #36812, #50114 ) ) ;
#80967 = CARTESIAN_POINT ( 'NONE',  ( 11.08349330513380160, -4.000000000000000000, 4.898587196589415787E-16 ) ) ;
#80968 = ADVANCED_FACE ( 'NONE', ( #50915 ), #69022, .T. ) ;
#80969 = CARTESIAN_POINT ( 'NONE',  ( 33.21587117940961775, 465.5376284999449581, 9.463823683337858839 ) ) ;
#80970 = CARTESIAN_POINT ( 'NONE',  ( 25.11650669486618881, 4.898587196589411843E-16, -4.000000000000000888 ) ) ;
#80971 = EDGE_CURVE ( 'NONE', #74005, #47858, #43139, .T. ) ;
#80972 = CARTESIAN_POINT ( 'NONE',  ( -6.928203230275507885, -64.73520732746426631, 4.000000000000002665 ) ) ;
#80973 = CARTESIAN_POINT ( 'NONE',  ( 4.259258436597560760, 11.59113387677236595, -5.000000000000000000 ) ) ;
#80974 = CARTESIAN_POINT ( 'NONE',  ( -5.782971157185549771, -5.000000000000000000, -96.70384082256207137 ) ) ;
#80975 = FACE_OUTER_BOUND ( 'NONE', #59622, .T. ) ;
#80976 = CARTESIAN_POINT ( 'NONE',  ( 114.2391797980453276, -59.99999999999998579, 181.3573912910646015 ) ) ;
#80977 = VECTOR ( 'NONE', #67179, 999.9999999999998863 ) ;
#80978 = EDGE_CURVE ( 'NONE', #10704, #70423, #20793, .T. ) ;
#80979 = CARTESIAN_POINT ( 'NONE',  ( -108.8021899934185086, -29.99999999999995026, 184.6878429379334534 ) ) ;
#80980 = CARTESIAN_POINT ( 'NONE',  ( -63.23540892387794088, -18.63157451083668903, 70.70009706107828151 ) ) ;
#80981 = ORIENTED_EDGE ( 'NONE', *, *, #23819, .F. ) ;
#80982 = CARTESIAN_POINT ( 'NONE',  ( 0.4964154566687934422, 8.859816792613651515, -0.6543471694412386075 ) ) ;
#80983 = CARTESIAN_POINT ( 'NONE',  ( 95.12161555340847485, -59.99999999999024425, -7.142421816251681044 ) ) ;
#80984 = ORIENTED_EDGE ( 'NONE', *, *, #10539, .F. ) ;
#80985 = CARTESIAN_POINT ( 'NONE',  ( 1.007147449337442158, -42.95369000350973465, 31.04859829352065503 ) ) ;
#80986 = CARTESIAN_POINT ( 'NONE',  ( 4.401442555609581635E-16, -13.15625000204838280, -7.188101187500000044 ) ) ;
#80987 = ORIENTED_EDGE ( 'NONE', *, *, #65294, .T. ) ;
#80988 = CARTESIAN_POINT ( 'NONE',  ( 36.54984892593326151, 463.9827100737089722, 19.61538121061435547 ) ) ;
#80989 = ORIENTED_EDGE ( 'NONE', *, *, #43514, .F. ) ;
#80990 = FACE_OUTER_BOUND ( 'NONE', #73419, .T. ) ;
#80991 = CARTESIAN_POINT ( 'NONE',  ( -2.977408999572650039, -29.56250000204838813, -7.188101187500000933 ) ) ;
#80992 = CARTESIAN_POINT ( 'NONE',  ( -96.14679540281859715, -59.99999999999994316, 202.5905596799929356 ) ) ;
#80993 = CARTESIAN_POINT ( 'NONE',  ( -4.245164436738296132, -1.071807799196663913, 104.4592797835085349 ) ) ;
#80994 = CARTESIAN_POINT ( 'NONE',  ( 7.188101187500000044, -28.53125000204838813, 0.000000000000000000 ) ) ;
#80996 = EDGE_CURVE ( 'NONE', #95890, #8224, #82786, .T. ) ;
#80995 = AXIS2_PLACEMENT_3D ( 'NONE', #41777, #58505, #49864 ) ;
#80997 = CARTESIAN_POINT ( 'NONE',  ( 45.99999999999997158, 463.0783855722254430, 8.172228418139317441 ) ) ;
#80998 = CARTESIAN_POINT ( 'NONE',  ( -6.366267295126388781, 53.78408749334437999, -6.625582353314952044 ) ) ;
#80999 = CARTESIAN_POINT ( 'NONE',  ( 53.78349330513380266, 4.000000000000013323, 0.000000000000000000 ) ) ;
#81000 = CIRCLE ( 'NONE', #55, 7.499999999992679633 ) ;
#81001 = CARTESIAN_POINT ( 'NONE',  ( 1.836601268058450879E-15, 1.005902684993156715, 14.99698745252234566 ) ) ;
#81002 = CARTESIAN_POINT ( 'NONE',  ( -7.150053860865850375, 106.7826545391397843, 3.590189269391291571 ) ) ;
#81003 = CARTESIAN_POINT ( 'NONE',  ( -43.67706251530178463, 402.9872697375532766, 16.14665223012086415 ) ) ;
#81004 = CARTESIAN_POINT ( 'NONE',  ( 102.3020614934086723, -59.99999999999993605, 193.7906591577538222 ) ) ;
#81005 = CARTESIAN_POINT ( 'NONE',  ( -31.69449164194474022, -29.08087705339919538, 31.86155386896254171 ) ) ;
#81006 = CARTESIAN_POINT ( 'NONE',  ( -37.72161557782784058, 461.3708194167276702, 2.611246763486743117 ) ) ;
#81007 = CARTESIAN_POINT ( 'NONE',  ( 41.32804380067809547, -42.97744930290995313, 40.63765321593970725 ) ) ;
#81008 = CARTESIAN_POINT ( 'NONE',  ( 17.78317311657530553, -8.673617379884035472E-16, -13.66642973271117256 ) ) ;
#81009 = ORIENTED_EDGE ( 'NONE', *, *, #8471, .T. ) ;
#81010 = CARTESIAN_POINT ( 'NONE',  ( 6.692588830498429786, -7.935834885954432316, -0.04058884017440450576 ) ) ;
#81011 = AXIS2_PLACEMENT_3D ( 'NONE', #76142, #1162, #69146 ) ;
#81012 = CARTESIAN_POINT ( 'NONE',  ( -68.03595486504397627, -38.33397274148195777, 125.6715106722867148 ) ) ;
#81013 = ORIENTED_EDGE ( 'NONE', *, *, #20547, .T. ) ;
#81015 = DIRECTION ( 'NONE',  ( 0.5735764363510554853, 0.8191520442889852482, 0.000000000000000000 ) ) ;
#81014 = CARTESIAN_POINT ( 'NONE',  ( 9.087744254835127933, -4.999999999999999112, -17.48834560249285985 ) ) ;
#81016 = DIRECTION ( 'NONE',  ( 0.000000000000000000, 0.000000000000000000, -1.000000000000000000 ) ) ;
#81017 = CARTESIAN_POINT ( 'NONE',  ( -6.913779242700420546, 41.73441082398074542, -59.30275289623196500 ) ) ;
#81018 = CARTESIAN_POINT ( 'NONE',  ( 1.093953403843523242, 43.39644527504638916, -18.11016995274446373 ) ) ;
#81019 = CARTESIAN_POINT ( 'NONE',  ( 0.000000000000000000, -48.79941684889506348, 112.0000000000000000 ) ) ;
#81020 = CARTESIAN_POINT ( 'NONE',  ( -31.42312704992726680, 414.9721857482184646, 24.35715877706864774 ) ) ;
#81021 = DIRECTION ( 'NONE',  ( 0.000000000000000000, 0.000000000000000000, 1.000000000000000000 ) ) ;
#81022 = VECTOR ( 'NONE', #66679, 1000.000000000000000 ) ;
#81023 = CARTESIAN_POINT ( 'NONE',  ( 95.28179702667202378, -60.00000000000000711, 51.05854659839798870 ) ) ;
#81024 = DIRECTION ( 'NONE',  ( -1.000000000000000000, -1.224606353822377258E-16, -0.000000000000000000 ) ) ;
#81025 = FACE_BOUND ( 'NONE', #92737, .T. ) ;
#81026 = CARTESIAN_POINT ( 'NONE',  ( 8.641101172573151246, -5.000000000000001776, -72.37542516944607485 ) ) ;
#81027 = VERTEX_POINT ( 'NONE', #18599 ) ;
#81028 = EDGE_CURVE ( 'NONE', #58745, #71083, #34547, .T. ) ;
#81029 = CARTESIAN_POINT ( 'NONE',  ( -83.78196859787340145, -29.99999999999755929, -22.07823983344261976 ) ) ;
#81030 = ORIENTED_EDGE ( 'NONE', *, *, #22619, .F. ) ;
#81031 = CARTESIAN_POINT ( 'NONE',  ( -3.415272820067190462, -49.17042331394952726, 103.8818871663241339 ) ) ;
#81032 = CARTESIAN_POINT ( 'NONE',  ( -15.92744347757545853, 3.245128719852651056, -1.809264762054266562 ) ) ;
#81033 = CARTESIAN_POINT ( 'NONE',  ( 8.763392006745778673, 19.59990099439108135, 0.000000000000000000 ) ) ;
#81034 = DIRECTION ( 'NONE',  ( -1.000000000000000000, -0.000000000000000000, -0.000000000000000000 ) ) ;
#81035 = CARTESIAN_POINT ( 'NONE',  ( 9.220915120640583496, 28.95545113567915507, -3.870126578504840431 ) ) ;
#81036 = CARTESIAN_POINT ( 'NONE',  ( -5.082755093536326818, -24.59375000204838813, 5.082755093536325042 ) ) ;
#81037 = CONICAL_SURFACE ( 'NONE', #29516, 4.172000000000009479, 0.9599310885968813656 ) ;
#81038 = FACE_OUTER_BOUND ( 'NONE', #44150, .T. ) ;
#81040 = EDGE_CURVE ( 'NONE', #55434, #5546, #87956, .T. ) ;
#81039 = CARTESIAN_POINT ( 'NONE',  ( 7.004291983109769859, 40.56179000455576045, -71.01843131752761451 ) ) ;
#81041 = EDGE_CURVE ( 'NONE', #95250, #99083, #96577, .T. ) ;
#81042 = ORIENTED_EDGE ( 'NONE', *, *, #90069, .T. ) ;
#81043 = AXIS2_PLACEMENT_3D ( 'NONE', #77601, #5309, #52245 ) ;
#81045 = ORIENTED_EDGE ( 'NONE', *, *, #52011, .T. ) ;
#81044 = DIRECTION ( 'NONE',  ( 1.000000000000000000, 1.224606353822377258E-16, 0.000000000000000000 ) ) ;
#81046 = CARTESIAN_POINT ( 'NONE',  ( 81.37985195669844529, -32.56063285680090047, 146.8991821570098182 ) ) ;
#81047 = CARTESIAN_POINT ( 'NONE',  ( 14.46400437354099644, 2.949852469114451647, -3.921916857588237715 ) ) ;
#81048 = VERTEX_POINT ( 'NONE', #75738 ) ;
#81049 = CARTESIAN_POINT ( 'NONE',  ( -59.92177854689752792, 50.00000000000000711, -19.49351526723193473 ) ) ;
#81050 = CARTESIAN_POINT ( 'NONE',  ( 7.150931910075641440, -86.78625798522261903, -3.588457848165358843 ) ) ;
#81051 = CARTESIAN_POINT ( 'NONE',  ( -2.977408999572650039, -15.68750000204838635, -7.188101187500000933 ) ) ;
#81052 = CARTESIAN_POINT ( 'NONE',  ( 7.934883677559678716, 26.13160822062449995, 1.051380792122691421 ) ) ;
#81053 = ADVANCED_FACE ( 'NONE', ( #83298 ), #27227, .T. ) ;
#81054 =( BOUNDED_SURFACE ( )  B_SPLINE_SURFACE ( 3, 2, ( 
 ( #67647, #16972, #50900 ),
 ( #82213, #100526, #57400 ),
 ( #92427, #50371, #75177 ),
 ( #26687, #59023, #203 ),
 ( #34240, #74646, #83282 ),
 ( #33167, #59560, #91910 ),
 ( #18583, #51444, #7788 ),
 ( #40694, #73583, #106486 ),
 ( #32643, #65514, #98402 ),
 ( #24554, #25076, #57934 ),
 ( #58489, #90856, #49848 ),
 ( #730, #33696, #66570 ),
 ( #35843, #12045, #61153 ),
 ( #60634, #78381, #19668 ),
 ( #52505, #95118, #44977 ),
 ( #53581, #94039, #2885 ) ),
 .UNSPECIFIED., .F., .F., .T. ) 
 B_SPLINE_SURFACE_WITH_KNOTS ( ( 4, 2, 2, 2, 2, 2, 2, 4 ),
 ( 3, 3 ),
 ( 2.630274470449833757E-16, 0.0005221599045739626225, 0.001044319809147662217, 0.001566479713721361921, 0.002088639618295061624, 0.002610799522868761328, 0.003132959427442461031, 0.004177279236589860438 ),
 ( 0.000000000000000000, 1.000000000000000000 ),
 .UNSPECIFIED. ) 
 GEOMETRIC_REPRESENTATION_ITEM ( )  RATIONAL_B_SPLINE_SURFACE ( (
 ( 1.000000000000000000, 0.8909749942926979971, 1.000000000000000000),
 ( 1.000000000000000000, 0.8947619310247098001, 1.000000000000000000),
 ( 1.000000000000000000, 0.8978044232673220160, 1.000000000000000000),
 ( 1.000000000000000000, 0.9023043032728860213, 1.000000000000000000),
 ( 1.000000000000000000, 0.9037672509134783150, 1.000000000000000000),
 ( 1.000000000000000000, 0.9049062503963291038, 1.000000000000000000),
 ( 1.000000000000000000, 0.9045936109743369924, 1.000000000000000000),
 ( 1.000000000000000000, 0.9022616022707382610, 1.000000000000000000),
 ( 1.000000000000000000, 0.9002067130764697112, 1.000000000000000000),
 ( 1.000000000000000000, 0.8945795303826531431, 1.000000000000000000),
 ( 1.000000000000000000, 0.8910211780037325946, 1.000000000000000000),
 ( 1.000000000000000000, 0.8825640046898904911, 1.000000000000000000),
 ( 1.000000000000000000, 0.8776492255290634370, 1.000000000000000000),
 ( 1.000000000000000000, 0.8615337984044251218, 1.000000000000000000),
 ( 1.000000000000000000, 0.8487841387214820621, 1.000000000000000000),
 ( 1.000000000000000000, 0.8347624811021875368, 1.000000000000000000) ) ) 
 REPRESENTATION_ITEM ( '' )  SURFACE ( )  );
#81055 = CARTESIAN_POINT ( 'NONE',  ( -31.30247466046573379, -57.68739127208316120, 46.06264550376279487 ) ) ;
#81056 = CARTESIAN_POINT ( 'NONE',  ( 16.33222328768405163, 294.5674815784677776, 1.876697781737655779 ) ) ;
#81057 = ADVANCED_FACE ( 'NONE', ( #41126 ), #39550, .T. ) ;
#81058 = VERTEX_POINT ( 'NONE', #16306 ) ;
#81059 = CIRCLE ( 'NONE', #3553, 2.999999999999981792 ) ;
#81060 = SURFACE_STYLE_FILL_AREA ( #71378 ) ;
#81061 = FACE_OUTER_BOUND ( 'NONE', #19029, .T. ) ;
#81062 = CARTESIAN_POINT ( 'NONE',  ( 36.68673791898589087, 18.64284798592620618, -11.44574982650785167 ) ) ;
#81063 = EDGE_CURVE ( 'NONE', #91446, #27343, #27701, .T. ) ;
#81064 = DIRECTION ( 'NONE',  ( -1.000000000000000000, -1.224606353822377258E-16, -0.000000000000000000 ) ) ;
#81065 = EDGE_LOOP ( 'NONE', ( #24074, #76393, #48090, #30732 ) ) ;
#81066 = CARTESIAN_POINT ( 'NONE',  ( 5.656854249492378806, -14.37500000409677092, 5.656854249492381470 ) ) ;
#81067 = CARTESIAN_POINT ( 'NONE',  ( -16.31924431152875954, -15.65188151249610371, 31.57746562531465173 ) ) ;
#81068 = CARTESIAN_POINT ( 'NONE',  ( -37.83989825152028885, 491.6297408768477339, 12.44743998624950798 ) ) ;
#81069 = CARTESIAN_POINT ( 'NONE',  ( 32.83703342409250325, 465.7129651006319477, 11.08653443108778092 ) ) ;
#81070 = EDGE_CURVE ( 'NONE', #54954, #106311, #77711, .T. ) ;
#81071 = CARTESIAN_POINT ( 'NONE',  ( -3.594033448928638741, -9.156975712238445197, 6.225088131883843801 ) ) ;
#81072 = CARTESIAN_POINT ( 'NONE',  ( 0.000000000000000000, 0.000000000000000000, 0.000000000000000000 ) ) ;
#81073 = SHAPE_DEFINITION_REPRESENTATION ( #27828, #88164 ) ;
#81074 = CARTESIAN_POINT ( 'NONE',  ( -8.507502983303869115, -14.15209590839079290, 15.87009613063079883 ) ) ;
#81075 = ORIENTED_EDGE ( 'NONE', *, *, #78201, .F. ) ;
#81076 = CARTESIAN_POINT ( 'NONE',  ( -6.784314825330817200, -48.10473606785564726, 39.24654408518340887 ) ) ;
#81077 = CIRCLE ( 'NONE', #3576, 4.000000000000000000 ) ;
#81078 = CARTESIAN_POINT ( 'NONE',  ( -3.884543032214208491, 15.13241195026071928, 9.216463528758552570 ) ) ;
#81079 = CARTESIAN_POINT ( 'NONE',  ( 45.36923076923077502, 1.411358822780289120E-15, 0.000000000000000000 ) ) ;
#81080 = AXIS2_PLACEMENT_3D ( 'NONE', #9001, #92054, #83429 ) ;
#81081 = CARTESIAN_POINT ( 'NONE',  ( 72.73175990828099202, -38.32562016310332353, -30.13089435840664976 ) ) ;
#81082 = CARTESIAN_POINT ( 'NONE',  ( -53.08935917470201815, -30.00000000000000000, 52.21147893555080799 ) ) ;
#81083 =( LENGTH_UNIT ( ) NAMED_UNIT ( * ) SI_UNIT ( .MILLI., .METRE. ) );
#81084 = ORIENTED_EDGE ( 'NONE', *, *, #38504, .T. ) ;
#81085 = VECTOR ( 'NONE', #31387, 1000.000000000000000 ) ;
#81086 = CARTESIAN_POINT ( 'NONE',  ( 2.500000000000001776, -30.00000000000000000, -14.79019945774903633 ) ) ;
#81087 = CARTESIAN_POINT ( 'NONE',  ( 91.21982970888714704, -57.61350775420689274, 204.2106347837803071 ) ) ;
#81088 = PRESENTATION_LAYER_ASSIGNMENT (  '', '', ( #41525 ) ) ;
#81090 = CARTESIAN_POINT ( 'NONE',  ( 35.51382444471309441, 463.4141161792265962, 19.91564417027522538 ) ) ;
#81089 = AXIS2_PLACEMENT_3D ( 'NONE', #67415, #100291, #59319 ) ;
#81091 = CARTESIAN_POINT ( 'NONE',  ( -9.781457975134252081, 51.26649664470197365, -3.093893760390039827 ) ) ;
#81092 = CARTESIAN_POINT ( 'NONE',  ( 23.38163988287269390, 40.83906611472318815, 60.94087333791210170 ) ) ;
#81093 = CARTESIAN_POINT ( 'NONE',  ( -73.91169935318824002, -60.00000000000000000, 171.3249817331451084 ) ) ;
#81094 = CARTESIAN_POINT ( 'NONE',  ( -45.31383884518383098, 362.9196860876334085, 5.161789940898600548 ) ) ;
#81095 =( NAMED_UNIT ( * ) SI_UNIT ( $, .STERADIAN. ) SOLID_ANGLE_UNIT ( ) );
#81096 = CARTESIAN_POINT ( 'NONE',  ( -40.73878143178837519, 486.4834083601638213, 16.46716573231486436 ) ) ;
#81097 = CARTESIAN_POINT ( 'NONE',  ( -86.40020525432112208, -17.50209429613323309, 178.3865162827522113 ) ) ;
#81098 = ORIENTED_EDGE ( 'NONE', *, *, #86062, .T. ) ;
#81099 = CARTESIAN_POINT ( 'NONE',  ( 28.97004836423603535, 308.1417733683699112, -9.028218307027925604 ) ) ;
#81100 = VERTEX_POINT ( 'NONE', #80502 ) ;
#81101 = CARTESIAN_POINT ( 'NONE',  ( 3.250000000000015987, -5.629165124598843661, 1.734723475976807094E-15 ) ) ;
#81102 = ADVANCED_FACE ( 'NONE', ( #31990, #7670 ), #56211, .T. ) ;
#81103 = CARTESIAN_POINT ( 'NONE',  ( -111.8964183755431918, 22.97884757028484870, -55.94820918777161722 ) ) ;
#81104 = CARTESIAN_POINT ( 'NONE',  ( -84.37622072227169667, -52.73398876249148515, -14.54299705149653832 ) ) ;
#81105 = CIRCLE ( 'NONE', #94923, 5.000000000000001776 ) ;
#81106 = CARTESIAN_POINT ( 'NONE',  ( 63.81650669486618455, 4.000000000000015099, 4.898587196589422689E-16 ) ) ;
#81107 = CARTESIAN_POINT ( 'NONE',  ( 4.000000000000000000, 4.898587196589412829E-16, -6.838999999999999524 ) ) ;
#81108 = VERTEX_POINT ( 'NONE', #89148 ) ;
#81109 = VECTOR ( 'NONE', #42261, 1000.000000000000000 ) ;
#81110 = CARTESIAN_POINT ( 'NONE',  ( 27.26387865205136762, 36.83098680558968852, -7.556984339686136920 ) ) ;
#81111 = CARTESIAN_POINT ( 'NONE',  ( 13.92251770464348937, 2.731537496222212535, -5.554657554294999855 ) ) ;
#81112 = EDGE_CURVE ( 'NONE', #91653, #100209, #14706, .T. ) ;
#81113 = CARTESIAN_POINT ( 'NONE',  ( -13.60704923275180711, -1.734723475976807094E-15, 10.45706415777857679 ) ) ;
#81114 = DIRECTION ( 'NONE',  ( 0.000000000000000000, -1.000000000000000000, 0.000000000000000000 ) ) ;
#81115 = EDGE_CURVE ( 'NONE', #49442, #3603, #24451, .T. ) ;
#81116 = CARTESIAN_POINT ( 'NONE',  ( 89.32114860119857269, -29.99999999999995026, 17.89867789164953393 ) ) ;
#81117 = AXIS2_PLACEMENT_3D ( 'NONE', #9005, #76396, #41911 ) ;
#81118 = CARTESIAN_POINT ( 'NONE',  ( -76.02915898839707154, -49.90876059677169962, 133.3426292687217369 ) ) ;
#81119 = EDGE_LOOP ( 'NONE', ( #67347, #48284, #39980, #87485 ) ) ;
#81120 = CARTESIAN_POINT ( 'NONE',  ( 94.39688282193469604, -57.61984102425716969, 204.5389246678256256 ) ) ;
#81121 = CARTESIAN_POINT ( 'NONE',  ( 28.35788784190019385, 34.17668351136055804, 8.951742554474883207 ) ) ;
#81122 = CARTESIAN_POINT ( 'NONE',  ( 38.87647009787237806, 310.5762796638829855, 1.738341351311467387 ) ) ;
#81123 = ADVANCED_FACE ( 'NONE', ( #48137 ), #105330, .T. ) ;
#81124 = DIRECTION ( 'NONE',  ( 0.000000000000000000, -1.000000000000000000, 0.000000000000000000 ) ) ;
#81125 = VERTEX_POINT ( 'NONE', #57284 ) ;
#81126 = CYLINDRICAL_SURFACE ( 'NONE', #54355, 66.50000000000000000 ) ;
#81127 = CARTESIAN_POINT ( 'NONE',  ( 0.000000000000000000, 0.000000000000000000, -0.7256075382097185722 ) ) ;
#81128 = CARTESIAN_POINT ( 'NONE',  ( -2.977408999572650039, -21.68750000204838813, -7.188101187500001821 ) ) ;
#81129 = EDGE_CURVE ( 'NONE', #74216, #88975, #49198, .T. ) ;
#81130 = EDGE_CURVE ( 'NONE', #10915, #84815, #63945, .T. ) ;
#81131 = LINE ( 'NONE', #48749, #22327 ) ;
#81132 = CARTESIAN_POINT ( 'NONE',  ( 6.326416241096634252, -1.324101276589547238, -6.831531844319973956 ) ) ;
#81133 = CARTESIAN_POINT ( 'NONE',  ( 0.6437396368863147478, 35.01890123696630042, 27.41570566740858794 ) ) ;
#81134 = CARTESIAN_POINT ( 'NONE',  ( -16.96000587140901317, 45.76999459631175426, -4.188133835394263649 ) ) ;
#81135 = VECTOR ( 'NONE', #28014, 999.9999999999998863 ) ;
#81136 = EDGE_LOOP ( 'NONE', ( #98248, #50479, #74852, #37014 ) ) ;
#81137 = CARTESIAN_POINT ( 'NONE',  ( 0.2595206531158508190, 2.531175536751804067, 6.499999999999995559 ) ) ;
#81139 = CARTESIAN_POINT ( 'NONE',  ( 28.78019115065667322, -18.63880091324738686, 29.02949882689319949 ) ) ;
#81138 = CARTESIAN_POINT ( 'NONE',  ( -20.43766876253514653, -14.21045842199441012, 34.90391904204521012 ) ) ;
#81140 = CARTESIAN_POINT ( 'NONE',  ( -4.963060401946981948, 52.14582460415977749, -6.071815141832103357 ) ) ;
#81141 = ORIENTED_EDGE ( 'NONE', *, *, #19941, .F. ) ;
#81142 = VERTEX_POINT ( 'NONE', #40062 ) ;
#81143 = DIRECTION ( 'NONE',  ( -1.000000000000000000, -1.224606353822377258E-16, -0.000000000000000000 ) ) ;
#81144 = DIRECTION ( 'NONE',  ( 0.000000000000000000, 0.000000000000000000, -1.000000000000000000 ) ) ;
#81145 = DIRECTION ( 'NONE',  ( -1.000000000000000000, 0.000000000000000000, 0.000000000000000000 ) ) ;
#81146 = LINE ( 'NONE', #56329, #62160 ) ;
#81147 = DIRECTION ( 'NONE',  ( 0.5735764363510491570, -0.8191520442889895781, 1.003171929053522035E-16 ) ) ;
#81148 = CARTESIAN_POINT ( 'NONE',  ( 0.000000000000000000, 4.898587196589412829E-16, -4.000000000000000000 ) ) ;
#81149 = ORIENTED_EDGE ( 'NONE', *, *, #93544, .T. ) ;
#81150 = CARTESIAN_POINT ( 'NONE',  ( 49.67928414888689304, -59.99999999999997868, -37.96746462862734006 ) ) ;
#81151 = CARTESIAN_POINT ( 'NONE',  ( 82.06105073464702571, -29.99999999999996447, 146.2738422045464119 ) ) ;
#81153 = CARTESIAN_POINT ( 'NONE',  ( -83.13706915486389448, -45.33804393721257497, -14.25701659862332171 ) ) ;
#81152 = VECTOR ( 'NONE', #74010, 1000.000000000000000 ) ;
#81154 = CARTESIAN_POINT ( 'NONE',  ( 71.80342808059909032, -30.00000000000000000, -19.71766482350836469 ) ) ;
#81155 = VECTOR ( 'NONE', #39679, 1000.000000000000000 ) ;
#81156 = CARTESIAN_POINT ( 'NONE',  ( 46.79100380508914725, 13.36652303332992275, -15.81652940118055284 ) ) ;
#81157 = ORIENTED_EDGE ( 'NONE', *, *, #30734, .F. ) ;
#81158 = ORIENTED_EDGE ( 'NONE', *, *, #26243, .F. ) ;
#81159 = EDGE_LOOP ( 'NONE', ( #34784, #40629, #87691, #9559 ) ) ;
#81160 = SURFACE_SIDE_STYLE ('',( #64991 ) ) ;
#81161 = DIRECTION ( 'NONE',  ( 1.000000000000000000, 0.000000000000000000, -1.160749806054361473E-16 ) ) ;
#81162 = SURFACE_SIDE_STYLE ('',( #106502 ) ) ;
#81163 = CYLINDRICAL_SURFACE ( 'NONE', #32834, 8.000000000000000000 ) ;
#81165 = CIRCLE ( 'NONE', #57056, 1.000000000000000222 ) ;
#81164 = CARTESIAN_POINT ( 'NONE',  ( -43.06478785906146811, 345.9681365877381154, 10.01537130693817623 ) ) ;
#81166 = CARTESIAN_POINT ( 'NONE',  ( -3.410363394089228173, -69.13634986858798470, 13.41598603787099186 ) ) ;
#81167 = CARTESIAN_POINT ( 'NONE',  ( -46.00000000000572697, 486.0748346210346540, 1.693312618872886866 ) ) ;
#81168 = CARTESIAN_POINT ( 'NONE',  ( 7.724940478959218106E-16, 0.6351314446025488891, -6.500000000000000888 ) ) ;
#81169 = ORIENTED_EDGE ( 'NONE', *, *, #93001, .T. ) ;
#81171 = EDGE_CURVE ( 'NONE', #16558, #59167, #43215, .T. ) ;
#81170 = CARTESIAN_POINT ( 'NONE',  ( -9.147602679903698686, 44.02377986342360572, 13.63549886291783508 ) ) ;
#81172 = AXIS2_PLACEMENT_3D ( 'NONE', #42463, #83453, #66209 ) ;
#81173 = VERTEX_POINT ( 'NONE', #105846 ) ;
#81174 = DIRECTION ( 'NONE',  ( 0.000000000000000000, -1.000000000000000000, 0.000000000000000000 ) ) ;
#81175 = CARTESIAN_POINT ( 'NONE',  ( -6.499999999999999112, -3.752776749732587902, -6.064240316920403551 ) ) ;
#81176 = CARTESIAN_POINT ( 'NONE',  ( 18.58349330513380337, 1.593028355512270567E-15, 0.000000000000000000 ) ) ;
#81177 = CARTESIAN_POINT ( 'NONE',  ( -32.81683603912411229, -59.99999999999996447, 37.99185413034007297 ) ) ;
#81178 = CARTESIAN_POINT ( 'NONE',  ( 66.48165699634022019, -32.53116164569385660, 86.87811383088407524 ) ) ;
#81179 = ORIENTED_EDGE ( 'NONE', *, *, #41458, .T. ) ;
#81180 = CARTESIAN_POINT ( 'NONE',  ( 41.13675135394154836, 465.3862164892198052, 16.49847611935184943 ) ) ;
#81181 = CARTESIAN_POINT ( 'NONE',  ( -6.880652008360423899, 9.211763961707752912, 1.310808761845548620 ) ) ;
#81182 = CARTESIAN_POINT ( 'NONE',  ( 0.000000000000000000, 0.000000000000000000, 63.00000000000000000 ) ) ;
#81183 = ORIENTED_EDGE ( 'NONE', *, *, #46512, .T. ) ;
#81184 = CARTESIAN_POINT ( 'NONE',  ( 47.57405721301110901, 17.76112721455492505, 14.43871205879827180 ) ) ;
#81185 = AXIS2_PLACEMENT_3D ( 'NONE', #47569, #88054, #5529 ) ;
#81186 = CARTESIAN_POINT ( 'NONE',  ( -36.65209206386415275, 491.4469928998125852, 12.33162904370220225 ) ) ;
#81187 = AXIS2_PLACEMENT_3D ( 'NONE', #17701, #922, #82954 ) ;
#81188 = CARTESIAN_POINT ( 'NONE',  ( -5.656854249492379694, -30.12500000409677270, -5.656854249492380582 ) ) ;
#81189 = CARTESIAN_POINT ( 'NONE',  ( 2.617993873628172263, -5.000000000000000000, -10.00000000000000000 ) ) ;
#81190 = CARTESIAN_POINT ( 'NONE',  ( 31.14131030317610538, 3.851859888774471706E-31, 5.000000000000001776 ) ) ;
#81191 = DIRECTION ( 'NONE',  ( 0.000000000000000000, -1.000000000000000000, 0.000000000000000000 ) ) ;
#81192 = EDGE_CURVE ( 'NONE', #55214, #67654, #23915, .T. ) ;
#81193 = CARTESIAN_POINT ( 'NONE',  ( 9.381394091586571449, 32.01349605581611257, 3.465950112474259992 ) ) ;
#81194 = CARTESIAN_POINT ( 'NONE',  ( 13.50000000000000355, 7.794228634059978233, -1.205771365940065953 ) ) ;
#81195 = ORIENTED_EDGE ( 'NONE', *, *, #47799, .F. ) ;
#81196 = CARTESIAN_POINT ( 'NONE',  ( 38.09999999999998721, 0.000000000000000000, 3.309499999999999886 ) ) ;
#81197 = CARTESIAN_POINT ( 'NONE',  ( -3.313708498984760276, -10.53124999999999289, -8.000000000000000000 ) ) ;
#81198 = CARTESIAN_POINT ( 'NONE',  ( 4.309564269304543949, -60.00000000000002132, 39.63068050932632502 ) ) ;
#81199 = CARTESIAN_POINT ( 'NONE',  ( -96.89808418466809314, -29.99999999999999645, 191.1144671784673505 ) ) ;
#81200 = CARTESIAN_POINT ( 'NONE',  ( -40.85715431133397146, 485.0116719597020847, -3.999197217707391339 ) ) ;
#81201 = CARTESIAN_POINT ( 'NONE',  ( 50.53031853463637901, -57.67793883620915807, 78.60926899548999813 ) ) ;
#81202 = CARTESIAN_POINT ( 'NONE',  ( -0.3344869795709685123, 26.06211867389157177, -38.29264199900394772 ) ) ;
#81203 = SHAPE_REPRESENTATION ( '14. Sleeve', ( #10728 ), #66095 ) ;
#81204 = CARTESIAN_POINT ( 'NONE',  ( 19.63219237063851352, -25.70262390305547129, -38.48832213154430093 ) ) ;
#81205 = PRODUCT_DEFINITION ( 'UNKNOWN', '', #59335, #51015 ) ;
#81206 = PRESENTATION_STYLE_ASSIGNMENT (( #98461 ) ) ;
#81207 = CARTESIAN_POINT ( 'NONE',  ( -4.221541119508299467, -59.99999999999998579, 39.63083687578825476 ) ) ;
#81208 = CARTESIAN_POINT ( 'NONE',  ( -0.3201071873350568309, -69.98621145874830063, 12.99022420585184712 ) ) ;
#81209 = CARTESIAN_POINT ( 'NONE',  ( 6.134138981404819724, 53.39921523940185466, 8.206960596703554600 ) ) ;
#81210 = CARTESIAN_POINT ( 'NONE',  ( -86.20315129297270573, -57.43435110080902462, 193.3030521547261742 ) ) ;
#81211 = AXIS2_PLACEMENT_3D ( 'NONE', #6900, #15522, #48414 ) ;
#81212 = EDGE_LOOP ( 'NONE', ( #86711, #103539, #97, #88991 ) ) ;
#81213 = CARTESIAN_POINT ( 'NONE',  ( 17.50000000000003197, 51.95328275803498741, 61.04403218098684647 ) ) ;
#81214 = CARTESIAN_POINT ( 'NONE',  ( 30.29343180852530537, 12.93058661249367702, 41.94895705695244459 ) ) ;
#81215 = CARTESIAN_POINT ( 'NONE',  ( -9.055784372474096955, -22.06795988364936534, 27.56849869070046921 ) ) ;
#81216 = FACE_OUTER_BOUND ( 'NONE', #39545, .T. ) ;
#81217 = AXIS2_PLACEMENT_3D ( 'NONE', #98564, #16595, #49486 ) ;
#81219 = CARTESIAN_POINT ( 'NONE',  ( 41.35836404316623316, 461.4284568614619388, 2.579347946915451217 ) ) ;
#81218 = CARTESIAN_POINT ( 'NONE',  ( -99.66151320157483440, -59.99999999999997158, 195.9182448172588238 ) ) ;
#81220 = ORIENTED_EDGE ( 'NONE', *, *, #61740, .T. ) ;
#81221 = DIRECTION ( 'NONE',  ( 1.000000000000000000, 0.000000000000000000, 0.000000000000000000 ) ) ;
#81222 = CARTESIAN_POINT ( 'NONE',  ( -7.499997280422835644, -2.963001255690722147, -20.99866594762864480 ) ) ;
#81223 = CARTESIAN_POINT ( 'NONE',  ( 15.49777301142466968, 34.92625999296609507, 22.93171183856468787 ) ) ;
#81224 = MECHANICAL_DESIGN_GEOMETRIC_PRESENTATION_REPRESENTATION (  '', ( #64112 ), #8940 ) ;
#81225 = CARTESIAN_POINT ( 'NONE',  ( 34.61135223818107676, 301.0186358733434986, -8.614137653301380482 ) ) ;
#81226 = CYLINDRICAL_SURFACE ( 'NONE', #63978, 5.000000000000000888 ) ;
#81227 = EDGE_CURVE ( 'NONE', #8974, #49616, #74219, .T. ) ;
#81228 = AXIS2_PLACEMENT_3D ( 'NONE', #42335, #34283, #58538 ) ;
#81229 = FILL_AREA_STYLE ('',( #89875 ) ) ;
#81230 = CARTESIAN_POINT ( 'NONE',  ( 73.10382484696803829, -60.00000000000000711, 163.4081499180699097 ) ) ;
#81231 = CARTESIAN_POINT ( 'NONE',  ( -33.63427961064055438, 325.9154870834976236, -4.827994974213513757 ) ) ;
#81232 = EDGE_LOOP ( 'NONE', ( #43332, #19564, #41241, #9797, #35552, #89061, #62837, #12058, #36507, #65738, #89303, #6326, #27621, #75563 ) ) ;
#81233 = CARTESIAN_POINT ( 'NONE',  ( -1.217592056924591271, -29.99999999999998934, 7.214394986259497600 ) ) ;
#81234 = DIRECTION ( 'NONE',  ( -1.000000000000000000, 0.000000000000000000, 0.000000000000000000 ) ) ;
#81236 = CARTESIAN_POINT ( 'NONE',  ( 4.551587301587304957, -1.200583151104947843, 104.4018401814738155 ) ) ;
#81235 = CARTESIAN_POINT ( 'NONE',  ( 43.57856552656106430, -59.99999999999991473, 62.86110226080823793 ) ) ;
#81237 = CARTESIAN_POINT ( 'NONE',  ( 14.29190075645216851, 12.99999999999999289, 0.000000000000000000 ) ) ;
#81238 = CARTESIAN_POINT ( 'NONE',  ( -4.348929473936903101, -1.784082633676044916, 103.6864098602936082 ) ) ;
#81239 = EDGE_LOOP ( 'NONE', ( #27582, #33204, #19509, #36264, #103732, #16656, #56876 ) ) ;
#81240 = CARTESIAN_POINT ( 'NONE',  ( -25.26650806423123896, 307.7638625427180727, 9.604356516990046444 ) ) ;
#81241 = EDGE_CURVE ( 'NONE', #26579, #54099, #37915, .T. ) ;
#81242 = ORIENTED_EDGE ( 'NONE', *, *, #7944, .T. ) ;
#81243 = CARTESIAN_POINT ( 'NONE',  ( -7.499174415388573091E-15, 1.500000000000000444, 61.23540616453487218 ) ) ;
#81244 = ADVANCED_FACE ( 'NONE', ( #18467 ), #96642, .T. ) ;
#81245 = SURFACE_SIDE_STYLE ('',( #23590 ) ) ;
#81246 = ORIENTED_EDGE ( 'NONE', *, *, #17436, .T. ) ;
#81247 = CARTESIAN_POINT ( 'NONE',  ( -60.62677696746903422, 48.00000000000000000, 24.18439665018601303 ) ) ;
#81248 = CARTESIAN_POINT ( 'NONE',  ( 6.459500862574912183, -11.87485980093861748, 10.39038571060456917 ) ) ;
#81250 = CARTESIAN_POINT ( 'NONE',  ( -114.5996607398657403, -60.00000000003901590, 175.3916813916542310 ) ) ;
#81249 = CONICAL_SURFACE ( 'NONE', #91601, 3.400000000000000355, 0.9599310885968748153 ) ;
#81251 = CARTESIAN_POINT ( 'NONE',  ( 6.692649149972420553, -4.003391779698787900, -6.852343209863739126 ) ) ;
#81252 = CARTESIAN_POINT ( 'NONE',  ( 51.69788177101781201, -59.99999999999997158, 76.10749672676838884 ) ) ;
#81253 = DIRECTION ( 'NONE',  ( -0.000000000000000000, 1.000000000000000000, -0.000000000000000000 ) ) ;
#81254 = DIRECTION ( 'NONE',  ( 1.000000000000000000, 0.000000000000000000, 0.000000000000000000 ) ) ;
#81255 = VECTOR ( 'NONE', #50103, 1000.000000000000000 ) ;
#81257 = CARTESIAN_POINT ( 'NONE',  ( 14.23383089391777645, -18.58706205641739828, 27.09268482856279903 ) ) ;
#81256 = CARTESIAN_POINT ( 'NONE',  ( -113.5293469826316084, -59.99999999999994316, 153.5981017735323633 ) ) ;
#81259 = CARTESIAN_POINT ( 'NONE',  ( 102.8324458336581841, -38.00000000000000000, 173.0407927310912441 ) ) ;
#81258 = UNCERTAINTY_MEASURE_WITH_UNIT (LENGTH_MEASURE( 1.000000000000000082E-05 ), #96212, 'distance_accuracy_value', 'NONE');
#81260 = CARTESIAN_POINT ( 'NONE',  ( 37.88504238421471371, 463.4171042825133213, 19.90923349043903556 ) ) ;
#81261 = CARTESIAN_POINT ( 'NONE',  ( -47.01177656439008246, -25.69492208876496164, 42.17939420022488406 ) ) ;
#81262 = CIRCLE ( 'NONE', #70973, 4.000000000000001776 ) ;
#81263 = CARTESIAN_POINT ( 'NONE',  ( 38.58349330513380693, 4.898587196589405926E-16, -4.000000000000001776 ) ) ;
#81264 = ORIENTED_EDGE ( 'NONE', *, *, #2931, .F. ) ;
#81265 = DIRECTION ( 'NONE',  ( -1.000000000000000000, 0.000000000000000000, 0.000000000000000000 ) ) ;
#81266 = CARTESIAN_POINT ( 'NONE',  ( 16.13482245078226285, 21.13350007393007601, 3.415357648796183199 ) ) ;
#81267 = CARTESIAN_POINT ( 'NONE',  ( 6.394343112843831278, -3.776352960569627104, 6.540835195019758075 ) ) ;
#81268 = CARTESIAN_POINT ( 'NONE',  ( 62.59428447264396311, 4.898587196589294500E-16, -4.000000000000007105 ) ) ;
#81269 = CARTESIAN_POINT ( 'NONE',  ( 0.000000000000000000, 1.000000000000000888, -12.00000000000003908 ) ) ;
#81270 = CARTESIAN_POINT ( 'NONE',  ( 30.24427031855517711, 312.0196691915732004, -8.325478004009855937 ) ) ;
#81271 = EDGE_LOOP ( 'NONE', ( #64781, #61578, #85281, #68966 ) ) ;
#81272 = CARTESIAN_POINT ( 'NONE',  ( 5.688569873206568595, -47.04879514976503430, 103.9352763293502022 ) ) ;
#81273 = ORIENTED_EDGE ( 'NONE', *, *, #89354, .T. ) ;
#81274 = CARTESIAN_POINT ( 'NONE',  ( 105.0447870504740848, -30.00000000000308731, 195.3166338682954972 ) ) ;
#81275 = CARTESIAN_POINT ( 'NONE',  ( 5.947848185899612616, 41.98179895519294291, -59.44139658209459043 ) ) ;
#81276 = CARTESIAN_POINT ( 'NONE',  ( 94.32107141816914009, -30.00000000000000711, 113.8930112096862644 ) ) ;
#81277 = CARTESIAN_POINT ( 'NONE',  ( 7.896165657598944065, 101.2108886862802564, -1.307894402814545387 ) ) ;
#81278 = ORIENTED_EDGE ( 'NONE', *, *, #49212, .T. ) ;
#81279 = B_SPLINE_CURVE_WITH_KNOTS ( 'NONE', 3,
 ( #13778, #62894, #14306, #87168, #22976, #47210, #104387, #14841, #54765, #5698 ),
 .UNSPECIFIED., .F., .F.,
 ( 4, 2, 2, 2, 4 ),
 ( 0.000000000000000000, 0.001993803085173306063, 0.003987606170346612126, 0.005981409255519918623, 0.007975212340693225987 ),
 .UNSPECIFIED. ) ;
#81280 = ORIENTED_EDGE ( 'NONE', *, *, #55966, .F. ) ;
#81281 = VERTEX_POINT ( 'NONE', #41654 ) ;
#81282 = CARTESIAN_POINT ( 'NONE',  ( 33.07276483573664905, 438.9325140356084489, 23.89537236861388081 ) ) ;
#81283 = CARTESIAN_POINT ( 'NONE',  ( 22.45593966533183306, 25.48384861978522409, 32.96011743078131673 ) ) ;
#81284 = CARTESIAN_POINT ( 'NONE',  ( -40.63205167635505433, 465.1703340539525016, 17.16604311417211548 ) ) ;
#81285 = EDGE_LOOP ( 'NONE', ( #62359, #44571, #34376, #79132, #45919 ) ) ;
#81287 = ADVANCED_FACE ( 'NONE', ( #9271 ), #83694, .F. ) ;
#81286 = CARTESIAN_POINT ( 'NONE',  ( 42.35751940687331540, 435.3789575402772130, 19.45706151681951823 ) ) ;
#81288 = VERTEX_POINT ( 'NONE', #46439 ) ;
#81289 = CARTESIAN_POINT ( 'NONE',  ( 6.249999999999998224, 9.237604307034018802, 0.000000000000000000 ) ) ;
#81290 = CARTESIAN_POINT ( 'NONE',  ( 78.90889072956846917, -38.68051256261696835, 190.7199075547812015 ) ) ;
#81291 = CARTESIAN_POINT ( 'NONE',  ( 11.93318256644231745, 6.455544146699622843, 8.908725066499764367 ) ) ;
#81292 = DIRECTION ( 'NONE',  ( 0.000000000000000000, 0.000000000000000000, -1.000000000000000000 ) ) ;
#81293 = CARTESIAN_POINT ( 'NONE',  ( 40.84703668878825766, 325.1337667956213977, 9.320964315343294615 ) ) ;
#81294 = CARTESIAN_POINT ( 'NONE',  ( 9.522120649308408957, 45.61249502152110580, -15.15976961885343499 ) ) ;
#81295 = B_SPLINE_CURVE_WITH_KNOTS ( 'NONE', 3,
 ( #62938, #95832, #5746, #30051 ),
 .UNSPECIFIED., .F., .F.,
 ( 4, 4 ),
 ( 0.0007494527726711166030, 0.02469145274879585433 ),
 .UNSPECIFIED. ) ;
#81296 = AXIS2_PLACEMENT_3D ( 'NONE', #85603, #23934, #40604 ) ;
#81297 = DIRECTION ( 'NONE',  ( -0.8191520442889975717, 0.000000000000000000, -0.5735764363510378328 ) ) ;
#81298 = CIRCLE ( 'NONE', #19399, 4.000000000000000888 ) ;
#81299 = CARTESIAN_POINT ( 'NONE',  ( -4.348929473936721912, -48.21591736632260705, 103.6864098602935513 ) ) ;
#81300 = SURFACE_SIDE_STYLE ('',( #6894 ) ) ;
#81301 = DIRECTION ( 'NONE',  ( 1.000000000000000000, 0.000000000000000000, 0.000000000000000000 ) ) ;
#81302 = ORIENTED_EDGE ( 'NONE', *, *, #38045, .F. ) ;
#81303 = CARTESIAN_POINT ( 'NONE',  ( 32.14400760092454590, 464.7181002246658181, 11.03224828307627980 ) ) ;
#81305 = CARTESIAN_POINT ( 'NONE',  ( -25.59654319921001075, 305.1310134180918112, 10.44692895254650900 ) ) ;
#81304 = SHAPE_REPRESENTATION_RELATIONSHIP ( 'NONE' , 'NONE' ,  #16335, #43474 ) ;
#81306 = CARTESIAN_POINT ( 'NONE',  ( -3.910186774093565631, -48.93965723599501416, 104.5757226097576194 ) ) ;
#81307 = CARTESIAN_POINT ( 'NONE',  ( 37.85084083633365282, 438.0234350436313093, 4.171260309356235929 ) ) ;
#81308 = CARTESIAN_POINT ( 'NONE',  ( -3.313708498984760720, -15.03124999999999289, -8.000000000000000000 ) ) ;
#81309 = CARTESIAN_POINT ( 'NONE',  ( 7.145435414194573731, -19.16271036021109353, 35.18478150345621458 ) ) ;
#81310 = VECTOR ( 'NONE', #102123, 1000.000000000000114 ) ;
#81311 = VECTOR ( 'NONE', #66631, 1000.000000000000000 ) ;
#81312 = CARTESIAN_POINT ( 'NONE',  ( 6.560339683636790653, 297.0608611330067674, 7.566031652892246662 ) ) ;
#81313 = CARTESIAN_POINT ( 'NONE',  ( 16.53805850995897941, 303.5675046017279897, 9.876558242819349687 ) ) ;
#81314 = ORIENTED_EDGE ( 'NONE', *, *, #25553, .F. ) ;
#81315 = CARTESIAN_POINT ( 'NONE',  ( 86.14124937075833088, -24.76901598059708220, 180.5798086085166574 ) ) ;
#81316 = CARTESIAN_POINT ( 'NONE',  ( 2.797297131808757609, 15.83452282593334282, -9.607612890400021755 ) ) ;
#81317 = EDGE_CURVE ( 'NONE', #90625, #16689, #84562, .T. ) ;
#81318 = CARTESIAN_POINT ( 'NONE',  ( -4.678819457397875858, 143.9212778189118183, 5.000000000000004441 ) ) ;
#81319 = ORIENTED_EDGE ( 'NONE', *, *, #63567, .T. ) ;
#81320 = CARTESIAN_POINT ( 'NONE',  ( 94.19163151293176384, -57.67257257346210508, 22.55351835139595806 ) ) ;
#81321 = DIRECTION ( 'NONE',  ( -1.000000000000000000, 0.000000000000000000, 0.000000000000000000 ) ) ;
#81322 = FACE_OUTER_BOUND ( 'NONE', #37163, .T. ) ;
#81323 = CARTESIAN_POINT ( 'NONE',  ( 52.56483885390523625, 40.83906611471594061, -38.23529411764706509 ) ) ;
#81324 = ADVANCED_FACE ( 'NONE', ( #102009 ), #70771, .F. ) ;
#81325 = CIRCLE ( 'NONE', #40002, 4.000000000000001776 ) ;
#81326 = AXIS2_PLACEMENT_3D ( 'NONE', #50253, #73989, #65908 ) ;
#81327 = CARTESIAN_POINT ( 'NONE',  ( -51.84566471874714466, -38.00000000000001421, 53.44666163652544100 ) ) ;
#81328 = CARTESIAN_POINT ( 'NONE',  ( 53.08934989192464826, -30.00000000000000000, 52.21148837440648549 ) ) ;
#81330 = DIRECTION ( 'NONE',  ( -0.000000000000000000, 1.000000000000000000, -0.000000000000000000 ) ) ;
#81329 = CARTESIAN_POINT ( 'NONE',  ( 31.46253585067004721, 1.340359594676612611E-15, 0.000000000000000000 ) ) ;
#81331 = AXIS2_PLACEMENT_3D ( 'NONE', #95060, #44916, #103139 ) ;
#81332 = CARTESIAN_POINT ( 'NONE',  ( -28.45521705596416950, 17.07436234393353303, 41.11936415921380927 ) ) ;
#81333 = CARTESIAN_POINT ( 'NONE',  ( -7.322849800245838203, -11.36060796471280376, -1.080221117633409222E-14 ) ) ;
#81334 = CARTESIAN_POINT ( 'NONE',  ( -27.42214779293654203, 36.77249561759260388, -7.587514376366431890 ) ) ;
#81335 = CARTESIAN_POINT ( 'NONE',  ( 9.999999999999998224, 15.00000000000000000, -2.701558353794592193 ) ) ;
#81336 = PLANE ( 'NONE',  #44272 ) ;
#81337 = AXIS2_PLACEMENT_3D ( 'NONE', #73057, #32110, #43380 ) ;
#81338 = CARTESIAN_POINT ( 'NONE',  ( -97.09057885222009077, -37.99999999999984368, 192.8439867981303735 ) ) ;
#81339 = EDGE_CURVE ( 'NONE', #41783, #80882, #85305, .T. ) ;
#81340 = EDGE_LOOP ( 'NONE', ( #72460, #16150, #36588, #3956, #19196 ) ) ;
#81341 = FACE_OUTER_BOUND ( 'NONE', #4438, .T. ) ;
#81342 = CARTESIAN_POINT ( 'NONE',  ( 30.00000000000000000, 0.000000000000000000, 0.000000000000000000 ) ) ;
#81343 =( BOUNDED_SURFACE ( )  B_SPLINE_SURFACE ( 3, 2, ( 
 ( #21709, #5497, #55086 ),
 ( #88014, #14094, #47000 ),
 ( #66788, #3112, #99674 ),
 ( #2568, #91603, #84030 ),
 ( #44652, #3655, #44108 ),
 ( #92649, #27968, #77536 ) ),
 .UNSPECIFIED., .F., .F., .F. ) 
 B_SPLINE_SURFACE_WITH_KNOTS ( ( 4, 2, 4 ),
 ( 3, 3 ),
 ( 0.03206831234578212675, 0.03607477026923534835, 0.04008122819268857689 ),
 ( 0.000000000000000000, 1.000000000000000000 ),
 .UNSPECIFIED. ) 
 GEOMETRIC_REPRESENTATION_ITEM ( )  RATIONAL_B_SPLINE_SURFACE ( (
 ( 1.000000000000000000, 0.8047780936700352772, 1.000000000000000000),
 ( 1.000000000000000000, 0.8123790890099109596, 1.000000000000000000),
 ( 1.000000000000000000, 0.8190678900508677751, 1.000000000000000000),
 ( 1.000000000000000000, 0.8192345188317070592, 1.000000000000000000),
 ( 1.000000000000000000, 0.8126126219723366351, 1.000000000000000000),
 ( 1.000000000000000000, 0.8047712657247791945, 1.000000000000000000) ) ) 
 REPRESENTATION_ITEM ( '' )  SURFACE ( )  );
#81345 = CARTESIAN_POINT ( 'NONE',  ( -61.30845488575270963, -21.77000553945882899, -22.67001081305290811 ) ) ;
#81344 = CARTESIAN_POINT ( 'NONE',  ( -3.898086217683921717, 13.33789614101572596, -0.2204769333330995063 ) ) ;
#81346 = B_SPLINE_CURVE_WITH_KNOTS ( 'NONE', 3,
 ( #74528, #604, #9258, #23902, #24953, #41115, #32518, #26047, #65390, #75601, #91797, #1699, #90730, #16846, #66447, #50261, #83163, #24439, #25499, #1147, #66994, #34655 ),
 .UNSPECIFIED., .F., .F.,
 ( 4, 2, 2, 2, 2, 2, 2, 2, 2, 2, 4 ),
 ( 0.006964068074043565891, 0.007215909760093224858, 0.007467751446142882957, 0.007971434818242206094, 0.008475118190341527497, 0.008726959876391188198, 0.008978801562440848899, 0.009482484934540168567, 0.009986168306639488235, 0.01048985167873880964, 0.01099353505083812930 ),
 .UNSPECIFIED. ) ;
#81347 = ORIENTED_EDGE ( 'NONE', *, *, #5226, .T. ) ;
#81348 = EDGE_LOOP ( 'NONE', ( #57794, #84321, #80746, #24574, #77172 ) ) ;
#81349 = DIRECTION ( 'NONE',  ( -1.000000000000000000, -1.224606353822377258E-16, -0.000000000000000000 ) ) ;
#81350 = CARTESIAN_POINT ( 'NONE',  ( 10.69678357099577859, 43.19292212010790877, -15.34149409327725877 ) ) ;
#81351 = DIRECTION ( 'NONE',  ( -1.000000000000000000, 0.000000000000000000, 0.000000000000000000 ) ) ;
#81352 = CARTESIAN_POINT ( 'NONE',  ( -66.47461584428864967, -60.00000000000000000, -33.73856253821774231 ) ) ;
#81353 = ORIENTED_EDGE ( 'NONE', *, *, #16156, .F. ) ;
#81354 = CARTESIAN_POINT ( 'NONE',  ( 9.889416687731754863, -23.16239103124826926, -30.52333014326384131 ) ) ;
#81355 = DIRECTION ( 'NONE',  ( -1.000000000000000000, -1.224606353822377258E-16, -0.000000000000000000 ) ) ;
#81356 = CARTESIAN_POINT ( 'NONE',  ( 98.97281587209958786, -52.79378276922967927, 194.7734842299395552 ) ) ;
#81357 = AXIS2_PLACEMENT_3D ( 'NONE', #88171, #22926, #55247 ) ;
#81359 = CARTESIAN_POINT ( 'NONE',  ( 2.435347819570957628E-07, -57.67120202539301488, -44.61186700419775519 ) ) ;
#81358 =( NAMED_UNIT ( * ) SI_UNIT ( $, .STERADIAN. ) SOLID_ANGLE_UNIT ( ) );
#81360 = CARTESIAN_POINT ( 'NONE',  ( -82.17563137770380877, -39.49871834766265977, 162.1473386807309680 ) ) ;
#81361 = VERTEX_POINT ( 'NONE', #11391 ) ;
#81362 =( GEOMETRIC_REPRESENTATION_CONTEXT ( 3 ) GLOBAL_UNCERTAINTY_ASSIGNED_CONTEXT ( ( #52096 ) ) GLOBAL_UNIT_ASSIGNED_CONTEXT ( ( #79866, #83578, #91698 ) ) REPRESENTATION_CONTEXT ( 'NONE', 'WORKASPACE' ) );
#81363 = ORIENTED_EDGE ( 'NONE', *, *, #28946, .T. ) ;
#81364 = STYLED_ITEM ( 'NONE', ( #50564 ), #51906 ) ;
#81365 = VERTEX_POINT ( 'NONE', #11933 ) ;
#81366 = DIRECTION ( 'NONE',  ( 1.000000000000000000, 0.000000000000000000, 0.000000000000000000 ) ) ;
#81367 = EDGE_CURVE ( 'NONE', #14964, #57174, #77811, .T. ) ;
#81368 = CARTESIAN_POINT ( 'NONE',  ( -5.000000000000000000, -15.25461064037155801, 12.58690023576528816 ) ) ;
#81369 = ORIENTED_EDGE ( 'NONE', *, *, #47700, .F. ) ;
#81370 = DIRECTION ( 'NONE',  ( 0.000000000000000000, -1.000000000000000000, 0.000000000000000000 ) ) ;
#81371 = CARTESIAN_POINT ( 'NONE',  ( -88.26372640434641426, 34.25047185182970111, -44.13186320217320713 ) ) ;
#81372 = CARTESIAN_POINT ( 'NONE',  ( -9.240220675753752388, 15.98931925350938243, -3.827754797005808562 ) ) ;
#81374 = STYLED_ITEM ( 'NONE', ( #88224 ), #13026 ) ;
#81373 = CARTESIAN_POINT ( 'NONE',  ( -112.4426759231622270, -57.67115411723771956, 189.8075418672916044 ) ) ;
#81375 = CARTESIAN_POINT ( 'NONE',  ( -9.881511277310785601, 294.6462811792092680, 1.569873444576042942 ) ) ;
#81376 = CARTESIAN_POINT ( 'NONE',  ( 0.000000000000000000, 0.000000000000000000, 15.00000000000000178 ) ) ;
#81377 = CARTESIAN_POINT ( 'NONE',  ( -1.219990203180580712, 25.73133127544792842, 39.18389656347510197 ) ) ;
#81378 = LINE ( 'NONE', #6968, #7194 ) ;
#81379 = COLOUR_RGB ( '', 0.66274510, 0.83137255, 0.94901961) ;
#81380 = EDGE_CURVE ( 'NONE', #90212, #59052, #30269, .T. ) ;
#81381 = CARTESIAN_POINT ( 'NONE',  ( -73.46108764834735894, -30.00000000000002132, -28.33320811291743269 ) ) ;
#81382 = CARTESIAN_POINT ( 'NONE',  ( -4.277630366265612771, -59.99999999999996447, 41.98954236073067392 ) ) ;
#81383 = CARTESIAN_POINT ( 'NONE',  ( -53.26811894799450897, -29.10352339782401998, 52.81850898772155034 ) ) ;
#81384 = CARTESIAN_POINT ( 'NONE',  ( 8.000000000000000000, -27.49999999999999645, 0.000000000000000000 ) ) ;
#81385 = ORIENTED_EDGE ( 'NONE', *, *, #94290, .F. ) ;
#81386 = CARTESIAN_POINT ( 'NONE',  ( -97.47867875887877176, -52.80715018427295604, 195.2329016805694835 ) ) ;
#81387 = CARTESIAN_POINT ( 'NONE',  ( -6.618938675458717391, 296.2345938570451267, -10.01875627916766121 ) ) ;
#81388 = VERTEX_POINT ( 'NONE', #44862 ) ;
#81389 = CARTESIAN_POINT ( 'NONE',  ( -17.88153669719137540, 43.22040693656918364, 5.216588465419869536 ) ) ;
#81390 = CARTESIAN_POINT ( 'NONE',  ( 91.42363583869570220, -38.37299437492562504, -4.571104111833916406 ) ) ;
#81391 = DIRECTION ( 'NONE',  ( 0.000000000000000000, -1.000000000000000000, 0.000000000000000000 ) ) ;
#81392 = CARTESIAN_POINT ( 'NONE',  ( 4.401442555609581635E-16, -11.65625000204838635, -7.188101187500000044 ) ) ;
#81393 = DIRECTION ( 'NONE',  ( -0.000000000000000000, -0.000000000000000000, -1.000000000000000000 ) ) ;
#81394 = CARTESIAN_POINT ( 'NONE',  ( 84.62708170603004021, -29.99999999999998579, 166.7775509064786945 ) ) ;
#81395 = AXIS2_PLACEMENT_3D ( 'NONE', #35894, #1867, #17557 ) ;
#81396 = CARTESIAN_POINT ( 'NONE',  ( -10.28624191511816832, 43.25714326066847804, -15.40779740156204980 ) ) ;
#81397 = CARTESIAN_POINT ( 'NONE',  ( 0.000000000000000000, 67.05096163904791240, 0.000000000000000000 ) ) ;
#81398 = EDGE_CURVE ( 'NONE', #20548, #51009, #34105, .T. ) ;
#81399 = CARTESIAN_POINT ( 'NONE',  ( -6.815830331203684977, -1.215378054691643734E-13, -6.171384342982610072 ) ) ;
#81400 = ORIENTED_EDGE ( 'NONE', *, *, #45715, .F. ) ;
#81401 = VERTEX_POINT ( 'NONE', #3862 ) ;
#81402 = CARTESIAN_POINT ( 'NONE',  ( 49.31972742781113794, -39.51545095625337467, 49.64355539421404728 ) ) ;
#81403 = AXIS2_PLACEMENT_3D ( 'NONE', #56356, #229, #15386 ) ;
#81404 = CARTESIAN_POINT ( 'NONE',  ( 6.767547407775503565, 41.65232290981239771, -58.92985917264464035 ) ) ;
#81405 = CARTESIAN_POINT ( 'NONE',  ( 36.34514833454822735, 28.20980986297035997, -11.89218482807859623 ) ) ;
#81406 = ORIENTED_EDGE ( 'NONE', *, *, #46154, .T. ) ;
#81408 = EDGE_CURVE ( 'NONE', #14483, #48969, #15635, .T. ) ;
#81407 = CARTESIAN_POINT ( 'NONE',  ( -91.20514477336200798, -38.35364638569411255, 26.38587643249713821 ) ) ;
#81409 = ORIENTED_EDGE ( 'NONE', *, *, #84349, .F. ) ;
#81410 = CARTESIAN_POINT ( 'NONE',  ( 98.59472948510774870, -38.35583824562067434, 80.17062742606734105 ) ) ;
#81411 = CARTESIAN_POINT ( 'NONE',  ( 12.36022260502946324, 17.95405137183332300, -8.703727511220279212 ) ) ;
#81412 = DIRECTION ( 'NONE',  ( 0.5735764363510462704, 0.8191520442889915765, 0.000000000000000000 ) ) ;
#81413 = CARTESIAN_POINT ( 'NONE',  ( 105.4324068091576123, -60.15130706364090685, 153.9750241106484054 ) ) ;
#81414 = CARTESIAN_POINT ( 'NONE',  ( -31.76669557235910091, 439.7354465714767571, 23.77638826982954967 ) ) ;
#81415 = CARTESIAN_POINT ( 'NONE',  ( 23.05189055320607849, 27.41800202946304310, 33.19783182242376540 ) ) ;
#81416 = CARTESIAN_POINT ( 'NONE',  ( -36.31305047672606179, 353.1205851602086341, 1.341197250394855489 ) ) ;
#81417 = CARTESIAN_POINT ( 'NONE',  ( 3.231361472310781746, -68.72154468990221687, 13.04944395591344275 ) ) ;
#81418 = CARTESIAN_POINT ( 'NONE',  ( 75.95252160951538656, -59.99999999999998579, 186.7850688652185340 ) ) ;
#81419 = EDGE_CURVE ( 'NONE', #47808, #12223, #102551, .T. ) ;
#81420 = CARTESIAN_POINT ( 'NONE',  ( -43.61263226029857520, 434.4864728595579209, 10.89080223165826133 ) ) ;
#81421 = ORIENTED_EDGE ( 'NONE', *, *, #103082, .F. ) ;
#81422 = CARTESIAN_POINT ( 'NONE',  ( 56.33911714990668429, -60.32421506786621279, 72.31300496870655081 ) ) ;
#81423 = CARTESIAN_POINT ( 'NONE',  ( -27.29321646936245926, 296.3890529966017766, -1.667088702040937065 ) ) ;
#81424 = EDGE_CURVE ( 'NONE', #58869, #102845, #48182, .T. ) ;
#81425 = DIRECTION ( 'NONE',  ( -1.000000000000000000, -0.000000000000000000, 0.000000000000000000 ) ) ;
#81426 = CARTESIAN_POINT ( 'NONE',  ( -5.346098296770412261, -4.999999999999997335, -15.46179592075988474 ) ) ;
#81427 = ORIENTED_EDGE ( 'NONE', *, *, #75805, .F. ) ;
#81429 = CARTESIAN_POINT ( 'NONE',  ( -9.226882652173665988, -53.46780552115761509, 23.14412647329060491 ) ) ;
#81428 = CARTESIAN_POINT ( 'NONE',  ( -45.71963733757685588, -30.00000000000000000, 56.30991746768096817 ) ) ;
#81430 = CARTESIAN_POINT ( 'NONE',  ( 6.397334739185443375, -3.000000000000000444, 4.916373759799320453 ) ) ;
#81431 = DIRECTION ( 'NONE',  ( -1.000000000000000000, -1.224606353822377258E-16, -0.000000000000000000 ) ) ;
#81432 = CARTESIAN_POINT ( 'NONE',  ( 7.000000000000000000, 0.000000000000000000, -10.42450674750459072 ) ) ;
#81433 = CARTESIAN_POINT ( 'NONE',  ( -8.000000000000001776, -31.15625000000000355, 3.313708498984758943 ) ) ;
#81434 = LINE ( 'NONE', #90078, #14081 ) ;
#81435 = CARTESIAN_POINT ( 'NONE',  ( 63.45785145800994798, 48.00000000000000000, -14.99006954567211380 ) ) ;
#81436 = CONICAL_SURFACE ( 'NONE', #55566, 4.000000000000001776, 0.9599310885968808105 ) ;
#81437 = ORIENTED_EDGE ( 'NONE', *, *, #43057, .F. ) ;
#81438 = CARTESIAN_POINT ( 'NONE',  ( 83.17827088202682262, -42.97663241860097116, 176.6375309832781113 ) ) ;
#81439 = CARTESIAN_POINT ( 'NONE',  ( 4.669237227182971850, -14.10230343174356982, -8.329624332552803878 ) ) ;
#81440 = CARTESIAN_POINT ( 'NONE',  ( -3.999995229665001428, -8.688226215992830959, 6.928205984420947594 ) ) ;
#81441 = ORIENTED_EDGE ( 'NONE', *, *, #94957, .T. ) ;
#81442 = AXIS2_PLACEMENT_3D ( 'NONE', #67821, #57574, #50546 ) ;
#81443 = DIRECTION ( 'NONE',  ( 0.000000000000000000, 0.000000000000000000, 1.000000000000000000 ) ) ;
#81444 = CARTESIAN_POINT ( 'NONE',  ( 7.334017076207792307, -3.381213663715690654, -18.44266608209203895 ) ) ;
#81445 = CARTESIAN_POINT ( 'NONE',  ( 41.46829321581945749, 485.6036604809296477, -3.691894868447965550 ) ) ;
#81446 = CARTESIAN_POINT ( 'NONE',  ( 14.99515772855951568, 1.250937070399753770, 0.4481625125234917628 ) ) ;
#81447 = CIRCLE ( 'NONE', #52197, 5.000000000000001776 ) ;
#81448 = DIRECTION ( 'NONE',  ( 0.000000000000000000, 0.000000000000000000, 1.000000000000000000 ) ) ;
#81449 = EDGE_CURVE ( 'NONE', #57174, #46619, #73979, .T. ) ;
#81450 = SHAPE_REPRESENTATION_RELATIONSHIP ( 'NONE' , 'NONE' ,  #7490, #44833 ) ;
#81451 = CARTESIAN_POINT ( 'NONE',  ( 38.50591796967749758, 25.20373685550617182, 13.03523540767606370 ) ) ;
#81452 = SURFACE_STYLE_USAGE ( .BOTH. , #8107 ) ;
#81453 = EDGE_CURVE ( 'NONE', #101318, #41106, #29239, .T. ) ;
#81455 = CARTESIAN_POINT ( 'NONE',  ( -11.88042901237385074, 16.69099646536233550, -9.298101453719690213 ) ) ;
#81454 = CARTESIAN_POINT ( 'NONE',  ( -22.28878110947537650, -27.20780569876249189, 37.41599501972370945 ) ) ;
#81456 = CARTESIAN_POINT ( 'NONE',  ( 7.188101187500000044, -16.15625000204838457, 0.000000000000000000 ) ) ;
#81457 = CARTESIAN_POINT ( 'NONE',  ( -64.32759900502631467, 40.83906611473152992, -11.06576400653637116 ) ) ;
#81458 = CARTESIAN_POINT ( 'NONE',  ( -6.907083948287215058, 41.55068305711947829, -58.85924204532965831 ) ) ;
#81459 = ORIENTED_EDGE ( 'NONE', *, *, #60626, .F. ) ;
#81460 = CARTESIAN_POINT ( 'NONE',  ( -19.48979057729603426, 49.99890399319770751, 60.12824249908928209 ) ) ;
#81461 = CARTESIAN_POINT ( 'NONE',  ( 23.61912243982836301, 25.88172202072039241, 30.76971916150039377 ) ) ;
#81462 = CARTESIAN_POINT ( 'NONE',  ( 36.64823341582351190, 437.5392299810055192, 4.281405873620245828 ) ) ;
#81463 = FACE_OUTER_BOUND ( 'NONE', #8781, .T. ) ;
#81464 = CARTESIAN_POINT ( 'NONE',  ( 9.165151389911699198, 249.9999999999999432, -4.000000000000002665 ) ) ;
#81465 = ORIENTED_EDGE ( 'NONE', *, *, #11970, .F. ) ;
#81466 = CARTESIAN_POINT ( 'NONE',  ( 11.66210838966212293, 15.93376395241612897, -9.569172803016048334 ) ) ;
#81467 = PLANE ( 'NONE',  #44471 ) ;
#81468 = AXIS2_PLACEMENT_3D ( 'NONE', #32800, #82382, #47875 ) ;
#81469 = EDGE_LOOP ( 'NONE', ( #4802, #31987, #103705, #72172 ) ) ;
#81470 = SURFACE_SIDE_STYLE ('',( #15692 ) ) ;
#81471 = CARTESIAN_POINT ( 'NONE',  ( 0.000000000000000000, 0.000000000000000000, -4.425378966781146950 ) ) ;
#81472 = CARTESIAN_POINT ( 'NONE',  ( 46.00000000000000000, 500.0000000000002274, 0.000000000000000000 ) ) ;
#81473 = CARTESIAN_POINT ( 'NONE',  ( -110.7216341579778032, -60.00000000000000000, 149.4927839103214637 ) ) ;
#81474 = DIRECTION ( 'NONE',  ( 1.000000000000000000, 0.000000000000000000, 0.000000000000000000 ) ) ;
#81475 = CARTESIAN_POINT ( 'NONE',  ( 43.65900554256388233, 484.6127093603670914, 3.254021613880305974 ) ) ;
#81476 = FACE_OUTER_BOUND ( 'NONE', #42691, .T. ) ;
#81477 = CARTESIAN_POINT ( 'NONE',  ( -32.81992448453853939, 465.7192846569224685, 11.17271167765295559 ) ) ;
#81478 = B_SPLINE_CURVE_WITH_KNOTS ( 'NONE', 3,
 ( #97006, #80814, #97516, #63602, #23146, #7444, #48443, #64138, #6927, #30715, #40360, #105107, #72203, #31248, #20664, #23681, #88922, #88397, #56528, #81334, #89458, #73239 ),
 .UNSPECIFIED., .F., .F.,
 ( 4, 2, 2, 2, 2, 2, 2, 2, 2, 2, 4 ),
 ( 0.007109265277489604240, 0.007613110377180124996, 0.008116955476870645753, 0.008368878026715901794, 0.008620800576561156101, 0.009124645676251668183, 0.009376568226096925959, 0.009628490775942183735, 0.01013233587563269408, 0.01063618097532320617, 0.01114002607501371825 ),
 .UNSPECIFIED. ) ;
#81480 = CARTESIAN_POINT ( 'NONE',  ( -15.30823401445666043, 3.112986885588304276, -3.167215778809110649 ) ) ;
#81479 = CARTESIAN_POINT ( 'NONE',  ( 9.739726766104318756, -5.000000000001365130, -87.61747884499031613 ) ) ;
#81481 = CARTESIAN_POINT ( 'NONE',  ( -81.92653451457113079, -53.51318851167744839, 180.9174972423841439 ) ) ;
#81482 = ORIENTED_EDGE ( 'NONE', *, *, #97534, .T. ) ;
#81483 = VERTEX_POINT ( 'NONE', #79853 ) ;
#81484 = ORIENTED_EDGE ( 'NONE', *, *, #32522, .F. ) ;
#81485 = SPHERICAL_SURFACE ( 'NONE', #94008, 1.000000000000000000 ) ;
#81486 = EDGE_CURVE ( 'NONE', #76952, #5281, #29478, .T. ) ;
#81487 = LINE ( 'NONE', #97158, #80136 ) ;
#81488 = DIRECTION ( 'NONE',  ( -0.000000000000000000, -1.000000000000000000, -0.000000000000000000 ) ) ;
#81489 = CARTESIAN_POINT ( 'NONE',  ( 30.00000000000000355, 461.9594878872943582, 14.33673855775172079 ) ) ;
#81490 = CARTESIAN_POINT ( 'NONE',  ( 55.00571552735602410, 4.000000000000013323, 0.000000000000000000 ) ) ;
#81491 = CARTESIAN_POINT ( 'NONE',  ( 0.000000000000000000, 0.000000000000000000, 0.000000000000000000 ) ) ;
#81492 = EDGE_CURVE ( 'NONE', #12821, #44704, #91495, .T. ) ;
#81493 = CARTESIAN_POINT ( 'NONE',  ( 109.5675852999991662, -29.99999999999999645, 170.1819856699497961 ) ) ;
#81494 = CARTESIAN_POINT ( 'NONE',  ( -109.5916892278405470, -30.00000000000001776, 172.2591039824585550 ) ) ;
#81495 = CARTESIAN_POINT ( 'NONE',  ( -61.37073833729998995, -60.34629577541569034, 86.28566146466783948 ) ) ;
#81496 = ORIENTED_EDGE ( 'NONE', *, *, #67340, .T. ) ;
#81497 = CARTESIAN_POINT ( 'NONE',  ( 62.81009128990557144, 38.95404459711129164, -10.81681776479946144 ) ) ;
#81498 = CARTESIAN_POINT ( 'NONE',  ( 97.01038254189587917, -60.00000000003893064, 46.46193752217217110 ) ) ;
#81499 = ORIENTED_EDGE ( 'NONE', *, *, #8255, .F. ) ;
#81500 = CYLINDRICAL_SURFACE ( 'NONE', #101006, 7.000000000000011546 ) ;
#81501 = CARTESIAN_POINT ( 'NONE',  ( 5.082755093536324154, -13.71875000204838457, 5.082755093536326818 ) ) ;
#81502 = AXIS2_PLACEMENT_3D ( 'NONE', #25752, #12556, #67758 ) ;
#81503 = CARTESIAN_POINT ( 'NONE',  ( -8.990409435379676850, -5.000000000000000000, -71.93151781322266913 ) ) ;
#81504 = ORIENTED_EDGE ( 'NONE', *, *, #52145, .F. ) ;
#81505 = DIRECTION ( 'NONE',  ( 0.000000000000000000, 1.000000000000000000, 0.000000000000000000 ) ) ;
#81506 = EDGE_LOOP ( 'NONE', ( #52983, #53020, #20441 ) ) ;
#81507 = CARTESIAN_POINT ( 'NONE',  ( -1.469576158976823947E-15, -24.87499999999999289, 8.000000000000000000 ) ) ;
#81508 = CARTESIAN_POINT ( 'NONE',  ( -98.98947487261378342, -60.00000000000000000, 75.03658297502093433 ) ) ;
#81509 = CARTESIAN_POINT ( 'NONE',  ( 7.188101187500001821, -25.43750000204838813, -2.977408999572650483 ) ) ;
#81510 = CARTESIAN_POINT ( 'NONE',  ( 46.00000000000000000, 462.4524393752382139, 6.584174932629923482 ) ) ;
#81511 = CARTESIAN_POINT ( 'NONE',  ( 17.63841679208134394, 43.19886265510177026, -6.169146188730260327 ) ) ;
#81512 = AXIS2_PLACEMENT_3D ( 'NONE', #75819, #2988, #10546 ) ;
#81513 = CARTESIAN_POINT ( 'NONE',  ( -5.453027751480597374, 54.16931316411591979, -6.031152949374162020 ) ) ;
#81514 = DIRECTION ( 'NONE',  ( 1.000000000000000000, 1.224606353822377258E-16, 0.000000000000000000 ) ) ;
#81515 = CARTESIAN_POINT ( 'NONE',  ( -23.54225815529405708, 28.03385386361086873, 30.74635459162657014 ) ) ;
#81516 = ADVANCED_FACE ( 'NONE', ( #97102 ), #71755, .F. ) ;
#81517 = CARTESIAN_POINT ( 'NONE',  ( 102.0111507166176921, -60.00000000000002132, 127.8858238654740944 ) ) ;
#81518 = CARTESIAN_POINT ( 'NONE',  ( -32.84146244817398497, -56.84655200642422557, 37.45245214281151647 ) ) ;
#81519 = CARTESIAN_POINT ( 'NONE',  ( -2.706785074969853877, -49.45229994201851298, 103.4519997648589538 ) ) ;
#81520 = CIRCLE ( 'NONE', #57433, 4.000000000000007105 ) ;
#81521 = CARTESIAN_POINT ( 'NONE',  ( 39.71597467038597529, -29.14573511708929132, 36.18980527160656635 ) ) ;
#81522 = CARTESIAN_POINT ( 'NONE',  ( 22.25669491856071858, 3.851859888774471706E-31, 5.000000000000001776 ) ) ;
#81523 = ORIENTED_EDGE ( 'NONE', *, *, #66561, .F. ) ;
#81524 = CARTESIAN_POINT ( 'NONE',  ( -7.801339272325196639, 88.58731471959703185, -1.788609912539676161 ) ) ;
#81525 = CARTESIAN_POINT ( 'NONE',  ( -73.90592356584222955, -38.32656427293123613, 159.5603895101343426 ) ) ;
#81526 = EDGE_LOOP ( 'NONE', ( #27165, #25096, #66177, #14766 ) ) ;
#81528 = CARTESIAN_POINT ( 'NONE',  ( 92.53532739719321398, 5.000000000000021316, 0.000000000000000000 ) ) ;
#81527 = DIRECTION ( 'NONE',  ( -1.000000000000000000, 0.000000000000000000, 0.000000000000000000 ) ) ;
#81529 = CARTESIAN_POINT ( 'NONE',  ( -33.16497501406121984, 438.9508968883769171, 23.91452439717005873 ) ) ;
#81530 = CARTESIAN_POINT ( 'NONE',  ( 6.585531397294616340, 4.023063057964797018, 6.499999999999997335 ) ) ;
#81531 = DIRECTION ( 'NONE',  ( 0.000000000000000000, 0.000000000000000000, -1.000000000000000000 ) ) ;
#81532 = CARTESIAN_POINT ( 'NONE',  ( -39.57869015843257898, 437.2512761492686195, 5.285341955748192433 ) ) ;
#81533 = CARTESIAN_POINT ( 'NONE',  ( 5.477578620271511767, -88.16501439016107611, -2.459398706554656311 ) ) ;
#81534 = DIRECTION ( 'NONE',  ( -1.000000000000000000, -1.224606353822377258E-16, -0.000000000000000000 ) ) ;
#81535 = CARTESIAN_POINT ( 'NONE',  ( 93.48957285444535614, -60.00000000000001421, 36.96153506271591027 ) ) ;
#81536 = CARTESIAN_POINT ( 'NONE',  ( 14.95520043898952522, 4.194724623210934311, -5.164345506890662740 ) ) ;
#81537 = CIRCLE ( 'NONE', #35094, 0.9999999999999988898 ) ;
#81538 = AXIS2_PLACEMENT_3D ( 'NONE', #80107, #6754, #47732 ) ;
#81539 = DIRECTION ( 'NONE',  ( -1.000000000000000000, -1.224606353822377258E-16, -0.000000000000000000 ) ) ;
#81540 = CARTESIAN_POINT ( 'NONE',  ( -2.500000000000000444, -12.75203052241420743, 21.42349665395800073 ) ) ;
#81541 = EDGE_LOOP ( 'NONE', ( #13771, #37458, #95978, #69303, #68484 ) ) ;
#81542 = STYLED_ITEM ( 'NONE', ( #38356 ), #19013 ) ;
#81543 = CARTESIAN_POINT ( 'NONE',  ( -89.14514748770606900, -29.99999999999991473, 188.9207774528190384 ) ) ;
#81544 = ORIENTED_EDGE ( 'NONE', *, *, #59875, .F. ) ;
#81545 = CARTESIAN_POINT ( 'NONE',  ( -3.351415491885648024, -49.00496204699513925, 104.3291447875367339 ) ) ;
#81546 = CARTESIAN_POINT ( 'NONE',  ( -15.90404091945035070, 3.516460376326330017, -2.884095128127718066 ) ) ;
#81547 = CARTESIAN_POINT ( 'NONE',  ( 8.588409832245909925, 23.79849351031133509, 4.999999999998157918 ) ) ;
#81548 = DIRECTION ( 'NONE',  ( -1.000000000000000000, -1.224606353822377258E-16, -0.000000000000000000 ) ) ;
#81549 = CARTESIAN_POINT ( 'NONE',  ( -22.88936581296984585, 28.17682283790767173, -30.74716342950141623 ) ) ;
#81550 = VECTOR ( 'NONE', #46450, 1000.000000000000114 ) ;
#81551 = CARTESIAN_POINT ( 'NONE',  ( 7.188101187500000044, -24.03125000204838457, 0.000000000000000000 ) ) ;
#81552 = DIRECTION ( 'NONE',  ( 0.000000000000000000, -1.000000000000000000, 0.000000000000000000 ) ) ;
#81553 = CARTESIAN_POINT ( 'NONE',  ( 19.00000000000000711, 4.000000000000000888, -1.500000000000001332 ) ) ;
#81554 = ORIENTED_EDGE ( 'NONE', *, *, #89191, .F. ) ;
#81556 = VERTEX_POINT ( 'NONE', #89023 ) ;
#81555 = FACE_OUTER_BOUND ( 'NONE', #59700, .T. ) ;
#81557 = CARTESIAN_POINT ( 'NONE',  ( 81.85470369756671971, -36.02805305272049452, 154.5082235924975578 ) ) ;
#81558 = CARTESIAN_POINT ( 'NONE',  ( -63.67138272020815748, 38.95383793066860534, 8.334564508068538657 ) ) ;
#81559 = LINE ( 'NONE', #7687, #29944 ) ;
#81560 = ORIENTED_EDGE ( 'NONE', *, *, #80737, .F. ) ;
#81561 = CARTESIAN_POINT ( 'NONE',  ( -45.43592567508400748, 50.00000000000001421, 43.65922790991991320 ) ) ;
#81562 = CARTESIAN_POINT ( 'NONE',  ( -14.97540207516782118, 1.269614109200695840, -0.8865648853131175011 ) ) ;
#81563 = CARTESIAN_POINT ( 'NONE',  ( 7.188101187500000933, -13.06250000204838280, -2.977408999572650483 ) ) ;
#81564 = CARTESIAN_POINT ( 'NONE',  ( 7.211357414135268762, 27.98853460065558707, 3.467230644691330355 ) ) ;
#81565 = CARTESIAN_POINT ( 'NONE',  ( 49.37224559707967586, -60.00000000000000711, -32.19427091295325738 ) ) ;
#81566 = CARTESIAN_POINT ( 'NONE',  ( -40.46187072321335165, -57.69130470027779012, 56.40641529803505705 ) ) ;
#81567 = B_SPLINE_SURFACE_WITH_KNOTS ( 'NONE', 1, 3, ( 
 ( #79653, #39220, #5249, #4717, #5764, #70515, #94805, #37654, #38178, #54836, #6281, #21981, #29558, #62429, #71034, #38686, #103925, #71552, #63494, #89877, #81755, #15445, #23574, #41318, #76199, #49399, #73132, #15985 ),
 ( #43317, #73678, #64548, #56422, #82308, #2301, #89355, #8418, #48336, #68116, #97414, #24113, #32183, #81231, #10402, #106036, #57485, #74208, #287, #35250, #101013, #33253, #7348, #48862, #106580, #40257, #65066, #66126 ) ),
 .UNSPECIFIED., .F., .F., .F.,
 ( 2, 2 ),
 ( 4, 2, 2, 2, 2, 2, 2, 2, 2, 2, 2, 2, 2, 4 ),
 ( 0.000000000000000000, 1.000000000000000000 ),
 ( 0.08901491201581737678, 0.1032490540155679704, 0.1174831960153185778, 0.1317173380150691853, 0.1459514800148197788, 0.1744197640143299588, 0.2028880480138401388, 0.2598246160128514504, 0.3167611840118632616, 0.4306343200098861623, 0.5445074560079088410, 0.6583805920059359051, 0.7722537280039543095, 1.000000000000000000 ),
 .UNSPECIFIED. ) ;
#81568 = CARTESIAN_POINT ( 'NONE',  ( -7.500000000000000888, -3.000671055698259870, -20.99923901233272971 ) ) ;
#81569 = EDGE_CURVE ( 'NONE', #4842, #58946, #28967, .T. ) ;
#81570 = ORIENTED_EDGE ( 'NONE', *, *, #1980, .T. ) ;
#81571 = AXIS2_PLACEMENT_3D ( 'NONE', #104750, #30901, #47566 ) ;
#81572 = SURFACE_STYLE_USAGE ( .BOTH. , #97773 ) ;
#81573 = CARTESIAN_POINT ( 'NONE',  ( 2.849088235197430485, 70.33548021428394748, 5.000000000000000000 ) ) ;
#81574 = CARTESIAN_POINT ( 'NONE',  ( -1.469576158976823947E-15, -18.87499999999999289, 8.000000000000000000 ) ) ;
#81575 = ADVANCED_FACE ( 'NONE', ( #38370 ), #32929, .T. ) ;
#81576 = CARTESIAN_POINT ( 'NONE',  ( 0.000000000000000000, -30.00000000000000000, 0.000000000000000000 ) ) ;
#81577 = ORIENTED_EDGE ( 'NONE', *, *, #94451, .F. ) ;
#81578 = CARTESIAN_POINT ( 'NONE',  ( -2.977408999572650039, -29.18750000204839523, -7.188101187500001821 ) ) ;
#81579 = CARTESIAN_POINT ( 'NONE',  ( 26.68896952748668383, -30.19711848523571263, 38.93503799944183186 ) ) ;
#81580 = CARTESIAN_POINT ( 'NONE',  ( -39.59091745083550506, 490.2217143383006714, 11.38611456561468316 ) ) ;
#81581 = COLOUR_RGB ( '', 0.66274510, 0.83137255, 0.94901961) ;
#81582 = CARTESIAN_POINT ( 'NONE',  ( 0.3342036119824616791, 52.16127839274962952, -7.792586909974158260 ) ) ;
#81583 = CARTESIAN_POINT ( 'NONE',  ( -5.656854249492381470, -16.06249999999999289, 5.656854249492379694 ) ) ;
#81584 = CARTESIAN_POINT ( 'NONE',  ( 35.03794650530581123, 439.1670263218123864, 24.09217910952948216 ) ) ;
#81585 = VECTOR ( 'NONE', #52189, 1000.000000000000000 ) ;
#81586 = PRODUCT_CONTEXT ( 'NONE', #82395, 'mechanical' ) ;
#81587 = CARTESIAN_POINT ( 'NONE',  ( -9.536842176398147686, 32.64235369883989790, 3.014135744008175966 ) ) ;
#81588 = ORIENTED_EDGE ( 'NONE', *, *, #3641, .F. ) ;
#81589 = CARTESIAN_POINT ( 'NONE',  ( 0.000000000000000000, -4.000000000000003553, 112.0000000000000000 ) ) ;
#81590 = EDGE_CURVE ( 'NONE', #18346, #87281, #100915, .T. ) ;
#81591 = CARTESIAN_POINT ( 'NONE',  ( 18.58349330513380693, 1.593028355512270962E-15, 0.000000000000000000 ) ) ;
#81592 = COLOUR_RGB ( '', 0.66274510, 0.83137255, 0.94901961) ;
#81593 = CARTESIAN_POINT ( 'NONE',  ( 66.26095113931063452, -4.000000000000000000, 0.000000000000000000 ) ) ;
#81594 = CARTESIAN_POINT ( 'NONE',  ( 13.25260485096620933, -23.44304414601906927, -38.53988249343816364 ) ) ;
#81595 = CARTESIAN_POINT ( 'NONE',  ( 92.53532739719321398, 1.030564683017419500E-14, 0.000000000000000000 ) ) ;
#81596 = DIRECTION ( 'NONE',  ( 1.150791560227848297E-16, -0.3420201433256725987, 0.9396926207859068736 ) ) ;
#81597 = ORIENTED_EDGE ( 'NONE', *, *, #5476, .T. ) ;
#81598 = CARTESIAN_POINT ( 'NONE',  ( 0.000000000000000000, 4.898587196589413815E-16, -4.000000000000000888 ) ) ;
#81599 = CARTESIAN_POINT ( 'NONE',  ( 111.9947854193034402, -57.67108030077226033, 191.3410972543836408 ) ) ;
#81600 = PRESENTATION_STYLE_ASSIGNMENT (( #16357 ) ) ;
#81601 = CARTESIAN_POINT ( 'NONE',  ( -9.635262854140592026, 51.40918690193957019, -2.123770696076897391 ) ) ;
#81602 = DIRECTION ( 'NONE',  ( -1.000000000000000000, -1.224606353822377258E-16, -0.000000000000000000 ) ) ;
#81603 = CARTESIAN_POINT ( 'NONE',  ( -6.368327914470341966, 53.78267287650600537, 6.628995654898029777 ) ) ;
#81604 = CARTESIAN_POINT ( 'NONE',  ( -74.68708113791835501, -60.00000000000000000, 178.7673637760337613 ) ) ;
#81605 = CARTESIAN_POINT ( 'NONE',  ( -33.08751701378358945, 301.6823158026044780, 11.49690784967660662 ) ) ;
#81606 = SURFACE_SIDE_STYLE ('',( #32585 ) ) ;
#81607 = CARTESIAN_POINT ( 'NONE',  ( -32.16694665535142406, 298.7751107022914425, -9.134474995491629556 ) ) ;
#81608 = CARTESIAN_POINT ( 'NONE',  ( -83.28797064766409619, -60.96659139404700767, 191.1653894862643597 ) ) ;
#81610 = ORIENTED_EDGE ( 'NONE', *, *, #28438, .F. ) ;
#81609 = AXIS2_PLACEMENT_3D ( 'NONE', #18620, #25114, #51481 ) ;
#81611 = CARTESIAN_POINT ( 'NONE',  ( 30.56684744126956232, 310.6574340941369314, -8.419107643419287967 ) ) ;
#81612 = AXIS2_PLACEMENT_3D ( 'NONE', #22593, #87299, #21012 ) ;
#81613 = ORIENTED_EDGE ( 'NONE', *, *, #68744, .T. ) ;
#81614 = DIRECTION ( 'NONE',  ( 0.000000000000000000, -1.000000000000000000, 0.000000000000000000 ) ) ;
#81615 = EDGE_CURVE ( 'NONE', #8430, #79845, #55282, .T. ) ;
#81616 = CARTESIAN_POINT ( 'NONE',  ( -5.802268690544500451, -3.456390741716395709, 103.8899761878886494 ) ) ;
#81617 = AXIS2_PLACEMENT_3D ( 'NONE', #20091, #19557, #52393 ) ;
#81618 = CARTESIAN_POINT ( 'NONE',  ( -84.93482623333412107, -52.74702798847152962, -13.23012522214947317 ) ) ;
#81619 = DIRECTION ( 'NONE',  ( -1.000000000000000000, -1.224606353822377258E-16, -0.000000000000000000 ) ) ;
#81620 = DIRECTION ( 'NONE',  ( 1.000000000000000000, 0.000000000000000000, -0.000000000000000000 ) ) ;
#81621 = EDGE_LOOP ( 'NONE', ( #59658, #41732, #42839, #21217, #64916, #92615, #54749, #80453, #70669, #58347, #86600, #50793, #92436, #14416, #77552, #70910, #66717, #24656, #56025, #14295, #21141, #82747, #65515, #15382, #13734, #43571, #96140, #94947, #29498, #89239 ) ) ;
#81622 = CARTESIAN_POINT ( 'NONE',  ( -32.45893998669878044, 464.7013998967537418, 16.05169235329088195 ) ) ;
#81623 = CARTESIAN_POINT ( 'NONE',  ( 10.14798799572017529, 15.71901827466141377, -10.24181171185648331 ) ) ;
#81624 = ADVANCED_FACE ( 'NONE', ( #50647 ), #56968, .T. ) ;
#81625 = EDGE_CURVE ( 'NONE', #6335, #88975, #65609, .T. ) ;
#81626 = CARTESIAN_POINT ( 'NONE',  ( -2.227375807148842313, -1.734723475976807094E-15, -17.01589776168603407 ) ) ;
#81627 = DIRECTION ( 'NONE',  ( 0.000000000000000000, 0.9024170203239317845, -0.4308636924012935743 ) ) ;
#81628 = CARTESIAN_POINT ( 'NONE',  ( 57.68379620845067279, -29.99999999999995026, -33.51799637603287607 ) ) ;
#81629 = CARTESIAN_POINT ( 'NONE',  ( -76.34156285824845156, -46.43775314653531439, 131.9850733549745883 ) ) ;
#81630 = ORIENTED_EDGE ( 'NONE', *, *, #49869, .T. ) ;
#81631 = CARTESIAN_POINT ( 'NONE',  ( 54.44934741818074286, -29.99999999999998224, 75.82777139632159447 ) ) ;
#81632 = CARTESIAN_POINT ( 'NONE',  ( 7.551560007654696705, 88.00910351806992082, -2.648022159607839487 ) ) ;
#81633 = CARTESIAN_POINT ( 'NONE',  ( 93.16704160177832250, -57.65532162308603858, -16.80702944056087844 ) ) ;
#81634 = B_SPLINE_CURVE_WITH_KNOTS ( 'NONE', 3,
 ( #15719, #56146, #98230, #15184, #16791, #65869, #64291, #48073, #56698, #99276, #16248, #31929, #33523, #80974, #97689, #97162, #80445, #89621, #7610, #8159, #48605, #98748, #49134, #106305, #33001, #49678, #40529, #8690, #24385, #24903, #41064, #39488, #73949, #57756 ),
 .UNSPECIFIED., .F., .F.,
 ( 4, 2, 2, 2, 2, 2, 2, 2, 2, 2, 2, 2, 2, 2, 2, 2, 4 ),
 ( 0.000000000000000000, 0.06250000000000000000, 0.1250000000000000000, 0.1875000000000000000, 0.2500000000000000000, 0.3125000000000000000, 0.3750000000000000000, 0.4375000000000000000, 0.5000000000000000000, 0.5625000000000000000, 0.6250000000000000000, 0.6875000000000000000, 0.7500000000000000000, 0.8125000000000000000, 0.8750000000000000000, 0.9375000000000000000, 1.000000000000000000 ),
 .UNSPECIFIED. ) ;
#81635 = ORIENTED_EDGE ( 'NONE', *, *, #22212, .T. ) ;
#81636 = CARTESIAN_POINT ( 'NONE',  ( 72.85555555555556850, -3.309500000000000774, 0.000000000000000000 ) ) ;
#81637 = DIRECTION ( 'NONE',  ( 0.000000000000000000, -1.000000000000000000, 0.000000000000000000 ) ) ;
#81638 = EDGE_LOOP ( 'NONE', ( #50207, #36473, #1235, #49108 ) ) ;
#81639 = CARTESIAN_POINT ( 'NONE',  ( 3.867124570037480336, 16.79637511870748412, -5.835187682821653787 ) ) ;
#81640 = CARTESIAN_POINT ( 'NONE',  ( -12.50000000000000711, 16.77477480092213824, -34.50590452214681392 ) ) ;
#81641 = CARTESIAN_POINT ( 'NONE',  ( 0.000000000000000000, 0.000000000000000000, 0.000000000000000000 ) ) ;
#81642 = CARTESIAN_POINT ( 'NONE',  ( -1.320432766682874540E-15, -18.03125000204838457, 7.188101187500000044 ) ) ;
#81643 = CARTESIAN_POINT ( 'NONE',  ( 6.625705691649121931, -5.306270977113076270, -7.795653906408811729 ) ) ;
#81644 = SURFACE_STYLE_FILL_AREA ( #82189 ) ;
#81645 = SURFACE_STYLE_FILL_AREA ( #48752 ) ;
#81646 = CARTESIAN_POINT ( 'NONE',  ( -7.500000000000000000, -4.732323933430413909, -7.493854309896103238 ) ) ;
#81647 = CARTESIAN_POINT ( 'NONE',  ( -1.469576158976823947E-15, -13.06250000409676915, 8.000000000000000000 ) ) ;
#81648 = EDGE_CURVE ( 'NONE', #83274, #72947, #74936, .T. ) ;
#81649 = AXIS2_PLACEMENT_3D ( 'NONE', #41101, #65901, #99312 ) ;
#81650 = ORIENTED_EDGE ( 'NONE', *, *, #44240, .F. ) ;
#81651 = CARTESIAN_POINT ( 'NONE',  ( -7.326726048548432679, 41.40616594562586528, -69.28044392950745589 ) ) ;
#81653 = CARTESIAN_POINT ( 'NONE',  ( 31.24783293400658835, -56.84949674888247984, 36.70056667471371981 ) ) ;
#81652 = CARTESIAN_POINT ( 'NONE',  ( -4.277630366265612771, -59.99999999999996447, 41.98954236073067392 ) ) ;
#81654 = CARTESIAN_POINT ( 'NONE',  ( -4.063202461714976899, 52.05771371934300618, -6.989737321421222838 ) ) ;
#81655 = VERTEX_POINT ( 'NONE', #49609 ) ;
#81656 = EDGE_CURVE ( 'NONE', #93736, #86218, #88141, .T. ) ;
#81657 = AXIS2_PLACEMENT_3D ( 'NONE', #27250, #27786, #20229 ) ;
#81658 = ORIENTED_EDGE ( 'NONE', *, *, #74077, .T. ) ;
#81660 = CARTESIAN_POINT ( 'NONE',  ( 0.6465847505401471906, 51.32305258032151585, 10.08284153374933467 ) ) ;
#81659 = CARTESIAN_POINT ( 'NONE',  ( 89.93133926947346879, 1.016364837396684119E-14, 0.000000000000000000 ) ) ;
#81661 = DIRECTION ( 'NONE',  ( -1.000000000000000000, -1.224606353822377258E-16, -0.000000000000000000 ) ) ;
#81662 = CARTESIAN_POINT ( 'NONE',  ( -11.68525014344062818, 302.5966531034369496, -10.05424063234815613 ) ) ;
#81663 = CARTESIAN_POINT ( 'NONE',  ( 6.075691126275640563, 41.99394904787047977, -68.91429206828460963 ) ) ;
#81664 = ADVANCED_FACE ( 'NONE', ( #8089 ), #20936, .T. ) ;
#81665 = CARTESIAN_POINT ( 'NONE',  ( 0.4150347205025879394, 45.32703121288628978, 18.68203640562379064 ) ) ;
#81666 = CARTESIAN_POINT ( 'NONE',  ( 12.13034742782428310, 49.99999999999999289, -93.82352941176471006 ) ) ;
#81667 = VERTEX_POINT ( 'NONE', #9141 ) ;
#81668 = CARTESIAN_POINT ( 'NONE',  ( 23.69449890484973054, -59.99999999999999289, -41.54738999840723324 ) ) ;
#81669 = LINE ( 'NONE', #99457, #103242 ) ;
#81670 = AXIS2_PLACEMENT_3D ( 'NONE', #34868, #74212, #33257 ) ;
#81671 = CARTESIAN_POINT ( 'NONE',  ( 30.00000000000000355, 461.9311049912211047, 11.83317730145386015 ) ) ;
#81672 = CARTESIAN_POINT ( 'NONE',  ( 1.517883041479706208E-15, -5.000000000000000888, -97.00000000000000000 ) ) ;
#81673 =( BOUNDED_SURFACE ( )  B_SPLINE_SURFACE ( 3, 2, ( 
 ( #11787, #59304, #69519 ),
 ( #93254, #11249, #51179 ),
 ( #68996, #18324, #3724 ),
 ( #84633, #19417, #19948 ),
 ( #44717, #52251, #28031 ),
 ( #36654, #85162, #77606 ),
 ( #61435, #102407, #27504 ),
 ( #52788, #85714, #44178 ),
 ( #75467, #60900, #9654 ),
 ( #26960, #84098, #1561 ),
 ( #10720, #100800, #10198 ),
 ( #77068, #94331, #20494 ),
 ( #43110, #101871, #93791 ),
 ( #60379, #67914, #36127 ) ),
 .UNSPECIFIED., .F., .F., .F. ) 
 B_SPLINE_SURFACE_WITH_KNOTS ( ( 4, 2, 2, 2, 2, 2, 4 ),
 ( 3, 3 ),
 ( 0.000000000000000000, 0.002028361404254495556, 0.004056722808508991113, 0.006085084212763486669, 0.008113445617017982225, 0.01217016842552697334, 0.01622689123403596445 ),
 ( 0.000000000000000000, 1.000000000000000000 ),
 .UNSPECIFIED. ) 
 GEOMETRIC_REPRESENTATION_ITEM ( )  RATIONAL_B_SPLINE_SURFACE ( (
 ( 1.000000000000000000, 0.7071067811865476838, 1.000000000000000000),
 ( 1.000000000000000000, 0.7270538103684279774, 1.000000000000000000),
 ( 1.000000000000000000, 0.7474775509999233014, 1.000000000000000000),
 ( 1.000000000000000000, 0.7877120837787837671, 1.000000000000000000),
 ( 1.000000000000000000, 0.8076198138824922657, 1.000000000000000000),
 ( 1.000000000000000000, 0.8446812442348378136, 1.000000000000000000),
 ( 1.000000000000000000, 0.8620019270876144724, 1.000000000000000000),
 ( 1.000000000000000000, 0.8939173377915230478, 1.000000000000000000),
 ( 1.000000000000000000, 0.9085622752435040805, 1.000000000000000000),
 ( 1.000000000000000000, 0.9477746975871859103, 1.000000000000000000),
 ( 1.000000000000000000, 0.9672053386932838448, 1.000000000000000000),
 ( 1.000000000000000000, 0.9933317393958381869, 1.000000000000000000),
 ( 1.000000000000000000, 1.000004063029856116, 1.000000000000000000),
 ( 1.000000000000000000, 1.000000000000000000, 1.000000000000000000) ) ) 
 REPRESENTATION_ITEM ( '' )  SURFACE ( )  );
#81674 = LINE ( 'NONE', #90862, #30604 ) ;
#81675 = ORIENTED_EDGE ( 'NONE', *, *, #39193, .F. ) ;
#81676 = ORIENTED_EDGE ( 'NONE', *, *, #101156, .F. ) ;
#81677 = ORIENTED_EDGE ( 'NONE', *, *, #93974, .T. ) ;
#81678 = CARTESIAN_POINT ( 'NONE',  ( 1.248908473850341538, 53.88172734546416365, 8.832198851183429511 ) ) ;
#81679 = CARTESIAN_POINT ( 'NONE',  ( 37.47001334519036675, 40.63833030000166247, -58.98724826624130202 ) ) ;
#81680 = CARTESIAN_POINT ( 'NONE',  ( -37.56673239365849781, 27.88554838446201600, 10.95617127781066102 ) ) ;
#81681 = CARTESIAN_POINT ( 'NONE',  ( 23.89727872382834661, 303.8791563162774310, 10.16063969049587712 ) ) ;
#81682 = CARTESIAN_POINT ( 'NONE',  ( -37.68702322361429680, 382.9563223952199564, 5.553542584039877994 ) ) ;
#81683 = CARTESIAN_POINT ( 'NONE',  ( -4.857172966777105749, -65.88657749106603490, 13.84720118471725314 ) ) ;
#81684 = CARTESIAN_POINT ( 'NONE',  ( 27.10511071441176867, -1.200000000000000030E-05, -8.806984339686344754 ) ) ;
#81685 = ORIENTED_EDGE ( 'NONE', *, *, #95627, .T. ) ;
#81686 = CARTESIAN_POINT ( 'NONE',  ( -10.20362117609958474, 43.27384007481603589, 15.40779740156164834 ) ) ;
#81687 = EDGE_LOOP ( 'NONE', ( #52999, #47494, #82110, #95684 ) ) ;
#81688 = CARTESIAN_POINT ( 'NONE',  ( -6.931554132363010545, -3.000000000000119904, -71.13906995426670221 ) ) ;
#81689 = DIRECTION ( 'NONE',  ( 0.000000000000000000, 0.000000000000000000, 1.000000000000000000 ) ) ;
#81690 = DIRECTION ( 'NONE',  ( -1.000000000000000000, -1.224606353822377258E-16, -0.000000000000000000 ) ) ;
#81691 = FACE_OUTER_BOUND ( 'NONE', #85676, .T. ) ;
#81692 = CARTESIAN_POINT ( 'NONE',  ( 66.15239626261548267, -56.85959143212516409, 99.15857335605178946 ) ) ;
#81693 = VECTOR ( 'NONE', #74302, 1000.000000000000000 ) ;
#81694 = ORIENTED_EDGE ( 'NONE', *, *, #21354, .F. ) ;
#81695 = CARTESIAN_POINT ( 'NONE',  ( 17.50000000000004974, 48.00000000000341771, 64.09949417230997426 ) ) ;
#81696 = CARTESIAN_POINT ( 'NONE',  ( 11.31153846153846132, 1.411358822780289120E-15, 0.000000000000000000 ) ) ;
#81697 = CONICAL_SURFACE ( 'NONE', #105812, 3.309500000000001663, 0.9599310885968770357 ) ;
#81698 = CARTESIAN_POINT ( 'NONE',  ( -72.13200937809398283, -57.67118076099990986, -33.88443861317198724 ) ) ;
#81699 = EDGE_CURVE ( 'NONE', #26344, #24916, #7082, .T. ) ;
#81700 = AXIS2_PLACEMENT_3D ( 'NONE', #75228, #18634, #43419 ) ;
#81702 = ORIENTED_EDGE ( 'NONE', *, *, #80311, .T. ) ;
#81701 = CIRCLE ( 'NONE', #59336, 4.000000000000000888 ) ;
#81703 = SURFACE_STYLE_FILL_AREA ( #88767 ) ;
#81704 = DIRECTION ( 'NONE',  ( -1.000000000000000000, 0.000000000000000000, 0.000000000000000000 ) ) ;
#81705 = ADVANCED_FACE ( 'NONE', ( #59315 ), #32128, .F. ) ;
#81706 = CARTESIAN_POINT ( 'NONE',  ( -34.34094660029732182, 491.0078558915762983, 12.00869558947848859 ) ) ;
#81707 = EDGE_CURVE ( 'NONE', #35136, #61647, #79143, .T. ) ;
#81708 = CARTESIAN_POINT ( 'NONE',  ( 8.000000000000000000, -24.68750000409677270, 0.000000000000000000 ) ) ;
#81709 = CARTESIAN_POINT ( 'NONE',  ( -5.219866590718559962, -5.000000000000000000, 8.922269033012391048 ) ) ;
#81710 = DIRECTION ( 'NONE',  ( -0.000000000000000000, 1.000000000000000000, -0.000000000000000000 ) ) ;
#81711 = EDGE_CURVE ( 'NONE', #20373, #21459, #32916, .T. ) ;
#81712 = PRESENTATION_STYLE_ASSIGNMENT (( #104965 ) ) ;
#81713 = CARTESIAN_POINT ( 'NONE',  ( -9.999733828770100530, 7.500380388541294074, 0.000000000000000000 ) ) ;
#81714 = CARTESIAN_POINT ( 'NONE',  ( 13.86650669486618881, 1.474610560812782335E-15, 0.000000000000000000 ) ) ;
#81715 = EDGE_LOOP ( 'NONE', ( #27366, #85946, #103338, #338, #5020, #35986 ) ) ;
#81716 = FILL_AREA_STYLE ('',( #8379 ) ) ;
#81717 = EDGE_CURVE ( 'NONE', #80543, #72025, #46675, .T. ) ;
#81718 = DIRECTION ( 'NONE',  ( 0.000000000000000000, -1.000000000000000000, 0.000000000000000000 ) ) ;
#81719 = CARTESIAN_POINT ( 'NONE',  ( -19.99999999999999289, -4.000000000000000000, -1.500000000000000000 ) ) ;
#81720 = CARTESIAN_POINT ( 'NONE',  ( -98.13696214071765667, -30.00000000000000000, 190.3767244705021824 ) ) ;
#81721 = VECTOR ( 'NONE', #36242, 999.9999999999998863 ) ;
#81722 = CARTESIAN_POINT ( 'NONE',  ( 56.98335268332530745, -57.67624654868168932, 97.45941025163602944 ) ) ;
#81724 = CARTESIAN_POINT ( 'NONE',  ( -9.590257352332137941, 7.202916011546355080, 2.216224026219065557 ) ) ;
#81723 = CARTESIAN_POINT ( 'NONE',  ( 6.338673411933466006, 41.81695763293575396, -59.02782193812689115 ) ) ;
#81725 = CARTESIAN_POINT ( 'NONE',  ( 16.22921596069147654, -24.49376654032824874, -38.52325167225695424 ) ) ;
#81726 = SURFACE_STYLE_FILL_AREA ( #91974 ) ;
#81728 = AXIS2_PLACEMENT_3D ( 'NONE', #28984, #61850, #52657 ) ;
#81727 = UNCERTAINTY_MEASURE_WITH_UNIT (LENGTH_MEASURE( 1.000000000000000082E-05 ), #78317, 'distance_accuracy_value', 'NONE');
#81729 = CARTESIAN_POINT ( 'NONE',  ( 16.75187969033441604, 36.38380281757147827, -24.30698433969211791 ) ) ;
#81730 = CARTESIAN_POINT ( 'NONE',  ( -21.88569129304039862, -60.00000000000001421, 40.49459113871581195 ) ) ;
#81731 = COLOUR_RGB ( '', 0.72549020, 0.75294118, 0.79215686) ;
#81732 =( REPRESENTATION_RELATIONSHIP ('NONE','NONE', #69581, #66748 ) REPRESENTATION_RELATIONSHIP_WITH_TRANSFORMATION ( #29270 )SHAPE_REPRESENTATION_RELATIONSHIP( ) );
#81733 = CARTESIAN_POINT ( 'NONE',  ( 26.84999999999999787, -3.309499999999999886, 0.000000000000000000 ) ) ;
#81734 = CARTESIAN_POINT ( 'NONE',  ( 36.71005241817402975, 463.3006260613077529, 20.13736821485172612 ) ) ;
#81735 = VECTOR ( 'NONE', #90177, 1000.000000000000000 ) ;
#81736 = CARTESIAN_POINT ( 'NONE',  ( -87.07927923840189521, -31.70337234844439323, 187.6114794693314423 ) ) ;
#81737 = ORIENTED_EDGE ( 'NONE', *, *, #93339, .F. ) ;
#81738 = CARTESIAN_POINT ( 'NONE',  ( 17.49999999999544897, 49.80818831228071986, 62.14041309008325698 ) ) ;
#81739 = CARTESIAN_POINT ( 'NONE',  ( 7.999999999999998224, -12.59374999999999467, 3.313708498984766049 ) ) ;
#81740 = CARTESIAN_POINT ( 'NONE',  ( -8.083102543024720532, -29.03117134383523634, 28.72105206599581351 ) ) ;
#81741 = CIRCLE ( 'NONE', #80071, 1.999999999999999778 ) ;
#81742 = DIRECTION ( 'NONE',  ( 0.000000000000000000, 1.000000000000000000, 0.000000000000000000 ) ) ;
#81744 = CARTESIAN_POINT ( 'NONE',  ( 3.185868710026582118, -70.04133017128596350, 13.36558777622290961 ) ) ;
#81743 = CARTESIAN_POINT ( 'NONE',  ( -104.0121244633587878, -59.99999999999999289, 190.7717994844543909 ) ) ;
#81745 = ORIENTED_EDGE ( 'NONE', *, *, #26221, .F. ) ;
#81746 = PRESENTATION_STYLE_ASSIGNMENT (( #48854 ) ) ;
#81747 = CARTESIAN_POINT ( 'NONE',  ( -5.885102640077104041, -4.999999999999960920, -15.35622078683719849 ) ) ;
#81748 = CARTESIAN_POINT ( 'NONE',  ( -7.212408192734266699, 32.01517089320368825, -3.465038817813884453 ) ) ;
#81749 = CARTESIAN_POINT ( 'NONE',  ( 28.93681320501227106, 306.6321427781763873, -9.151182930968348117 ) ) ;
#81750 = FACE_OUTER_BOUND ( 'NONE', #46684, .T. ) ;
#81751 = EDGE_CURVE ( 'NONE', #57113, #2149, #60487, .T. ) ;
#81752 = CARTESIAN_POINT ( 'NONE',  ( -7.897196874019792645, -81.20872795832192992, -1.302055520192090032 ) ) ;
#81753 = CARTESIAN_POINT ( 'NONE',  ( 72.07026148667476662, -59.99999999999998579, 154.8034499132735675 ) ) ;
#81754 = CARTESIAN_POINT ( 'NONE',  ( 114.5925949185997439, -60.00000000000001421, 172.8113841322393682 ) ) ;
#81755 = CARTESIAN_POINT ( 'NONE',  ( -45.49982102694234953, 388.3127959276886827, 7.886590035822850453 ) ) ;
#81756 = VERTEX_POINT ( 'NONE', #93270 ) ;
#81757 = CARTESIAN_POINT ( 'NONE',  ( -7.719366823438956970, -29.99999999999998579, 1.311865339813678588 ) ) ;
#81758 = CARTESIAN_POINT ( 'NONE',  ( 0.08224679563970911655, -6.145890662064644516, 5.355005115540896199 ) ) ;
#81759 =( LENGTH_UNIT ( ) NAMED_UNIT ( * ) SI_UNIT ( .MILLI., .METRE. ) );
#81761 = LINE ( 'NONE', #89360, #63222 ) ;
#81760 = CARTESIAN_POINT ( 'NONE',  ( 34.17730524443083340, -14.21045842199440656, 38.95112099893761837 ) ) ;
#81762 = CARTESIAN_POINT ( 'NONE',  ( 43.41041896048977833, 463.0441421627334080, 5.626145546387755658 ) ) ;
#81763 = ORIENTED_EDGE ( 'NONE', *, *, #65258, .F. ) ;
#81764 = UNCERTAINTY_MEASURE_WITH_UNIT (LENGTH_MEASURE( 1.000000000000000082E-05 ), #56235, 'distance_accuracy_value', 'NONE');
#81765 = CARTESIAN_POINT ( 'NONE',  ( -8.000000000000000000, -22.24999999999999289, -9.797174393178825657E-16 ) ) ;
#81766 = ORIENTED_EDGE ( 'NONE', *, *, #52220, .T. ) ;
#81767 = DIRECTION ( 'NONE',  ( 0.000000000000000000, 1.000000000000000000, 0.000000000000000000 ) ) ;
#81768 = AXIS2_PLACEMENT_3D ( 'NONE', #24848, #9685, #100824 ) ;
#81769 = DIRECTION ( 'NONE',  ( 0.000000000000000000, 0.000000000000000000, -1.000000000000000000 ) ) ;
#81770 = CARTESIAN_POINT ( 'NONE',  ( 41.50669491856072568, -5.000000000000000000, 6.123233995736768255E-16 ) ) ;
#81771 = CARTESIAN_POINT ( 'NONE',  ( 10.28624191511840280, 46.12099395432375104, 12.90779740156148847 ) ) ;
#81772 = VERTEX_POINT ( 'NONE', #61449 ) ;
#81773 = CARTESIAN_POINT ( 'NONE',  ( -10.00000000000000355, 15.00000000000000000, -10.00000000000000000 ) ) ;
#81774 = CARTESIAN_POINT ( 'NONE',  ( 5.000000000000000888, -12.45789892056853532, 11.15956302481758300 ) ) ;
#81775 = CARTESIAN_POINT ( 'NONE',  ( -73.28166430171110335, -59.99999999999997868, 185.8704270832439818 ) ) ;
#81776 = DIRECTION ( 'NONE',  ( -1.000000000000000000, -0.000000000000000000, -0.000000000000000000 ) ) ;
#81777 = CARTESIAN_POINT ( 'NONE',  ( 84.62254331935226048, -60.00000000000000000, 199.8705729347711610 ) ) ;
#81779 = CARTESIAN_POINT ( 'NONE',  ( 17.08831453699968961, -56.87710783578985030, 33.63502463005767851 ) ) ;
#81778 = CARTESIAN_POINT ( 'NONE',  ( -107.3650189024811681, -30.00000000000002842, 190.7478110277085648 ) ) ;
#81780 = CARTESIAN_POINT ( 'NONE',  ( 89.12305573924987812, -37.99999999999999289, 73.21436059126565965 ) ) ;
#81781 = CARTESIAN_POINT ( 'NONE',  ( 0.000000000000000000, 0.000000000000000000, 0.000000000000000000 ) ) ;
#81782 = EDGE_CURVE ( 'NONE', #95649, #29485, #22682, .T. ) ;
#81783 = CARTESIAN_POINT ( 'NONE',  ( -47.01588246310362251, -29.15368591072060411, 43.19123847651081149 ) ) ;
#81784 = B_SPLINE_CURVE_WITH_KNOTS ( 'NONE', 3,
 ( #57408, #82764, #65525, #100535, #26698, #33705, #98412, #98925, #25086, #16980, #49858, #65530, #39148, #96323, #39674, #90330, #97348, #72028, #15908, #81680 ),
 .UNSPECIFIED., .F., .F.,
 ( 4, 2, 2, 2, 2, 2, 2, 2, 2, 4 ),
 ( 0.003017764547143146799, 0.003522452000831426643, 0.004027139454519706487, 0.004531826908207986331, 0.005036514361896267042, 0.005288858088740406097, 0.005541201815584546886, 0.006045889269272826730, 0.006550576722961107441, 0.007055264176649387285 ),
 .UNSPECIFIED. ) ;
#81785 = CARTESIAN_POINT ( 'NONE',  ( -17.34830914839865201, 18.64284798592992232, 34.29224544877759939 ) ) ;
#81786 = ORIENTED_EDGE ( 'NONE', *, *, #106008, .F. ) ;
#81787 = FILL_AREA_STYLE ('',( #40815 ) ) ;
#81788 = CARTESIAN_POINT ( 'NONE',  ( 7.126148245860624009, 41.12758397993106740, -58.55282951229289523 ) ) ;
#81789 = CARTESIAN_POINT ( 'NONE',  ( 29.01988888469873018, 321.8047804620298393, 14.12772110426748284 ) ) ;
#81790 = CARTESIAN_POINT ( 'NONE',  ( -6.010545793716514417E-15, 5.948846446048893455, -2.696295709017758391 ) ) ;
#81791 = EDGE_CURVE ( 'NONE', #55300, #98139, #57047, .T. ) ;
#81792 = LINE ( 'NONE', #73713, #44771 ) ;
#81793 = CARTESIAN_POINT ( 'NONE',  ( 23.95564068939877345, 305.6666757346319514, -9.824255363917307804 ) ) ;
#81794 = VERTEX_POINT ( 'NONE', #20506 ) ;
#81795 = CARTESIAN_POINT ( 'NONE',  ( 4.464768147782974594, -48.00301508167390807, 102.6740199126133888 ) ) ;
#81796 = EDGE_LOOP ( 'NONE', ( #94040, #12015, #98034, #47675 ) ) ;
#81797 = CARTESIAN_POINT ( 'NONE',  ( 81.59718390748527383, -30.00000000000000711, -5.918344230650005144 ) ) ;
#81798 = CARTESIAN_POINT ( 'NONE',  ( 46.86466781827407857, 13.70365495135300016, 15.14281811549618340 ) ) ;
#81799 = CARTESIAN_POINT ( 'NONE',  ( 11.28351131189992174, -9.073918974790322167, -0.5344654698446129615 ) ) ;
#81800 = CARTESIAN_POINT ( 'NONE',  ( 92.42131551263139499, -30.00000000000000355, 102.6390630386317326 ) ) ;
#81801 = CARTESIAN_POINT ( 'NONE',  ( 7.986539162393897939, 101.0267282894254635, -0.5321833565149908241 ) ) ;
#81802 = ORIENTED_EDGE ( 'NONE', *, *, #69934, .T. ) ;
#81803 = AXIS2_PLACEMENT_3D ( 'NONE', #22176, #87957, #22712 ) ;
#81804 = ORIENTED_EDGE ( 'NONE', *, *, #89010, .F. ) ;
#81805 = ORIENTED_EDGE ( 'NONE', *, *, #78118, .T. ) ;
#81806 = CARTESIAN_POINT ( 'NONE',  ( 0.01678220608715907600, 0.7854258608507247441, -8.000000000000001776 ) ) ;
#81807 = CARTESIAN_POINT ( 'NONE',  ( 22.13738121435902428, 25.65584458174092930, 32.60528274926500814 ) ) ;
#81808 = CIRCLE ( 'NONE', #6061, 5.000000000000001776 ) ;
#81809 =( NAMED_UNIT ( * ) PLANE_ANGLE_UNIT ( ) SI_UNIT ( $, .RADIAN. ) );
#81810 = ORIENTED_EDGE ( 'NONE', *, *, #21161, .T. ) ;
#81811 = EDGE_CURVE ( 'NONE', #16675, #85958, #82966, .T. ) ;
#81812 = CARTESIAN_POINT ( 'NONE',  ( 9.482993638194542996, 107.4434872025367724, -3.177441187500465780 ) ) ;
#81813 = EDGE_LOOP ( 'NONE', ( #38506, #69595, #63152, #47266, #30680 ) ) ;
#81814 = CARTESIAN_POINT ( 'NONE',  ( 12.61650669486618881, 1.474610560812782335E-15, 0.000000000000000000 ) ) ;
#81815 = CARTESIAN_POINT ( 'NONE',  ( 86.53517077683734726, -38.61542584032831371, 199.3319270115290749 ) ) ;
#81816 = CARTESIAN_POINT ( 'NONE',  ( 33.50421398922629379, 488.2600042842303196, 10.59612602190272312 ) ) ;
#81817 =( GEOMETRIC_REPRESENTATION_CONTEXT ( 3 ) GLOBAL_UNCERTAINTY_ASSIGNED_CONTEXT ( ( #83266 ) ) GLOBAL_UNIT_ASSIGNED_CONTEXT ( ( #35376, #11579, #94108 ) ) REPRESENTATION_CONTEXT ( 'NONE', 'WORKASPACE' ) );
#81818 = VECTOR ( 'NONE', #26809, 1000.000000000000000 ) ;
#81819 = CARTESIAN_POINT ( 'NONE',  ( 30.50659871040408078, 318.9590941947862461, 13.89418334184498427 ) ) ;
#81820 = CIRCLE ( 'NONE', #102557, 10.00000000000000000 ) ;
#81821 = FACE_OUTER_BOUND ( 'NONE', #57016, .T. ) ;
#81822 = CIRCLE ( 'NONE', #35374, 4.000000000000000888 ) ;
#81823 = LINE ( 'NONE', #7946, #61438 ) ;
#81824 = AXIS2_PLACEMENT_3D ( 'NONE', #41014, #56104, #73359 ) ;
#81825 = CARTESIAN_POINT ( 'NONE',  ( -41.35951450184050771, 460.7308729162644454, 2.709719765164665617 ) ) ;
#81826 = CARTESIAN_POINT ( 'NONE',  ( -4.725902370229717597, -47.47364726308471461, 103.4500010546492490 ) ) ;
#81827 = CARTESIAN_POINT ( 'NONE',  ( 32.71902930631058837, 485.4797908183053323, 6.287473911065069920 ) ) ;
#81828 = VERTEX_POINT ( 'NONE', #60916 ) ;
#81829 = CARTESIAN_POINT ( 'NONE',  ( 2.109905305157752764, -49.78906980863433063, 102.5368276707881137 ) ) ;
#81830 = CARTESIAN_POINT ( 'NONE',  ( -28.24278080084331322, 297.1537272779650607, 10.44109103508797887 ) ) ;
#81831 = CARTESIAN_POINT ( 'NONE',  ( 7.315042831255333944, 54.29841258322443309, -2.636459647254548511 ) ) ;
#81832 = UNCERTAINTY_MEASURE_WITH_UNIT (LENGTH_MEASURE( 1.000000000000000082E-05 ), #101047, 'distance_accuracy_value', 'NONE');
#81833 = EDGE_CURVE ( 'NONE', #44644, #58313, #94882, .T. ) ;
#81834 =( NAMED_UNIT ( * ) SI_UNIT ( $, .STERADIAN. ) SOLID_ANGLE_UNIT ( ) );
#81835 = CARTESIAN_POINT ( 'NONE',  ( -3.313708498984760720, -12.03124999999999289, -8.000000000000000000 ) ) ;
#81836 = DIRECTION ( 'NONE',  ( 0.000000000000000000, -1.000000000000000000, 0.000000000000000000 ) ) ;
#81837 =( BOUNDED_SURFACE ( )  B_SPLINE_SURFACE ( 3, 2, ( 
 ( #81445, #38905, #97115 ),
 ( #31366, #14063, #72830 ),
 ( #64242, #16195, #81978 ),
 ( #30831, #56647, #22736 ) ),
 .UNSPECIFIED., .F., .F., .F. ) 
 B_SPLINE_SURFACE_WITH_KNOTS ( ( 4, 4 ),
 ( 3, 3 ),
 ( 0.007093323349943533689, 0.03301372383216878009 ),
 ( 0.000000000000000000, 1.000000000000000000 ),
 .UNSPECIFIED. ) 
 GEOMETRIC_REPRESENTATION_ITEM ( )  RATIONAL_B_SPLINE_SURFACE ( (
 ( 1.000000000000000000, 0.8381405729291011575, 1.000000000000000000),
 ( 1.000000000000000000, 0.8381407632135386976, 1.000000000000000000),
 ( 1.000000000000000000, 0.8381408010577027223, 1.000000000000000000),
 ( 1.000000000000000000, 0.8381406085692050256, 1.000000000000000000) ) ) 
 REPRESENTATION_ITEM ( '' )  SURFACE ( )  );
#81838 = EDGE_CURVE ( 'NONE', #78825, #51255, #69009, .T. ) ;
#81839 = DIRECTION ( 'NONE',  ( 0.5735764363510440500, 0.8191520442889932418, 0.000000000000000000 ) ) ;
#81840 = EDGE_CURVE ( 'NONE', #71103, #88610, #53862, .T. ) ;
#81841 = CARTESIAN_POINT ( 'NONE',  ( 0.000000000000000000, 303.8518027762758038, 9.936999415352289589 ) ) ;
#81842 = ORIENTED_EDGE ( 'NONE', *, *, #91719, .F. ) ;
#81843 = CARTESIAN_POINT ( 'NONE',  ( 85.63209264575189650, -32.09773112560883845, 181.8786679553494139 ) ) ;
#81844 = DIRECTION ( 'NONE',  ( 0.8660254037844374864, -0.5000000000000019984, 0.000000000000000000 ) ) ;
#81845 = VERTEX_POINT ( 'NONE', #53343 ) ;
#81846 = CARTESIAN_POINT ( 'NONE',  ( 80.85454081142110283, -57.67117862881983825, -29.75008775089105839 ) ) ;
#81847 = CARTESIAN_POINT ( 'NONE',  ( 42.58433969240391548, 479.4768267386956495, 9.887265036232028237 ) ) ;
#81848 = EDGE_CURVE ( 'NONE', #63111, #74912, #7162, .T. ) ;
#81849 = CARTESIAN_POINT ( 'NONE',  ( 29.49969761086837039, 8.554442461696856626, 42.10535821593482808 ) ) ;
#81850 = AXIS2_PLACEMENT_3D ( 'NONE', #67568, #19589, #85337 ) ;
#81851 = EDGE_CURVE ( 'NONE', #60121, #73382, #51732, .T. ) ;
#81852 = CARTESIAN_POINT ( 'NONE',  ( -81.23006925269818623, -30.00000000000000000, 0.5274897246537498807 ) ) ;
#81853 = CARTESIAN_POINT ( 'NONE',  ( 28.43348347353515493, 17.76907357228465756, 40.77956405912743065 ) ) ;
#81854 = CARTESIAN_POINT ( 'NONE',  ( 7.137815226410160641, -3.000000000000000000, -4.175893272574602300 ) ) ;
#81855 = LINE ( 'NONE', #88391, #15318 ) ;
#81857 = DIRECTION ( 'NONE',  ( -1.000000000000000000, -1.224606353822377258E-16, -0.000000000000000000 ) ) ;
#81856 = CARTESIAN_POINT ( 'NONE',  ( 17.33349330513380337, -7.703719777548943412E-31, 4.000000000000001776 ) ) ;
#81858 = CYLINDRICAL_SURFACE ( 'NONE', #28757, 1.250000000000001110 ) ;
#81859 = CARTESIAN_POINT ( 'NONE',  ( -29.07959870117770862, 18.85554092054060149, 39.75803059074582535 ) ) ;
#81860 = CARTESIAN_POINT ( 'NONE',  ( -15.43380028733834841, 44.00385025579843301, -5.763122072303904275 ) ) ;
#81861 = CARTESIAN_POINT ( 'NONE',  ( 5.911778709945830101, -81.13338160583427339, 1.058844270818174227 ) ) ;
#81862 = CARTESIAN_POINT ( 'NONE',  ( -18.42187549159172733, -25.79542283499425892, -30.46429929900222078 ) ) ;
#81863 = DIRECTION ( 'NONE',  ( 0.000000000000000000, 0.000000000000000000, 1.000000000000000000 ) ) ;
#81864 = CARTESIAN_POINT ( 'NONE',  ( 33.88237199998285121, 485.0486819176492759, 1.241522336454517594 ) ) ;
#81866 = VECTOR ( 'NONE', #103250, 999.9999999999998863 ) ;
#81865 = B_SPLINE_CURVE_WITH_KNOTS ( 'NONE', 3,
 ( #768, #90356, #57434, #33735, #82256, #97372, #241, #56370, #39699, #23533, #42868, #10493, #52015, #18624, #36421, #94080, #75219, #51484, #50939, #92474, #76822, #18080 ),
 .UNSPECIFIED., .F., .F.,
 ( 4, 2, 2, 2, 2, 2, 2, 2, 2, 2, 4 ),
 ( 0.002861759807556418182, 0.003365147677020101629, 0.003868535546483784643, 0.004875311285411144599, 0.005127005220142985889, 0.005378699154874826312, 0.005630393089606666734, 0.005882087024338508024, 0.006385474893802188870, 0.006637168828534030160, 0.006888862763265871450 ),
 .UNSPECIFIED. ) ;
#81867 = ORIENTED_EDGE ( 'NONE', *, *, #29467, .F. ) ;
#81868 = CARTESIAN_POINT ( 'NONE',  ( 17.33349330513380693, 1.593028355512270962E-15, 0.000000000000000000 ) ) ;
#81869 =( LENGTH_UNIT ( ) NAMED_UNIT ( * ) SI_UNIT ( .MILLI., .METRE. ) );
#81870 = CARTESIAN_POINT ( 'NONE',  ( 7.500000000000002665, 4.320742148886384193, -27.76523484934585895 ) ) ;
#81871 = CARTESIAN_POINT ( 'NONE',  ( -21.15837276345346041, -18.88847407013843949, -33.56547457277724078 ) ) ;
#81873 = CARTESIAN_POINT ( 'NONE',  ( -24.94440323778573543, -21.77047479305005595, -29.25379890206748712 ) ) ;
#81872 = LINE ( 'NONE', #7998, #24379 ) ;
#81874 = AXIS2_PLACEMENT_3D ( 'NONE', #19951, #3727, #28033 ) ;
#81875 = ORIENTED_EDGE ( 'NONE', *, *, #85574, .F. ) ;
#81876 = B_SPLINE_CURVE_WITH_KNOTS ( 'NONE', 3,
 ( #16643, #25299, #58157, #91084, #39866, #105128, #73808, #73261, #32854, #90000, #65731, #49532, #82441, #15574, #47403, #31782, #74338, #106161, #80298, #412, #81887, #32322, #48466, #81354, #16106, #105642, #65193, #6948, #8007, #33379 ),
 .UNSPECIFIED., .F., .F.,
 ( 4, 2, 2, 2, 2, 2, 2, 2, 2, 2, 2, 2, 2, 2, 4 ),
 ( 0.000000000000000000, 0.004502481766811746930, 0.009004963533623493860, 0.01800992706724694262, 0.02026116795065281695, 0.02251240883405868781, 0.02701489060087041219, 0.03601985413449383666, 0.04502481766811725766, 0.05402978120174068560, 0.05853226296855238570, 0.06303474473536410660, 0.06753722650217582057, 0.06978846738558167062, 0.07203970826898753455 ),
 .UNSPECIFIED. ) ;
#81877 = ORIENTED_EDGE ( 'NONE', *, *, #38797, .F. ) ;
#81879 = VECTOR ( 'NONE', #10577, 1000.000000000000000 ) ;
#81878 = CARTESIAN_POINT ( 'NONE',  ( -10.00000000000000355, 15.00000000000000000, -10.00000000000000000 ) ) ;
#81880 = CIRCLE ( 'NONE', #19977, 0.9999999999999875655 ) ;
#81881 = EDGE_CURVE ( 'NONE', #96201, #3065, #8859, .T. ) ;
#81882 = CARTESIAN_POINT ( 'NONE',  ( -8.000000000000000000, -29.84374999999999645, -3.313708498984762496 ) ) ;
#81883 = FACE_OUTER_BOUND ( 'NONE', #94555, .T. ) ;
#81884 = AXIS2_PLACEMENT_3D ( 'NONE', #44789, #11859, #77680 ) ;
#81885 = CARTESIAN_POINT ( 'NONE',  ( -88.32040418460222497, -60.00000000000000711, -21.20476073071671763 ) ) ;
#81886 = ORIENTED_EDGE ( 'NONE', *, *, #37992, .T. ) ;
#81887 = CARTESIAN_POINT ( 'NONE',  ( 17.04335540256958481, -25.31244954732083130, -30.48127871544292589 ) ) ;
#81888 = PRESENTATION_LAYER_ASSIGNMENT (  '', '', ( #18199 ) ) ;
#81889 = CARTESIAN_POINT ( 'NONE',  ( 0.000000000000000000, 81.00000000000000000, 0.000000000000000000 ) ) ;
#81890 = VECTOR ( 'NONE', #96404, 999.9999999999998863 ) ;
#81891 = CARTESIAN_POINT ( 'NONE',  ( -3.351410929237275571, -0.9950782767056199907, 104.3292106331608835 ) ) ;
#81892 = AXIS2_PLACEMENT_3D ( 'NONE', #62435, #75543, #13319 ) ;
#81894 = CARTESIAN_POINT ( 'NONE',  ( -46.89572507581434024, 12.86406951795958520, 16.16260000396507834 ) ) ;
#81893 = DIRECTION ( 'NONE',  ( 0.5735764363510442720, -0.8191520442889930198, 1.003171929053526349E-16 ) ) ;
#81895 = VERTEX_POINT ( 'NONE', #102424 ) ;
#81896 = AXIS2_PLACEMENT_3D ( 'NONE', #102799, #18722, #12177 ) ;
#81897 = VERTEX_POINT ( 'NONE', #28565 ) ;
#81898 = VERTEX_POINT ( 'NONE', #94344 ) ;
#81899 = CARTESIAN_POINT ( 'NONE',  ( 28.85163153077909115, 319.8032021574594523, 12.62209958446642588 ) ) ;
#81900 = EDGE_CURVE ( 'NONE', #105469, #84646, #49523, .T. ) ;
#81901 = CARTESIAN_POINT ( 'NONE',  ( -5.000000000000000000, -15.43644767549520580, 12.61250542914465811 ) ) ;
#81902 = CYLINDRICAL_SURFACE ( 'NONE', #31168, 1.250000000000001110 ) ;
#81903 = ORIENTED_EDGE ( 'NONE', *, *, #3641, .T. ) ;
#81904 = DIRECTION ( 'NONE',  ( -1.000000000000000000, -1.224606353822377258E-16, -0.000000000000000000 ) ) ;
#81905 = CARTESIAN_POINT ( 'NONE',  ( -0.000000000000000000, 17.51648154115788714, -55.02144460582525909 ) ) ;
#81906 = CARTESIAN_POINT ( 'NONE',  ( -33.00496812084397646, 465.6658704666172639, 15.15901827095664522 ) ) ;
#81907 = CARTESIAN_POINT ( 'NONE',  ( -29.62390339563712160, -57.68322450639401211, 45.06481242858825453 ) ) ;
#81908 = CARTESIAN_POINT ( 'NONE',  ( -2.977408999572654480, -33.12500000204838813, 7.188101187499999156 ) ) ;
#81909 = CARTESIAN_POINT ( 'NONE',  ( 7.344133061198927059, -67.44494392680579153, 3.176267128233876136 ) ) ;
#81910 = LINE ( 'NONE', #24258, #85629 ) ;
#81911 = CARTESIAN_POINT ( 'NONE',  ( 1.011040197152363929, 28.02085159631482369, -38.74701891561100098 ) ) ;
#81912 = CARTESIAN_POINT ( 'NONE',  ( 33.15797435408901350, -29.99999999999994671, -37.92174772678599481 ) ) ;
#81913 = CARTESIAN_POINT ( 'NONE',  ( -25.54656159126955117, -59.99999999999990763, 43.65498583421084788 ) ) ;
#81914 = CARTESIAN_POINT ( 'NONE',  ( -54.70400683262975861, -18.68943135379251785, 51.56070947385185121 ) ) ;
#81915 = CARTESIAN_POINT ( 'NONE',  ( 3.972670526825609283, 18.38964615182245410, -5.763849554103598116 ) ) ;
#81916 = ORIENTED_EDGE ( 'NONE', *, *, #11892, .T. ) ;
#81917 = CARTESIAN_POINT ( 'NONE',  ( -95.67593075084288046, -37.68573934914535783, 192.9981947302272260 ) ) ;
#81918 = CARTESIAN_POINT ( 'NONE',  ( -7.653149674035952366, 294.7103690674142626, -6.445128602722142830 ) ) ;
#81919 = EDGE_CURVE ( 'NONE', #10644, #8974, #67467, .T. ) ;
#81920 = CARTESIAN_POINT ( 'NONE',  ( 9.923336144128633407, -3.232982157722304351, 15.16488001955000975 ) ) ;
#81921 = ORIENTED_EDGE ( 'NONE', *, *, #53077, .T. ) ;
#81922 = LINE ( 'NONE', #40953, #11483 ) ;
#81923 = CARTESIAN_POINT ( 'NONE',  ( 110.0758566615390919, -38.35596056441075774, 185.5239908131719062 ) ) ;
#81924 = CARTESIAN_POINT ( 'NONE',  ( 63.56127108291158123, 4.000000000000013323, 0.000000000000000000 ) ) ;
#81925 = CARTESIAN_POINT ( 'NONE',  ( -5.612570156906559582, 51.99084277534022647, -6.070783327326104484 ) ) ;
#81926 = CARTESIAN_POINT ( 'NONE',  ( -9.846553493373482624, 302.6513161806682888, 9.894388782117784942 ) ) ;
#81927 = STYLED_ITEM ( 'NONE', ( #86292 ), #99717 ) ;
#81928 = DIRECTION ( 'NONE',  ( 1.000000000000000000, 0.000000000000000000, 0.000000000000000000 ) ) ;
#81929 = CARTESIAN_POINT ( 'NONE',  ( 84.45385566677610711, -30.00000000000000355, 165.1424632750193382 ) ) ;
#81930 = EDGE_CURVE ( 'NONE', #87882, #58831, #51894, .T. ) ;
#81931 = CARTESIAN_POINT ( 'NONE',  ( 37.00151214921998388, 491.8254423329678957, 12.57683263657896688 ) ) ;
#81932 = CARTESIAN_POINT ( 'NONE',  ( -32.13004029922196736, 464.8241378157327404, 14.61694575657911166 ) ) ;
#81933 = DIRECTION ( 'NONE',  ( 0.000000000000000000, 0.000000000000000000, 1.000000000000000000 ) ) ;
#81934 = ORIENTED_EDGE ( 'NONE', *, *, #99693, .F. ) ;
#81935 = ORIENTED_EDGE ( 'NONE', *, *, #72828, .T. ) ;
#81936 = CARTESIAN_POINT ( 'NONE',  ( 48.74081811396350616, -56.82235822615641041, 54.29662734949555158 ) ) ;
#81937 = CARTESIAN_POINT ( 'NONE',  ( 6.770722867741076456, 41.58070725240481380, -58.79856991761213436 ) ) ;
#81938 = CARTESIAN_POINT ( 'NONE',  ( 9.323069064330987032, 51.33816002439836268, 3.784642684411407831 ) ) ;
#81939 = ORIENTED_EDGE ( 'NONE', *, *, #54014, .T. ) ;
#81940 = CARTESIAN_POINT ( 'NONE',  ( -96.80470072259791436, -38.35514435266657074, 69.38109125240286801 ) ) ;
#81941 = ORIENTED_EDGE ( 'NONE', *, *, #61958, .F. ) ;
#81942 = FACE_OUTER_BOUND ( 'NONE', #101094, .T. ) ;
#81943 = CARTESIAN_POINT ( 'NONE',  ( 91.32288730115537589, -38.35303533275899213, 27.69273911151131529 ) ) ;
#81944 = CARTESIAN_POINT ( 'NONE',  ( 10.63868951441825494, 13.01770488547337123, -10.01969491620919328 ) ) ;
#81945 = CARTESIAN_POINT ( 'NONE',  ( -27.10511071441183617, 34.75829513984614039, 7.556984339678626483 ) ) ;
#81946 = CARTESIAN_POINT ( 'NONE',  ( 100.6486840550021640, -37.84864322520951418, 144.5881869147006000 ) ) ;
#81947 = DIRECTION ( 'NONE',  ( 1.000000000000000000, -0.000000000000000000, -0.000000000000000000 ) ) ;
#81948 = CARTESIAN_POINT ( 'NONE',  ( -28.34990703596096395, 308.9679587906881579, -9.065518352637484512 ) ) ;
#81949 = CARTESIAN_POINT ( 'NONE',  ( 6.326445470157510798, 6.578717624163890498, -2.268395195563515099 ) ) ;
#81950 = CARTESIAN_POINT ( 'NONE',  ( 74.36630564409178135, -60.00000000000000000, 175.8464028054124810 ) ) ;
#81951 = AXIS2_PLACEMENT_3D ( 'NONE', #85647, #101292, #69456 ) ;
#81952 = ADVANCED_FACE ( 'NONE', ( #79204 ), #93256, .T. ) ;
#81953 = FACE_OUTER_BOUND ( 'NONE', #53336, .T. ) ;
#81954 = VERTEX_POINT ( 'NONE', #56502 ) ;
#81955 = CARTESIAN_POINT ( 'NONE',  ( 61.32550633558473407, -25.58970342268792209, 69.10268843958327523 ) ) ;
#81956 = CARTESIAN_POINT ( 'NONE',  ( -24.54082342953966034, 303.7793720978580723, -9.799731773458871587 ) ) ;
#81957 = CARTESIAN_POINT ( 'NONE',  ( -2.499999999999996003, -8.000000000000000000, -14.79019945774904166 ) ) ;
#81958 =( GEOMETRIC_REPRESENTATION_CONTEXT ( 3 ) GLOBAL_UNCERTAINTY_ASSIGNED_CONTEXT ( ( #15994 ) ) GLOBAL_UNIT_ASSIGNED_CONTEXT ( ( #104552, #96999, #88907 ) ) REPRESENTATION_CONTEXT ( 'NONE', 'WORKASPACE' ) );
#81959 = CARTESIAN_POINT ( 'NONE',  ( -9.384368963317969659, -5.000000000000000000, -18.81659302942708223 ) ) ;
#81961 = CARTESIAN_POINT ( 'NONE',  ( -4.044615342289579196, 54.03559733567681178, 7.473308606069148929 ) ) ;
#81960 = CARTESIAN_POINT ( 'NONE',  ( -69.83122382787961158, -29.99999999991972999, 126.8444822361123130 ) ) ;
#81962 = CARTESIAN_POINT ( 'NONE',  ( -42.47047798398502749, 355.1276945667507334, 15.62095130985220059 ) ) ;
#81963 = CARTESIAN_POINT ( 'NONE',  ( -38.54780640362174893, 25.36754422839498702, -11.41492091183227586 ) ) ;
#81964 = CARTESIAN_POINT ( 'NONE',  ( 84.73333333333332007, 1.023464760207051730E-14, 0.000000000000000000 ) ) ;
#81965 = CARTESIAN_POINT ( 'NONE',  ( -5.656854249492379694, -31.43749999999999289, -5.656854249492380582 ) ) ;
#81966 = CIRCLE ( 'NONE', #45801, 11.00000000000000000 ) ;
#81967 = STYLED_ITEM ( 'NONE', ( #34225 ), #88446 ) ;
#81968 = CIRCLE ( 'NONE', #35522, 7.000000000000000000 ) ;
#81969 = VECTOR ( 'NONE', #102635, 1000.000000000000000 ) ;
#81970 = CARTESIAN_POINT ( 'NONE',  ( 91.95555555555554861, 4.172000000000019249, 5.109226446042768454E-16 ) ) ;
#81971 =( GEOMETRIC_REPRESENTATION_CONTEXT ( 3 ) GLOBAL_UNCERTAINTY_ASSIGNED_CONTEXT ( ( #60228 ) ) GLOBAL_UNIT_ASSIGNED_CONTEXT ( ( #106042, #88301, #39747 ) ) REPRESENTATION_CONTEXT ( 'NONE', 'WORKASPACE' ) );
#81972 = EDGE_LOOP ( 'NONE', ( #52409, #92111, #106397, #84819 ) ) ;
#81973 = CARTESIAN_POINT ( 'NONE',  ( 81.36577150990262908, -56.99468229981764722, 181.4257631377957125 ) ) ;
#81974 = CARTESIAN_POINT ( 'NONE',  ( 5.833333333333327708, -46.27176886455111315, 103.8776713793258750 ) ) ;
#81975 = CARTESIAN_POINT ( 'NONE',  ( -39.46184362519017697, 438.4175760117823870, 22.75062681417281496 ) ) ;
#81976 = VERTEX_POINT ( 'NONE', #38249 ) ;
#81977 = CARTESIAN_POINT ( 'NONE',  ( 6.683837171061802529, -3.955946848495957457, 6.851900933636990487 ) ) ;
#81978 = CARTESIAN_POINT ( 'NONE',  ( 38.83535783861245250, 468.9533400912722527, 0.4924304409069520938 ) ) ;
#81979 = SURFACE_STYLE_USAGE ( .BOTH. , #55054 ) ;
#81980 = DIRECTION ( 'NONE',  ( -1.000000000000000000, 0.000000000000000000, 0.000000000000000000 ) ) ;
#81981 = AXIS2_PLACEMENT_3D ( 'NONE', #34573, #25412, #26482 ) ;
#81982 = EDGE_CURVE ( 'NONE', #15547, #25416, #25113, .T. ) ;
#81983 = FILL_AREA_STYLE_COLOUR ( '', #2614 ) ;
#81984 =( BOUNDED_CURVE ( )  B_SPLINE_CURVE ( 2, ( #91621, #76473, #43065, #27452, #60332, #41986, #66805, #17730, #956 ),
 .UNSPECIFIED., .F., .F. ) 
 B_SPLINE_CURVE_WITH_KNOTS ( ( 3, 2, 2, 2, 3 ),
 ( 0.2500000000000000555, 0.2573529411764705621, 0.2647058823529411797, 0.2720588235294116863, 0.2794117647058823040 ),
 .UNSPECIFIED. ) 
 CURVE ( )  GEOMETRIC_REPRESENTATION_ITEM ( )  RATIONAL_B_SPLINE_CURVE ( ( 0.9999999999999994449, 0.9238795325112872936, 1.000000000000000000, 0.9238795325112867385, 1.000000000000000000, 0.9238795325112867385, 1.000000000000000000, 0.9238795325112872936, 0.9999999999999994449 ) ) 
 REPRESENTATION_ITEM ( '' )  );
#81985 = EDGE_CURVE ( 'NONE', #27751, #33663, #50200, .T. ) ;
#81986 = PRESENTATION_STYLE_ASSIGNMENT (( #16202 ) ) ;
#81987 = EDGE_CURVE ( 'NONE', #33722, #97138, #89432, .T. ) ;
#81988 = CARTESIAN_POINT ( 'NONE',  ( 6.838238910409968341, -3.993980678889280878, -6.572970348078617242 ) ) ;
#81989 = CARTESIAN_POINT ( 'NONE',  ( 0.5674423241763830728, 26.02818786376027660, 38.38311945757907040 ) ) ;
#81991 = CARTESIAN_POINT ( 'NONE',  ( -10.83414860630037602, 18.76830525476172440, -9.162768138102793003 ) ) ;
#81990 = CARTESIAN_POINT ( 'NONE',  ( -11.33263781917016466, -20.80137080723078213, 35.49740132007826077 ) ) ;
#81992 = B_SPLINE_CURVE_WITH_KNOTS ( 'NONE', 3,
 ( #16082, #58684, #7442, #48962, #73237, #917, #58135, #91061, #25830, #7983, #100192, #32296, #50040, #67311 ),
 .UNSPECIFIED., .F., .F.,
 ( 4, 2, 2, 2, 2, 2, 4 ),
 ( 6.938893903907228378E-18, 0.0004833252911870726618, 0.0009666505823741383847, 0.001208313227967711253, 0.001449975873561284339, 0.001691638519154857207, 0.001933301164748430293 ),
 .UNSPECIFIED. ) ;
#81993 = CARTESIAN_POINT ( 'NONE',  ( 7.188101187500000044, -13.15625000204838280, 0.000000000000000000 ) ) ;
#81994 = CARTESIAN_POINT ( 'NONE',  ( -63.03617022304293727, 40.83906611473187809, -16.93907820429951983 ) ) ;
#81995 = DIRECTION ( 'NONE',  ( 0.5735764363510554853, 0.8191520442889852482, 0.000000000000000000 ) ) ;
#81996 = AXIS2_PLACEMENT_3D ( 'NONE', #77956, #52600, #37001 ) ;
#81997 = EDGE_LOOP ( 'NONE', ( #96601, #68194, #63006, #93513, #102474, #104186 ) ) ;
#81998 = CARTESIAN_POINT ( 'NONE',  ( -19.35735956073961006, 49.90708382026840439, 61.17470024478767243 ) ) ;
#81999 = FACE_OUTER_BOUND ( 'NONE', #96211, .T. ) ;
#82000 = AXIS2_PLACEMENT_3D ( 'NONE', #53024, #93495, #102093 ) ;
#82001 = CARTESIAN_POINT ( 'NONE',  ( -9.609486011791425142, 143.0915023496523020, -5.000000000000000888 ) ) ;
#82002 = CARTESIAN_POINT ( 'NONE',  ( -7.225703553025885739, -5.000000000000001776, -73.19314196553557395 ) ) ;
#82003 = CARTESIAN_POINT ( 'NONE',  ( 4.036225360327396317, 54.13868825708020438, 7.154357340812832255 ) ) ;
#82004 = ORIENTED_EDGE ( 'NONE', *, *, #10670, .F. ) ;
#82005 = CARTESIAN_POINT ( 'NONE',  ( -4.472135954999579610, -85.00000000000000000, 4.000000000000001776 ) ) ;
#82006 = CARTESIAN_POINT ( 'NONE',  ( -4.093111970549610845, 52.07643660103700256, 6.911618801915782484 ) ) ;
#82007 = ORIENTED_EDGE ( 'NONE', *, *, #53088, .F. ) ;
#82008 = DIRECTION ( 'NONE',  ( -0.000000000000000000, -1.000000000000000000, -0.000000000000000000 ) ) ;
#82009 = EDGE_CURVE ( 'NONE', #9858, #41746, #31305, .T. ) ;
#82010 = CARTESIAN_POINT ( 'NONE',  ( 7.770228158362350257, 5.000000000000004441, 6.123233995736770227E-16 ) ) ;
#82011 = CARTESIAN_POINT ( 'NONE',  ( 0.000000000000000000, -46.00000000000000000, 112.0000000000000000 ) ) ;
#82012 = CARTESIAN_POINT ( 'NONE',  ( -102.3130725222324173, -60.00000000000000000, 94.57084542267037364 ) ) ;
#82013 = CARTESIAN_POINT ( 'NONE',  ( 28.43952395724156190, 17.90362770311681828, -40.70652153699805353 ) ) ;
#82014 = CARTESIAN_POINT ( 'NONE',  ( -13.63130828375568981, 294.5445729804733901, -10.06530370901874250 ) ) ;
#82015 = CARTESIAN_POINT ( 'NONE',  ( -19.70764564238371719, 304.7954121406193622, 9.925013215726785631 ) ) ;
#82016 = DIRECTION ( 'NONE',  ( 0.000000000000000000, -1.000000000000000000, 0.000000000000000000 ) ) ;
#82018 = CARTESIAN_POINT ( 'NONE',  ( 30.00000000000000355, 490.2049413361779671, 6.956578744621319643 ) ) ;
#82017 = CARTESIAN_POINT ( 'NONE',  ( 2.617478844992707110, -5.000000000000015099, -94.73972676610841859 ) ) ;
#82019 = CARTESIAN_POINT ( 'NONE',  ( -85.33556072388859093, -25.38633735136824399, 170.5422650236019990 ) ) ;
#82020 = VECTOR ( 'NONE', #47218, 1000.000000000000227 ) ;
#82021 = EDGE_LOOP ( 'NONE', ( #87943, #60238, #51064, #103801, #70226, #56707 ) ) ;
#82022 = CARTESIAN_POINT ( 'NONE',  ( 7.500000000000005329, 9.833333333333344584, -68.91429205785459544 ) ) ;
#82023 = ORIENTED_EDGE ( 'NONE', *, *, #7059, .F. ) ;
#82024 = ORIENTED_EDGE ( 'NONE', *, *, #68947, .T. ) ;
#82025 = CARTESIAN_POINT ( 'NONE',  ( 30.00000000000000000, 0.000000000000000000, 0.000000000000000000 ) ) ;
#82026 = EDGE_CURVE ( 'NONE', #101726, #65472, #46744, .T. ) ;
#82028 = LINE ( 'NONE', #66389, #57714 ) ;
#82027 = CIRCLE ( 'NONE', #71717, 4.172000000000009479 ) ;
#82029 = ADVANCED_BREP_SHAPE_REPRESENTATION ( '', ( #87940, #10728 ), #26637 ) ;
#82030 = ORIENTED_EDGE ( 'NONE', *, *, #36601, .T. ) ;
#82031 = CARTESIAN_POINT ( 'NONE',  ( 2.019483917365790222E-25, 304.8518027762758038, 8.936999415352287812 ) ) ;
#82032 = DIRECTION ( 'NONE',  ( -1.000000000000000000, 0.000000000000000000, 0.000000000000000000 ) ) ;
#82033 = VECTOR ( 'NONE', #57698, 1000.000000000000000 ) ;
#82034 = CARTESIAN_POINT ( 'NONE',  ( 7.869432500659452323, 64.69453614009762532, -5.000000000000000888 ) ) ;
#82035 = DIRECTION ( 'NONE',  ( 0.000000000000000000, -1.000000000000000000, 0.000000000000000000 ) ) ;
#82036 = CARTESIAN_POINT ( 'NONE',  ( -3.311033882356798252E-14, 37.21016666119783167, -27.24999999999961986 ) ) ;
#82037 = CARTESIAN_POINT ( 'NONE',  ( 110.2448519957423940, -60.00000000000004974, 128.1456905595833575 ) ) ;
#82038 = CARTESIAN_POINT ( 'NONE',  ( -109.5128114756446109, -29.99999999999999289, 168.1048973186342437 ) ) ;
#82039 = CARTESIAN_POINT ( 'NONE',  ( -61.32847699634096017, -49.91700379991620906, 80.89165352633736461 ) ) ;
#82040 = VECTOR ( 'NONE', #9446, 1000.000000000000000 ) ;
#82041 = EDGE_LOOP ( 'NONE', ( #44671, #26574, #5752, #18839 ) ) ;
#82042 = CARTESIAN_POINT ( 'NONE',  ( 54.08561378075543047, 38.95410943244764468, 34.09344903348132050 ) ) ;
#82043 = CARTESIAN_POINT ( 'NONE',  ( 94.41996065847817476, -60.00000000002924594, 4.935578748710270247 ) ) ;
#82044 = CIRCLE ( 'NONE', #94084, 4.000000000000000888 ) ;
#82046 = VERTEX_POINT ( 'NONE', #54365 ) ;
#82045 = CONICAL_SURFACE ( 'NONE', #78589, 5.000000000000001776, 0.9599310885968803664 ) ;
#82047 = CARTESIAN_POINT ( 'NONE',  ( 3.789235738929097472E-05, -46.43475214916913529, 31.62877531779723839 ) ) ;
#82049 = AXIS2_PLACEMENT_3D ( 'NONE', #84715, #43195, #1099 ) ;
#82048 = CARTESIAN_POINT ( 'NONE',  ( 4.401442555609581635E-16, -11.65625000204838635, -7.188101187500000044 ) ) ;
#82050 = DIRECTION ( 'NONE',  ( 0.000000000000000000, 0.8813945903473795473, -0.4723807533191579089 ) ) ;
#82051 = EDGE_LOOP ( 'NONE', ( #32635, #29315, #87433, #71204 ) ) ;
#82052 = EDGE_CURVE ( 'NONE', #98139, #55300, #60552, .T. ) ;
#82053 = CARTESIAN_POINT ( 'NONE',  ( 73.59428447264397732, -1.232595164407830946E-29, 4.000000000000007105 ) ) ;
#82054 = EDGE_LOOP ( 'NONE', ( #76660, #37060, #9059, #63183 ) ) ;
#82055 = PRESENTATION_STYLE_ASSIGNMENT (( #33019 ) ) ;
#82057 = CIRCLE ( 'NONE', #35610, 4.000000000000001776 ) ;
#82056 = CARTESIAN_POINT ( 'NONE',  ( -109.8027852057873304, -60.00000000000000000, 141.6978195183435787 ) ) ;
#82058 = PRESENTATION_STYLE_ASSIGNMENT (( #50232 ) ) ;
#82059 = CARTESIAN_POINT ( 'NONE',  ( -1.320432766682874540E-15, -27.40625000204838813, 7.188101187500000044 ) ) ;
#82060 = CARTESIAN_POINT ( 'NONE',  ( 35.37498230280639433, 485.2520700389516151, -2.749549059028474129 ) ) ;
#82061 = VECTOR ( 'NONE', #35508, 1000.000000000000000 ) ;
#82062 = CARTESIAN_POINT ( 'NONE',  ( 16.64348903516512834, 43.75610143575153899, -4.157797401561768247 ) ) ;
#82063 = CARTESIAN_POINT ( 'NONE',  ( -3.462314351619998121, 19.87222038490562070, -6.085962419574315163 ) ) ;
#82064 = CARTESIAN_POINT ( 'NONE',  ( -11.08666809900981676, -4.983486105408843514, -12.57803232073183786 ) ) ;
#82065 = CARTESIAN_POINT ( 'NONE',  ( 51.01037695545453232, 450.0000000000002274, 13.20242257375370976 ) ) ;
#82066 = ADVANCED_FACE ( 'NONE', ( #13392 ), #26168, .T. ) ;
#82067 = CARTESIAN_POINT ( 'NONE',  ( -7.045965687440312486, 106.3039246378603480, 3.790395326974321133 ) ) ;
#82068 = CARTESIAN_POINT ( 'NONE',  ( -24.29723907929130178, 27.70462894893682204, 31.30642834101307770 ) ) ;
#82069 = CARTESIAN_POINT ( 'NONE',  ( 105.7114380630162032, -60.00000000000002132, 157.1102875351544981 ) ) ;
#82070 = CARTESIAN_POINT ( 'NONE',  ( -33.96339871129490007, -60.30850206294380200, 38.68848327799536690 ) ) ;
#82071 =( NAMED_UNIT ( * ) SI_UNIT ( $, .STERADIAN. ) SOLID_ANGLE_UNIT ( ) );
#82072 = CONICAL_SURFACE ( 'NONE', #56182, 3.309499999999999886, 0.7853981633974369547 ) ;
#82073 = CARTESIAN_POINT ( 'NONE',  ( 40.12088697054482367, -60.25518400732138957, 43.34133863879944926 ) ) ;
#82074 = ORIENTED_EDGE ( 'NONE', *, *, #404, .T. ) ;
#82075 = CARTESIAN_POINT ( 'NONE',  ( 43.69860345152648051, 434.4324800463855922, 11.31831452735614008 ) ) ;
#82076 = CARTESIAN_POINT ( 'NONE',  ( -76.85615192407949792, -38.44451095924269168, 183.6527095178624336 ) ) ;
#82077 = ORIENTED_EDGE ( 'NONE', *, *, #80906, .T. ) ;
#82078 = CARTESIAN_POINT ( 'NONE',  ( 2.499999999999999112, -9.944420556259451871, 19.25618705785077722 ) ) ;
#82079 = CARTESIAN_POINT ( 'NONE',  ( -10.17607823674123146, 16.00406820528922225, -10.18698793785925005 ) ) ;
#82081 = EDGE_CURVE ( 'NONE', #101431, #67639, #38763, .T. ) ;
#82080 = CARTESIAN_POINT ( 'NONE',  ( -49.19734730806123224, 7.744866885593231665, -16.05423930868188265 ) ) ;
#82082 = CARTESIAN_POINT ( 'NONE',  ( 6.222803527742078344, 4.089662073612393201, 6.499999999999997335 ) ) ;
#82083 = DIRECTION ( 'NONE',  ( 0.000000000000000000, 1.000000000000000000, 0.000000000000000000 ) ) ;
#82084 = CARTESIAN_POINT ( 'NONE',  ( -37.88754858252848834, 25.36997296304242511, 13.42524253834038284 ) ) ;
#82085 = CARTESIAN_POINT ( 'NONE',  ( 4.660674839411966808, -86.31782485304408681, -3.778981567323765223 ) ) ;
#82086 = CARTESIAN_POINT ( 'NONE',  ( 38.54515645702225868, 1.482358050883964840E-15, 0.000000000000000000 ) ) ;
#82087 = AXIS2_PLACEMENT_3D ( 'NONE', #9886, #17480, #91366 ) ;
#82088 = CARTESIAN_POINT ( 'NONE',  ( 110.9798546403277442, -60.00000000000000711, 151.9418731052118403 ) ) ;
#82089 = CARTESIAN_POINT ( 'NONE',  ( -1.257498747432114650, -53.98194347854916231, 40.94539907224319109 ) ) ;
#82090 = AXIS2_PLACEMENT_3D ( 'NONE', #85682, #77040, #44694 ) ;
#82091 = CARTESIAN_POINT ( 'NONE',  ( -6.928203230275509661, -65.00000000000000000, -4.000000000000002665 ) ) ;
#82092 = VERTEX_POINT ( 'NONE', #21533 ) ;
#82093 = CARTESIAN_POINT ( 'NONE',  ( -97.76776492929941753, -29.99999999999996447, 190.7297597677326166 ) ) ;
#82094 = EDGE_LOOP ( 'NONE', ( #85565, #55236, #13980, #78392, #11185, #72935, #19808, #79744 ) ) ;
#82095 = CARTESIAN_POINT ( 'NONE',  ( -3.375205455332774385, -49.11005739349737809, 104.1122683773797490 ) ) ;
#82096 = CARTESIAN_POINT ( 'NONE',  ( -15.91255636217404756, 3.418437750274899489, 2.532291868554421121 ) ) ;
#82097 = CARTESIAN_POINT ( 'NONE',  ( 4.259258436598990727, 140.4088661232431150, 5.000000000000000000 ) ) ;
#82098 = CARTESIAN_POINT ( 'NONE',  ( -19.99999999999999289, 4.000000000000000888, 25.00000000000000000 ) ) ;
#82099 = CARTESIAN_POINT ( 'NONE',  ( 9.645512969475850795, 26.98896849324273717, -2.645801731561390646 ) ) ;
#82100 = CARTESIAN_POINT ( 'NONE',  ( 4.401442555609581635E-16, -28.15625000204838813, -7.188101187500000044 ) ) ;
#82101 = CARTESIAN_POINT ( 'NONE',  ( 83.28888888888889142, 1.023464760207051730E-14, 0.000000000000000000 ) ) ;
#82102 = CARTESIAN_POINT ( 'NONE',  ( 7.418912130467639088, 41.12212895980070471, -69.28711560576921613 ) ) ;
#82103 = ORIENTED_EDGE ( 'NONE', *, *, #81130, .T. ) ;
#82104 = B_SPLINE_CURVE_WITH_KNOTS ( 'NONE', 3,
 ( #30155, #80257, #29641, #13930, #90357, #65553 ),
 .UNSPECIFIED., .F., .F.,
 ( 4, 2, 4 ),
 ( -4.698498716301610638E-06, 0.0003457374136928005972, 0.0006961733261019028771 ),
 .UNSPECIFIED. ) ;
#82106 = ORIENTED_EDGE ( 'NONE', *, *, #33785, .F. ) ;
#82105 = CARTESIAN_POINT ( 'NONE',  ( 4.999999999999993783, -4.000000000000003553, 102.2532056551910387 ) ) ;
#82107 = CARTESIAN_POINT ( 'NONE',  ( 79.39643088476593391, -56.84711113037113961, 163.2850302358858983 ) ) ;
#82108 = DIRECTION ( 'NONE',  ( 0.000000000000000000, 0.000000000000000000, 1.000000000000000000 ) ) ;
#82109 = AXIS2_PLACEMENT_3D ( 'NONE', #98430, #7816, #106516 ) ;
#82110 = ORIENTED_EDGE ( 'NONE', *, *, #7708, .F. ) ;
#82111 =( NAMED_UNIT ( * ) PLANE_ANGLE_UNIT ( ) SI_UNIT ( $, .RADIAN. ) );
#82112 = CARTESIAN_POINT ( 'NONE',  ( -14.37349357813612372, 2.004823033976885771, 4.269535008073903626 ) ) ;
#82113 = CARTESIAN_POINT ( 'NONE',  ( 5.082755093536325930, -11.46875000204838635, -5.082755093536325042 ) ) ;
#82114 = CARTESIAN_POINT ( 'NONE',  ( 6.943926999490791729, 29.46699007373851842, -3.973092371898545139 ) ) ;
#82115 = CARTESIAN_POINT ( 'NONE',  ( -16.34903003639686503, -60.00000000000001421, -36.33396904264586880 ) ) ;
#82116 = CARTESIAN_POINT ( 'NONE',  ( 11.53045486031959754, 45.53936973856496451, 13.95636496209353794 ) ) ;
#82117 = EDGE_CURVE ( 'NONE', #12173, #86477, #58301, .T. ) ;
#82118 = EDGE_LOOP ( 'NONE', ( #86026, #98173 ) ) ;
#82119 = FILL_AREA_STYLE_COLOUR ( '', #52305 ) ;
#82120 = VECTOR ( 'NONE', #28619, 999.9999999999998863 ) ;
#82121 = COLOUR_RGB ( '', 0.08235294, 0.09019608, 0.10196078) ;
#82122 = CARTESIAN_POINT ( 'NONE',  ( 11.84999999999999787, -3.309499999999999886, 0.000000000000000000 ) ) ;
#82123 = ADVANCED_FACE ( 'NONE', ( #364 ), #101873, .T. ) ;
#82124 = CARTESIAN_POINT ( 'NONE',  ( 7.493767109741696686, 40.39058573922605433, -59.41312748714017289 ) ) ;
#82125 = CARTESIAN_POINT ( 'NONE',  ( 8.099999999999999645, 4.898587196589413815E-16, -4.000000000000000888 ) ) ;
#82126 = CARTESIAN_POINT ( 'NONE',  ( 2.977408999572650927, -29.37500000204838457, -7.188101187500001821 ) ) ;
#82127 = AXIS2_PLACEMENT_3D ( 'NONE', #28292, #94053, #79454 ) ;
#82128 = CARTESIAN_POINT ( 'NONE',  ( 23.25461545940108721, -27.85505135366320317, 37.69763505033436957 ) ) ;
#82129 = VECTOR ( 'NONE', #39326, 1000.000000000000000 ) ;
#82130 = CARTESIAN_POINT ( 'NONE',  ( 9.926810856659656679, 15.46725112412266334, 1.404490565847983152 ) ) ;
#82131 = AXIS2_PLACEMENT_3D ( 'NONE', #46260, #103948, #79146 ) ;
#82132 = CARTESIAN_POINT ( 'NONE',  ( 2.449293598294707400E-16, 4.000000000000000000, 2.000000000000000888 ) ) ;
#82133 = CARTESIAN_POINT ( 'NONE',  ( 40.17576961386068746, 438.0154178803811647, 22.24081819228610613 ) ) ;
#82134 = SHAPE_DEFINITION_REPRESENTATION ( #51766, #63931 ) ;
#82135 = CARTESIAN_POINT ( 'NONE',  ( -9.918579450955565591, 33.79303912968686774, 1.297207292923860056 ) ) ;
#82136 = VERTEX_POINT ( 'NONE', #90484 ) ;
#82137 = AXIS2_PLACEMENT_3D ( 'NONE', #26259, #93614, #34340 ) ;
#82138 = CARTESIAN_POINT ( 'NONE',  ( -34.62919541716505023, 437.4394979580210361, 4.999019296795436773 ) ) ;
#82139 = VECTOR ( 'NONE', #75118, 1000.000000000000000 ) ;
#82140 = CARTESIAN_POINT ( 'NONE',  ( 13.85787468398986100, 43.09645778404858163, -91.44857208682125815 ) ) ;
#82141 = CARTESIAN_POINT ( 'NONE',  ( 41.50669491856072568, 1.482358050883964840E-15, 0.000000000000000000 ) ) ;
#82142 = CARTESIAN_POINT ( 'NONE',  ( 43.30868969682389036, -5.000000000000009770, 0.000000000000000000 ) ) ;
#82143 = EDGE_CURVE ( 'NONE', #93742, #68161, #10551, .T. ) ;
#82144 = B_SPLINE_CURVE_WITH_KNOTS ( 'NONE', 3,
 ( #91229, #25995, #34605, #92251, #66942, #58856 ),
 .UNSPECIFIED., .F., .F.,
 ( 4, 2, 4 ),
 ( 0.000000000000000000, 0.001990940508721421830, 0.003981881017442843659 ),
 .UNSPECIFIED. ) ;
#82145 = ORIENTED_EDGE ( 'NONE', *, *, #49824, .T. ) ;
#82146 = FACE_OUTER_BOUND ( 'NONE', #47982, .T. ) ;
#82147 = CARTESIAN_POINT ( 'NONE',  ( 113.8984031219851545, -57.67123714865640949, 180.8430928919092935 ) ) ;
#82148 = CARTESIAN_POINT ( 'NONE',  ( 35.22347075582237608, 464.3861918352842508, 19.05313339797742600 ) ) ;
#82149 = EDGE_CURVE ( 'NONE', #33365, #6815, #72603, .T. ) ;
#82150 = CARTESIAN_POINT ( 'NONE',  ( 4.000000000000000000, 17.85270131633358304, 5.744562646538042827 ) ) ;
#82151 = CARTESIAN_POINT ( 'NONE',  ( -1.448103213439668968, -5.000000000000000000, -72.00384268476057059 ) ) ;
#82152 = CARTESIAN_POINT ( 'NONE',  ( 36.62770931978901956, 26.04034622320522274, 11.37685887764211046 ) ) ;
#82153 = CARTESIAN_POINT ( 'NONE',  ( -80.26644129451693743, -59.99999999999999289, 196.3324352422349364 ) ) ;
#82154 = CARTESIAN_POINT ( 'NONE',  ( -27.18908553330205180, 296.5274986157688772, 10.30015177545897842 ) ) ;
#82155 = FILL_AREA_STYLE ('',( #106425 ) ) ;
#82156 = CARTESIAN_POINT ( 'NONE',  ( -40.85254446136673323, 441.7500193615117610, 25.53625856138344474 ) ) ;
#82157 = VECTOR ( 'NONE', #91763, 1000.000000000000000 ) ;
#82158 = CARTESIAN_POINT ( 'NONE',  ( -84.15525122082756582, -57.43313533274019989, 190.9243139192301442 ) ) ;
#82159 = ORIENTED_EDGE ( 'NONE', *, *, #25919, .T. ) ;
#82160 = CARTESIAN_POINT ( 'NONE',  ( 21.64331233096206475, 305.0431391404469537, -8.959384353494732167 ) ) ;
#82161 = ORIENTED_EDGE ( 'NONE', *, *, #88764, .T. ) ;
#82162 = CARTESIAN_POINT ( 'NONE',  ( -7.211357414135266097, -12.01146539934442359, 3.467230644691328578 ) ) ;
#82163 = ADVANCED_FACE ( 'NONE', ( #26333 ), #15708, .T. ) ;
#82164 = DIRECTION ( 'NONE',  ( -0.000000000000000000, -0.000000000000000000, -1.000000000000000000 ) ) ;
#82165 = CARTESIAN_POINT ( 'NONE',  ( -84.40018563635376836, -45.26636761344531124, -9.144727243375324832 ) ) ;
#82166 = CARTESIAN_POINT ( 'NONE',  ( -42.61140200160145497, 465.9030374194823594, 13.21253569360412783 ) ) ;
#82167 = PRESENTATION_STYLE_ASSIGNMENT (( #67993 ) ) ;
#82168 = ORIENTED_EDGE ( 'NONE', *, *, #73474, .T. ) ;
#82169 = CARTESIAN_POINT ( 'NONE',  ( 27.10511071441177222, 36.88665068479793518, -7.556984339679249985 ) ) ;
#82170 = CARTESIAN_POINT ( 'NONE',  ( 53.08934989192464826, -30.00000000000000000, 52.21148837440648549 ) ) ;
#82172 = CIRCLE ( 'NONE', #90817, 5.000000000000000000 ) ;
#82171 = CARTESIAN_POINT ( 'NONE',  ( -14.86825985028395181, -1.734723475976807094E-15, -8.569529079644194525 ) ) ;
#82173 = SURFACE_SIDE_STYLE ('',( #90818 ) ) ;
#82174 = CARTESIAN_POINT ( 'NONE',  ( -32.64482578944674884, -14.21045842199435150, -35.33261186109891128 ) ) ;
#82175 = CARTESIAN_POINT ( 'NONE',  ( -74.27483541950718404, -60.32442628959149999, 133.2375759543508025 ) ) ;
#82176 = ORIENTED_EDGE ( 'NONE', *, *, #10088, .F. ) ;
#82177 = CARTESIAN_POINT ( 'NONE',  ( 77.40131791002600892, -14.21045842199445630, 153.6837402093314324 ) ) ;
#82178 = CARTESIAN_POINT ( 'NONE',  ( 6.944031699373470978, 85.53460654556131715, 3.972913591453821613 ) ) ;
#82179 = CARTESIAN_POINT ( 'NONE',  ( 104.6107560558906471, -57.67118654542982625, 96.35458815996260284 ) ) ;
#82180 = ORIENTED_EDGE ( 'NONE', *, *, #8428, .T. ) ;
#82181 = CARTESIAN_POINT ( 'NONE',  ( 28.23128044651457458, 34.17513526713322847, 9.355917131510365081 ) ) ;
#82182 = AXIS2_PLACEMENT_3D ( 'NONE', #24736, #18238, #51094 ) ;
#82183 = CARTESIAN_POINT ( 'NONE',  ( 0.5805565836007654523, 7.505553499465140277, 2.211437577243512467E-16 ) ) ;
#82184 = ORIENTED_EDGE ( 'NONE', *, *, #51509, .F. ) ;
#82185 = CARTESIAN_POINT ( 'NONE',  ( 0.000000000000000000, 0.000000000000000000, 0.000000000000000000 ) ) ;
#82186 = DIRECTION ( 'NONE',  ( 0.000000000000000000, 0.000000000000000000, -1.000000000000000000 ) ) ;
#82187 = CARTESIAN_POINT ( 'NONE',  ( -7.188101187500000044, -19.90625000204838457, -8.802885111219163269E-16 ) ) ;
#82188 = CARTESIAN_POINT ( 'NONE',  ( 7.779103221381273414, -4.168986698926031131, -7.929128246061905472 ) ) ;
#82189 = FILL_AREA_STYLE ('',( #31562 ) ) ;
#82190 = SURFACE_SIDE_STYLE ('',( #81645 ) ) ;
#82191 = EDGE_CURVE ( 'NONE', #4872, #45384, #64017, .T. ) ;
#82192 = CARTESIAN_POINT ( 'NONE',  ( -17.89001738438791733, 45.34603189753767083, -5.216234635019829646 ) ) ;
#82193 =( NAMED_UNIT ( * ) PLANE_ANGLE_UNIT ( ) SI_UNIT ( $, .RADIAN. ) );
#82194 = VERTEX_POINT ( 'NONE', #99629 ) ;
#82195 = CARTESIAN_POINT ( 'NONE',  ( -7.204797958417223924, 41.05104878663154722, -70.50691237690513447 ) ) ;
#82196 = AXIS2_PLACEMENT_3D ( 'NONE', #29818, #77278, #69202 ) ;
#82198 = CARTESIAN_POINT ( 'NONE',  ( 29.96487401954387764, -56.85533909424443522, 36.18029637999577375 ) ) ;
#82197 = CARTESIAN_POINT ( 'NONE',  ( -4.003587701499910168, -48.94962346669722564, 104.5574048719304301 ) ) ;
#82199 = CARTESIAN_POINT ( 'NONE',  ( -4.206614587654213366, 51.73457005021325017, -7.924384222582498971 ) ) ;
#82200 = ORIENTED_EDGE ( 'NONE', *, *, #19424, .T. ) ;
#82201 = EDGE_CURVE ( 'NONE', #52915, #83314, #105342, .T. ) ;
#82202 = VERTEX_POINT ( 'NONE', #9018 ) ;
#82203 = MECHANICAL_DESIGN_GEOMETRIC_PRESENTATION_REPRESENTATION (  '', ( #77062 ), #23654 ) ;
#82205 = CARTESIAN_POINT ( 'NONE',  ( 0.3340480107103283580, 52.16129231206663519, 7.792553844401801655 ) ) ;
#82204 = DIRECTION ( 'NONE',  ( 0.000000000000000000, -1.000000000000000000, 0.000000000000000000 ) ) ;
#82206 = VECTOR ( 'NONE', #29412, 1000.000000000000000 ) ;
#82207 =( LENGTH_UNIT ( ) NAMED_UNIT ( * ) SI_UNIT ( .MILLI., .METRE. ) );
#82208 = FACE_OUTER_BOUND ( 'NONE', #81065, .T. ) ;
#82209 = AXIS2_PLACEMENT_3D ( 'NONE', #1631, #25437, #65327 ) ;
#82210 =( GEOMETRIC_REPRESENTATION_CONTEXT ( 3 ) GLOBAL_UNCERTAINTY_ASSIGNED_CONTEXT ( ( #72004 ) ) GLOBAL_UNIT_ASSIGNED_CONTEXT ( ( #64316, #87528, #12550 ) ) REPRESENTATION_CONTEXT ( 'NONE', 'WORKASPACE' ) );
#82211 = CARTESIAN_POINT ( 'NONE',  ( 8.559508646656350805, 53.68473964988125857, -4.031152949374623873 ) ) ;
#82212 = CARTESIAN_POINT ( 'NONE',  ( 98.31310517497099966, 1.030564683017419500E-14, 0.000000000000000000 ) ) ;
#82213 = CARTESIAN_POINT ( 'NONE',  ( -37.43130592801911405, 464.0780360861290319, 19.48660943767402998 ) ) ;
#82214 = ORIENTED_EDGE ( 'NONE', *, *, #987, .F. ) ;
#82215 = CARTESIAN_POINT ( 'NONE',  ( 92.56707009034266775, -60.00000000000000000, -10.65961130115607247 ) ) ;
#82216 = B_SPLINE_CURVE_WITH_KNOTS ( 'NONE', 3,
 ( #65728, #99680, #25851, #47924, #98607, #25296, #80831, #31779 ),
 .UNSPECIFIED., .F., .F.,
 ( 4, 2, 2, 4 ),
 ( 2.459764730722484167E-07, 0.001920659145285706550, 0.002880865729692022332, 0.003841072314098338547 ),
 .UNSPECIFIED. ) ;
#82217 = DIRECTION ( 'NONE',  ( -0.000000000000000000, 1.000000000000000000, -0.000000000000000000 ) ) ;
#82219 = ADVANCED_FACE ( 'NONE', ( #58659 ), #83446, .F. ) ;
#82218 = CARTESIAN_POINT ( 'NONE',  ( 32.03945371335148451, 464.8492019110282740, 12.52442169461163246 ) ) ;
#82220 = MECHANICAL_DESIGN_GEOMETRIC_PRESENTATION_REPRESENTATION (  '', ( #13301 ), #96018 ) ;
#82221 = CARTESIAN_POINT ( 'NONE',  ( -11.69538631874851653, -5.000000000000000000, -88.12269504201408665 ) ) ;
#82222 = DIRECTION ( 'NONE',  ( -0.000000000000000000, 0.000000000000000000, -1.000000000000000000 ) ) ;
#82223 = VERTEX_POINT ( 'NONE', #75890 ) ;
#82224 = CARTESIAN_POINT ( 'NONE',  ( 17.50000000000002842, 45.00000000000000711, 100.0000000000000000 ) ) ;
#82225 = EDGE_LOOP ( 'NONE', ( #11662, #26740, #46905, #2412 ) ) ;
#82226 = EDGE_LOOP ( 'NONE', ( #72854, #62259, #42995, #31719 ) ) ;
#82227 = CARTESIAN_POINT ( 'NONE',  ( -8.559508646656370345, 53.68473964988125857, -4.031152949374577688 ) ) ;
#82228 = CARTESIAN_POINT ( 'NONE',  ( 46.50260525563992076, 39.63181832368864832, -46.56948742080178505 ) ) ;
#82229 = DIRECTION ( 'NONE',  ( -1.000000000000000000, -1.224606353822377258E-16, -0.000000000000000000 ) ) ;
#82230 = CARTESIAN_POINT ( 'NONE',  ( -36.06456757113840439, 330.6367415789401321, -3.201966090863014536 ) ) ;
#82231 = CARTESIAN_POINT ( 'NONE',  ( -3.379087390341638741, -69.90378107111884276, 13.41250649815817830 ) ) ;
#82232 = CARTESIAN_POINT ( 'NONE',  ( 2.323340773569810391, -49.78385856118777752, 102.3935653434436830 ) ) ;
#82233 = CARTESIAN_POINT ( 'NONE',  ( 12.50000000000000355, 27.22490228149561631, -44.76726718883759304 ) ) ;
#82234 = ORIENTED_EDGE ( 'NONE', *, *, #62129, .F. ) ;
#82235 = LINE ( 'NONE', #16994, #99392 ) ;
#82236 = ORIENTED_EDGE ( 'NONE', *, *, #22220, .T. ) ;
#82237 = CIRCLE ( 'NONE', #102879, 18.07003550757956845 ) ;
#82238 = CARTESIAN_POINT ( 'NONE',  ( -7.500000000000003553, -2.999999999998154365, -69.80246343544763477 ) ) ;
#82239 =( LENGTH_UNIT ( ) NAMED_UNIT ( * ) SI_UNIT ( .MILLI., .METRE. ) );
#82240 = CARTESIAN_POINT ( 'NONE',  ( 3.963177594442894858, -48.71124122727862016, 103.9032426698779403 ) ) ;
#82241 = CIRCLE ( 'NONE', #16807, 0.9999999999999984457 ) ;
#82243 = ORIENTED_EDGE ( 'NONE', *, *, #5400, .F. ) ;
#82242 = CARTESIAN_POINT ( 'NONE',  ( -58.93042220256725017, -59.99999999999997158, 79.07426381573431229 ) ) ;
#82244 = CARTESIAN_POINT ( 'NONE',  ( 65.12589038046561996, -53.38532643392667865, 93.95558868601008840 ) ) ;
#82245 = ORIENTED_EDGE ( 'NONE', *, *, #69001, .F. ) ;
#82246 = CARTESIAN_POINT ( 'NONE',  ( 17.50000000000003553, 48.75234879777378438, 64.07562946667630399 ) ) ;
#82247 = CARTESIAN_POINT ( 'NONE',  ( 0.9654893961777153422, -30.00000000000000355, 7.122964895856731538 ) ) ;
#82248 = CARTESIAN_POINT ( 'NONE',  ( -94.73097995338159194, -57.65973493957909568, -7.453110678737913553 ) ) ;
#82249 = ADVANCED_FACE ( 'NONE', ( #77499 ), #78545, .T. ) ;
#82250 = B_SPLINE_CURVE_WITH_KNOTS ( 'NONE', 3,
 ( #57757, #22787, #31415, #65870, #30883, #98749, #105791, #14641 ),
 .UNSPECIFIED., .F., .F.,
 ( 4, 2, 2, 4 ),
 ( 0.004673709593152167857, 0.005837709341827654677, 0.007001709090503141497, 0.009329708587854115137 ),
 .UNSPECIFIED. ) ;
#82251 = ORIENTED_EDGE ( 'NONE', *, *, #88667, .T. ) ;
#82252 =( NAMED_UNIT ( * ) PLANE_ANGLE_UNIT ( ) SI_UNIT ( $, .RADIAN. ) );
#82253 = LINE ( 'NONE', #239, #59249 ) ;
#82254 = EDGE_CURVE ( 'NONE', #74863, #100726, #76000, .T. ) ;
#82255 = AXIS2_PLACEMENT_3D ( 'NONE', #93894, #21624, #28661 ) ;
#82256 = CARTESIAN_POINT ( 'NONE',  ( 6.047133232705633965, 51.82847809756811586, -6.273795380418080825 ) ) ;
#82257 = CARTESIAN_POINT ( 'NONE',  ( -4.852941176470586093, 40.00000000000132871, -70.80672828634229177 ) ) ;
#82258 = CARTESIAN_POINT ( 'NONE',  ( 8.000000000000000000, -23.18750000409677270, 0.000000000000000000 ) ) ;
#82259 = CARTESIAN_POINT ( 'NONE',  ( 0.4037800551813748862, 7.199367570657604354, 0.5303295852573147728 ) ) ;
#82260 = DIRECTION ( 'NONE',  ( -0.5735764363510494901, -0.8191520442889894671, 0.000000000000000000 ) ) ;
#82261 = CARTESIAN_POINT ( 'NONE',  ( 23.09999999999999432, 1.533819458162526451E-15, 0.000000000000000000 ) ) ;
#82262 = AXIS2_PLACEMENT_3D ( 'NONE', #4677, #6236, #71509 ) ;
#82263 = CARTESIAN_POINT ( 'NONE',  ( -5.904546178069103313, 4.631679053609773611, 5.000000000000000000 ) ) ;
#82264 = CARTESIAN_POINT ( 'NONE',  ( 0.000000000000000000, 294.8518027762758038, 9.936999415352289589 ) ) ;
#82265 = DIRECTION ( 'NONE',  ( 0.000000000000000000, 0.000000000000000000, 1.000000000000000000 ) ) ;
#82266 = ORIENTED_EDGE ( 'NONE', *, *, #71268, .T. ) ;
#82267 = CARTESIAN_POINT ( 'NONE',  ( -30.00000000000000000, 0.000000000000000000, 0.000000000000000000 ) ) ;
#82268 = CARTESIAN_POINT ( 'NONE',  ( 85.31310517497098544, 5.000000000000020428, 0.000000000000000000 ) ) ;
#82269 = CARTESIAN_POINT ( 'NONE',  ( -5.000000000000000000, -42.29207564866745628, 4.347359059871835463 ) ) ;
#82270 = CARTESIAN_POINT ( 'NONE',  ( -98.14828879091820113, -30.00000000000000355, 190.3627818008955899 ) ) ;
#82271 = EDGE_CURVE ( 'NONE', #17374, #44553, #11675, .T. ) ;
#82272 = MECHANICAL_DESIGN_GEOMETRIC_PRESENTATION_REPRESENTATION (  '', ( #73641 ), #9904 ) ;
#82273 = CARTESIAN_POINT ( 'NONE',  ( -39.80234998357077103, 485.2146942042872979, -4.378040023498154021 ) ) ;
#82274 = PRESENTATION_LAYER_ASSIGNMENT (  '', '', ( #46115 ) ) ;
#82275 = CARTESIAN_POINT ( 'NONE',  ( 69.01947847511793555, -57.68200961577189645, 147.4487533431950226 ) ) ;
#82277 = CARTESIAN_POINT ( 'NONE',  ( -9.540057778879830863, 53.58151691157907948, 1.989242606643393474 ) ) ;
#82276 = LINE ( 'NONE', #64520, #3582 ) ;
#82278 = ADVANCED_FACE ( 'NONE', ( #51610 ), #101763, .T. ) ;
#82279 = CARTESIAN_POINT ( 'NONE',  ( 5.739522349644341048, -21.75746304180372093, -38.54665207307362351 ) ) ;
#82280 = CARTESIAN_POINT ( 'NONE',  ( 1.083333333333333259, -6.880090707843076636, -5.848636054922048189 ) ) ;
#82281 = CARTESIAN_POINT ( 'NONE',  ( -46.00000000000000000, 436.0345727778312721, 16.01583062807923596 ) ) ;
#82282 = CARTESIAN_POINT ( 'NONE',  ( -8.461568262860977185, -59.99999999999998579, 39.63601601260060647 ) ) ;
#82283 = CIRCLE ( 'NONE', #77134, 4.000000000000007105 ) ;
#82284 = VECTOR ( 'NONE', #78537, 1000.000000000000000 ) ;
#82285 = CARTESIAN_POINT ( 'NONE',  ( 12.25865980111967701, 17.70980365415343627, 8.828502505339814732 ) ) ;
#82286 = CARTESIAN_POINT ( 'NONE',  ( 35.53321744913674252, 463.4104023594617843, 19.92304894059051890 ) ) ;
#82287 = CARTESIAN_POINT ( 'NONE',  ( -86.21016422779933919, -53.80605556536726652, 192.1622240966613049 ) ) ;
#82288 = EDGE_LOOP ( 'NONE', ( #41192, #51040, #58362, #59897, #17222 ) ) ;
#82289 = FACE_OUTER_BOUND ( 'NONE', #49074, .T. ) ;
#82290 = CARTESIAN_POINT ( 'NONE',  ( 9.098035229686777470, -13.55677388152806806, 16.35626862400982517 ) ) ;
#82291 = CARTESIAN_POINT ( 'NONE',  ( -8.197116350937552198, -42.95771439283771542, 31.04260219330700465 ) ) ;
#82292 =( BOUNDED_SURFACE ( )  B_SPLINE_SURFACE ( 3, 2, ( 
 ( #36432, #52026, #60682 ),
 ( #102176, #61748, #69302 ),
 ( #2943, #93025, #11026 ),
 ( #19187, #53624, #84937 ) ),
 .UNSPECIFIED., .F., .F., .F. ) 
 B_SPLINE_SURFACE_WITH_KNOTS ( ( 4, 4 ),
 ( 3, 3 ),
 ( -3.903127820947815962E-18, 0.0007499009164755671619 ),
 ( 0.000000000000000000, 1.000000000000000000 ),
 .UNSPECIFIED. ) 
 GEOMETRIC_REPRESENTATION_ITEM ( )  RATIONAL_B_SPLINE_SURFACE ( (
 ( 1.000000000000000000, 0.7301269460247310494, 1.000000000000000000),
 ( 1.000000000000000000, 0.7327382575064720349, 1.000000000000000000),
 ( 1.000000000000000000, 0.7350727526496287911, 1.000000000000000000),
 ( 1.000000000000000000, 0.7370557512816016121, 1.000000000000000000) ) ) 
 REPRESENTATION_ITEM ( '' )  SURFACE ( )  );
#82293 = DIRECTION ( 'NONE',  ( 0.000000000000000000, 0.000000000000000000, 1.000000000000000000 ) ) ;
#82294 = STYLED_ITEM ( 'NONE', ( #2479 ), #9074 ) ;
#82296 = CARTESIAN_POINT ( 'NONE',  ( 1.364254058415848236, -70.64897445287397204, 13.05800878275180033 ) ) ;
#82295 = CARTESIAN_POINT ( 'NONE',  ( -98.59376555388014651, -59.99999999999996447, 196.3422130118438531 ) ) ;
#82297 = ORIENTED_EDGE ( 'NONE', *, *, #60113, .T. ) ;
#82298 = FILL_AREA_STYLE ('',( #49389 ) ) ;
#82299 = AXIS2_PLACEMENT_3D ( 'NONE', #100853, #43161, #76043 ) ;
#82300 = CARTESIAN_POINT ( 'NONE',  ( -7.579218993349681632, -4.999999999985669241, -17.00320663868540905 ) ) ;
#82301 = CARTESIAN_POINT ( 'NONE',  ( 16.75187969033571989, 34.99134772383131065, 21.80698433968582961 ) ) ;
#82302 = CARTESIAN_POINT ( 'NONE',  ( 30.12025201962617160, 308.0360787568225760, -8.818471063241863916 ) ) ;
#82303 = DIRECTION ( 'NONE',  ( -1.000000000000000000, -0.000000000000000000, -0.000000000000000000 ) ) ;
#82304 = CARTESIAN_POINT ( 'NONE',  ( -7.150931910075641440, -83.21374201477736676, -3.588457848165358843 ) ) ;
#82305 = DIRECTION ( 'NONE',  ( -1.000000000000000000, -1.224606353822377258E-16, -0.000000000000000000 ) ) ;
#82306 = PRESENTATION_LAYER_ASSIGNMENT (  '', '', ( #54739 ) ) ;
#82307 = CARTESIAN_POINT ( 'NONE',  ( 112.0515757376121542, -60.00000000000002842, 140.8507904390172598 ) ) ;
#82308 = CARTESIAN_POINT ( 'NONE',  ( -24.80105969489321893, 306.0237540681346218, -9.745911707962003234 ) ) ;
#82309 = EDGE_LOOP ( 'NONE', ( #2049, #62077, #6459, #101856, #51554, #22383 ) ) ;
#82310 = CARTESIAN_POINT ( 'NONE',  ( -3.030991683532509029, -29.99999999999999645, 6.776004774809743836 ) ) ;
#82311 = CARTESIAN_POINT ( 'NONE',  ( 0.7145311798163195283, -4.618802153516994302, 8.000000000000000000 ) ) ;
#82312 = DIRECTION ( 'NONE',  ( -0.5356766697699745228, 0.1574227122301985193, -0.8296195484306273515 ) ) ;
#82313 = CARTESIAN_POINT ( 'NONE',  ( 5.683639242321874896, -2.934261738049317003, 103.9372442403038264 ) ) ;
#82314 = CARTESIAN_POINT ( 'NONE',  ( 3.641358249959525395, 22.19731953646417466, -4.999999999999999112 ) ) ;
#82315 = CARTESIAN_POINT ( 'NONE',  ( 8.559508646656407649, -1.200000000000000030E-05, 1.531152949374444239 ) ) ;
#82316 = EDGE_LOOP ( 'NONE', ( #81523, #14420, #3995, #60947 ) ) ;
#82317 = CARTESIAN_POINT ( 'NONE',  ( -20.43433360646712416, 304.8965913596235850, 8.946491893676210339 ) ) ;
#82318 = ORIENTED_EDGE ( 'NONE', *, *, #101224, .T. ) ;
#82319 = CARTESIAN_POINT ( 'NONE',  ( 34.63713372481439023, 485.1220453274884221, -1.973566398568655123 ) ) ;
#82320 =( BOUNDED_CURVE ( )  B_SPLINE_CURVE ( 2, ( #103848, #14827, #29994 ),
 .UNSPECIFIED., .F., .F. ) 
 B_SPLINE_CURVE_WITH_KNOTS ( ( 3, 3 ),
 ( 0.000000000000000000, 1.000000000000000000 ),
 .UNSPECIFIED. ) 
 CURVE ( )  GEOMETRIC_REPRESENTATION_ITEM ( )  RATIONAL_B_SPLINE_CURVE ( ( 1.000000000000000000, 1.857142857142858317, 1.000000000000000000 ) ) 
 REPRESENTATION_ITEM ( '' )  );
#82321 = CARTESIAN_POINT ( 'NONE',  ( 32.04854177564008211, 486.3112398708905175, 5.779390795271076797 ) ) ;
#82322 = VERTEX_POINT ( 'NONE', #61327 ) ;
#82323 = EDGE_CURVE ( 'NONE', #93278, #30721, #39901, .T. ) ;
#82324 = CARTESIAN_POINT ( 'NONE',  ( 64.32759900504497352, 48.00000000000000000, -11.06576400629120549 ) ) ;
#82325 = CARTESIAN_POINT ( 'NONE',  ( 5.000000000000000000, -14.98862091075390701, 12.50620160667418368 ) ) ;
#82326 = CARTESIAN_POINT ( 'NONE',  ( -30.56258723643923503, -59.99999999998762945, 46.02415584283473038 ) ) ;
#82328 = CARTESIAN_POINT ( 'NONE',  ( 46.00000000000000000, 435.9962990437406916, 13.93498389398033410 ) ) ;
#82327 = CIRCLE ( 'NONE', #35884, 3.500000000000000000 ) ;
#82329 = ORIENTED_EDGE ( 'NONE', *, *, #59656, .T. ) ;
#82330 = CARTESIAN_POINT ( 'NONE',  ( 95.88519897241275203, -60.00000000000002842, 202.5558118362681626 ) ) ;
#82332 = CARTESIAN_POINT ( 'NONE',  ( 13.32414351401617303, -29.02978351584501837, 28.80459947957771760 ) ) ;
#82331 = CARTESIAN_POINT ( 'NONE',  ( -108.4361608695136994, -30.00000000000004974, 186.7333242197273080 ) ) ;
#82333 = EDGE_CURVE ( 'NONE', #54238, #33159, #64097, .T. ) ;
#82335 = SURFACE_STYLE_USAGE ( .BOTH. , #49429 ) ;
#82334 = PRODUCT_DEFINITION_CONTEXT ( 'detailed design', #87919, 'design' ) ;
#82336 =( NAMED_UNIT ( * ) PLANE_ANGLE_UNIT ( ) SI_UNIT ( $, .RADIAN. ) );
#82337 = AXIS2_PLACEMENT_3D ( 'NONE', #19801, #94728, #93653 ) ;
#82338 = EDGE_CURVE ( 'NONE', #105711, #105140, #98466, .T. ) ;
#82339 = CARTESIAN_POINT ( 'NONE',  ( -43.48272077847599348, -56.80150791866010707, 46.32055055518623732 ) ) ;
#82340 = CARTESIAN_POINT ( 'NONE',  ( -0.1696942726969380422, 35.07848972003357346, -27.25872117772604852 ) ) ;
#82341 = EDGE_LOOP ( 'NONE', ( #7619, #17753 ) ) ;
#82342 = DIRECTION ( 'NONE',  ( 0.000000000000000000, -1.000000000000000000, 0.000000000000000000 ) ) ;
#82343 = DIRECTION ( 'NONE',  ( 0.000000000000000000, -1.000000000000000000, 0.000000000000000000 ) ) ;
#82344 = CARTESIAN_POINT ( 'NONE',  ( 40.88293604215247967, 432.5779639752643675, 26.56799667982232549 ) ) ;
#82345 = DIRECTION ( 'NONE',  ( 0.000000000000000000, -1.000000000000000000, 0.000000000000000000 ) ) ;
#82346 = CARTESIAN_POINT ( 'NONE',  ( 13.56846521071778255, 303.5479320962715519, -10.06459103807807587 ) ) ;
#82347 = CARTESIAN_POINT ( 'NONE',  ( -30.00000000000558487, 487.3958844382141251, 6.449680606608591660 ) ) ;
#82348 = ORIENTED_EDGE ( 'NONE', *, *, #86828, .T. ) ;
#82349 = CARTESIAN_POINT ( 'NONE',  ( 4.581218816254647663, -47.80086643547572578, 103.5404609598622443 ) ) ;
#82350 = CIRCLE ( 'NONE', #96138, 5.000000000000002665 ) ;
#82351 = ORIENTED_EDGE ( 'NONE', *, *, #24161, .F. ) ;
#82352 = CARTESIAN_POINT ( 'NONE',  ( 79.65125166320837025, -30.00000000000000000, -14.25942181426082556 ) ) ;
#82353 = DIRECTION ( 'NONE',  ( 0.000000000000000000, -0.9676758637755515924, 0.2521971900442986914 ) ) ;
#82355 = EDGE_CURVE ( 'NONE', #68317, #36313, #19315, .T. ) ;
#82354 = CARTESIAN_POINT ( 'NONE',  ( 6.750000000000016875, -11.69134295108991495, 0.000000000000000000 ) ) ;
#82356 = DIRECTION ( 'NONE',  ( 0.000000000000000000, -1.000000000000000000, 0.000000000000000000 ) ) ;
#82357 = CARTESIAN_POINT ( 'NONE',  ( 90.43235478266818461, -29.99999999999999645, 91.02177936252034840 ) ) ;
#82358 = CARTESIAN_POINT ( 'NONE',  ( 22.33349330513380693, -3.851859888774471706E-31, 4.000000000000001776 ) ) ;
#82359 = VERTEX_POINT ( 'NONE', #45145 ) ;
#82360 = EDGE_LOOP ( 'NONE', ( #36580, #41611, #91845, #16100, #5478, #98411 ) ) ;
#82361 = ORIENTED_EDGE ( 'NONE', *, *, #57418, .T. ) ;
#82362 = STYLED_ITEM ( 'NONE', ( #12928 ), #26717 ) ;
#82363 = CARTESIAN_POINT ( 'NONE',  ( 33.21102376836596193, 438.9613914113129454, 23.92328486949907784 ) ) ;
#82364 = CARTESIAN_POINT ( 'NONE',  ( -6.619572829881549936, 41.38254192478331106, -70.73105035172459054 ) ) ;
#82365 = CIRCLE ( 'NONE', #13435, 1.000000000000014433 ) ;
#82366 = FILL_AREA_STYLE_COLOUR ( '', #20409 ) ;
#82367 = CARTESIAN_POINT ( 'NONE',  ( -30.24422310998454577, 336.7236929599040991, 17.61079458025261602 ) ) ;
#82368 = ORIENTED_EDGE ( 'NONE', *, *, #96960, .T. ) ;
#82369 = CARTESIAN_POINT ( 'NONE',  ( 9.537291425704607306, 107.6440437733276951, 3.012810007366001130 ) ) ;
#82370 = ORIENTED_EDGE ( 'NONE', *, *, #29911, .T. ) ;
#82371 = DIRECTION ( 'NONE',  ( -1.000000000000000000, -1.224606353822377258E-16, -0.000000000000000000 ) ) ;
#82372 = CARTESIAN_POINT ( 'NONE',  ( 79.35189136647100838, -38.72593919592400624, 191.7211272454419202 ) ) ;
#82373 = CARTESIAN_POINT ( 'NONE',  ( 32.65560599211094939, 434.9894379982545729, 13.53857720042920043 ) ) ;
#82374 = CARTESIAN_POINT ( 'NONE',  ( 34.18266571248467045, 303.5689682991300060, 11.95674675998675518 ) ) ;
#82375 = DIRECTION ( 'NONE',  ( 0.000000000000000000, 0.000000000000000000, 1.000000000000000000 ) ) ;
#82376 = CYLINDRICAL_SURFACE ( 'NONE', #49307, 4.000000000000000000 ) ;
#82377 = CARTESIAN_POINT ( 'NONE',  ( 0.000000000000000000, 0.000000000000000000, 0.000000000000000000 ) ) ;
#82378 = DIRECTION ( 'NONE',  ( 0.000000000000000000, -1.000000000000000000, 0.000000000000000000 ) ) ;
#82379 = DIRECTION ( 'NONE',  ( -1.000000000000000000, -1.224606353822377258E-16, -0.000000000000000000 ) ) ;
#82380 = EDGE_CURVE ( 'NONE', #57615, #99036, #93086, .T. ) ;
#82381 = B_SPLINE_CURVE_WITH_KNOTS ( 'NONE', 3,
 ( #98393, #57392, #75167, #90304, #8845, #1260, #99439, #34227 ),
 .UNSPECIFIED., .F., .F.,
 ( 4, 2, 2, 4 ),
 ( 0.000000000000000000, 0.001046156454241313960, 0.002092312908482627919, 0.004184625816965175174 ),
 .UNSPECIFIED. ) ;
#82382 = DIRECTION ( 'NONE',  ( -0.000000000000000000, 1.000000000000000000, -0.000000000000000000 ) ) ;
#82383 = ORIENTED_EDGE ( 'NONE', *, *, #46901, .F. ) ;
#82384 = VECTOR ( 'NONE', #925, 1000.000000000000000 ) ;
#82385 = CARTESIAN_POINT ( 'NONE',  ( -24.57118404873822826, 295.6022528646752221, 10.09816379703451616 ) ) ;
#82386 = CARTESIAN_POINT ( 'NONE',  ( 7.370082443888056112, 54.30877847509226086, -2.387610232865688520 ) ) ;
#82387 = CARTESIAN_POINT ( 'NONE',  ( -13.88435755502521474, 42.00000000000000000, -90.88030988970933777 ) ) ;
#82388 = CARTESIAN_POINT ( 'NONE',  ( -5.656854249492379694, -10.43749999999999112, -5.656854249492380582 ) ) ;
#82389 = CARTESIAN_POINT ( 'NONE',  ( 35.12853135170308860, -35.58808086419043093, 44.33031536753241397 ) ) ;
#82390 = ADVANCED_FACE ( 'NONE', ( #60278 ), #62396, .T. ) ;
#82391 = EDGE_CURVE ( 'NONE', #99054, #74596, #8925, .T. ) ;
#82392 = CARTESIAN_POINT ( 'NONE',  ( 9.150944205135592924, 294.9553539103914659, 4.044928260314501145 ) ) ;
#82393 = VECTOR ( 'NONE', #83335, 1000.000000000000000 ) ;
#82394 = FACE_OUTER_BOUND ( 'NONE', #53408, .T. ) ;
#82395 = APPLICATION_CONTEXT ( 'automotive_design' ) ;
#82396 = CARTESIAN_POINT ( 'NONE',  ( 84.47753516669979490, -57.45055748378986493, 191.4165636158805057 ) ) ;
#82398 = EDGE_CURVE ( 'NONE', #74466, #10334, #50644, .T. ) ;
#82397 = CIRCLE ( 'NONE', #4875, 4.000000000000001776 ) ;
#82399 = CARTESIAN_POINT ( 'NONE',  ( 21.36650669486618881, 4.898587196589413815E-16, -4.000000000000000888 ) ) ;
#82400 = CARTESIAN_POINT ( 'NONE',  ( 1.288479777019286333E-15, 37.86482112153536406, 10.52123582012688274 ) ) ;
#82401 = VERTEX_POINT ( 'NONE', #64882 ) ;
#82402 = CARTESIAN_POINT ( 'NONE',  ( 94.71006489888094393, -57.65966216332807903, -7.938468930687816005 ) ) ;
#82403 = DIRECTION ( 'NONE',  ( -0.8191520442889884679, 1.003171929053520679E-16, 0.5735764363510508224 ) ) ;
#82404 =( NAMED_UNIT ( * ) PLANE_ANGLE_UNIT ( ) SI_UNIT ( $, .RADIAN. ) );
#82405 = CARTESIAN_POINT ( 'NONE',  ( 29.35352825446852165, 8.824359840618530626, 42.06917583815489081 ) ) ;
#82406 = EDGE_CURVE ( 'NONE', #58206, #91320, #96801, .T. ) ;
#82407 = CARTESIAN_POINT ( 'NONE',  ( -81.39487957031619203, -30.00000000000000355, -10.09601113538941597 ) ) ;
#82408 = EDGE_CURVE ( 'NONE', #64296, #67545, #33075, .T. ) ;
#82409 = PRESENTATION_LAYER_ASSIGNMENT (  '', '', ( #4893 ) ) ;
#82410 = CARTESIAN_POINT ( 'NONE',  ( 28.88579667808768647, 18.87341229088494643, 39.88979553324821836 ) ) ;
#82411 = DIRECTION ( 'NONE',  ( 1.000000000000000000, 0.000000000000000000, -0.000000000000000000 ) ) ;
#82412 = AXIS2_PLACEMENT_3D ( 'NONE', #22962, #54753, #72540 ) ;
#82414 = CARTESIAN_POINT ( 'NONE',  ( 0.000000000000000000, 0.000000000000000000, -1.971869939371574620 ) ) ;
#82413 = CARTESIAN_POINT ( 'NONE',  ( 4.147911490760948894, -48.94936983711307477, 104.5115833471886191 ) ) ;
#82415 = EDGE_CURVE ( 'NONE', #101117, #67401, #31491, .T. ) ;
#82416 = CARTESIAN_POINT ( 'NONE',  ( -48.02835407290534420, -1.200000000000000030E-05, -15.60535821593460248 ) ) ;
#82417 = CARTESIAN_POINT ( 'NONE',  ( -28.52991250593621331, 16.51520549712914132, 41.35291476382062115 ) ) ;
#82418 = SURFACE_SIDE_STYLE ('',( #41951 ) ) ;
#82419 = CARTESIAN_POINT ( 'NONE',  ( 24.63846153846153797, 4.172000000000003261, 0.000000000000000000 ) ) ;
#82420 = CARTESIAN_POINT ( 'NONE',  ( 0.000000000000000000, 0.000000000000000000, -10.00000000000000000 ) ) ;
#82421 = AXIS2_PLACEMENT_3D ( 'NONE', #19377, #20970, #85121 ) ;
#82422 = ADVANCED_FACE ( 'NONE', ( #57302 ), #74029, .F. ) ;
#82423 = FACE_OUTER_BOUND ( 'NONE', #50623, .T. ) ;
#82424 = AXIS2_PLACEMENT_3D ( 'NONE', #82683, #41695, #98337 ) ;
#82425 = B_SPLINE_CURVE_WITH_KNOTS ( 'NONE', 3,
 ( #28700, #86914, #27643, #44316, #103088, #77210, #3322, #21144, #11932, #54496 ),
 .UNSPECIFIED., .F., .F.,
 ( 4, 2, 2, 2, 4 ),
 ( 0.000000000000000000, 0.001057229007211967810, 0.002114458014423935620, 0.003171687021635903429, 0.004228916028847871239 ),
 .UNSPECIFIED. ) ;
#82426 = ORIENTED_EDGE ( 'NONE', *, *, #26185, .F. ) ;
#82427 = CARTESIAN_POINT ( 'NONE',  ( -6.633460018062062424, 3.141069750844269759, 14.66750529547399218 ) ) ;
#82428 = CARTESIAN_POINT ( 'NONE',  ( 4.010857135589731489E-16, 21.85270131633359014, 7.000000000000016875 ) ) ;
#82429 = CYLINDRICAL_SURFACE ( 'NONE', #78595, 4.000000000000000000 ) ;
#82431 = DIRECTION ( 'NONE',  ( -1.000000000000000000, -1.224606353822377258E-16, -0.000000000000000000 ) ) ;
#82430 = CARTESIAN_POINT ( 'NONE',  ( 5.290067270632322405, -1.200000000000000030E-05, 6.031152949374479100 ) ) ;
#82432 = VERTEX_POINT ( 'NONE', #40078 ) ;
#82433 =( NAMED_UNIT ( * ) PLANE_ANGLE_UNIT ( ) SI_UNIT ( $, .RADIAN. ) );
#82434 = CIRCLE ( 'NONE', #96239, 4.000000000000007105 ) ;
#82435 = ORIENTED_EDGE ( 'NONE', *, *, #30910, .T. ) ;
#82436 = CARTESIAN_POINT ( 'NONE',  ( 42.76313255034848737, 461.1833584523197374, 3.199811539391409720 ) ) ;
#82437 = AXIS2_PLACEMENT_3D ( 'NONE', #85720, #11793, #87834 ) ;
#82438 = DIRECTION ( 'NONE',  ( 0.000000000000000000, -1.000000000000000000, 0.000000000000000000 ) ) ;
#82439 = CARTESIAN_POINT ( 'NONE',  ( -81.46780060742058538, -60.00000000000000000, -27.04454207428921464 ) ) ;
#82440 = ORIENTED_EDGE ( 'NONE', *, *, #34154, .T. ) ;
#82441 = CARTESIAN_POINT ( 'NONE',  ( 46.74337182782031164, -35.07991228416439355, -28.45280748186943853 ) ) ;
#82442 = DIRECTION ( 'NONE',  ( -1.000000000000000000, -1.224606353822377258E-16, -0.000000000000000000 ) ) ;
#82443 = CARTESIAN_POINT ( 'NONE',  ( -3.386166401410786619, -0.8620773598010494920, 104.0373207615035085 ) ) ;
#82444 = CARTESIAN_POINT ( 'NONE',  ( -47.44718022415302272, 11.18620753528886524, 16.71882890723488302 ) ) ;
#82445 = EDGE_LOOP ( 'NONE', ( #2629, #24220 ) ) ;
#82446 = ORIENTED_EDGE ( 'NONE', *, *, #77516, .T. ) ;
#82447 = VERTEX_POINT ( 'NONE', #105865 ) ;
#82448 = CARTESIAN_POINT ( 'NONE',  ( 30.24426401564364753, 336.7248776613420205, 17.61103644359287301 ) ) ;
#82449 = CARTESIAN_POINT ( 'NONE',  ( -5.000000000000000000, -13.87446176118090868, 11.25142367425977774 ) ) ;
#82450 = CARTESIAN_POINT ( 'NONE',  ( 8.143901214329899974E-15, 79.50000000000000000, -66.50000000000000000 ) ) ;
#82451 = VERTEX_POINT ( 'NONE', #22864 ) ;
#82452 = EDGE_CURVE ( 'NONE', #45904, #100031, #65765, .T. ) ;
#82453 = DIRECTION ( 'NONE',  ( -1.000000000000000000, -1.224606353822377258E-16, -0.000000000000000000 ) ) ;
#82454 = CARTESIAN_POINT ( 'NONE',  ( -66.76860190796567451, 46.03420836107012093, 33.38430095398283726 ) ) ;
#82455 = VECTOR ( 'NONE', #53397, 1000.000000000000000 ) ;
#82456 = FACE_OUTER_BOUND ( 'NONE', #3384, .T. ) ;
#82457 = CARTESIAN_POINT ( 'NONE',  ( -70.46077158043857480, -57.68242143155622159, 157.6729293506350018 ) ) ;
#82458 = CARTESIAN_POINT ( 'NONE',  ( -2.977408999572654480, -28.62500000204838457, 7.188101187499999156 ) ) ;
#82459 = CARTESIAN_POINT ( 'NONE',  ( -30.75723595955501111, 13.12755156482207397, 41.50738620754120944 ) ) ;
#82460 = CONICAL_SURFACE ( 'NONE', #101408, 4.000000000000001776, 0.9599310885968774798 ) ;
#82461 = CARTESIAN_POINT ( 'NONE',  ( 1.224646799147352073E-15, 49.99999999999999289, -75.00000000000001421 ) ) ;
#82462 = DIRECTION ( 'NONE',  ( 0.000000000000000000, -1.000000000000000000, 0.000000000000000000 ) ) ;
#82463 = CARTESIAN_POINT ( 'NONE',  ( -32.64482578944674884, -14.21045842199435150, -35.33261186109891128 ) ) ;
#82464 = EDGE_CURVE ( 'NONE', #82728, #58245, #12083, .T. ) ;
#82465 = CARTESIAN_POINT ( 'NONE',  ( 74.60950000000003968, 4.898587196589412829E-16, -4.000000000000000000 ) ) ;
#82466 = EDGE_CURVE ( 'NONE', #33697, #89914, #10354, .T. ) ;
#82467 = CARTESIAN_POINT ( 'NONE',  ( -49.55661329154894901, -42.98050903381213317, 51.16523380042725222 ) ) ;
#82468 = COLOUR_RGB ( '', 0.72549020, 0.75294118, 0.79215686) ;
#82469 = CARTESIAN_POINT ( 'NONE',  ( 23.09999999999999432, 1.533819458162526451E-15, 0.000000000000000000 ) ) ;
#82470 = ORIENTED_EDGE ( 'NONE', *, *, #3949, .F. ) ;
#82471 = CARTESIAN_POINT ( 'NONE',  ( -99.19657323886772815, -45.25086945323192111, 193.2043375118490189 ) ) ;
#82472 = DIRECTION ( 'NONE',  ( 0.000000000000000000, -1.000000000000000000, 0.000000000000000000 ) ) ;
#82473 = CIRCLE ( 'NONE', #41136, 4.000000000000001776 ) ;
#82474 = CARTESIAN_POINT ( 'NONE',  ( 12.40668049911506721, -3.381773713679836924, 20.61118434233718233 ) ) ;
#82475 = EDGE_LOOP ( 'NONE', ( #100127, #88428, #52734, #95365 ) ) ;
#82476 = DIRECTION ( 'NONE',  ( -0.5735764363510494901, -0.8191520442889894671, 0.000000000000000000 ) ) ;
#82477 = CARTESIAN_POINT ( 'NONE',  ( 104.3671382054701269, -38.40621937790043461, 198.0855672510112981 ) ) ;
#82478 = DIRECTION ( 'NONE',  ( -0.000000000000000000, 1.000000000000000000, -0.000000000000000000 ) ) ;
#82479 = CARTESIAN_POINT ( 'NONE',  ( 37.33349330513379982, 4.000000000000002665, 0.000000000000000000 ) ) ;
#82481 = EDGE_CURVE ( 'NONE', #97550, #26330, #51345, .T. ) ;
#82480 = CARTESIAN_POINT ( 'NONE',  ( 29.34999999999999787, -3.309499999999999886, 4.475777889183790779E-16 ) ) ;
#82482 =( LENGTH_UNIT ( ) NAMED_UNIT ( * ) SI_UNIT ( .MILLI., .METRE. ) );
#82483 = CARTESIAN_POINT ( 'NONE',  ( 84.80995380922897198, -30.00000000000000000, 168.5163431953775444 ) ) ;
#82484 = B_SPLINE_SURFACE_WITH_KNOTS ( 'NONE', 3, 3, ( 
 ( #102382, #61414, #78105, #53824, #70020, #29086, #52228, #86230 ),
 ( #77044, #21496, #85138, #45230, #4223, #95359, #13353, #76504 ),
 ( #102919, #61952, #60358, #86757, #2613, #12825, #93233, #68975 ),
 ( #28009, #45745, #93769, #19926, #85687, #56470, #63536, #89400 ),
 ( #72664, #6865, #31703, #80218, #6322, #14411, #105564, #5293 ),
 ( #62999, #88338, #23618, #95895, #31188, #105047, #55919, #7389 ),
 ( #71595, #97461, #38213, #47322, #104500, #22021, #80751, #72137 ),
 ( #103966, #73175, #14950, #39789, #81275, #64590, #15494, #64073 ),
 ( #48381, #40302, #96432, #88861, #47844, #32229, #46280, #22568 ),
 ( #106080, #96948, #23082, #65108, #30108, #71076, #98005, #39264 ) ),
 .UNSPECIFIED., .F., .F., .F.,
 ( 4, 2, 2, 2, 4 ),
 ( 4, 2, 2, 4 ),
 ( 0.000000000000000000, 0.1250000000000000000, 0.2500000000000000000, 0.5000000000000000000, 1.000000000000000000 ),
 ( 0.000000000000000000, 0.2500000000000000000, 0.5000000000000000000, 1.000000000000000000 ),
 .UNSPECIFIED. ) ;
#82485 = CARTESIAN_POINT ( 'NONE',  ( 35.80547854523823759, 490.7930927354842652, 12.38248481219585884 ) ) ;
#82486 = CARTESIAN_POINT ( 'NONE',  ( -28.88699125077563679, 13.70431814614562249, 39.88880000601581344 ) ) ;
#82487 = CYLINDRICAL_SURFACE ( 'NONE', #15616, 4.250000000000000000 ) ;
#82488 = ORIENTED_EDGE ( 'NONE', *, *, #46775, .F. ) ;
#82489 = ORIENTED_EDGE ( 'NONE', *, *, #29019, .T. ) ;
#82490 = CARTESIAN_POINT ( 'NONE',  ( 51.13673169834419241, -46.43880812507573808, 55.14390178788891461 ) ) ;
#82491 = CARTESIAN_POINT ( 'NONE',  ( 6.373568729748126493, 41.63985758277738114, -58.70717962065710793 ) ) ;
#82492 = CARTESIAN_POINT ( 'NONE',  ( 9.807764809528846328, 51.30006693791943917, 2.674187944274665441 ) ) ;
#82493 =( BOUNDED_SURFACE ( )  B_SPLINE_SURFACE ( 3, 2, ( 
 ( #12328, #38754, #24183 ),
 ( #7414, #49475, #106106 ),
 ( #89943, #81299, #48929 ),
 ( #106646, #47872, #8486 ),
 ( #105588, #80779, #97484 ),
 ( #24703, #90478, #40326 ),
 ( #23640, #81826, #56495 ),
 ( #7950, #39813, #65135 ),
 ( #98031, #57026, #25243 ),
 ( #32254, #16047, #16585 ),
 ( #41391, #73209, #32797 ),
 ( #40856, #58098, #89426 ) ),
 .UNSPECIFIED., .F., .F., .F. ) 
 B_SPLINE_SURFACE_WITH_KNOTS ( ( 4, 2, 2, 2, 2, 4 ),
 ( 3, 3 ),
 ( -1.734723475976807094E-18, 0.001187588843296132415, 0.001781383264944199490, 0.002375177686592266565, 0.003562766529888400716, 0.004750355373184534866 ),
 ( 0.000000000000000000, 1.000000000000000000 ),
 .UNSPECIFIED. ) 
 GEOMETRIC_REPRESENTATION_ITEM ( )  RATIONAL_B_SPLINE_SURFACE ( (
 ( 1.000000000000000000, 0.9359444767143318966, 1.000000000000000000),
 ( 1.000000000000000000, 0.9295581727144616169, 1.000000000000000000),
 ( 1.000000000000000000, 0.9234593375674587934, 1.000000000000000000),
 ( 1.000000000000000000, 0.9150808072273582949, 1.000000000000000000),
 ( 1.000000000000000000, 0.9124161408737813117, 1.000000000000000000),
 ( 1.000000000000000000, 0.9074047588826391619, 1.000000000000000000),
 ( 1.000000000000000000, 0.9050663310859912158, 1.000000000000000000),
 ( 1.000000000000000000, 0.8987692007139892469, 1.000000000000000000),
 ( 1.000000000000000000, 0.8954627112851045734, 1.000000000000000000),
 ( 1.000000000000000000, 0.8909338199770817646, 1.000000000000000000),
 ( 1.000000000000000000, 0.8897377579434112560, 1.000000000000000000),
 ( 1.000000000000000000, 0.8897565210026093796, 1.000000000000000000) ) ) 
 REPRESENTATION_ITEM ( '' )  SURFACE ( )  );
#82494 = VERTEX_POINT ( 'NONE', #91825 ) ;
#82495 = CARTESIAN_POINT ( 'NONE',  ( -92.68075250878385418, -38.35495479572327326, 40.78232060307920648 ) ) ;
#82496 = ORIENTED_EDGE ( 'NONE', *, *, #80392, .F. ) ;
#82497 = CARTESIAN_POINT ( 'NONE',  ( 0.000000000000000000, 200.0000000000000000, 0.000000000000000000 ) ) ;
#82498 = CARTESIAN_POINT ( 'NONE',  ( 98.33859083302846216, -38.35583377044250852, 78.64617500602120970 ) ) ;
#82499 = CARTESIAN_POINT ( 'NONE',  ( 13.61336331607695094, 22.69764540326648117, 2.516109114288500592 ) ) ;
#82500 = CARTESIAN_POINT ( 'NONE',  ( 96.00343290813454189, -45.28274520479027387, 106.3261782004091174 ) ) ;
#82501 = CARTESIAN_POINT ( 'NONE',  ( -89.99999999999997158, -52.00000000000000000, 194.0238439516549818 ) ) ;
#82502 = CONICAL_SURFACE ( 'NONE', #58403, 5.000000000000001776, 0.9599310885968803664 ) ;
#82503 = CARTESIAN_POINT ( 'NONE',  ( -34.54824451023232257, 338.5131454125937012, -0.8343175004005460860 ) ) ;
#82504 = CARTESIAN_POINT ( 'NONE',  ( 6.683837171061806082, 7.911893696991934455, 7.436622852660996417E-19 ) ) ;
#82505 = CARTESIAN_POINT ( 'NONE',  ( 74.38028640914956213, -60.00000000000000711, 175.9798948562111889 ) ) ;
#82506 =( GEOMETRIC_REPRESENTATION_CONTEXT ( 3 ) GLOBAL_UNCERTAINTY_ASSIGNED_CONTEXT ( ( #42934 ) ) GLOBAL_UNIT_ASSIGNED_CONTEXT ( ( #59490, #75647, #76173 ) ) REPRESENTATION_CONTEXT ( 'NONE', 'WORKASPACE' ) );
#82507 = CARTESIAN_POINT ( 'NONE',  ( 17.63369058254861699, 45.00000000000000711, 63.00619685671904335 ) ) ;
#82508 = ORIENTED_EDGE ( 'NONE', *, *, #105197, .T. ) ;
#82509 = CARTESIAN_POINT ( 'NONE',  ( 62.17692095058880142, -36.00921868072364163, 76.36134944486762777 ) ) ;
#82510 = CARTESIAN_POINT ( 'NONE',  ( -26.70424429299868763, 296.1616889006899669, -1.717105780328246567 ) ) ;
#82511 = CARTESIAN_POINT ( 'NONE',  ( 9.423567810130279554, -51.98776212902039617, 23.65038982378345622 ) ) ;
#82512 = CARTESIAN_POINT ( 'NONE',  ( -8.991848411656118145, -5.000000000000000000, -17.27917748744093629 ) ) ;
#82514 = CARTESIAN_POINT ( 'NONE',  ( -35.23448287039504834, 485.0606775613101718, -1.508972397133680143 ) ) ;
#82513 = CARTESIAN_POINT ( 'NONE',  ( -87.05474304109419847, -38.36446612063756589, -20.80080902016944577 ) ) ;
#82515 = CARTESIAN_POINT ( 'NONE',  ( -32.00452718204254410, 333.4532925135374626, 17.36126857274863156 ) ) ;
#82516 = DIRECTION ( 'NONE',  ( 1.000000000000000000, 1.224606353822377258E-16, 0.000000000000000000 ) ) ;
#82517 = CYLINDRICAL_SURFACE ( 'NONE', #50595, 4.000000000000000888 ) ;
#82518 = CARTESIAN_POINT ( 'NONE',  ( -5.656854249492381470, -25.06249999999999289, 5.656854249492379694 ) ) ;
#82519 = CARTESIAN_POINT ( 'NONE',  ( -9.739726766103894207, -3.000000000000002665, -82.38252115500876016 ) ) ;
#82520 = CIRCLE ( 'NONE', #17086, 8.000000000000000000 ) ;
#82521 = EDGE_CURVE ( 'NONE', #82573, #98241, #103641, .T. ) ;
#82522 = COLOUR_RGB ( '', 0.40784314, 0.44705882, 0.49803922) ;
#82523 = CIRCLE ( 'NONE', #89461, 5.000000000000011546 ) ;
#82524 = CARTESIAN_POINT ( 'NONE',  ( 88.20199406385988539, 1.030564683017419500E-14, 0.000000000000000000 ) ) ;
#82525 = ORIENTED_EDGE ( 'NONE', *, *, #100937, .F. ) ;
#82526 = CARTESIAN_POINT ( 'NONE',  ( 82.76483955553528915, -53.62660239749297375, 185.2436993791692998 ) ) ;
#82527 = CARTESIAN_POINT ( 'NONE',  ( 43.48224507221030422, 485.4751843846681254, 4.033548163687394883 ) ) ;
#82528 = CARTESIAN_POINT ( 'NONE',  ( -8.000000000000000000, -9.031250004096769146, -3.313708498984762496 ) ) ;
#82529 = VERTEX_POINT ( 'NONE', #19575 ) ;
#82530 = DIRECTION ( 'NONE',  ( -1.000000000000000000, -1.224606353822377258E-16, -0.000000000000000000 ) ) ;
#82531 = DIRECTION ( 'NONE',  ( -1.000000000000000000, -1.224606353822377258E-16, -0.000000000000000000 ) ) ;
#82532 = CARTESIAN_POINT ( 'NONE',  ( -32.20627048526868208, 464.6794164287650801, 10.68709986547766988 ) ) ;
#82533 = FACE_OUTER_BOUND ( 'NONE', #50510, .T. ) ;
#82534 = LINE ( 'NONE', #7042, #2328 ) ;
#82535 =( GEOMETRIC_REPRESENTATION_CONTEXT ( 3 ) GLOBAL_UNCERTAINTY_ASSIGNED_CONTEXT ( ( #7420 ) ) GLOBAL_UNIT_ASSIGNED_CONTEXT ( ( #62957, #45194, #21983 ) ) REPRESENTATION_CONTEXT ( 'NONE', 'WORKASPACE' ) );
#82536 = AXIS2_PLACEMENT_3D ( 'NONE', #76433, #66767, #59214 ) ;
#82537 = CARTESIAN_POINT ( 'NONE',  ( 74.07777777777778283, 6.915964383211875250E-15, 0.000000000000000000 ) ) ;
#82538 = FACE_OUTER_BOUND ( 'NONE', #19782, .T. ) ;
#82541 = CIRCLE ( 'NONE', #22296, 3.309500000000001663 ) ;
#82540 = CARTESIAN_POINT ( 'NONE',  ( -15.42518680700535505, 22.80197049373886742, -2.000786945160570429 ) ) ;
#82539 = CARTESIAN_POINT ( 'NONE',  ( -8.340838532639699210, -19.57404221892459617, 35.25850611839925364 ) ) ;
#82542 = B_SPLINE_CURVE_WITH_KNOTS ( 'NONE', 3,
 ( #66081, #33741, #75222, #66615 ),
 .UNSPECIFIED., .F., .F.,
 ( 4, 4 ),
 ( 1.001051563156762085E-15, 0.001949579373385036327 ),
 .UNSPECIFIED. ) ;
#82543 = CARTESIAN_POINT ( 'NONE',  ( 4.401442555609581635E-16, -15.78125000204838635, -7.188101187500000044 ) ) ;
#82544 = CARTESIAN_POINT ( 'NONE',  ( 0.000000000000000000, 80.00000000000000000, -8.000000000000014211 ) ) ;
#82545 = CARTESIAN_POINT ( 'NONE',  ( 92.53532739719321398, 5.000000000000020428, 0.000000000000000000 ) ) ;
#82546 = EDGE_CURVE ( 'NONE', #46570, #20548, #99564, .T. ) ;
#82547 = CIRCLE ( 'NONE', #53231, 6.499999999999999112 ) ;
#82548 = ORIENTED_EDGE ( 'NONE', *, *, #8268, .T. ) ;
#82549 = EDGE_CURVE ( 'NONE', #106390, #72737, #10874, .T. ) ;
#82550 = CARTESIAN_POINT ( 'NONE',  ( -19.48249511158732261, 49.99632329421929455, 60.25369351552990338 ) ) ;
#82551 = CARTESIAN_POINT ( 'NONE',  ( 7.500000000000000000, 4.732328341851994580, -7.493855119309152713 ) ) ;
#82552 = LINE ( 'NONE', #2688, #4554 ) ;
#82554 = CARTESIAN_POINT ( 'NONE',  ( 55.49475206934125282, -21.76998406339067671, -24.27117048680137756 ) ) ;
#82553 = CARTESIAN_POINT ( 'NONE',  ( 4.649619579745470688, 54.30983937696358055, 6.194660934072837577 ) ) ;
#82555 = ORIENTED_EDGE ( 'NONE', *, *, #54946, .F. ) ;
#82556 = VECTOR ( 'NONE', #49350, 1000.000000000000000 ) ;
#82557 = CARTESIAN_POINT ( 'NONE',  ( -6.000469943554648466, -89.00070491670501838, 0.2622423038614462021 ) ) ;
#82558 = FILL_AREA_STYLE ('',( #75523 ) ) ;
#82559 = EDGE_LOOP ( 'NONE', ( #72791, #81658, #48917, #77362, #82176 ) ) ;
#82560 = PRESENTATION_STYLE_ASSIGNMENT (( #80954 ) ) ;
#82561 = FILL_AREA_STYLE ('',( #64786 ) ) ;
#82562 = MECHANICAL_DESIGN_GEOMETRIC_PRESENTATION_REPRESENTATION (  '', ( #56764 ), #63883 ) ;
#82563 = CARTESIAN_POINT ( 'NONE',  ( -34.17192354664857845, 40.55982561316064050, -60.71114593581258845 ) ) ;
#82564 = CARTESIAN_POINT ( 'NONE',  ( -95.53743085115178246, -59.99999999999999289, 52.85914003497030933 ) ) ;
#82565 = PLANE ( 'NONE',  #66915 ) ;
#82566 = CARTESIAN_POINT ( 'NONE',  ( 6.463178677061750754, 2.643201791673480905, 6.839998497243177766 ) ) ;
#82567 = CARTESIAN_POINT ( 'NONE',  ( 41.13640268182594184, 465.3860676345191791, 16.49894919583628905 ) ) ;
#82568 = CARTESIAN_POINT ( 'NONE',  ( -32.87806366422623228, 464.9425629022531439, 11.07779413895617004 ) ) ;
#82570 = CARTESIAN_POINT ( 'NONE',  ( 32.11606453551802787, 486.2854634841322650, 5.773331070944215604 ) ) ;
#82569 = CARTESIAN_POINT ( 'NONE',  ( 1.308996937483426937, -5.000000000000002665, -75.00000000000001421 ) ) ;
#82571 = TOROIDAL_SURFACE ( 'NONE', #103300, 59.50000000000000000, 0.5000000000000000000 ) ;
#82572 = CARTESIAN_POINT ( 'NONE',  ( -85.40752079689818288, -21.99789027431144461, 165.0058301840674915 ) ) ;
#82573 = VERTEX_POINT ( 'NONE', #99347 ) ;
#82574 = ORIENTED_EDGE ( 'NONE', *, *, #4983, .F. ) ;
#82575 = VERTEX_POINT ( 'NONE', #2252 ) ;
#82576 = DIRECTION ( 'NONE',  ( 0.000000000000000000, 0.000000000000000000, -1.000000000000000000 ) ) ;
#82577 = DIRECTION ( 'NONE',  ( 1.000000000000000000, 0.000000000000000000, 0.000000000000000000 ) ) ;
#82578 = EDGE_LOOP ( 'NONE', ( #98493, #43291, #39169, #78543 ) ) ;
#82579 = PLANE ( 'NONE',  #30660 ) ;
#82580 = PRESENTATION_STYLE_ASSIGNMENT (( #50719 ) ) ;
#82581 = DIRECTION ( 'NONE',  ( -1.000000000000000000, -0.000000000000000000, -0.000000000000000000 ) ) ;
#82582 = CARTESIAN_POINT ( 'NONE',  ( -3.866854618780460662, 16.79548022286313724, 5.835366698912954675 ) ) ;
#82583 = DIRECTION ( 'NONE',  ( -1.000000000000000000, -0.000000000000000000, -0.000000000000000000 ) ) ;
#82584 = CARTESIAN_POINT ( 'NONE',  ( -20.24579557674108088, 304.8297271373347144, -10.00469232190996927 ) ) ;
#82585 = DIRECTION ( 'NONE',  ( 0.000000000000000000, 1.000000000000000000, 0.000000000000000000 ) ) ;
#82586 = AXIS2_PLACEMENT_3D ( 'NONE', #14332, #55839, #24594 ) ;
#82587 = CARTESIAN_POINT ( 'NONE',  ( 109.4365241820779460, -29.99999999999997158, 178.4894931318444264 ) ) ;
#82588 = CARTESIAN_POINT ( 'NONE',  ( -103.0033221043092482, -14.21045842199434084, 193.8525198385365798 ) ) ;
#82589 = CARTESIAN_POINT ( 'NONE',  ( -64.65631851940639763, -18.62622571681349015, 74.52696835048116952 ) ) ;
#82590 = ORIENTED_EDGE ( 'NONE', *, *, #24204, .F. ) ;
#82591 = CARTESIAN_POINT ( 'NONE',  ( 28.18312358715398247, 38.95287143380507899, 57.16470827993371984 ) ) ;
#82592 = CARTESIAN_POINT ( 'NONE',  ( 114.3145214074224612, -60.00000000001458744, 180.5198259458585142 ) ) ;
#82593 = VERTEX_POINT ( 'NONE', #68073 ) ;
#82594 = CARTESIAN_POINT ( 'NONE',  ( 4.115445282636351898, -56.87775089494874692, 33.36138305263114745 ) ) ;
#82596 = CARTESIAN_POINT ( 'NONE',  ( -100.6278159255352023, -37.82081252527048321, 144.5841055454753246 ) ) ;
#82595 = VECTOR ( 'NONE', #94599, 1000.000000000000000 ) ;
#82597 = CARTESIAN_POINT ( 'NONE',  ( 7.188101187499999156, -13.62500000204838457, 2.977408999572654924 ) ) ;
#82598 = CARTESIAN_POINT ( 'NONE',  ( -9.432319653624512412, -5.000000000000000000, -70.68463330168729897 ) ) ;
#82599 = ORIENTED_EDGE ( 'NONE', *, *, #105815, .T. ) ;
#82600 = CARTESIAN_POINT ( 'NONE',  ( 0.000000000000000000, 38.67090180175566871, -23.23666318551310539 ) ) ;
#82601 = ORIENTED_EDGE ( 'NONE', *, *, #106767, .T. ) ;
#82602 = CARTESIAN_POINT ( 'NONE',  ( 0.000000000000000000, 0.000000000000000000, 4.000000000000000000 ) ) ;
#82603 = CARTESIAN_POINT ( 'NONE',  ( -44.85383984935189972, -60.00000000000000000, 60.30378881490838694 ) ) ;
#82604 = CARTESIAN_POINT ( 'NONE',  ( 9.442659817596066318, -56.44252752747822655, 30.29540378708609794 ) ) ;
#82605 = CARTESIAN_POINT ( 'NONE',  ( -7.188101187500001821, -20.37500000204838457, -2.977408999572651371 ) ) ;
#82606 = DIRECTION ( 'NONE',  ( 1.000000000000000000, 1.224606353822377258E-16, 0.000000000000000000 ) ) ;
#82608 = EDGE_CURVE ( 'NONE', #98120, #97131, #74371, .T. ) ;
#82607 = CARTESIAN_POINT ( 'NONE',  ( 32.28552837373269568, 464.7648866755952213, 15.30384310833107975 ) ) ;
#82609 = CARTESIAN_POINT ( 'NONE',  ( -2.652001306203245701, 20.85810219201849947, -6.481200489579615365 ) ) ;
#82610 = CARTESIAN_POINT ( 'NONE',  ( 1.000000000000000000, -26.67919295183541095, -6.179716592098927208 ) ) ;
#82611 = CARTESIAN_POINT ( 'NONE',  ( 32.81992448453858913, 465.7192846569213316, 11.17271167765314388 ) ) ;
#82612 = EDGE_CURVE ( 'NONE', #8540, #70974, #60013, .T. ) ;
#82613 = CARTESIAN_POINT ( 'NONE',  ( 15.90614609307868932, -3.157894736842108863, 14.66382285868950852 ) ) ;
#82614 = CARTESIAN_POINT ( 'NONE',  ( -24.41558313457672469, 27.38491394452228533, 32.32218024782103072 ) ) ;
#82615 = CARTESIAN_POINT ( 'NONE',  ( 86.91792654137822183, -60.00000000000002132, 29.36145308659259712 ) ) ;
#82616 = CARTESIAN_POINT ( 'NONE',  ( -33.23717309666378128, -46.43422961256527515, 35.74388805338151798 ) ) ;
#82617 = AXIS2_PLACEMENT_3D ( 'NONE', #86069, #13729, #20300 ) ;
#82618 = CIRCLE ( 'NONE', #39598, 5.000000000000010658 ) ;
#82619 = CARTESIAN_POINT ( 'NONE',  ( 42.14189753562169471, -39.52400511673570094, 40.59849300099191538 ) ) ;
#82620 = DIRECTION ( 'NONE',  ( 0.000000000000000000, 0.000000000000000000, 1.000000000000000000 ) ) ;
#82621 = VERTEX_POINT ( 'NONE', #19038 ) ;
#82622 = CARTESIAN_POINT ( 'NONE',  ( 43.86611073477487821, 435.5752409525302937, 9.535927547466386045 ) ) ;
#82623 = COLOUR_RGB ( '', 0.72549020, 0.75294118, 0.79215686) ;
#82624 = CARTESIAN_POINT ( 'NONE',  ( -76.80863678880248813, -38.44002279010879164, 183.4121976866223918 ) ) ;
#82625 = ORIENTED_EDGE ( 'NONE', *, *, #21083, .F. ) ;
#82627 = CARTESIAN_POINT ( 'NONE',  ( 40.07586470527510158, 337.7832441655235129, 20.21182470898328631 ) ) ;
#82626 = CARTESIAN_POINT ( 'NONE',  ( 47.33349330513379982, 4.000000000000002665, 0.000000000000000000 ) ) ;
#82628 = CARTESIAN_POINT ( 'NONE',  ( -14.11595029531626722, 2.410436752329290222, 5.024000119293328126 ) ) ;
#82629 = CARTESIAN_POINT ( 'NONE',  ( 15.64878411475365638, 36.78373704832291224, 23.72567384382491795 ) ) ;
#82630 = DIRECTION ( 'NONE',  ( 1.000000000000000000, 1.224606353822377258E-16, 0.000000000000000000 ) ) ;
#82631 = EDGE_CURVE ( 'NONE', #104741, #60462, #101941, .T. ) ;
#82632 = DIRECTION ( 'NONE',  ( -0.000000000000000000, -0.000000000000000000, 1.000000000000000000 ) ) ;
#82633 = CARTESIAN_POINT ( 'NONE',  ( -31.27146333409443812, 363.0590912728651460, 21.43603929113760387 ) ) ;
#82634 = AXIS2_PLACEMENT_3D ( 'NONE', #100505, #1798, #9353 ) ;
#82635 = CARTESIAN_POINT ( 'NONE',  ( 108.2925581171813434, -59.99999999999999289, 131.0643579034831134 ) ) ;
#82636 = CARTESIAN_POINT ( 'NONE',  ( 39.34999999999999432, -3.309499999999999886, 0.000000000000000000 ) ) ;
#82637 =( BOUNDED_SURFACE ( )  B_SPLINE_SURFACE ( 3, 2, ( 
 ( #22886, #64910, #7714 ),
 ( #80545, #31510, #23957 ),
 ( #55723, #81078, #63337 ),
 ( #88653, #79496, #7188 ),
 ( #96232, #63866, #105371 ),
 ( #15822, #40623, #21829 ),
 ( #104293, #39057, #23412 ),
 ( #71937, #13687, #95686 ),
 ( #48702, #64391, #71392 ),
 ( #56256, #30983, #89189 ) ),
 .UNSPECIFIED., .F., .F., .F. ) 
 B_SPLINE_SURFACE_WITH_KNOTS ( ( 4, 2, 2, 2, 4 ),
 ( 3, 3 ),
 ( 0.002450517525418908181, 0.003060732775749477712, 0.003670948026080046809, 0.004891378526741185437, 0.007332239528063463560 ),
 ( 0.000000000000000000, 1.000000000000000000 ),
 .UNSPECIFIED. ) 
 GEOMETRIC_REPRESENTATION_ITEM ( )  RATIONAL_B_SPLINE_SURFACE ( (
 ( 1.000000000000000000, 0.7071067811865481278, 1.000000000000000000),
 ( 1.000000000000000000, 0.7344063550101855853, 1.000000000000000000),
 ( 1.000000000000000000, 0.7590375248711123124, 1.000000000000000000),
 ( 1.000000000000000000, 0.8038331608703979114, 1.000000000000000000),
 ( 1.000000000000000000, 0.8240352460865458806, 1.000000000000000000),
 ( 1.000000000000000000, 0.8791017378334128329, 1.000000000000000000),
 ( 1.000000000000000000, 0.9085032776980890290, 1.000000000000000000),
 ( 1.000000000000000000, 0.9784170511696809180, 1.000000000000000000),
 ( 1.000000000000000000, 0.9996598051696596876, 1.000000000000000000),
 ( 1.000000000000000000, 1.000000000000000000, 1.000000000000000000) ) ) 
 REPRESENTATION_ITEM ( '' )  SURFACE ( )  );
#82638 = CARTESIAN_POINT ( 'NONE',  ( -5.290067270632216712, -1.200000000000000030E-05, 7.281152949374556371 ) ) ;
#82639 = AXIS2_PLACEMENT_3D ( 'NONE', #75309, #100123, #66159 ) ;
#82640 = ORIENTED_EDGE ( 'NONE', *, *, #33108, .T. ) ;
#82641 = CARTESIAN_POINT ( 'NONE',  ( -97.61388050977055286, -29.99999999999991118, 190.8267997822536302 ) ) ;
#82642 = ORIENTED_EDGE ( 'NONE', *, *, #53315, .F. ) ;
#82643 = AXIS2_PLACEMENT_3D ( 'NONE', #37348, #85887, #93963 ) ;
#82644 = CARTESIAN_POINT ( 'NONE',  ( 25.97856261898818531, 37.20666516320237349, -8.258827374226497042 ) ) ;
#82645 = CYLINDRICAL_SURFACE ( 'NONE', #28756, 4.000000000000000000 ) ;
#82646 = CARTESIAN_POINT ( 'NONE',  ( 3.363293968491885888, 121.3118620733033168, 5.000000000000000000 ) ) ;
#82647 = CARTESIAN_POINT ( 'NONE',  ( 25.98780635108152737, 307.2400872882208773, 10.71531891313127183 ) ) ;
#82648 = CARTESIAN_POINT ( 'NONE',  ( 9.918010731619567366, 26.20848315156774788, -1.300854425901584621 ) ) ;
#82649 = CARTESIAN_POINT ( 'NONE',  ( -5.082755093536326818, -20.09375000204838457, 5.082755093536325042 ) ) ;
#82650 = CARTESIAN_POINT ( 'NONE',  ( -3.566423465315849750, -0.9305320722653663834, 103.5097305745183576 ) ) ;
#82651 = CARTESIAN_POINT ( 'NONE',  ( 6.806778131844891000, 41.25019534418786549, -70.74215739200818120 ) ) ;
#82652 = ADVANCED_FACE ( 'NONE', ( #18482 ), #82662, .F. ) ;
#82653 = AXIS2_PLACEMENT_3D ( 'NONE', #19519, #76099, #1122 ) ;
#82654 = VERTEX_POINT ( 'NONE', #76687 ) ;
#82655 = CARTESIAN_POINT ( 'NONE',  ( 80.02940799275995687, -53.38023646017801838, 163.9019173082060661 ) ) ;
#82656 =( LENGTH_UNIT ( ) NAMED_UNIT ( * ) SI_UNIT ( .MILLI., .METRE. ) );
#82657 = CARTESIAN_POINT ( 'NONE',  ( 9.537291425704605530, 87.64404377332773777, 3.012810007365998022 ) ) ;
#82658 = ORIENTED_EDGE ( 'NONE', *, *, #28103, .T. ) ;
#82659 = FILL_AREA_STYLE ('',( #74026 ) ) ;
#82660 = DIRECTION ( 'NONE',  ( 0.000000000000000000, 1.000000000000000000, -0.000000000000000000 ) ) ;
#82661 = CARTESIAN_POINT ( 'NONE',  ( 38.56639310406619359, 27.31833143340870507, -12.97492099455193149 ) ) ;
#82662 = CYLINDRICAL_SURFACE ( 'NONE', #26234, 7.000000000000000000 ) ;
#82663 = CARTESIAN_POINT ( 'NONE',  ( -66.35471210918942120, -60.00000000000000000, -27.72999305472536236 ) ) ;
#82664 = CARTESIAN_POINT ( 'NONE',  ( -33.09102985894170246, 433.0213902170605138, 24.60354821821731264 ) ) ;
#82665 = EDGE_CURVE ( 'NONE', #23893, #101293, #2798, .T. ) ;
#82666 = ORIENTED_EDGE ( 'NONE', *, *, #101926, .F. ) ;
#82667 = DIRECTION ( 'NONE',  ( 0.000000000000000000, -0.000000000000000000, 1.000000000000000000 ) ) ;
#82668 = CIRCLE ( 'NONE', #6904, 8.000000000000007105 ) ;
#82669 = CARTESIAN_POINT ( 'NONE',  ( 38.34155876363057303, 18.64284798592657921, -2.616639027923388205 ) ) ;
#82670 = CARTESIAN_POINT ( 'NONE',  ( 86.58330031195315257, -46.47876529169381143, 190.3702665925659119 ) ) ;
#82671 = CARTESIAN_POINT ( 'NONE',  ( 0.000000000000000000, 0.000000000000000000, -1.446714285714285841 ) ) ;
#82672 = CARTESIAN_POINT ( 'NONE',  ( -2.977408999572650039, -32.18750000204838813, -7.188101187500001821 ) ) ;
#82673 = CARTESIAN_POINT ( 'NONE',  ( -14.84266821126132285, 4.606643506689745315, 5.685020543979530494 ) ) ;
#82674 = EDGE_CURVE ( 'NONE', #57765, #26186, #27942, .T. ) ;
#82675 = CARTESIAN_POINT ( 'NONE',  ( 41.66068395357901011, 437.6580662123523098, 21.73548463238672923 ) ) ;
#82676 = CONTEXT_DEPENDENT_SHAPE_REPRESENTATION ( #14182, #45818 ) ;
#82677 = CARTESIAN_POINT ( 'NONE',  ( 49.26505482459812413, 8.072780847947159444, 15.39015249100645732 ) ) ;
#82678 = ORIENTED_EDGE ( 'NONE', *, *, #61085, .T. ) ;
#82679 = LINE ( 'NONE', #99372, #69814 ) ;
#82680 = ADVANCED_FACE ( 'NONE', ( #8764 ), #41669, .T. ) ;
#82681 = CARTESIAN_POINT ( 'NONE',  ( 0.000000000000000000, 0.000000000000000000, 0.000000000000000000 ) ) ;
#82682 = EDGE_CURVE ( 'NONE', #36077, #68266, #99901, .T. ) ;
#82683 = CARTESIAN_POINT ( 'NONE',  ( 0.000000000000000000, -4.000000000000003553, 112.0000000000000000 ) ) ;
#82684 = TOROIDAL_SURFACE ( 'NONE', #60312, 61.00000000000000000, 0.5000000000000000000 ) ;
#82685 = EDGE_LOOP ( 'NONE', ( #20465, #73738, #26493, #63220 ) ) ;
#82686 = SURFACE_STYLE_USAGE ( .BOTH. , #8791 ) ;
#82687 = CARTESIAN_POINT ( 'NONE',  ( -42.51410301899422706, 462.6487061729604306, 3.764838390874527541 ) ) ;
#82688 = CARTESIAN_POINT ( 'NONE',  ( 107.5635267603475143, -57.67122975978698918, 113.7780230091279492 ) ) ;
#82689 = ADVANCED_FACE ( 'NONE', ( #1172 ), #43130, .T. ) ;
#82690 = VECTOR ( 'NONE', #39192, 1000.000000000000227 ) ;
#82691 = CARTESIAN_POINT ( 'NONE',  ( 34.16642289233192287, 463.8422268500521000, 18.98106911353298187 ) ) ;
#82692 = CARTESIAN_POINT ( 'NONE',  ( 27.61650669486618881, -3.999999999999998224, 0.000000000000000000 ) ) ;
#82693 = CARTESIAN_POINT ( 'NONE',  ( 33.86650669486618881, 4.898587196589413815E-16, -4.000000000000000888 ) ) ;
#82694 = DIRECTION ( 'NONE',  ( -1.000000000000000000, -1.224606353822377258E-16, -0.000000000000000000 ) ) ;
#82695 = CARTESIAN_POINT ( 'NONE',  ( -81.88052546256818687, -59.99999999999998579, 197.9492418936315232 ) ) ;
#82696 = DIRECTION ( 'NONE',  ( 0.000000000000000000, 1.000000000000000000, 0.000000000000000000 ) ) ;
#82697 = CARTESIAN_POINT ( 'NONE',  ( -40.93292669599463096, 378.0706848361106722, 26.55786848468904537 ) ) ;
#82698 = CARTESIAN_POINT ( 'NONE',  ( -84.53199363263830435, -50.18958262607095122, 188.2551344591533109 ) ) ;
#82700 = ADVANCED_FACE ( 'NONE', ( #13538 ), #88178, .T. ) ;
#82699 = EDGE_LOOP ( 'NONE', ( #31610, #105236, #41151, #19507 ) ) ;
#82701 = CARTESIAN_POINT ( 'NONE',  ( 25.78481569285033714, 306.6490176242861025, -8.604953696922189366 ) ) ;
#82702 = AXIS2_PLACEMENT_3D ( 'NONE', #93120, #27372, #2503 ) ;
#82703 = AXIS2_PLACEMENT_3D ( 'NONE', #36902, #27759, #42826 ) ;
#82704 = ORIENTED_EDGE ( 'NONE', *, *, #3949, .T. ) ;
#82705 = CARTESIAN_POINT ( 'NONE',  ( -7.986539162393899716, -13.97327171057452411, -0.5321833565149880485 ) ) ;
#82706 = B_SPLINE_CURVE_WITH_KNOTS ( 'NONE', 3,
 ( #81771, #7893, #40800, #73693, #74753, #106596, #32745, #8433, #98500, #65617, #832, #33803, #24650, #301, #57503, #90425, #41332, #58043, #74224, #33269, #99022, #53682 ),
 .UNSPECIFIED., .F., .F.,
 ( 4, 2, 2, 2, 2, 2, 2, 2, 2, 2, 4 ),
 ( 0.003083058008555209992, 0.003587558145623159604, 0.003839808214157137880, 0.004092058282691116156, 0.004596558419759067503, 0.004848808488293042743, 0.005101058556827017983, 0.006110058830962923279, 0.006614558968030877228, 0.006866809036564849866, 0.007119059105098823372 ),
 .UNSPECIFIED. ) ;
#82707 = DIRECTION ( 'NONE',  ( -1.000000000000000000, -1.224606353822377258E-16, -0.000000000000000000 ) ) ;
#82708 = CARTESIAN_POINT ( 'NONE',  ( -84.20675286544745575, -45.26271561791529052, -10.90008403679102678 ) ) ;
#82709 = VECTOR ( 'NONE', #53880, 1000.000000000000000 ) ;
#82710 = CARTESIAN_POINT ( 'NONE',  ( -4.442085480450870705, -13.39242828886067826, -9.057376035804495018 ) ) ;
#82711 = CARTESIAN_POINT ( 'NONE',  ( -4.261688254080127969, 11.55297089381481790, -5.000000000000000888 ) ) ;
#82712 = CARTESIAN_POINT ( 'NONE',  ( 66.00571552735603120, 6.975173280561618775E-15, 0.000000000000000000 ) ) ;
#82713 = CARTESIAN_POINT ( 'NONE',  ( -33.68177706158878237, 464.5004658938952389, 17.05886715805492670 ) ) ;
#82714 = CARTESIAN_POINT ( 'NONE',  ( 69.92761780597730592, -4.000000000000000000, 0.000000000000000000 ) ) ;
#82715 = CARTESIAN_POINT ( 'NONE',  ( -5.404594501095027787E-15, 34.25047185182970111, 44.13186320217320713 ) ) ;
#82716 = CARTESIAN_POINT ( 'NONE',  ( -36.33173443512122702, 437.9974107914313208, 4.196572296727017815 ) ) ;
#82717 = VECTOR ( 'NONE', #95633, 1000.000000000000000 ) ;
#82718 = CARTESIAN_POINT ( 'NONE',  ( 8.309465130445103043, -30.00000000000003197, -39.88086614825118659 ) ) ;
#82719 = CARTESIAN_POINT ( 'NONE',  ( -76.37321092434198988, -36.02324841633205210, 123.8609354419510566 ) ) ;
#82720 = ORIENTED_EDGE ( 'NONE', *, *, #11707, .T. ) ;
#82721 = CARTESIAN_POINT ( 'NONE',  ( 74.38357847894150154, -30.00000000000000711, 152.0601407382578429 ) ) ;
#82722 = CARTESIAN_POINT ( 'NONE',  ( 7.744329845603314944, 88.46288230153457732, -2.018701143083231120 ) ) ;
#82723 = CARTESIAN_POINT ( 'NONE',  ( 101.7828819589541496, -57.67122312341045642, 79.74621725149124529 ) ) ;
#82724 = ORIENTED_EDGE ( 'NONE', *, *, #46901, .T. ) ;
#82725 = DIRECTION ( 'NONE',  ( 0.000000000000000000, -1.000000000000000000, 0.000000000000000000 ) ) ;
#82726 = AXIS2_PLACEMENT_3D ( 'NONE', #88825, #31155, #79668 ) ;
#82727 = CYLINDRICAL_SURFACE ( 'NONE', #64927, 4.000000000000000888 ) ;
#82728 = VERTEX_POINT ( 'NONE', #78283 ) ;
#82729 = FACE_OUTER_BOUND ( 'NONE', #85254, .T. ) ;
#82730 = FILL_AREA_STYLE ('',( #57374 ) ) ;
#82731 = FACE_OUTER_BOUND ( 'NONE', #1786, .T. ) ;
#82732 = CARTESIAN_POINT ( 'NONE',  ( -2.977408999572654480, -10.62500000204838813, 7.188101187499999156 ) ) ;
#82733 = CARTESIAN_POINT ( 'NONE',  ( 43.52075891743749736, 484.7805561108179973, 4.063293749110879816 ) ) ;
#82734 = CARTESIAN_POINT ( 'NONE',  ( 13.86650669486618881, 4.898587196589411843E-16, -4.000000000000000888 ) ) ;
#82735 = EDGE_CURVE ( 'NONE', #48529, #63779, #60638, .T. ) ;
#82736 = LINE ( 'NONE', #8838, #80657 ) ;
#82737 = CARTESIAN_POINT ( 'NONE',  ( -10.63258248847111531, 48.00000000000000000, -95.64586607611548175 ) ) ;
#82738 = EDGE_LOOP ( 'NONE', ( #61924, #86800, #83772, #75121, #69585 ) ) ;
#82739 = CARTESIAN_POINT ( 'NONE',  ( -7.168069589493909710, 40.56151012121110710, -70.87151392390727267 ) ) ;
#82740 = CARTESIAN_POINT ( 'NONE',  ( 28.40064430096010639, -36.00640833670148311, 32.00032701160584026 ) ) ;
#82741 = VECTOR ( 'NONE', #60425, 1000.000000000000000 ) ;
#82742 = CARTESIAN_POINT ( 'NONE',  ( 35.45927743045602654, 433.4366494758652948, 5.520752814291649102 ) ) ;
#82743 = EDGE_CURVE ( 'NONE', #3401, #55657, #83010, .T. ) ;
#82744 = ORIENTED_EDGE ( 'NONE', *, *, #14937, .T. ) ;
#82746 = CARTESIAN_POINT ( 'NONE',  ( -0.9990332814551574625, 14.07295282070545994, 51.25458646076748437 ) ) ;
#82745 = B_SPLINE_CURVE_WITH_KNOTS ( 'NONE', 3,
 ( #41423, #74839, #18240, #51095, #84015, #32831, #393, #33360, #73783, #106684, #65710, #98592, #24738, #90510, #91063, #48223, #55768, #63914, #88177, #104895 ),
 .UNSPECIFIED., .F., .F.,
 ( 4, 2, 2, 2, 2, 2, 2, 2, 2, 4 ),
 ( 0.002817615579195576793, 0.003321638736722653390, 0.003825661894249729553, 0.004329685051776806584, 0.004833708209303882314, 0.005337731366830958911, 0.005589742945594498510, 0.005841754524358047651, 0.006345777681885138993, 0.006849800839412230336 ),
 .UNSPECIFIED. ) ;
#82747 = ORIENTED_EDGE ( 'NONE', *, *, #62176, .T. ) ;
#82749 = FACE_OUTER_BOUND ( 'NONE', #99595, .T. ) ;
#82748 = CARTESIAN_POINT ( 'NONE',  ( 103.5111111111111057, 4.172000000000019249, 0.000000000000000000 ) ) ;
#82750 = DIRECTION ( 'NONE',  ( 1.000000000000000000, 0.000000000000000000, 1.871721906610600077E-16 ) ) ;
#82751 = CARTESIAN_POINT ( 'NONE',  ( -30.00000000000000000, 0.000000000000000000, 0.000000000000000000 ) ) ;
#82752 = CARTESIAN_POINT ( 'NONE',  ( 32.94994279514025948, 464.9549361168423047, 15.12478419437806210 ) ) ;
#82753 = CARTESIAN_POINT ( 'NONE',  ( 1.248878403638263412, 16.16541945263409019, -50.37088816262370727 ) ) ;
#82754 = ORIENTED_EDGE ( 'NONE', *, *, #67974, .T. ) ;
#82755 = B_SPLINE_CURVE_WITH_KNOTS ( 'NONE', 3,
 ( #43719, #3271, #37263, #102498, #60469, #4328, #36211, #94419, #52876, #19499, #70659, #53418, #103033, #103553, #70126, #93874, #93347, #68548 ),
 .UNSPECIFIED., .F., .F.,
 ( 4, 2, 2, 2, 2, 2, 2, 2, 4 ),
 ( 0.007125446813973600017, 0.007629686116325595964, 0.008133925418677592778, 0.008638164721029588725, 0.009142404023381584671, 0.009646643325733580618, 0.01015088262808557656, 0.01065512193043757251, 0.01115936123278956846 ),
 .UNSPECIFIED. ) ;
#82756 = CARTESIAN_POINT ( 'NONE',  ( 88.12498868022365173, -60.00000000000001421, -21.45487254486462447 ) ) ;
#82757 = CARTESIAN_POINT ( 'NONE',  ( -9.295423129716056110, 45.72519545954835962, 14.93632663516901893 ) ) ;
#82758 = CARTESIAN_POINT ( 'NONE',  ( -15.94660519413343813, -2.877896041580118691, 14.72412135074108619 ) ) ;
#82759 = DIRECTION ( 'NONE',  ( 0.5735764363510442720, -0.8191520442889930198, 1.003171929053526349E-16 ) ) ;
#82760 = VERTEX_POINT ( 'NONE', #77229 ) ;
#82761 = EDGE_CURVE ( 'NONE', #34748, #13321, #50281, .T. ) ;
#82762 = AXIS2_PLACEMENT_3D ( 'NONE', #12554, #95102, #91509 ) ;
#82763 = B_SPLINE_CURVE_WITH_KNOTS ( 'NONE', 3,
 ( #88905, #91574, #99644, #100703 ),
 .UNSPECIFIED., .F., .F.,
 ( 4, 4 ),
 ( 0.000000000000000000, 0.001455730951134404224 ),
 .UNSPECIFIED. ) ;
#82764 = CARTESIAN_POINT ( 'NONE',  ( -37.40675222085440055, 27.65931068607314458, 13.45617127781066458 ) ) ;
#82765 = EDGE_LOOP ( 'NONE', ( #5977, #95315, #91546, #40600, #22032, #99536 ) ) ;
#82766 = ORIENTED_EDGE ( 'NONE', *, *, #68601, .T. ) ;
#82767 = CARTESIAN_POINT ( 'NONE',  ( 7.999912353029502654, 81.00017529396907889, -0.2691822806795008405 ) ) ;
#82768 = SURFACE_STYLE_USAGE ( .BOTH. , #101618 ) ;
#82769 = DIRECTION ( 'NONE',  ( -0.000000000000000000, -0.000000000000000000, -1.000000000000000000 ) ) ;
#82770 = CARTESIAN_POINT ( 'NONE',  ( 80.97977184163765685, 1.030564683017419500E-14, 0.000000000000000000 ) ) ;
#82771 = CARTESIAN_POINT ( 'NONE',  ( 87.02528036306804893, -60.18762643930987366, -6.133291105691159650 ) ) ;
#82772 = CARTESIAN_POINT ( 'NONE',  ( -45.47616038644186176, 382.7747991321946301, 7.369568083445501294 ) ) ;
#82773 = CARTESIAN_POINT ( 'NONE',  ( -3.958687006365356975, -68.40474125555384433, 13.56240833589197514 ) ) ;
#82774 = CARTESIAN_POINT ( 'NONE',  ( 12.50000000000000711, 35.28456030440094793, -54.82782442755426189 ) ) ;
#82775 = ORIENTED_EDGE ( 'NONE', *, *, #62908, .T. ) ;
#82776 = CARTESIAN_POINT ( 'NONE',  ( -9.088874843304111550, 43.98892613297807230, 13.78954861775553731 ) ) ;
#82777 = ORIENTED_EDGE ( 'NONE', *, *, #20423, .F. ) ;
#82778 = ADVANCED_FACE ( 'NONE', ( #20648 ), #61598, .F. ) ;
#82779 = CARTESIAN_POINT ( 'NONE',  ( -7.421727621021489973, -3.000000000000118128, -70.37058875307404548 ) ) ;
#82780 = CARTESIAN_POINT ( 'NONE',  ( -51.98383481243817528, -38.33605321803858601, 73.39120586448642314 ) ) ;
#82781 = CARTESIAN_POINT ( 'NONE',  ( 43.00000000000000000, 464.8825480873695710, 15.07585856869435936 ) ) ;
#82783 = EDGE_LOOP ( 'NONE', ( #72884, #51315, #104708, #99167 ) ) ;
#82782 = CARTESIAN_POINT ( 'NONE',  ( -61.64506658729265354, -59.99999999999998579, 86.85893902245692288 ) ) ;
#82784 = CARTESIAN_POINT ( 'NONE',  ( 66.02827394672999617, -18.62689932795539960, 78.34043094791800854 ) ) ;
#82785 = ORIENTED_EDGE ( 'NONE', *, *, #24497, .T. ) ;
#82786 = CIRCLE ( 'NONE', #80995, 4.000000000000007105 ) ;
#82787 = CARTESIAN_POINT ( 'NONE',  ( -1.727368016638141196E-09, 38.95322581935191408, 63.66965480466879512 ) ) ;
#82788 = CARTESIAN_POINT ( 'NONE',  ( -7.188101187500000044, -22.90625000204838457, -8.802885111219163269E-16 ) ) ;
#82789 = CIRCLE ( 'NONE', #91430, 65.50000000000000000 ) ;
#82790 = CARTESIAN_POINT ( 'NONE',  ( -113.3221076330293471, -57.67118219814813784, 155.4948299128208191 ) ) ;
#82791 = ADVANCED_FACE ( 'NONE', ( #53487 ), #93417, .T. ) ;
#82792 = VERTEX_POINT ( 'NONE', #78808 ) ;
#82793 = AXIS2_PLACEMENT_3D ( 'NONE', #93706, #43553, #77520 ) ;
#82794 = SURFACE_STYLE_USAGE ( .BOTH. , #93011 ) ;
#82795 = LINE ( 'NONE', #75762, #24766 ) ;
#82796 = CARTESIAN_POINT ( 'NONE',  ( -37.62595466100607666, 491.2446780561959372, 12.18850516984483612 ) ) ;
#82797 = CIRCLE ( 'NONE', #81089, 6.999999999999999112 ) ;
#82798 = DIRECTION ( 'NONE',  ( 0.000000000000000000, -1.000000000000000000, 0.000000000000000000 ) ) ;
#82799 = CARTESIAN_POINT ( 'NONE',  ( 5.656854249492380582, -24.50000000409677270, -5.656854249492379694 ) ) ;
#82800 = DIRECTION ( 'NONE',  ( 0.000000000000000000, 0.000000000000000000, -1.000000000000000000 ) ) ;
#82801 = CARTESIAN_POINT ( 'NONE',  ( 23.15769230769230802, 1.411358822780289120E-15, 0.000000000000000000 ) ) ;
#82802 = CIRCLE ( 'NONE', #54984, 3.309500000000001663 ) ;
#82803 = CARTESIAN_POINT ( 'NONE',  ( 9.482945380845299255, 32.44333058778931189, 3.177595346755239802 ) ) ;
#82804 = CARTESIAN_POINT ( 'NONE',  ( 0.000000000000000000, 0.000000000000000000, 0.000000000000000000 ) ) ;
#82805 = CARTESIAN_POINT ( 'NONE',  ( 51.88291765282896506, 333.6183258647170646, 267.1969486012836228 ) ) ;
#82806 = CARTESIAN_POINT ( 'NONE',  ( -3.572352985694997152, 15.21714514899093018, -9.341953373613581135 ) ) ;
#82807 = ORIENTED_EDGE ( 'NONE', *, *, #49034, .F. ) ;
#82808 = DIRECTION ( 'NONE',  ( -1.000000000000000000, -1.224606353822377258E-16, -0.000000000000000000 ) ) ;
#82809 = SURFACE_STYLE_USAGE ( .BOTH. , #8909 ) ;
#82810 = CARTESIAN_POINT ( 'NONE',  ( 4.276117748942277252, -60.00000000000000711, 39.63074977821929679 ) ) ;
#82811 = CARTESIAN_POINT ( 'NONE',  ( -96.93821243838389989, -30.00000000000000000, 191.1029387296386517 ) ) ;
#82812 = EDGE_CURVE ( 'NONE', #80103, #51980, #41736, .T. ) ;
#82813 = ORIENTED_EDGE ( 'NONE', *, *, #10434, .F. ) ;
#82814 = CARTESIAN_POINT ( 'NONE',  ( 23.86650669486618881, 4.000000000000003553, 4.898587196589414801E-16 ) ) ;
#82815 = CARTESIAN_POINT ( 'NONE',  ( 70.82442282108941356, -57.68208708914901450, 160.7729576061657610 ) ) ;
#82816 = CONICAL_SURFACE ( 'NONE', #58733, 4.000000000000001776, 0.9599310885968808105 ) ;
#82818 = CARTESIAN_POINT ( 'NONE',  ( -9.896718155645521264, 7.425134178940658636, 1.133880678298145650 ) ) ;
#82817 = CARTESIAN_POINT ( 'NONE',  ( 3.313708498984762496, -15.96875000409677270, 7.999999999999998224 ) ) ;
#82819 = EDGE_CURVE ( 'NONE', #30981, #20310, #85324, .T. ) ;
#82820 = CARTESIAN_POINT ( 'NONE',  ( 5.331005461825221836, -21.69790887411561187, -38.54718089058046360 ) ) ;
#82821 = CARTESIAN_POINT ( 'NONE',  ( -7.500000000000000000, -4.330127018922203419, -0.9999999999999974465 ) ) ;
#82822 = CARTESIAN_POINT ( 'NONE',  ( -29.12862619358356753, -60.00000000000001421, 42.62327244784807334 ) ) ;
#82823 = CARTESIAN_POINT ( 'NONE',  ( 11.61253032626837189, 15.70682449265374458, 9.633805627537904925 ) ) ;
#82824 = CARTESIAN_POINT ( 'NONE',  ( 0.000000000000000000, 0.000000000000000000, 1.734723475976807094E-15 ) ) ;
#82825 = CARTESIAN_POINT ( 'NONE',  ( -86.89610268328752340, -35.42331563151877560, 187.9280089145808574 ) ) ;
#82826 = ADVANCED_FACE ( 'NONE', ( #4938 ), #63178, .T. ) ;
#82827 = ORIENTED_EDGE ( 'NONE', *, *, #88383, .T. ) ;
#82828 = CARTESIAN_POINT ( 'NONE',  ( 19.01558148378777346, 49.54233067771700405, 61.88543008400887402 ) ) ;
#82829 = CARTESIAN_POINT ( 'NONE',  ( 12.06828428419903076, -6.477429270778858772, 19.90153083308154081 ) ) ;
#82830 = CARTESIAN_POINT ( 'NONE',  ( -8.054587700577721776, -25.54953564508612729, 28.14066466568578662 ) ) ;
#82831 = CARTESIAN_POINT ( 'NONE',  ( -27.10511071441183262, -1.200000000000000030E-05, 8.806984339686158236 ) ) ;
#82832 = CARTESIAN_POINT ( 'NONE',  ( -41.60913992197761502, 468.1836805815477192, 17.09491368641011633 ) ) ;
#82834 = CARTESIAN_POINT ( 'NONE',  ( 3.350244361011366578, -68.60885486349103246, 13.06616826839196221 ) ) ;
#82833 = CARTESIAN_POINT ( 'NONE',  ( -102.1400935414211801, -60.00000000000002132, 193.9895109154659849 ) ) ;
#82835 = ORIENTED_EDGE ( 'NONE', *, *, #11335, .F. ) ;
#82836 = CIRCLE ( 'NONE', #36395, 4.000000000000000888 ) ;
#82837 = CARTESIAN_POINT ( 'NONE',  ( -37.88504238421052861, 463.4171042825119002, 19.90923349044181379 ) ) ;
#82838 = CARTESIAN_POINT ( 'NONE',  ( 15.76197929006133869, 34.59888885235105960, 23.83685467299613592 ) ) ;
#82839 = CARTESIAN_POINT ( 'NONE',  ( 29.01392623672715132, 306.7126468544000772, -9.132303470068400486 ) ) ;
#82840 = DIRECTION ( 'NONE',  ( -1.000000000000000000, -1.224606353822377258E-16, -0.000000000000000000 ) ) ;
#82841 = CARTESIAN_POINT ( 'NONE',  ( -6.928203230275508773, -84.73116675491002070, -4.000000000000002665 ) ) ;
#82842 = DIRECTION ( 'NONE',  ( 0.000000000000000000, 0.000000000000000000, 1.000000000000000000 ) ) ;
#82843 = CARTESIAN_POINT ( 'NONE',  ( 111.4777457387739048, -59.99999999999993605, 136.6117272317642630 ) ) ;
#82844 = ORIENTED_EDGE ( 'NONE', *, *, #47594, .F. ) ;
#82845 = CARTESIAN_POINT ( 'NONE',  ( 4.699999999999999289, 6.499999999999999112, 0.000000000000000000 ) ) ;
#82846 = CYLINDRICAL_SURFACE ( 'NONE', #98774, 8.000000000000000000 ) ;
#82847 =( LENGTH_UNIT ( ) NAMED_UNIT ( * ) SI_UNIT ( .MILLI., .METRE. ) );
#82848 = CARTESIAN_POINT ( 'NONE',  ( -33.71029056097432886, 485.0094969250626491, -0.6083101643363590938 ) ) ;
#82849 = EDGE_CURVE ( 'NONE', #72747, #21935, #105487, .T. ) ;
#82850 = CARTESIAN_POINT ( 'NONE',  ( 43.60687476841235366, 374.6170328897057402, 14.40570227514321466 ) ) ;
#82851 = CARTESIAN_POINT ( 'NONE',  ( 25.59999999999999787, 1.533819458162526451E-15, 0.000000000000000000 ) ) ;
#82852 = VERTEX_POINT ( 'NONE', #85878 ) ;
#82853 = UNCERTAINTY_MEASURE_WITH_UNIT (LENGTH_MEASURE( 1.000000000000000082E-05 ), #93826, 'distance_accuracy_value', 'NONE');
#82854 = AXIS2_PLACEMENT_3D ( 'NONE', #55735, #14756, #97276 ) ;
#82855 = AXIS2_PLACEMENT_3D ( 'NONE', #48663, #81548, #92 ) ;
#82856 = DIRECTION ( 'NONE',  ( 0.000000000000000000, 0.000000000000000000, -1.000000000000000000 ) ) ;
#82857 = ORIENTED_EDGE ( 'NONE', *, *, #40633, .T. ) ;
#82858 = AXIS2_PLACEMENT_3D ( 'NONE', #5570, #23376, #89152 ) ;
#82859 = SURFACE_SIDE_STYLE ('',( #105535 ) ) ;
#82860 = CARTESIAN_POINT ( 'NONE',  ( 16.00000000000006750, 2.437231117875682695, 5.694551215225515328 ) ) ;
#82861 = EDGE_CURVE ( 'NONE', #40039, #41445, #55489, .T. ) ;
#82862 = CARTESIAN_POINT ( 'NONE',  ( -64.32759900504490247, 48.00000000000000000, -11.06576400629244361 ) ) ;
#82863 = CARTESIAN_POINT ( 'NONE',  ( 4.999999999999960920, -12.67914701489953622, 11.71967441881639438 ) ) ;
#82864 = CARTESIAN_POINT ( 'NONE',  ( -40.15229402368767353, -60.00000000001941203, 56.59167717116910268 ) ) ;
#82865 = CONICAL_SURFACE ( 'NONE', #38171, 4.172000000000009479, 0.9599310885968813656 ) ;
#82866 = CARTESIAN_POINT ( 'NONE',  ( 43.91914608742546733, 435.5074579457412938, 9.837368328701776576 ) ) ;
#82867 = ORIENTED_EDGE ( 'NONE', *, *, #14177, .T. ) ;
#82868 = CARTESIAN_POINT ( 'NONE',  ( 98.90601695972424068, -60.00000000000001421, 74.53410781496819482 ) ) ;
#82870 = CARTESIAN_POINT ( 'NONE',  ( 15.48353078592144172, -29.03023710598939289, 28.89585879851779282 ) ) ;
#82869 = CARTESIAN_POINT ( 'NONE',  ( -71.69513722905418263, -59.99999999999990763, 172.8795092261717912 ) ) ;
#82871 = CARTESIAN_POINT ( 'NONE',  ( 37.71869766778865340, 461.3719613792328573, 2.612049572453471136 ) ) ;
#82873 = EDGE_CURVE ( 'NONE', #77549, #98888, #88513, .T. ) ;
#82872 = LINE ( 'NONE', #42406, #38001 ) ;
#82874 = CARTESIAN_POINT ( 'NONE',  ( -40.33321577437346406, -18.77737895441734040, 34.22531594715925252 ) ) ;
#82875 = CIRCLE ( 'NONE', #50147, 5.000000000000011546 ) ;
#82876 = CARTESIAN_POINT ( 'NONE',  ( 0.000000000000000000, 81.00000000000000000, 0.000000000000000000 ) ) ;
#82877 = ORIENTED_EDGE ( 'NONE', *, *, #89783, .F. ) ;
#82878 = DIRECTION ( 'NONE',  ( 0.000000000000000000, 0.000000000000000000, 1.000000000000000000 ) ) ;
#82879 = DIRECTION ( 'NONE',  ( 0.000000000000000000, -1.000000000000000000, 0.000000000000000000 ) ) ;
#82880 = CARTESIAN_POINT ( 'NONE',  ( 5.990573850131376332, -14.42843120744217877, 14.14171987952399512 ) ) ;
#82881 = CARTESIAN_POINT ( 'NONE',  ( 16.94582768995435984, 304.5649027789814909, -10.06098247776249188 ) ) ;
#82882 = CARTESIAN_POINT ( 'NONE',  ( -34.26359294763754093, 462.2983250974768339, 4.610187765825797257 ) ) ;
#82883 = ORIENTED_EDGE ( 'NONE', *, *, #21083, .T. ) ;
#82884 = CARTESIAN_POINT ( 'NONE',  ( 4.999999999999993783, -46.26205164319991070, 102.2532056550983128 ) ) ;
#82885 = CARTESIAN_POINT ( 'NONE',  ( 0.05458999538772667942, -1.264741368073333483, 6.499999999999999112 ) ) ;
#82886 = EDGE_LOOP ( 'NONE', ( #44129, #18757, #81630, #95629 ) ) ;
#82887 = CARTESIAN_POINT ( 'NONE',  ( 73.71532767159492039, -29.99999999990776445, 147.5689089691210540 ) ) ;
#82888 = CARTESIAN_POINT ( 'NONE',  ( 48.02835407290544367, 9.771516447483593382, 16.85535821593427386 ) ) ;
#82889 = DIRECTION ( 'NONE',  ( -1.000000000000000000, -1.224606353822377258E-16, -0.000000000000000000 ) ) ;
#82890 = DIRECTION ( 'NONE',  ( -1.000000000000000000, -1.224606353822377258E-16, -0.000000000000000000 ) ) ;
#82891 = CARTESIAN_POINT ( 'NONE',  ( 81.97453080922707613, -30.00000000000000000, 33.68671043929276010 ) ) ;
#82892 = CARTESIAN_POINT ( 'NONE',  ( 7.211357414135266986, 102.9885346006555551, 3.467230644691329911 ) ) ;
#82893 = ORIENTED_EDGE ( 'NONE', *, *, #91814, .T. ) ;
#82894 = EDGE_CURVE ( 'NONE', #8448, #24875, #49315, .T. ) ;
#82895 = AXIS2_PLACEMENT_3D ( 'NONE', #14365, #80701, #39216 ) ;
#82896 = VERTEX_POINT ( 'NONE', #105220 ) ;
#82897 = ORIENTED_EDGE ( 'NONE', *, *, #98895, .F. ) ;
#82898 = DIRECTION ( 'NONE',  ( 0.000000000000000000, 1.000000000000000000, 0.000000000000000000 ) ) ;
#82899 = CARTESIAN_POINT ( 'NONE',  ( 22.00881591061976650, 25.77023098277651414, 32.31265490242656568 ) ) ;
#82900 = CARTESIAN_POINT ( 'NONE',  ( -5.500000000000007994, 42.00000000000000000, -68.91429205818155879 ) ) ;
#82901 = AXIS2_PLACEMENT_3D ( 'NONE', #46400, #30773, #14532 ) ;
#82902 = CARTESIAN_POINT ( 'NONE',  ( -42.44404385065663377, 464.7189401834564819, 16.13499420399455175 ) ) ;
#82903 = CARTESIAN_POINT ( 'NONE',  ( -31.22166591873284958, 392.4860439548177169, 25.19642211891369499 ) ) ;
#82904 = FACE_OUTER_BOUND ( 'NONE', #77398, .T. ) ;
#82905 = ORIENTED_EDGE ( 'NONE', *, *, #29209, .F. ) ;
#82906 = CIRCLE ( 'NONE', #96688, 4.172000000000001485 ) ;
#82907 = VERTEX_POINT ( 'NONE', #40474 ) ;
#82908 = SURFACE_SIDE_STYLE ('',( #50003 ) ) ;
#82909 = CARTESIAN_POINT ( 'NONE',  ( 80.20710674972620779, -38.79645419531406958, 193.3540812050024158 ) ) ;
#82910 = FACE_OUTER_BOUND ( 'NONE', #66695, .T. ) ;
#82911 = CARTESIAN_POINT ( 'NONE',  ( 28.65390007077115797, 297.4029314509076016, 10.49725111039197145 ) ) ;
#82912 = DIRECTION ( 'NONE',  ( 0.5735764363510442720, -0.8191520442889930198, 1.003171929053526349E-16 ) ) ;
#82913 = CARTESIAN_POINT ( 'NONE',  ( -41.33517203638642457, 460.1869644147454892, 2.191757750720012776 ) ) ;
#82914 = CARTESIAN_POINT ( 'NONE',  ( 42.48134374264972735, 356.5879242656516226, 15.82646805172678661 ) ) ;
#82915 = CARTESIAN_POINT ( 'NONE',  ( 96.81745522565726958, -37.99999999999980815, 192.8977754549547967 ) ) ;
#82916 = AXIS2_PLACEMENT_3D ( 'NONE', #74124, #89273, #82222 ) ;
#82917 = SURFACE_STYLE_FILL_AREA ( #31733 ) ;
#82918 = ORIENTED_EDGE ( 'NONE', *, *, #11952, .T. ) ;
#82919 = CARTESIAN_POINT ( 'NONE',  ( -21.19348424345033521, 294.8901562694577478, 1.945151701991107540 ) ) ;
#82920 = DIRECTION ( 'NONE',  ( -0.9861333108788020718, 0.1659550938513554286, 0.000000000000000000 ) ) ;
#82921 = UNCERTAINTY_MEASURE_WITH_UNIT (LENGTH_MEASURE( 1.000000000000000082E-05 ), #8237, 'distance_accuracy_value', 'NONE');
#82922 = SURFACE_STYLE_USAGE ( .BOTH. , #33335 ) ;
#82923 = CARTESIAN_POINT ( 'NONE',  ( -7.777900015783948184, -4.169681370001537601, -7.928862157988302073 ) ) ;
#82924 = DIRECTION ( 'NONE',  ( 0.000000000000000000, -1.000000000000000000, 0.000000000000000000 ) ) ;
#82925 = CARTESIAN_POINT ( 'NONE',  ( 41.08349330513380693, 1.593028355512270567E-15, 0.000000000000000000 ) ) ;
#82926 = ORIENTED_EDGE ( 'NONE', *, *, #18362, .F. ) ;
#82927 = CARTESIAN_POINT ( 'NONE',  ( 13.37207953394533355, 5.000000000000002665, 0.000000000000000000 ) ) ;
#82928 = CARTESIAN_POINT ( 'NONE',  ( 85.16920355399095399, -46.56241956317034436, 187.9255957375985986 ) ) ;
#82929 =( LENGTH_UNIT ( ) NAMED_UNIT ( * ) SI_UNIT ( .MILLI., .METRE. ) );
#82930 =( NAMED_UNIT ( * ) SI_UNIT ( $, .STERADIAN. ) SOLID_ANGLE_UNIT ( ) );
#82931 = ORIENTED_EDGE ( 'NONE', *, *, #95168, .T. ) ;
#82932 = CARTESIAN_POINT ( 'NONE',  ( 91.38762156947538529, -57.66273077560735771, -20.33768330290320137 ) ) ;
#82933 = AXIS2_PLACEMENT_3D ( 'NONE', #19960, #35595, #68472 ) ;
#82934 = DIRECTION ( 'NONE',  ( 0.000000000000000000, -1.000000000000000000, 0.000000000000000000 ) ) ;
#82935 = DIRECTION ( 'NONE',  ( 0.000000000000000000, -1.000000000000000000, 0.000000000000000000 ) ) ;
#82936 =( BOUNDED_CURVE ( )  B_SPLINE_CURVE ( 2, ( #3251, #60449, #36722, #85225, #19479, #44244, #37244, #69587, #62043 ),
 .UNSPECIFIED., .F., .F. ) 
 B_SPLINE_CURVE_WITH_KNOTS ( ( 3, 2, 2, 2, 3 ),
 ( 0.8970588235294119084, 0.9044117647058824705, 0.9117647058823530326, 0.9191176470588235947, 0.9264705882352942679 ),
 .UNSPECIFIED. ) 
 CURVE ( )  GEOMETRIC_REPRESENTATION_ITEM ( )  RATIONAL_B_SPLINE_CURVE ( ( 0.9999999999999988898, 0.9238795325112878487, 1.000000000000000000, 0.9238795325112867385, 1.000000000000000000, 0.9238795325112867385, 1.000000000000000000, 0.9238795325112856283, 1.000000000000001110 ) ) 
 REPRESENTATION_ITEM ( '' )  );
#82937 = CARTESIAN_POINT ( 'NONE',  ( -81.36189305868806798, -30.00000000000000711, -1.402050496001596480 ) ) ;
#82938 = EDGE_CURVE ( 'NONE', #22959, #6669, #97116, .T. ) ;
#82939 = DIRECTION ( 'NONE',  ( 1.000000000000000000, 0.000000000000000000, 0.000000000000000000 ) ) ;
#82940 = PRESENTATION_LAYER_ASSIGNMENT (  '', '', ( #3741 ) ) ;
#82941 = CARTESIAN_POINT ( 'NONE',  ( 21.97272370781259099, 27.95363515319932191, -32.15429476237004280 ) ) ;
#82942 = DIRECTION ( 'NONE',  ( -0.5735764363510510444, -0.8191520442889883569, 0.000000000000000000 ) ) ;
#82944 = CARTESIAN_POINT ( 'NONE',  ( 0.000000000000000000, 1.502314598737159031E-15, -8.000000000000000000 ) ) ;
#82943 = CARTESIAN_POINT ( 'NONE',  ( -48.02835407290534420, -1.200000000000000030E-05, -16.85535821593460426 ) ) ;
#82945 = EDGE_CURVE ( 'NONE', #37313, #51545, #28008, .T. ) ;
#82946 = AXIS2_PLACEMENT_3D ( 'NONE', #84403, #24591, #8901 ) ;
#82947 = B_SPLINE_CURVE_WITH_KNOTS ( 'NONE', 3,
 ( #70197, #28715, #27662, #103105, #29254, #62135, #71767, #87983 ),
 .UNSPECIFIED., .F., .F.,
 ( 4, 2, 2, 4 ),
 ( 2.459764730735158427E-07, 0.001920659145285726066, 0.002880865729692052690, 0.003841072314098378879 ),
 .UNSPECIFIED. ) ;
#82948 = DIRECTION ( 'NONE',  ( 1.000000000000000000, 1.224606353822377258E-16, 0.000000000000000000 ) ) ;
#82949 = CARTESIAN_POINT ( 'NONE',  ( -28.43265695612109312, 17.35407036237647560, 40.99228818888992976 ) ) ;
#82950 = CARTESIAN_POINT ( 'NONE',  ( -12.50000000000000000, -3.000000000000000000, -9.904958390907868448 ) ) ;
#82951 = CARTESIAN_POINT ( 'NONE',  ( 4.472135954999578722, -84.86420795053444976, 4.000000000000001776 ) ) ;
#82952 = CARTESIAN_POINT ( 'NONE',  ( 21.84999999999999787, 1.533819458162526451E-15, 0.000000000000000000 ) ) ;
#82953 = FACE_OUTER_BOUND ( 'NONE', #30241, .T. ) ;
#82954 = DIRECTION ( 'NONE',  ( 0.000000000000000000, -1.000000000000000000, 0.000000000000000000 ) ) ;
#82955 = EDGE_CURVE ( 'NONE', #93124, #44948, #47499, .T. ) ;
#82956 = ORIENTED_EDGE ( 'NONE', *, *, #17362, .T. ) ;
#82957 = CARTESIAN_POINT ( 'NONE',  ( 29.83349330513380337, 1.593028355512270567E-15, 0.000000000000000000 ) ) ;
#82958 = FACE_OUTER_BOUND ( 'NONE', #90115, .T. ) ;
#82959 = CARTESIAN_POINT ( 'NONE',  ( -7.934996450857313199, 81.13137543527471962, -1.050865690281774123 ) ) ;
#82960 = CARTESIAN_POINT ( 'NONE',  ( -37.65422233906284077, -24.15452973042363638, -30.77166073587790507 ) ) ;
#82961 =( BOUNDED_SURFACE ( )  B_SPLINE_SURFACE ( 3, 2, ( 
 ( #43288, #43814, #67042 ),
 ( #10373, #51899, #76172 ),
 ( #50824, #75099, #19055 ),
 ( #19595, #51366, #2274 ),
 ( #76706, #35225, #27146 ),
 ( #84810, #33621, #84278 ),
 ( #1196, #66493, #99375 ),
 ( #17965, #34164, #27684 ),
 ( #11429, #99920, #92353 ),
 ( #26094, #92894, #91841 ),
 ( #10894, #1746, #44356 ),
 ( #35773, #83729, #68648 ),
 ( #101528, #9840, #52427 ),
 ( #60556, #58411, #91323 ),
 ( #85343, #68092, #75646 ),
 ( #67575, #34701, #18504 ),
 ( #9306, #59488, #50304 ),
 ( #100987, #100456, #60033 ),
 ( #26615, #77252, #21699 ),
 ( #53508, #54533, #29274 ),
 ( #4421, #77788, #87477 ),
 ( #61080, #38404, #14082 ),
 ( #45428, #95047, #36310 ),
 ( #62154, #96090, #36829 ),
 ( #63199, #104167, #71271 ),
 ( #54011, #30309, #69177 ),
 ( #12494, #52975, #4959 ),
 ( #21181, #22226, #85898 ),
 ( #69699, #37358, #46989 ),
 ( #46475, #103644, #78303 ),
 ( #37890, #86955, #70222 ),
 ( #28739, #102044, #20123 ),
 ( #13021, #103123, #93972 ),
 ( #45948, #78828, #70748 ),
 ( #3366, #29793, #102590 ),
 ( #5484, #11972, #55073 ),
 ( #62671, #95560, #13557 ),
 ( #79362, #88001, #44901 ),
 ( #20668, #3896, #28211 ),
 ( #61624, #94517, #86434 ),
 ( #47521, #5999, #38922 ),
 ( #90109, #97653, #106273 ),
 ( #71790, #73374, #16753 ),
 ( #7057, #98196, #105240 ),
 ( #41032, #80410, #79886 ),
 ( #40499, #65310, #39976 ),
 ( #48041, #96619, #89058 ),
 ( #31384, #104701, #15155 ),
 ( #97133, #6523, #49101 ),
 ( #57723, #105756, #24866 ),
 ( #80948, #64262, #24350 ),
 ( #32436, #22757, #57194 ),
 ( #39458, #73913, #23280 ),
 ( #48573, #16214, #30852 ),
 ( #56118, #98713, #89589 ),
 ( #7577, #72844, #31898 ),
 ( #72336, #55593, #64778 ),
 ( #23825, #82001, #88530 ) ),
 .UNSPECIFIED., .F., .F., .F. ) 
 B_SPLINE_SURFACE_WITH_KNOTS ( ( 4, 2, 2, 2, 2, 2, 2, 2, 2, 2, 2, 2, 2, 2, 2, 2, 2, 2, 2, 2, 2, 2, 2, 2, 2, 2, 2, 2, 4 ),
 ( 3, 3 ),
 ( 0.05905452279715409786, 0.05961352906526162787, 0.05989303219931539635, 0.05996290798282884194, 0.05999784587458556473, 0.06000658034752474196, 0.06001531482046391919, 0.06003278376634228058, 0.06017253533336916482, 0.06129054786958423873, 0.06240856040579931263, 0.06352657294201438654, 0.06464458547822946044, 0.06576259801444453434, 0.06799862308687466828, 0.07247067323173495001, 0.07694272337659524563, 0.08588682366631580911, 0.09483092395603638647, 0.1127191245354775273, 0.1306073251149186820, 0.1484955256943598367, 0.1663837262738009914, 0.1753278265635215549, 0.1842719268532421184, 0.1932160271429627096, 0.1976880772878230053, 0.1999241023602531531, 0.2021601274326832731 ),
 ( 0.000000000000000000, 1.000000000000000000 ),
 .UNSPECIFIED. ) 
 GEOMETRIC_REPRESENTATION_ITEM ( )  RATIONAL_B_SPLINE_SURFACE ( (
 ( 1.000000000000000000, 0.7071067811865475727, 1.000000000000000000),
 ( 1.000000000000000000, 0.7071067811865475727, 1.000000000000000000),
 ( 1.000000000000000000, 0.7071067811865475727, 1.000000000000000000),
 ( 1.000000000000000000, 0.7071067811865475727, 1.000000000000000000),
 ( 1.000000000000000000, 0.7071067811865475727, 1.000000000000000000),
 ( 1.000000000000000000, 0.7071067811865475727, 1.000000000000000000),
 ( 1.000000000000000000, 0.7071067811865475727, 1.000000000000000000),
 ( 1.000000000000000000, 0.7071067811865475727, 1.000000000000000000),
 ( 1.000000000000000000, 0.7071067811865475727, 1.000000000000000000),
 ( 1.000000000000000000, 0.7071067811865475727, 1.000000000000000000),
 ( 1.000000000000000000, 0.7071067811865475727, 1.000000000000000000),
 ( 1.000000000000000000, 0.7071067811865475727, 1.000000000000000000),
 ( 1.000000000000000000, 0.7071067811865475727, 1.000000000000000000),
 ( 1.000000000000000000, 0.7071067811865475727, 1.000000000000000000),
 ( 1.000000000000000000, 0.7071067811865475727, 1.000000000000000000),
 ( 1.000000000000000000, 0.7071067811865475727, 1.000000000000000000),
 ( 1.000000000000000000, 0.7071067811865475727, 1.000000000000000000),
 ( 1.000000000000000000, 0.7071067811865475727, 1.000000000000000000),
 ( 1.000000000000000000, 0.7071067811865474617, 1.000000000000000000),
 ( 1.000000000000000000, 0.7071067811865474617, 1.000000000000000000),
 ( 1.000000000000000000, 0.7071067811865475727, 1.000000000000000000),
 ( 1.000000000000000000, 0.7071067811865475727, 1.000000000000000000),
 ( 1.000000000000000000, 0.7071067811865475727, 1.000000000000000000),
 ( 1.000000000000000000, 0.7071067811865475727, 1.000000000000000000),
 ( 1.000000000000000000, 0.7071067811865475727, 1.000000000000000000),
 ( 1.000000000000000000, 0.7071067811865475727, 1.000000000000000000),
 ( 1.000000000000000000, 0.7071067811865474617, 1.000000000000000000),
 ( 1.000000000000000000, 0.7071067811865474617, 1.000000000000000000),
 ( 1.000000000000000000, 0.7071067811865475727, 1.000000000000000000),
 ( 1.000000000000000000, 0.7071067811865475727, 1.000000000000000000),
 ( 1.000000000000000000, 0.7071067811865475727, 1.000000000000000000),
 ( 1.000000000000000000, 0.7071067811865475727, 1.000000000000000000),
 ( 1.000000000000000000, 0.7071067811865475727, 1.000000000000000000),
 ( 1.000000000000000000, 0.7071067811865475727, 1.000000000000000000),
 ( 1.000000000000000000, 0.7071067811865474617, 1.000000000000000000),
 ( 1.000000000000000000, 0.7071067811865474617, 1.000000000000000000),
 ( 1.000000000000000000, 0.7071067811865475727, 1.000000000000000000),
 ( 1.000000000000000000, 0.7071067811865475727, 1.000000000000000000),
 ( 1.000000000000000000, 0.7071067811865474617, 1.000000000000000000),
 ( 1.000000000000000000, 0.7071067811865474617, 1.000000000000000000),
 ( 1.000000000000000000, 0.7071067811865475727, 1.000000000000000000),
 ( 1.000000000000000000, 0.7071067811865475727, 1.000000000000000000),
 ( 1.000000000000000000, 0.7071067811865474617, 1.000000000000000000),
 ( 1.000000000000000000, 0.7071067811865474617, 1.000000000000000000),
 ( 1.000000000000000000, 0.7071067811865475727, 1.000000000000000000),
 ( 1.000000000000000000, 0.7071067811865475727, 1.000000000000000000),
 ( 1.000000000000000000, 0.7071067811865475727, 1.000000000000000000),
 ( 1.000000000000000000, 0.7071067811865475727, 1.000000000000000000),
 ( 1.000000000000000000, 0.7071067811865475727, 1.000000000000000000),
 ( 1.000000000000000000, 0.7071067811865475727, 1.000000000000000000),
 ( 1.000000000000000000, 0.7071067811865473507, 1.000000000000000000),
 ( 1.000000000000000000, 0.7071067811865473507, 1.000000000000000000),
 ( 1.000000000000000000, 0.7071067811865475727, 1.000000000000000000),
 ( 1.000000000000000000, 0.7071067811865475727, 1.000000000000000000),
 ( 1.000000000000000000, 0.7071067811865475727, 1.000000000000000000),
 ( 1.000000000000000000, 0.7071067811865475727, 1.000000000000000000),
 ( 1.000000000000000000, 0.7071067811865475727, 1.000000000000000000),
 ( 1.000000000000000000, 0.7071067811865475727, 1.000000000000000000) ) ) 
 REPRESENTATION_ITEM ( '' )  SURFACE ( )  );
#82963 = DIRECTION ( 'NONE',  ( 0.000000000000000000, 0.000000000000000000, -1.000000000000000000 ) ) ;
#82962 = DIRECTION ( 'NONE',  ( -0.000000000000000000, 1.000000000000000000, -0.000000000000000000 ) ) ;
#82964 = EDGE_LOOP ( 'NONE', ( #20412, #48240, #23300, #36412 ) ) ;
#82965 = AXIS2_PLACEMENT_3D ( 'NONE', #56147, #89090, #57227 ) ;
#82966 = B_SPLINE_CURVE_WITH_KNOTS ( 'NONE', 3,
 ( #77620, #86263, #101363, #21022 ),
 .UNSPECIFIED., .F., .F.,
 ( 4, 4 ),
 ( 0.002500010780266304685, 0.005000000000000250772 ),
 .UNSPECIFIED. ) ;
#82967 = ORIENTED_EDGE ( 'NONE', *, *, #79768, .T. ) ;
#82968 = CARTESIAN_POINT ( 'NONE',  ( -26.94600335556788195, 34.81407801978571825, 7.556984339686089847 ) ) ;
#82969 = CIRCLE ( 'NONE', #36524, 0.5000000000000004441 ) ;
#82970 = CARTESIAN_POINT ( 'NONE',  ( 38.50925662097987612, 490.3066386719625598, 12.08729337933079862 ) ) ;
#82971 =( LENGTH_UNIT ( ) NAMED_UNIT ( * ) SI_UNIT ( .MILLI., .METRE. ) );
#82972 = CARTESIAN_POINT ( 'NONE',  ( -88.71913443814118239, -60.00000000000000711, -20.71346367143210188 ) ) ;
#82973 = VERTEX_POINT ( 'NONE', #72315 ) ;
#82974 = DIRECTION ( 'NONE',  ( 0.000000000000000000, 0.000000000000000000, 1.000000000000000000 ) ) ;
#82975 = CARTESIAN_POINT ( 'NONE',  ( 15.51004476304982838, 2.604548209198465525, 0.4043569039159928269 ) ) ;
#82976 = CARTESIAN_POINT ( 'NONE',  ( 101.5940187986382028, -52.72865695923380969, 192.6689692413239641 ) ) ;
#82978 = CARTESIAN_POINT ( 'NONE',  ( -47.07197767030570645, 13.48831169381985084, 14.79015211622733084 ) ) ;
#82977 = CARTESIAN_POINT ( 'NONE',  ( 33.06001105660368466, -32.07477916797628126, 32.97354630382984197 ) ) ;
#82979 = ORIENTED_EDGE ( 'NONE', *, *, #15996, .F. ) ;
#82980 = ORIENTED_EDGE ( 'NONE', *, *, #3329, .T. ) ;
#82981 = VERTEX_POINT ( 'NONE', #31367 ) ;
#82982 = CARTESIAN_POINT ( 'NONE',  ( 30.85676804175761845, 345.5934757462927109, 18.44563300946912321 ) ) ;
#82983 = CARTESIAN_POINT ( 'NONE',  ( 14.83349330513380337, 4.000000000000003553, 0.000000000000000000 ) ) ;
#82984 = CARTESIAN_POINT ( 'NONE',  ( 16.02938566285138222, 45.83159863292936365, 6.508120059605595920 ) ) ;
#82985 = ORIENTED_EDGE ( 'NONE', *, *, #64930, .T. ) ;
#82986 = EDGE_CURVE ( 'NONE', #85106, #1566, #2140, .T. ) ;
#82987 = DIRECTION ( 'NONE',  ( -0.000000000000000000, -0.000000000000000000, 1.000000000000000000 ) ) ;
#82988 = DIRECTION ( 'NONE',  ( -1.000000000000000000, 0.000000000000000000, 0.000000000000000000 ) ) ;
#82989 = LINE ( 'NONE', #57625, #106369 ) ;
#82990 = CARTESIAN_POINT ( 'NONE',  ( -24.14082041284044422, -57.67406494483144286, 42.97874410022470215 ) ) ;
#82991 = CARTESIAN_POINT ( 'NONE',  ( -2.977408999572650039, -33.68750000204839523, -7.188101187500001821 ) ) ;
#82992 = CARTESIAN_POINT ( 'NONE',  ( -29.77121734509604778, 18.16596778899117126, 39.60535821593506967 ) ) ;
#82993 = CARTESIAN_POINT ( 'NONE',  ( -26.54817876223620488, 310.6276912632132507, 11.31208242866018132 ) ) ;
#82994 = CARTESIAN_POINT ( 'NONE',  ( 5.000000000000000000, 6.123233995736766282E-16, -4.289342857142857568 ) ) ;
#82995 = CARTESIAN_POINT ( 'NONE',  ( -89.32121524059635931, -30.00000000000006750, 17.90039431539770121 ) ) ;
#82996 = EDGE_CURVE ( 'NONE', #39650, #5290, #89275, .T. ) ;
#82998 = ADVANCED_FACE ( 'NONE', ( #15663 ), #16196, .T. ) ;
#82997 = FACE_OUTER_BOUND ( 'NONE', #94616, .T. ) ;
#82999 = CARTESIAN_POINT ( 'NONE',  ( -50.59602062303963521, -22.19444373152758132, 45.92958069296322776 ) ) ;
#83000 = DIRECTION ( 'NONE',  ( 0.000000000000000000, 1.000000000000000000, 0.000000000000000000 ) ) ;
#83001 = VERTEX_POINT ( 'NONE', #501 ) ;
#83002 = CARTESIAN_POINT ( 'NONE',  ( -95.99521439327702410, -37.68773228063575687, 192.9684156188939994 ) ) ;
#83003 = CARTESIAN_POINT ( 'NONE',  ( -5.833922283738917969, 294.7609306416122195, -8.134666899072025004 ) ) ;
#83004 = CARTESIAN_POINT ( 'NONE',  ( 9.960411669762633480, -2.966372377354413281, 15.28833013202438451 ) ) ;
#83005 = ORIENTED_EDGE ( 'NONE', *, *, #71779, .T. ) ;
#83006 = CARTESIAN_POINT ( 'NONE',  ( -17.76478578597574298, 34.19219417800617578, -23.79420372548796436 ) ) ;
#83007 = CARTESIAN_POINT ( 'NONE',  ( 105.0832242103311103, -38.39226450554996717, 197.4063297836361812 ) ) ;
#83008 = CARTESIAN_POINT ( 'NONE',  ( -6.318250223874061420E-16, 9.147862274876551680, -8.047472243342934206 ) ) ;
#83009 = CARTESIAN_POINT ( 'NONE',  ( -6.388374826136157481, 51.65551423085587857, -6.604895695859905658 ) ) ;
#83010 = CIRCLE ( 'NONE', #24463, 5.000000000000010658 ) ;
#83011 = CARTESIAN_POINT ( 'NONE',  ( 31.08349330513380693, -4.000000000000000000, 4.898587196589415787E-16 ) ) ;
#83012 = PRESENTATION_STYLE_ASSIGNMENT (( #25894 ) ) ;
#83014 = CARTESIAN_POINT ( 'NONE',  ( 79.60966642660856962, -30.00000000000000711, 132.5630840557917054 ) ) ;
#83013 = UNCERTAINTY_MEASURE_WITH_UNIT (LENGTH_MEASURE( 1.000000000000000082E-05 ), #44311, 'distance_accuracy_value', 'NONE');
#83015 = AXIS2_PLACEMENT_3D ( 'NONE', #74889, #66827, #25887 ) ;
#83016 = CARTESIAN_POINT ( 'NONE',  ( 35.31256682049291840, 491.0612481437107704, 12.05460915451404880 ) ) ;
#83017 = CARTESIAN_POINT ( 'NONE',  ( -28.46830025707812339, 12.99948816575241395, 40.55052036360838486 ) ) ;
#83018 = CARTESIAN_POINT ( 'NONE',  ( -0.9999999999999943379, 0.000000000000000000, 101.0455488498966758 ) ) ;
#83019 = EDGE_CURVE ( 'NONE', #52034, #30747, #79614, .T. ) ;
#83020 = VERTEX_POINT ( 'NONE', #49625 ) ;
#83021 = ORIENTED_EDGE ( 'NONE', *, *, #3109, .F. ) ;
#83022 = CARTESIAN_POINT ( 'NONE',  ( 52.60578561560112831, -60.30795294419101538, 63.32323424420151525 ) ) ;
#83023 = FACE_OUTER_BOUND ( 'NONE', #74243, .T. ) ;
#83024 = AXIS2_PLACEMENT_3D ( 'NONE', #54726, #38076, #55260 ) ;
#83025 = DIRECTION ( 'NONE',  ( -1.000000000000000000, -1.224606353822377258E-16, -0.000000000000000000 ) ) ;
#83026 = ADVANCED_FACE ( 'NONE', ( #82533 ), #10226, .T. ) ;
#83027 = MECHANICAL_DESIGN_GEOMETRIC_PRESENTATION_REPRESENTATION (  '', ( #39916 ), #69276 ) ;
#83028 = ORIENTED_EDGE ( 'NONE', *, *, #21689, .T. ) ;
#83029 = CARTESIAN_POINT ( 'NONE',  ( -99.77955803787557443, -38.35585648701670891, 87.15852475401679555 ) ) ;
#83030 = VERTEX_POINT ( 'NONE', #10747 ) ;
#83031 = CARTESIAN_POINT ( 'NONE',  ( 109.4400761579602630, -38.35602592254275578, 149.2467366083292291 ) ) ;
#83032 = CARTESIAN_POINT ( 'NONE',  ( 13.79606237849683126, 22.99914945738909111, -0.5248391107339340778 ) ) ;
#83033 = CARTESIAN_POINT ( 'NONE',  ( 89.14633145472258491, -52.71673259819623070, 57.40858558930295885 ) ) ;
#83034 = SURFACE_SIDE_STYLE ('',( #66313 ) ) ;
#83035 = CARTESIAN_POINT ( 'NONE',  ( 5.974456367264334036E-20, 45.30391365246044444, -18.75000000000000355 ) ) ;
#83036 = CARTESIAN_POINT ( 'NONE',  ( -28.16657779764221203, 308.8746777916272777, -8.086782216783561239 ) ) ;
#83037 = ADVANCED_FACE ( 'NONE', ( #25393 ), #13304, .T. ) ;
#83038 = CARTESIAN_POINT ( 'NONE',  ( 74.01235824150077747, -59.99999999999999289, 172.3450624796163595 ) ) ;
#83039 = CARTESIAN_POINT ( 'NONE',  ( 17.60121130357612174, 45.00000000000000000, 63.09853793600694871 ) ) ;
#83040 = ORIENTED_EDGE ( 'NONE', *, *, #68691, .F. ) ;
#83041 = CARTESIAN_POINT ( 'NONE',  ( 61.54115679619849288, -46.43610433826334827, 79.75840819081285815 ) ) ;
#83042 = CARTESIAN_POINT ( 'NONE',  ( -20.49977525862255945, 302.8459220885800960, -10.00124997875688670 ) ) ;
#83043 = CARTESIAN_POINT ( 'NONE',  ( 0.08415458823012109124, 37.21016666119768246, 27.24999999999999645 ) ) ;
#83044 = CIRCLE ( 'NONE', #67578, 4.000000000000001776 ) ;
#83045 = DIRECTION ( 'NONE',  ( -1.000000000000000000, -1.224606353822377258E-16, -0.000000000000000000 ) ) ;
#83047 = CARTESIAN_POINT ( 'NONE',  ( -36.10664099193432719, 485.3877008568640008, -3.396001134007734290 ) ) ;
#83046 = CARTESIAN_POINT ( 'NONE',  ( -87.97678914366765923, -38.37031391392313395, -19.61794280459611528 ) ) ;
#83048 = CARTESIAN_POINT ( 'NONE',  ( -31.66192239831772071, 329.0498789714471854, 16.34307995493717769 ) ) ;
#83049 = CARTESIAN_POINT ( 'NONE',  ( -32.82334337205544017, 485.9852583078038606, 5.593860717071749811 ) ) ;
#83050 = CARTESIAN_POINT ( 'NONE',  ( -10.00000000000000355, 15.00000000000000000, -10.00000000000000000 ) ) ;
#83051 = CARTESIAN_POINT ( 'NONE',  ( 8.000000000000000000, -27.40625000000000000, -3.313708498984761608 ) ) ;
#83052 = AXIS2_PLACEMENT_3D ( 'NONE', #49718, #98273, #9250 ) ;
#83053 = EDGE_CURVE ( 'NONE', #76724, #12840, #21159, .T. ) ;
#83054 = CIRCLE ( 'NONE', #58727, 4.000000000000000888 ) ;
#83055 = B_SPLINE_CURVE_WITH_KNOTS ( 'NONE', 3,
 ( #62405, #54268, #86692, #30047, #55338, #61346, #71009, #45684, #88268, #78562, #70492, #46734, #95300, #94237, #53245, #95828, #14347, #12234, #103902, #45164 ),
 .UNSPECIFIED., .F., .F.,
 ( 4, 2, 2, 2, 2, 2, 2, 2, 2, 4 ),
 ( 0.006350122368084452386, 0.006854238585709724989, 0.007358354803334996724, 0.007610412912147635628, 0.007862471020960272797, 0.008366587238585540195, 0.008870703456210805860, 0.009374819673836073258, 0.009878935891461340657, 0.01038305210908660806 ),
 .UNSPECIFIED. ) ;
#83056 = DIRECTION ( 'NONE',  ( -1.000000000000000000, -1.224606353822377258E-16, -0.000000000000000000 ) ) ;
#83057 = ORIENTED_EDGE ( 'NONE', *, *, #34555, .T. ) ;
#83058 = CARTESIAN_POINT ( 'NONE',  ( 82.18972579398030121, -57.13749140910870494, 185.7775781806303428 ) ) ;
#83059 = CARTESIAN_POINT ( 'NONE',  ( 30.00000000000000000, 490.5636507777048791, 7.413185101890151785 ) ) ;
#83060 = DIRECTION ( 'NONE',  ( -1.000000000000000000, -0.000000000000000000, -0.000000000000000000 ) ) ;
#83061 = ORIENTED_EDGE ( 'NONE', *, *, #75906, .F. ) ;
#83062 = CYLINDRICAL_SURFACE ( 'NONE', #53211, 5.000000000000002665 ) ;
#83063 = CARTESIAN_POINT ( 'NONE',  ( 9.256208135396892800, -5.000000000000000888, -17.97305361429082993 ) ) ;
#83064 = DIRECTION ( 'NONE',  ( 0.000000000000000000, 0.000000000000000000, 1.000000000000000000 ) ) ;
#83065 = CARTESIAN_POINT ( 'NONE',  ( -16.85537930133409645, -24.70995007397846166, -38.51870997018118459 ) ) ;
#83066 = EDGE_CURVE ( 'NONE', #35120, #96476, #64160, .T. ) ;
#83067 = CARTESIAN_POINT ( 'NONE',  ( 53.64466222910518667, -60.00000000000000711, 81.43429093339135250 ) ) ;
#83068 = CARTESIAN_POINT ( 'NONE',  ( 46.00000000000000000, 488.3725375423206287, 3.127739281036224117 ) ) ;
#83069 = CARTESIAN_POINT ( 'NONE',  ( 10.39041109297083842, -13.86547299437372693, 31.87393420377066633 ) ) ;
#83070 = EDGE_CURVE ( 'NONE', #457, #73090, #64802, .T. ) ;
#83072 = CARTESIAN_POINT ( 'NONE',  ( -13.42014485437181825, 24.46368817018429453, -2.390721932681278084 ) ) ;
#83071 = CARTESIAN_POINT ( 'NONE',  ( -24.90621635141948076, -28.97586686355563401, 38.24361932259525787 ) ) ;
#83073 = ADVANCED_FACE ( 'NONE', ( #52276 ), #95188, .T. ) ;
#83074 = CARTESIAN_POINT ( 'NONE',  ( -5.082755093536325042, -11.09375000204838457, -5.082755093536325930 ) ) ;
#83075 = DIRECTION ( 'NONE',  ( -0.000000000000000000, -0.000000000000000000, -1.000000000000000000 ) ) ;
#83076 = ADVANCED_FACE ( 'NONE', ( #103498 ), #5343, .T. ) ;
#83077 = EDGE_LOOP ( 'NONE', ( #19788, #98830, #88493, #99738 ) ) ;
#83078 = ADVANCED_FACE ( 'NONE', ( #104550 ), #26323, .F. ) ;
#83079 = AXIS2_PLACEMENT_3D ( 'NONE', #9686, #1041, #42596 ) ;
#83080 = CARTESIAN_POINT ( 'NONE',  ( -19.23735690889347794, 49.80931112121790250, 61.48632125443229057 ) ) ;
#83081 = EDGE_CURVE ( 'NONE', #8054, #55679, #62467, .T. ) ;
#83082 =( LENGTH_UNIT ( ) NAMED_UNIT ( * ) SI_UNIT ( .MILLI., .METRE. ) );
#83083 = MECHANICAL_DESIGN_GEOMETRIC_PRESENTATION_REPRESENTATION (  '', ( #24601 ), #102100 ) ;
#83084 = DIRECTION ( 'NONE',  ( 0.000000000000000000, -1.000000000000000000, 0.000000000000000000 ) ) ;
#83086 = CARTESIAN_POINT ( 'NONE',  ( 43.48352109543510835, -21.77010373675058474, -26.80878052041629900 ) ) ;
#83085 = CARTESIAN_POINT ( 'NONE',  ( 23.15769230769230802, -4.171999999999999709, 0.000000000000000000 ) ) ;
#83087 = VERTEX_POINT ( 'NONE', #39835 ) ;
#83088 = CARTESIAN_POINT ( 'NONE',  ( -4.589357672516646502, -86.06206030977220678, -3.865585121226772891 ) ) ;
#83089 = DIRECTION ( 'NONE',  ( 0.000000000000000000, -1.000000000000000000, 0.000000000000000000 ) ) ;
#83090 = ORIENTED_EDGE ( 'NONE', *, *, #79500, .F. ) ;
#83091 = SURFACE_STYLE_USAGE ( .BOTH. , #17313 ) ;
#83092 =( NAMED_UNIT ( * ) PLANE_ANGLE_UNIT ( ) SI_UNIT ( $, .RADIAN. ) );
#83093 = CARTESIAN_POINT ( 'NONE',  ( -19.56509672771084141, 41.86698933908479603, -80.29965057802650108 ) ) ;
#83094 = CARTESIAN_POINT ( 'NONE',  ( -103.7206433085268884, -60.00000000000000000, 102.8025343256433075 ) ) ;
#83095 = DIRECTION ( 'NONE',  ( -1.000000000000000000, 0.000000000000000000, 0.000000000000000000 ) ) ;
#83096 = CARTESIAN_POINT ( 'NONE',  ( -43.74985542820371620, 435.5770091380364306, 16.96136490515579354 ) ) ;
#83097 = CARTESIAN_POINT ( 'NONE',  ( 31.21759734847655210, 387.2566916973277671, 24.99345285570965913 ) ) ;
#83099 = CARTESIAN_POINT ( 'NONE',  ( -15.51004476305004864, 2.604548209197934838, -0.4043569039035935786 ) ) ;
#83098 = CARTESIAN_POINT ( 'NONE',  ( -34.05377138046417684, 435.1042973066813033, 11.34048742922945685 ) ) ;
#83100 = CARTESIAN_POINT ( 'NONE',  ( -83.36631949438019262, -39.47759878546305856, 173.2594340369611814 ) ) ;
#83101 = ORIENTED_EDGE ( 'NONE', *, *, #37880, .F. ) ;
#83102 = DIRECTION ( 'NONE',  ( -0.000000000000000000, -0.000000000000000000, 1.000000000000000000 ) ) ;
#83103 = ORIENTED_EDGE ( 'NONE', *, *, #68476, .T. ) ;
#83104 = ORIENTED_EDGE ( 'NONE', *, *, #49995, .T. ) ;
#83105 = DIRECTION ( 'NONE',  ( 0.000000000000000000, -1.000000000000000000, 0.000000000000000000 ) ) ;
#83106 = CARTESIAN_POINT ( 'NONE',  ( -10.00000000000000355, 15.00000000000000000, -10.00000000000000000 ) ) ;
#83107 = ORIENTED_EDGE ( 'NONE', *, *, #31133, .F. ) ;
#83108 = CARTESIAN_POINT ( 'NONE',  ( -16.53376292628442812, 304.5679863953762947, 9.876672385353252537 ) ) ;
#83109 = CARTESIAN_POINT ( 'NONE',  ( 58.18888888888888999, 6.915964383211875250E-15, 0.000000000000000000 ) ) ;
#83110 = FACE_OUTER_BOUND ( 'NONE', #41260, .T. ) ;
#83111 = DIRECTION ( 'NONE',  ( -1.000000000000000000, -1.224606353822377258E-16, -0.000000000000000000 ) ) ;
#83112 =( GEOMETRIC_REPRESENTATION_CONTEXT ( 3 ) GLOBAL_UNCERTAINTY_ASSIGNED_CONTEXT ( ( #93411 ) ) GLOBAL_UNIT_ASSIGNED_CONTEXT ( ( #46948, #5957, #24830 ) ) REPRESENTATION_CONTEXT ( 'NONE', 'WORKASPACE' ) );
#83113 = DIRECTION ( 'NONE',  ( 0.000000000000000000, -1.000000000000000000, 0.000000000000000000 ) ) ;
#83114 = DIRECTION ( 'NONE',  ( 0.000000000000000000, 1.000000000000000000, 0.000000000000000000 ) ) ;
#83115 = CARTESIAN_POINT ( 'NONE',  ( -96.81748461682487061, -38.00000000001091394, 192.8978395531862020 ) ) ;
#83116 = CARTESIAN_POINT ( 'NONE',  ( 106.9110190588319540, -14.21045842199441367, 176.0591306608180844 ) ) ;
#83117 =( BOUNDED_SURFACE ( )  B_SPLINE_SURFACE ( 3, 2, ( 
 ( #88135, #80018, #31512 ),
 ( #6129, #39060, #71940 ),
 ( #104844, #64394, #27548 ),
 ( #37221, #78171, #59890 ) ),
 .UNSPECIFIED., .F., .F., .F. ) 
 B_SPLINE_SURFACE_WITH_KNOTS ( ( 4, 4 ),
 ( 3, 3 ),
 ( 0.01114851999725509704, 0.01303042415393934096 ),
 ( 0.000000000000000000, 0.8381935999574059437 ),
 .UNSPECIFIED. ) 
 GEOMETRIC_REPRESENTATION_ITEM ( )  RATIONAL_B_SPLINE_SURFACE ( (
 ( 1.000000000000000000, 0.8031285674522142815, 0.9362898844564289114),
 ( 1.000000000000000000, 0.7874857493404847641, 0.9312276682860687327),
 ( 1.000000000000000000, 0.7712021973814140452, 0.9259581024412611994),
 ( 1.000000000000000000, 0.7544987785202109665, 0.9205526622925915836) ) ) 
 REPRESENTATION_ITEM ( '' )  SURFACE ( )  );
#83118 = EDGE_CURVE ( 'NONE', #34066, #88975, #14162, .T. ) ;
#83119 = CARTESIAN_POINT ( 'NONE',  ( -112.8607363433238930, -60.00000000000000000, 189.7948125560051551 ) ) ;
#83120 = CARTESIAN_POINT ( 'NONE',  ( -58.58645841253417075, -32.54820420886014176, 65.51623946639922735 ) ) ;
#83121 = EDGE_LOOP ( 'NONE', ( #65723, #47710, #17197, #47402, #106077, #103745 ) ) ;
#83122 = CARTESIAN_POINT ( 'NONE',  ( 22.84345602534879660, 38.95245093555178073, 59.50021660759410480 ) ) ;
#83123 = CARTESIAN_POINT ( 'NONE',  ( 95.12578209733513290, -60.00000000000000000, 29.82219071690604295 ) ) ;
#83124 = EDGE_LOOP ( 'NONE', ( #97583, #38115, #62713, #90886, #50132, #43679 ) ) ;
#83125 = CARTESIAN_POINT ( 'NONE',  ( 2.989533877731477496, -25.54823926333440198, 28.14318220232473777 ) ) ;
#83126 = CARTESIAN_POINT ( 'NONE',  ( -104.8017842743203119, -52.71024585296110132, 161.0970186293872075 ) ) ;
#83127 = CARTESIAN_POINT ( 'NONE',  ( 4.401442555609581635E-16, -14.65625000204838457, -7.188101187500000044 ) ) ;
#83128 = MECHANICAL_DESIGN_GEOMETRIC_PRESENTATION_REPRESENTATION (  '', ( #55467 ), #17700 ) ;
#83129 = CARTESIAN_POINT ( 'NONE',  ( 17.50000000000000711, 2.500000000000000444, 25.00000000000000000 ) ) ;
#83130 = CARTESIAN_POINT ( 'NONE',  ( -10.45288716919457528, 45.35420570811798768, 15.39944944803833415 ) ) ;
#83131 = ORIENTED_EDGE ( 'NONE', *, *, #96302, .F. ) ;
#83132 = CARTESIAN_POINT ( 'NONE',  ( -6.750000000000015099, -11.69134295108991495, 0.000000000000000000 ) ) ;
#83133 = CARTESIAN_POINT ( 'NONE',  ( -70.37085192190031080, -60.00000000000000000, 143.4956404103314753 ) ) ;
#83134 = CARTESIAN_POINT ( 'NONE',  ( -4.284822031655025398, -1.092833614412312304, 104.4267991316944517 ) ) ;
#83135 = CARTESIAN_POINT ( 'NONE',  ( 4.401442555609581635E-16, -20.65625000204838813, -7.188101187500000044 ) ) ;
#83136 = DIRECTION ( 'NONE',  ( 0.000000000000000000, 1.000000000000000000, 0.000000000000000000 ) ) ;
#83137 = CARTESIAN_POINT ( 'NONE',  ( 16.64348903516523848, -1.200000000000000030E-05, 6.657797401561421857 ) ) ;
#83138 = CARTESIAN_POINT ( 'NONE',  ( 1.113440987313467412, 0.000000000000000000, 17.01589776168603763 ) ) ;
#83139 = CARTESIAN_POINT ( 'NONE',  ( 13.50000000000000533, 1.319989657865596744, -12.97199716660744961 ) ) ;
#83140 = LINE ( 'NONE', #57782, #101954 ) ;
#83141 = ADVANCED_FACE ( 'NONE', ( #7432 ), #5556, .T. ) ;
#83142 = CARTESIAN_POINT ( 'NONE',  ( 10.87267833667801398, -11.19338281451489081, 9.987533465452024473 ) ) ;
#83143 = CARTESIAN_POINT ( 'NONE',  ( -30.81186653459094416, 298.3092085573109671, -1.237150650991206025 ) ) ;
#83144 = CARTESIAN_POINT ( 'NONE',  ( 86.47130672191026690, -60.00000000000002132, 2.175088770990013742 ) ) ;
#83145 = CARTESIAN_POINT ( 'NONE',  ( -31.19799008952052333, -42.96357907512983587, 34.19655186448147788 ) ) ;
#83146 = CARTESIAN_POINT ( 'NONE',  ( -3.054195049253744187, -49.15491390355075652, 104.0345731970081147 ) ) ;
#83147 = CARTESIAN_POINT ( 'NONE',  ( 46.29580480807258169, -39.52690699740247027, 45.26178483514620865 ) ) ;
#83148 = CARTESIAN_POINT ( 'NONE',  ( 75.51533756583152979, -30.00000000000000355, -27.33238513093788669 ) ) ;
#83149 = EDGE_LOOP ( 'NONE', ( #9681, #79665, #104267, #44036, #24765, #54600, #46325, #18884 ) ) ;
#83150 = CARTESIAN_POINT ( 'NONE',  ( 43.80952869898890611, 434.9438303799720984, 12.65470026211498400 ) ) ;
#83151 = ADVANCED_FACE ( 'NONE', ( #73226 ), #38848, .F. ) ;
#83152 = CARTESIAN_POINT ( 'NONE',  ( -78.18292533485022489, -38.59614680129968889, 188.7774352412195924 ) ) ;
#83153 = ORIENTED_EDGE ( 'NONE', *, *, #45856, .F. ) ;
#83155 = SURFACE_SIDE_STYLE ('',( #50254 ) ) ;
#83154 = DIRECTION ( 'NONE',  ( -0.000000000000000000, -1.000000000000000000, -0.000000000000000000 ) ) ;
#83156 = CARTESIAN_POINT ( 'NONE',  ( 28.94718799180013491, -60.00000000000001421, 36.29242255566038722 ) ) ;
#83157 = CARTESIAN_POINT ( 'NONE',  ( -48.15203510316950286, 9.493368196138860071, -16.85535821593460781 ) ) ;
#83158 = DIRECTION ( 'NONE',  ( 0.000000000000000000, 1.000000000000000000, 0.000000000000000000 ) ) ;
#83159 = CARTESIAN_POINT ( 'NONE',  ( 38.51502786939645517, 460.0233756673477501, 2.043034587343977027 ) ) ;
#83160 = CARTESIAN_POINT ( 'NONE',  ( 0.5805565836007582359, 3.752776749732553263, -6.499999999999999112 ) ) ;
#83162 = CARTESIAN_POINT ( 'NONE',  ( -29.50104258278691205, 324.7387376422711895, 13.83862620216122075 ) ) ;
#83161 = AXIS2_PLACEMENT_3D ( 'NONE', #51146, #74883, #50094 ) ;
#83163 = CARTESIAN_POINT ( 'NONE',  ( 17.62344211657773485, 45.49768958935467822, 4.615364168318392579 ) ) ;
#83164 = EDGE_CURVE ( 'NONE', #29736, #70305, #76148, .T. ) ;
#83165 = CARTESIAN_POINT ( 'NONE',  ( 103.6184096593837722, -60.00000000000000000, 102.2032741284876209 ) ) ;
#83167 = CARTESIAN_POINT ( 'NONE',  ( 63.07777777777777573, 3.309500000000014541, 0.000000000000000000 ) ) ;
#83166 = CIRCLE ( 'NONE', #14317, 4.000000000000000888 ) ;
#83168 = EDGE_LOOP ( 'NONE', ( #46681, #2174, #98486, #56786, #11870 ) ) ;
#83169 = CARTESIAN_POINT ( 'NONE',  ( -93.04034664274190902, -30.00000000000006040, 191.1271326182357768 ) ) ;
#83170 = ORIENTED_EDGE ( 'NONE', *, *, #29325, .T. ) ;
#83171 = CARTESIAN_POINT ( 'NONE',  ( 25.99487131622766611, 37.06902177658768238, -9.387104646514996986 ) ) ;
#83172 = DIRECTION ( 'NONE',  ( 0.000000000000000000, 0.000000000000000000, 1.000000000000000000 ) ) ;
#83173 = DIRECTION ( 'NONE',  ( -1.000000000000000000, -1.224606353822377258E-16, -0.000000000000000000 ) ) ;
#83174 = CARTESIAN_POINT ( 'NONE',  ( 9.843039827103243766, 26.40916497491665993, -1.781495459429551786 ) ) ;
#83175 = MECHANICAL_DESIGN_GEOMETRIC_PRESENTATION_REPRESENTATION (  '', ( #102109 ), #17742 ) ;
#83176 = CARTESIAN_POINT ( 'NONE',  ( -7.188101187500001821, -17.37500000204838813, -2.977408999572651371 ) ) ;
#83177 = DIRECTION ( 'NONE',  ( 0.000000000000000000, 1.000000000000000000, 0.000000000000000000 ) ) ;
#83178 = PRODUCT_RELATED_PRODUCT_CATEGORY ( 'part', '', ( #70009 ) ) ;
#83179 = CARTESIAN_POINT ( 'NONE',  ( 32.33349330513379982, 1.593028355512270567E-15, 0.000000000000000000 ) ) ;
#83180 = ORIENTED_EDGE ( 'NONE', *, *, #87389, .F. ) ;
#83181 = CARTESIAN_POINT ( 'NONE',  ( 82.36683156209987544, -36.02441109180747958, 158.6170004785897447 ) ) ;
#83182 = CARTESIAN_POINT ( 'NONE',  ( 36.36650669486618881, 1.474610560812782335E-15, 0.000000000000000000 ) ) ;
#83183 = CARTESIAN_POINT ( 'NONE',  ( 9.253500431420432548, 86.29771549917710161, 3.792688295761950101 ) ) ;
#83184 = VERTEX_POINT ( 'NONE', #31235 ) ;
#83185 = SURFACE_STYLE_USAGE ( .BOTH. , #100429 ) ;
#83186 = DIRECTION ( 'NONE',  ( -1.000000000000000000, -0.000000000000000000, -0.000000000000000000 ) ) ;
#83187 = DIRECTION ( 'NONE',  ( 0.000000000000000000, 0.000000000000000000, 1.000000000000000000 ) ) ;
#83188 = CARTESIAN_POINT ( 'NONE',  ( -4.696906829037965636, 251.4399814748788913, -3.734050370377318018 ) ) ;
#83189 = CARTESIAN_POINT ( 'NONE',  ( -28.34860985744511908, 309.9008460147075539, 11.61304566638001390 ) ) ;
#83190 = CARTESIAN_POINT ( 'NONE',  ( -10.00000000000000355, 85.00000000000000000, 0.000000000000000000 ) ) ;
#83191 = ORIENTED_EDGE ( 'NONE', *, *, #70882, .F. ) ;
#83192 =( GEOMETRIC_REPRESENTATION_CONTEXT ( 3 ) GLOBAL_UNCERTAINTY_ASSIGNED_CONTEXT ( ( #100971 ) ) GLOBAL_UNIT_ASSIGNED_CONTEXT ( ( #35881, #33731, #58529 ) ) REPRESENTATION_CONTEXT ( 'NONE', 'WORKASPACE' ) );
#83193 =( LENGTH_UNIT ( ) NAMED_UNIT ( * ) SI_UNIT ( .MILLI., .METRE. ) );
#83194 = TOROIDAL_SURFACE ( 'NONE', #50454, 7.500000000000006217, 5.000000000000000000 ) ;
#83195 = DIRECTION ( 'NONE',  ( 0.000000000000000000, 0.000000000000000000, 1.000000000000000000 ) ) ;
#83196 = CARTESIAN_POINT ( 'NONE',  ( -5.000000000000000000, -65.47006268292325615, 15.04566776836145614 ) ) ;
#83197 = CARTESIAN_POINT ( 'NONE',  ( 14.87336202480038594, 23.06736695052138586, 1.011328272294861996 ) ) ;
#83198 = EDGE_CURVE ( 'NONE', #20836, #10763, #382, .T. ) ;
#83199 = CARTESIAN_POINT ( 'NONE',  ( 0.7840960880508188735, 34.26388638539432918, -29.48703832395431235 ) ) ;
#83200 = CARTESIAN_POINT ( 'NONE',  ( 7.188101187500000044, -34.15625000204838813, 0.000000000000000000 ) ) ;
#83201 = CARTESIAN_POINT ( 'NONE',  ( 0.000000000000000000, 0.000000000000000000, 15.00000000000000178 ) ) ;
#83202 = DIRECTION ( 'NONE',  ( 1.000000000000000000, 0.000000000000000000, 0.000000000000000000 ) ) ;
#83203 = CARTESIAN_POINT ( 'NONE',  ( 33.59806029755767298, 439.5207550827159366, 23.94543542408109005 ) ) ;
#83204 = ITEM_DEFINED_TRANSFORMATION ( 'NONE', 'NONE', #64500,  #10728 ) ;
#83205 = CARTESIAN_POINT ( 'NONE',  ( -9.333079356992103115, 31.77833080074871930, 3.592383266237781037 ) ) ;
#83206 = VERTEX_POINT ( 'NONE', #71641 ) ;
#83207 = DIRECTION ( 'NONE',  ( -1.000000000000000000, 0.000000000000000000, 0.000000000000000000 ) ) ;
#83208 = EDGE_CURVE ( 'NONE', #100031, #91474, #82763, .T. ) ;
#83209 = FILL_AREA_STYLE_COLOUR ( '', #82468 ) ;
#83210 = ADVANCED_FACE ( 'NONE', ( #96997 ), #17157, .T. ) ;
#83211 = FILL_AREA_STYLE ('',( #32573 ) ) ;
#83212 = ORIENTED_EDGE ( 'NONE', *, *, #75812, .T. ) ;
#83213 = CARTESIAN_POINT ( 'NONE',  ( 46.00000000000000000, 488.0491671480462514, 1.813224401588382717 ) ) ;
#83214 = ADVANCED_FACE ( 'NONE', ( #9031 ), #51079, .T. ) ;
#83215 = CARTESIAN_POINT ( 'NONE',  ( 88.48689482502902592, -5.000000000000000000, 0.000000000000000000 ) ) ;
#83216 = CARTESIAN_POINT ( 'NONE',  ( 114.0018284431585158, -57.67125466430193370, 179.4230632101373430 ) ) ;
#83217 = CARTESIAN_POINT ( 'NONE',  ( 33.72113281714197797, 434.9249850380938369, 12.79200524501336034 ) ) ;
#83218 = CARTESIAN_POINT ( 'NONE',  ( 3.177920610046286676, 15.40997900102463625, 6.239175027651493011 ) ) ;
#83219 = DIRECTION ( 'NONE',  ( 0.5735764363510468256, 0.8191520442889913545, 0.000000000000000000 ) ) ;
#83220 = DIRECTION ( 'NONE',  ( 1.000000000000000000, 0.000000000000000000, 0.000000000000000000 ) ) ;
#83221 = CARTESIAN_POINT ( 'NONE',  ( -79.47475843766400772, -59.99999999999999289, 195.3002843663804242 ) ) ;
#83222 =( GEOMETRIC_REPRESENTATION_CONTEXT ( 3 ) GLOBAL_UNCERTAINTY_ASSIGNED_CONTEXT ( ( #64275 ) ) GLOBAL_UNIT_ASSIGNED_CONTEXT ( ( #17440, #50308, #62024 ) ) REPRESENTATION_CONTEXT ( 'NONE', 'WORKASPACE' ) );
#83223 = CARTESIAN_POINT ( 'NONE',  ( 9.956455291700471832, 43.33337594337394449, -15.37426330073998315 ) ) ;
#83224 = CARTESIAN_POINT ( 'NONE',  ( 92.53532739719321398, 1.030564683017419500E-14, 0.000000000000000000 ) ) ;
#83225 = CARTESIAN_POINT ( 'NONE',  ( -39.24156521425334176, 307.7088117867400001, -7.003459073692002157 ) ) ;
#83226 = CARTESIAN_POINT ( 'NONE',  ( -86.15886759315432641, -21.41452658127618491, 176.4203065748977792 ) ) ;
#83227 = CIRCLE ( 'NONE', #102174, 1.000000000000009326 ) ;
#83228 = VERTEX_POINT ( 'NONE', #9561 ) ;
#83229 = CARTESIAN_POINT ( 'NONE',  ( -5.290067270632268226, 54.20842449845686417, -6.031152949374520844 ) ) ;
#83230 = CIRCLE ( 'NONE', #97013, 10.00000000000000000 ) ;
#83231 = ORIENTED_EDGE ( 'NONE', *, *, #6227, .F. ) ;
#83232 = CARTESIAN_POINT ( 'NONE',  ( -7.986452802927061612, -13.97309757691886922, 0.5332468218996361253 ) ) ;
#83233 = CARTESIAN_POINT ( 'NONE',  ( -5.596957125887390028, -2.684245481662593580, 103.9718581041641698 ) ) ;
#83234 = CARTESIAN_POINT ( 'NONE',  ( -85.72908938792220113, -52.74455777896098141, -8.197128046888657593 ) ) ;
#83235 = CARTESIAN_POINT ( 'NONE',  ( -4.837657582855711347, -12.04835165414239739, -8.962574246965099078 ) ) ;
#83236 = CARTESIAN_POINT ( 'NONE',  ( -16.32324275503853883, 43.86644259902494980, 4.188645491725135450 ) ) ;
#83237 = CIRCLE ( 'NONE', #50513, 0.5000000000000004441 ) ;
#83238 = DIRECTION ( 'NONE',  ( 1.000000000000000000, 1.224606353822377258E-16, 0.000000000000000000 ) ) ;
#83239 = CARTESIAN_POINT ( 'NONE',  ( -33.38752815995437828, 464.7252609253681612, 16.46839106284949494 ) ) ;
#83240 = CARTESIAN_POINT ( 'NONE',  ( 88.20421627925426833, 42.00000000000000000, 23.70422451874904013 ) ) ;
#83241 = CARTESIAN_POINT ( 'NONE',  ( 9.797174393178835518E-16, 81.00000000000000000, 8.000000000000007105 ) ) ;
#83242 = DIRECTION ( 'NONE',  ( 0.000000000000000000, 0.4999999999999996114, -0.8660254037844388186 ) ) ;
#83243 = EDGE_CURVE ( 'NONE', #100740, #8098, #92085, .T. ) ;
#83244 = CARTESIAN_POINT ( 'NONE',  ( 40.74889026577078965, -14.21045842199439591, -34.22240887780809260 ) ) ;
#83245 = CARTESIAN_POINT ( 'NONE',  ( -66.38286384437266463, -53.39006811827730559, 97.96284202452183365 ) ) ;
#83246 = ORIENTED_EDGE ( 'NONE', *, *, #15844, .F. ) ;
#83247 = CARTESIAN_POINT ( 'NONE',  ( 57.89978660429063240, -59.99999999999999289, 101.6248911977562699 ) ) ;
#83248 = CARTESIAN_POINT ( 'NONE',  ( 6.944371705245973025, 85.53899691424548735, -3.972324460300564297 ) ) ;
#83249 = CARTESIAN_POINT ( 'NONE',  ( 112.9340808439821586, -57.67120886779220257, 187.7003644414459416 ) ) ;
#83250 = ORIENTED_EDGE ( 'NONE', *, *, #11628, .F. ) ;
#83251 = DIRECTION ( 'NONE',  ( 0.000000000000000000, 0.000000000000000000, 1.000000000000000000 ) ) ;
#83252 = LINE ( 'NONE', #50873, #45996 ) ;
#83253 = VERTEX_POINT ( 'NONE', #98577 ) ;
#83254 = DIRECTION ( 'NONE',  ( -0.8191520442889884679, 1.003171929053520679E-16, 0.5735764363510509334 ) ) ;
#83255 =( GEOMETRIC_REPRESENTATION_CONTEXT ( 3 ) GLOBAL_UNCERTAINTY_ASSIGNED_CONTEXT ( ( #25767 ) ) GLOBAL_UNIT_ASSIGNED_CONTEXT ( ( #98562, #90486, #81834 ) ) REPRESENTATION_CONTEXT ( 'NONE', 'WORKASPACE' ) );
#83256 = CARTESIAN_POINT ( 'NONE',  ( 32.05241217997335212, 487.5077369494006803, 9.813907492612683470 ) ) ;
#83257 = DIRECTION ( 'NONE',  ( 0.000000000000000000, 1.000000000000000000, 0.000000000000000000 ) ) ;
#83258 = CARTESIAN_POINT ( 'NONE',  ( 2.977408999572650927, -14.37500000204838635, -7.188101187500001821 ) ) ;
#83259 = CARTESIAN_POINT ( 'NONE',  ( -0.04606493828583509142, -9.175055303659565453, -8.057411785091796119 ) ) ;
#83260 =( BOUNDED_SURFACE ( )  B_SPLINE_SURFACE ( 3, 3, ( 
 ( #42593, #37074, #86148, #67421 ),
 ( #45667, #37612, #43137, #78029 ),
 ( #102838, #70476, #100298, #29005 ),
 ( #61331, #94219, #59325, #102302 ),
 ( #92198, #78551, #50658, #4679 ),
 ( #103372, #12218, #18351, #99771 ) ),
 .UNSPECIFIED., .F., .F., .T. ) 
 B_SPLINE_SURFACE_WITH_KNOTS ( ( 4, 1, 1, 4 ),
 ( 4, 4 ),
 ( 0.000000000000000000, 0.4213833399777465738, 0.5213833399777465516, 0.9843640123765011740 ),
 ( 0.000000000000000000, 1.000000000000000000 ),
 .UNSPECIFIED. ) 
 GEOMETRIC_REPRESENTATION_ITEM ( )  RATIONAL_B_SPLINE_SURFACE ( (
 ( 1.000000000000000000, 0.3333333333333334259, 0.3333333333333334259, 1.000000000000000000),
 ( 1.000000000000000000, 0.3333333333333334259, 0.3333333333333334259, 1.000000000000000000),
 ( 1.000000000000000000, 0.3333333333333334259, 0.3333333333333334259, 1.000000000000000000),
 ( 1.000000000000000000, 0.3333333333333334259, 0.3333333333333334259, 1.000000000000000000),
 ( 1.000000000000000000, 0.3333333333333334259, 0.3333333333333334259, 1.000000000000000000),
 ( 1.000000000000000000, 0.3333333333333334259, 0.3333333333333334259, 1.000000000000000000) ) ) 
 REPRESENTATION_ITEM ( '' )  SURFACE ( )  );
#83261 = VECTOR ( 'NONE', #68735, 999.9999999999998863 ) ;
#83262 = CARTESIAN_POINT ( 'NONE',  ( 25.05982991920904723, -4.285714285714296246, -3.301565691951509063 ) ) ;
#83263 = DIRECTION ( 'NONE',  ( 0.000000000000000000, 0.000000000000000000, 1.000000000000000000 ) ) ;
#83264 = SURFACE_SIDE_STYLE ('',( #98898 ) ) ;
#83265 = CARTESIAN_POINT ( 'NONE',  ( -12.34835181856066555, -4.332967528434497062, -12.86601580078907148 ) ) ;
#83266 = UNCERTAINTY_MEASURE_WITH_UNIT (LENGTH_MEASURE( 1.000000000000000082E-05 ), #35376, 'distance_accuracy_value', 'NONE');
#83267 = MECHANICAL_DESIGN_GEOMETRIC_PRESENTATION_REPRESENTATION (  '', ( #2341 ), #105658 ) ;
#83268 = AXIS2_PLACEMENT_3D ( 'NONE', #82267, #49360, #105490 ) ;
#83269 = ORIENTED_EDGE ( 'NONE', *, *, #32719, .T. ) ;
#83270 = CARTESIAN_POINT ( 'NONE',  ( -7.404343286415054237, 40.29318263988768223, -70.39067260838145046 ) ) ;
#83271 = AXIS2_PLACEMENT_3D ( 'NONE', #106234, #57159, #90071 ) ;
#83272 = CARTESIAN_POINT ( 'NONE',  ( 32.48479210146626173, -32.55386965233949326, 32.82066705911088178 ) ) ;
#83273 = CARTESIAN_POINT ( 'NONE',  ( 32.70880207180495347, 321.7209935153538254, -4.878524035375318313 ) ) ;
#83274 = VERTEX_POINT ( 'NONE', #106668 ) ;
#83275 = CARTESIAN_POINT ( 'NONE',  ( 66.00571552735603120, 4.000000000000014211, 0.000000000000000000 ) ) ;
#83276 = EDGE_LOOP ( 'NONE', ( #9887, #12017, #50079, #87461 ) ) ;
#83278 =( LENGTH_UNIT ( ) NAMED_UNIT ( * ) SI_UNIT ( .MILLI., .METRE. ) );
#83277 = DIRECTION ( 'NONE',  ( 0.000000000000000000, -1.000000000000000000, 0.000000000000000000 ) ) ;
#83279 = CARTESIAN_POINT ( 'NONE',  ( 4.966176485634622217, 41.64999999999998437, -70.47555195150158625 ) ) ;
#83280 = CARTESIAN_POINT ( 'NONE',  ( -17.36371387429518975, 302.5953826724242504, -10.05438065605093456 ) ) ;
#83281 = CARTESIAN_POINT ( 'NONE',  ( 5.000000000000000000, 6.123233995736766282E-16, -0.02540000000000007530 ) ) ;
#83282 = CARTESIAN_POINT ( 'NONE',  ( -37.04971407824218943, 463.3105192861251567, 20.11836016812711492 ) ) ;
#83283 = ORIENTED_EDGE ( 'NONE', *, *, #16924, .F. ) ;
#83284 = EDGE_CURVE ( 'NONE', #75985, #86116, #29839, .T. ) ;
#83285 = CARTESIAN_POINT ( 'NONE',  ( 87.61970871457796761, -60.00000000000001421, -22.01029353022440915 ) ) ;
#83286 = CARTESIAN_POINT ( 'NONE',  ( 32.87547266101578458, 465.6993878536675879, 10.91512469976459343 ) ) ;
#83287 = CARTESIAN_POINT ( 'NONE',  ( 29.99999999999923972, 464.1662643419747951, 12.90481041407959673 ) ) ;
#83288 = DIRECTION ( 'NONE',  ( -1.000000000000000000, -1.224606353822377258E-16, -0.000000000000000000 ) ) ;
#83289 = ADVANCED_FACE ( 'NONE', ( #32817 ), #17681, .T. ) ;
#83290 = DIRECTION ( 'NONE',  ( -0.000000000000000000, -0.000000000000000000, -1.000000000000000000 ) ) ;
#83291 = ORIENTED_EDGE ( 'NONE', *, *, #67531, .F. ) ;
#83292 = FACE_OUTER_BOUND ( 'NONE', #73822, .T. ) ;
#83293 = ORIENTED_EDGE ( 'NONE', *, *, #70545, .F. ) ;
#83294 = EDGE_LOOP ( 'NONE', ( #95214, #51797, #30547, #102233 ) ) ;
#83295 = CARTESIAN_POINT ( 'NONE',  ( 6.928203230275510549, 84.73473843067414180, 4.000000000000000000 ) ) ;
#83296 = CARTESIAN_POINT ( 'NONE',  ( 6.169949891408691656, -6.308465495018314328, -2.073417244831073258 ) ) ;
#83297 = CARTESIAN_POINT ( 'NONE',  ( -16.18668061311517548, 35.07678708169574122, -21.93884963083486284 ) ) ;
#83298 = FACE_OUTER_BOUND ( 'NONE', #18864, .T. ) ;
#83299 = CARTESIAN_POINT ( 'NONE',  ( 87.01069706264078718, -60.18282985975657340, -5.594890968212038018 ) ) ;
#83300 = CARTESIAN_POINT ( 'NONE',  ( -40.81016822426350643, 312.4315563144064072, -5.816209787523243691 ) ) ;
#83301 = CARTESIAN_POINT ( 'NONE',  ( -18.59880227178827994, 304.6205263575372442, -9.049159319796237000 ) ) ;
#83302 = FACE_OUTER_BOUND ( 'NONE', #38308, .T. ) ;
#83303 = ORIENTED_EDGE ( 'NONE', *, *, #94304, .T. ) ;
#83304 = CARTESIAN_POINT ( 'NONE',  ( 6.500000000000000000, 3.453380256388234759, -0.6809028088495799880 ) ) ;
#83305 = ORIENTED_EDGE ( 'NONE', *, *, #56204, .F. ) ;
#83306 = DIRECTION ( 'NONE',  ( 0.000000000000000000, -1.000000000000000000, 0.000000000000000000 ) ) ;
#83307 = CARTESIAN_POINT ( 'NONE',  ( 4.284822031654944574, -48.90716638558773610, 104.4267991316944943 ) ) ;
#83308 = PRESENTATION_LAYER_ASSIGNMENT (  '', '', ( #52346 ) ) ;
#83310 = ORIENTED_EDGE ( 'NONE', *, *, #32310, .F. ) ;
#83309 = CARTESIAN_POINT ( 'NONE',  ( 6.488158982472050695, 51.34994349244383471, 7.647142150206464706 ) ) ;
#83311 = CARTESIAN_POINT ( 'NONE',  ( 76.80106626567913963, -49.90288268850643760, 137.4826183850342716 ) ) ;
#83312 = MECHANICAL_DESIGN_GEOMETRIC_PRESENTATION_REPRESENTATION (  '', ( #24743 ), #86801 ) ;
#83313 = ADVANCED_FACE ( 'NONE', ( #50028, #18225 ), #42468, .T. ) ;
#83314 = VERTEX_POINT ( 'NONE', #34950 ) ;
#83315 = CARTESIAN_POINT ( 'NONE',  ( 17.50000000000002487, 48.46901212408400283, 64.09337290743147264 ) ) ;
#83316 = CARTESIAN_POINT ( 'NONE',  ( 2.977408999572652260, -26.93750000204838457, 7.188101187500000044 ) ) ;
#83317 = CARTESIAN_POINT ( 'NONE',  ( -93.58432581829866592, -57.65368546899212987, -15.63533335066522767 ) ) ;
#83318 = ORIENTED_EDGE ( 'NONE', *, *, #68349, .T. ) ;
#83319 = CARTESIAN_POINT ( 'NONE',  ( 0.000000000000000000, 0.000000000000000000, -3.725171428571429022 ) ) ;
#83320 = CARTESIAN_POINT ( 'NONE',  ( 105.1047905290744069, -52.71716997988711029, 165.8147597789577219 ) ) ;
#83321 = CARTESIAN_POINT ( 'NONE',  ( -36.81712109022876689, 27.89045283345510740, -13.21917306905795009 ) ) ;
#83322 = DIRECTION ( 'NONE',  ( 0.000000000000000000, -1.000000000000000000, 0.000000000000000000 ) ) ;
#83323 = CARTESIAN_POINT ( 'NONE',  ( -8.000000000000001776, -25.34375000409676915, 3.313708498984758943 ) ) ;
#83324 = CARTESIAN_POINT ( 'NONE',  ( 0.000000000000000000, 5.629165124598847214, -3.250000000000007550 ) ) ;
#83325 = CARTESIAN_POINT ( 'NONE',  ( -36.32890656491792214, 26.02848181329492405, 12.39893532009519816 ) ) ;
#83326 = CARTESIAN_POINT ( 'NONE',  ( -7.439139359426217624, 41.00331351352566145, -59.84461297751296627 ) ) ;
#83327 = FACE_OUTER_BOUND ( 'NONE', #106469, .T. ) ;
#83328 = CARTESIAN_POINT ( 'NONE',  ( -7.093721425956736049, 304.7303285792975771, 9.911179277710184365 ) ) ;
#83329 = CARTESIAN_POINT ( 'NONE',  ( 51.88291765283140933, 268.1183258647170646, 182.1969486012845891 ) ) ;
#83330 = CARTESIAN_POINT ( 'NONE',  ( -3.979266480701241449, -30.00000000000000000, -6.940132439339150139 ) ) ;
#83331 = VERTEX_POINT ( 'NONE', #58120 ) ;
#83332 = CARTESIAN_POINT ( 'NONE',  ( 44.19067352157695439, 435.2576879214440169, 14.58866310346203576 ) ) ;
#83333 = DIRECTION ( 'NONE',  ( 0.000000000000000000, -1.000000000000000000, 0.000000000000000000 ) ) ;
#83334 = EDGE_CURVE ( 'NONE', #41772, #49495, #64239, .T. ) ;
#83335 = DIRECTION ( 'NONE',  ( 0.000000000000000000, -1.000000000000000000, -0.000000000000000000 ) ) ;
#83336 = CARTESIAN_POINT ( 'NONE',  ( -85.73097066636680097, -30.00000000000000355, 176.6817774525824802 ) ) ;
#83337 = EDGE_CURVE ( 'NONE', #64798, #48477, #46654, .T. ) ;
#83338 =( GEOMETRIC_REPRESENTATION_CONTEXT ( 3 ) GLOBAL_UNCERTAINTY_ASSIGNED_CONTEXT ( ( #18702 ) ) GLOBAL_UNIT_ASSIGNED_CONTEXT ( ( #68023, #41016, #8105 ) ) REPRESENTATION_CONTEXT ( 'NONE', 'WORKASPACE' ) );
#83339 = VECTOR ( 'NONE', #52935, 1000.000000000000000 ) ;
#83340 = EDGE_LOOP ( 'NONE', ( #79870, #72529, #56486, #102672 ) ) ;
#83341 = PLANE ( 'NONE',  #18621 ) ;
#83342 = CARTESIAN_POINT ( 'NONE',  ( 71.53995275910023111, -57.67933612627984274, 167.4204919677856651 ) ) ;
#83343 = EDGE_CURVE ( 'NONE', #35284, #98286, #12542, .T. ) ;
#83345 = CARTESIAN_POINT ( 'NONE',  ( -9.999999999999982236, 7.499999999999973355, 0.000000000000000000 ) ) ;
#83344 = SURFACE_STYLE_FILL_AREA ( #100589 ) ;
#83346 = CARTESIAN_POINT ( 'NONE',  ( 14.71715038006082565, -23.98991972335265999, -38.53165203909080105 ) ) ;
#83347 = CARTESIAN_POINT ( 'NONE',  ( -7.499999999999999112, -2.930060224340427677, -0.4701183149080218060 ) ) ;
#83348 = CARTESIAN_POINT ( 'NONE',  ( 32.28552837373269568, 464.7648866755952213, 15.30384310833107975 ) ) ;
#83349 = CARTESIAN_POINT ( 'NONE',  ( -38.20449057446243302, -60.00000000000000000, 49.74468476614604384 ) ) ;
#83350 = CARTESIAN_POINT ( 'NONE',  ( 0.000000000000000000, -3.035766082959412415E-15, 0.000000000000000000 ) ) ;
#83351 = CARTESIAN_POINT ( 'NONE',  ( 0.5680901257217666478, 45.34938084280606319, -18.61657585049056962 ) ) ;
#83352 = CARTESIAN_POINT ( 'NONE',  ( -86.01546372622856040, -53.81628179863218975, 191.9611049542646128 ) ) ;
#83353 = ORIENTED_EDGE ( 'NONE', *, *, #58055, .F. ) ;
#83354 = CARTESIAN_POINT ( 'NONE',  ( 8.000000000000000000, -12.49999999999999289, 0.000000000000000000 ) ) ;
#83355 = CARTESIAN_POINT ( 'NONE',  ( -9.379110170255547274, -56.88425848943947472, 33.37437879445704425 ) ) ;
#83356 = CARTESIAN_POINT ( 'NONE',  ( -6.786616733794231138, 41.72678875807561383, -59.11526074045958268 ) ) ;
#83357 = SURFACE_STYLE_FILL_AREA ( #42369 ) ;
#83359 = CARTESIAN_POINT ( 'NONE',  ( 2.762373655041346687, -70.28365225073746103, 13.27352019214896828 ) ) ;
#83358 = CARTESIAN_POINT ( 'NONE',  ( -39.62985215079022083, 316.5869118491702920, 7.204194025685374037 ) ) ;
#83360 = ORIENTED_EDGE ( 'NONE', *, *, #44908, .T. ) ;
#83362 = SURFACE_STYLE_FILL_AREA ( #82298 ) ;
#83361 =( GEOMETRIC_REPRESENTATION_CONTEXT ( 3 ) GLOBAL_UNCERTAINTY_ASSIGNED_CONTEXT ( ( #63211 ) ) GLOBAL_UNIT_ASSIGNED_CONTEXT ( ( #27598, #67489, #43205 ) ) REPRESENTATION_CONTEXT ( 'NONE', 'WORKASPACE' ) );
#83363 = CARTESIAN_POINT ( 'NONE',  ( -5.882666732301543355, -4.999999999999851674, -15.34024587939825857 ) ) ;
#83364 = CARTESIAN_POINT ( 'NONE',  ( -6.928203230275512325, 30.26930929695538808, -3.999999999999999112 ) ) ;
#83365 = CARTESIAN_POINT ( 'NONE',  ( 36.07978899617289414, 302.6969447429428897, -8.217629260179846185 ) ) ;
#83366 = CARTESIAN_POINT ( 'NONE',  ( 53.29999999999999716, 6.915964383211875250E-15, 0.000000000000000000 ) ) ;
#83367 = CARTESIAN_POINT ( 'NONE',  ( 6.849999999999999645, 0.000000000000000000, 0.000000000000000000 ) ) ;
#83368 =( NAMED_UNIT ( * ) SI_UNIT ( $, .STERADIAN. ) SOLID_ANGLE_UNIT ( ) );
#83369 = EDGE_CURVE ( 'NONE', #54043, #70963, #7388, .T. ) ;
#83370 = CARTESIAN_POINT ( 'NONE',  ( 105.8555784348092885, -14.21045842199437637, 186.2209013957143782 ) ) ;
#83371 = CARTESIAN_POINT ( 'NONE',  ( -83.03324683123243233, -32.55097867281028812, 159.1947170929300341 ) ) ;
#83372 = EDGE_LOOP ( 'NONE', ( #92327, #64039, #66863, #28878 ) ) ;
#83373 = DIRECTION ( 'NONE',  ( 0.000000000000000000, 0.000000000000000000, 1.000000000000000000 ) ) ;
#83374 = CARTESIAN_POINT ( 'NONE',  ( -9.646083234704192932, 253.0129060902346794, -2.643797197754266026 ) ) ;
#83375 = CARTESIAN_POINT ( 'NONE',  ( -48.02835407290516656, -1.200000000000000030E-05, 15.60535821593516737 ) ) ;
#83376 = VECTOR ( 'NONE', #42093, 1000.000000000000000 ) ;
#83377 = CARTESIAN_POINT ( 'NONE',  ( 44.46823338009918558, 1.482358050883964840E-15, 0.000000000000000000 ) ) ;
#83378 = CARTESIAN_POINT ( 'NONE',  ( 43.60048099680660272, 433.3730128036348219, 14.72755969045772950 ) ) ;
#83379 = EDGE_CURVE ( 'NONE', #48423, #67329, #67299, .T. ) ;
#83380 = CARTESIAN_POINT ( 'NONE',  ( 0.000000000000000000, 0.000000000000000000, 0.000000000000000000 ) ) ;
#83381 = ORIENTED_EDGE ( 'NONE', *, *, #54906, .T. ) ;
#83382 = CARTESIAN_POINT ( 'NONE',  ( -23.80680574697089469, 304.9792048259543549, 10.18372908566200330 ) ) ;
#83383 = ORIENTED_EDGE ( 'NONE', *, *, #18177, .T. ) ;
#83384 = DIRECTION ( 'NONE',  ( 0.000000000000000000, 0.000000000000000000, -1.000000000000000000 ) ) ;
#83385 = DIRECTION ( 'NONE',  ( 0.000000000000000000, 0.000000000000000000, -1.000000000000000000 ) ) ;
#83386 = CARTESIAN_POINT ( 'NONE',  ( 32.01581173012298365, 487.4782005592953738, 8.020290309139436857 ) ) ;
#83387 = ADVANCED_FACE ( 'NONE', ( #33883 ), #74301, .T. ) ;
#83388 = CARTESIAN_POINT ( 'NONE',  ( -50.94745919686192082, 50.00000000000000000, -37.05882352941185331 ) ) ;
#83389 = CARTESIAN_POINT ( 'NONE',  ( 30.00000000000000000, 500.0000000000002274, 0.000000000000000000 ) ) ;
#83390 = DIRECTION ( 'NONE',  ( 0.000000000000000000, 0.000000000000000000, 1.000000000000000000 ) ) ;
#83391 = EDGE_LOOP ( 'NONE', ( #91194, #93412, #24565, #30074, #63042, #55973 ) ) ;
#83392 = CARTESIAN_POINT ( 'NONE',  ( 104.7899765806434402, -60.00000000000002842, 199.3996562082950845 ) ) ;
#83394 = CARTESIAN_POINT ( 'NONE',  ( 16.76529464264830338, -39.47301229123248589, 30.70707182303599936 ) ) ;
#83393 = CARTESIAN_POINT ( 'NONE',  ( -74.93456164446882894, -30.00000000000001421, 156.1801137937684985 ) ) ;
#83396 =( NAMED_UNIT ( * ) SI_UNIT ( $, .STERADIAN. ) SOLID_ANGLE_UNIT ( ) );
#83395 = UNCERTAINTY_MEASURE_WITH_UNIT (LENGTH_MEASURE( 1.000000000000000082E-05 ), #43666, 'distance_accuracy_value', 'NONE');
#83397 = DIRECTION ( 'NONE',  ( 0.000000000000000000, 0.000000000000000000, 1.000000000000000000 ) ) ;
#83398 = CARTESIAN_POINT ( 'NONE',  ( -43.12859200516710700, -42.98411729920026403, 42.46969394239560103 ) ) ;
#83399 = DIRECTION ( 'NONE',  ( 1.000000000000000000, 1.224606353822377258E-16, 0.000000000000000000 ) ) ;
#83400 = UNCERTAINTY_MEASURE_WITH_UNIT (LENGTH_MEASURE( 1.000000000000000082E-05 ), #48821, 'distance_accuracy_value', 'NONE');
#83401 = VERTEX_POINT ( 'NONE', #84000 ) ;
#83402 = DIRECTION ( 'NONE',  ( 0.000000000000000000, -1.000000000000000000, 0.000000000000000000 ) ) ;
#83403 = CARTESIAN_POINT ( 'NONE',  ( 8.399370414911262017, 53.73747002930334560, 4.031152949374445349 ) ) ;
#83404 = CARTESIAN_POINT ( 'NONE',  ( 31.21933008645656926, 405.2090764464551853, 25.56980379099173817 ) ) ;
#83405 = LINE ( 'NONE', #93643, #95694 ) ;
#83406 = DIRECTION ( 'NONE',  ( -0.5735764363510497121, 0.8191520442889892450, 1.003171929053521665E-16 ) ) ;
#83407 = CARTESIAN_POINT ( 'NONE',  ( -34.06603414617824654, 462.4608636921087736, 4.846872666268491336 ) ) ;
#83408 = ORIENTED_EDGE ( 'NONE', *, *, #73816, .F. ) ;
#83409 = DIRECTION ( 'NONE',  ( -1.000000000000000000, 0.000000000000000000, 0.000000000000000000 ) ) ;
#83410 = ORIENTED_EDGE ( 'NONE', *, *, #83284, .T. ) ;
#83411 = CARTESIAN_POINT ( 'NONE',  ( 77.85795165744811186, -30.00000000009750778, 181.6895375475956769 ) ) ;
#83412 = CARTESIAN_POINT ( 'NONE',  ( 47.77500202626908532, 12.17856325595020195, 14.37326074422635003 ) ) ;
#83413 = AXIS2_PLACEMENT_3D ( 'NONE', #58121, #24725, #32284 ) ;
#83414 = CARTESIAN_POINT ( 'NONE',  ( 5.833333333333329485, -50.00000000000000000, 103.8776713793258608 ) ) ;
#83415 = CARTESIAN_POINT ( 'NONE',  ( 3.749999999999999112, 6.495190528383288253, -6.991905250253753756 ) ) ;
#83416 = CARTESIAN_POINT ( 'NONE',  ( 80.95702466713376566, -30.00000000000000355, 4.788817681754167666 ) ) ;
#83417 = STYLED_ITEM ( 'NONE', ( #52949 ), #98311 ) ;
#83418 = EDGE_CURVE ( 'NONE', #25863, #76724, #34993, .T. ) ;
#83419 = CARTESIAN_POINT ( 'NONE',  ( -23.38206103562286486, 304.7406344060533456, 10.13027383527492731 ) ) ;
#83420 = ORIENTED_EDGE ( 'NONE', *, *, #51762, .T. ) ;
#83421 = AXIS2_PLACEMENT_3D ( 'NONE', #13147, #95682, #46076 ) ;
#83422 = VECTOR ( 'NONE', #9142, 1000.000000000000000 ) ;
#83423 = ORIENTED_EDGE ( 'NONE', *, *, #81380, .F. ) ;
#83424 = EDGE_LOOP ( 'NONE', ( #79021, #23176, #51934, #55996, #21734 ) ) ;
#83425 = FACE_OUTER_BOUND ( 'NONE', #105578, .T. ) ;
#83426 = CARTESIAN_POINT ( 'NONE',  ( 0.000000000000000000, 0.000000000000000000, 4.000000000000000000 ) ) ;
#83427 = EDGE_CURVE ( 'NONE', #24916, #94714, #7969, .T. ) ;
#83428 = CARTESIAN_POINT ( 'NONE',  ( -31.38693051204033324, 427.9638760193610665, 23.57266965543569270 ) ) ;
#83429 = DIRECTION ( 'NONE',  ( 0.000000000000000000, 0.000000000000000000, 1.000000000000000000 ) ) ;
#83430 = ORIENTED_EDGE ( 'NONE', *, *, #55043, .T. ) ;
#83431 = CARTESIAN_POINT ( 'NONE',  ( 9.221346651730840449, 106.0483402006833984, -3.869102247876033740 ) ) ;
#83432 = ORIENTED_EDGE ( 'NONE', *, *, #94216, .T. ) ;
#83433 = CARTESIAN_POINT ( 'NONE',  ( 33.08902662345825973, 439.4144565034923744, 23.84226355454061874 ) ) ;
#83434 = CARTESIAN_POINT ( 'NONE',  ( 71.12902128746809183, -38.32834665643905936, 140.8005624972594774 ) ) ;
#83435 = CARTESIAN_POINT ( 'NONE',  ( 6.169949891408687215, 4.949864754179436943, -4.426582755167822292 ) ) ;
#83436 = CARTESIAN_POINT ( 'NONE',  ( 27.04196716693042646, 307.0757598473238090, 10.91257262733961753 ) ) ;
#83437 = DIRECTION ( 'NONE',  ( 0.000000000000000000, -1.000000000000000000, 0.000000000000000000 ) ) ;
#83438 = EDGE_LOOP ( 'NONE', ( #16029, #11070, #102389, #19462 ) ) ;
#83439 = CARTESIAN_POINT ( 'NONE',  ( 16.64348903516512834, 45.88445698070336931, -4.157797401561768247 ) ) ;
#83440 = DIRECTION ( 'NONE',  ( 0.000000000000000000, -1.000000000000000000, 0.000000000000000000 ) ) ;
#83441 = DIRECTION ( 'NONE',  ( -0.000000000000000000, -1.000000000000000000, -0.000000000000000000 ) ) ;
#83442 = CARTESIAN_POINT ( 'NONE',  ( 14.90069340504961737, 2.164550790745811248, -1.672538227366102914 ) ) ;
#83443 = ORIENTED_EDGE ( 'NONE', *, *, #93290, .F. ) ;
#83445 = CARTESIAN_POINT ( 'NONE',  ( -20.97754405179131254, 294.8763868968453608, 9.942224931492253504 ) ) ;
#83444 = FILL_AREA_STYLE_COLOUR ( '', #33103 ) ;
#83446 = PLANE ( 'NONE',  #17513 ) ;
#83447 = PRESENTATION_STYLE_ASSIGNMENT (( #82922 ) ) ;
#83448 = CARTESIAN_POINT ( 'NONE',  ( -6.523606932384105939, -4.893847819345124250, -7.213065638946083880 ) ) ;
#83449 = CARTESIAN_POINT ( 'NONE',  ( 34.47176506789151063, 489.5748983164542096, 11.69726377703232778 ) ) ;
#83450 = CARTESIAN_POINT ( 'NONE',  ( 63.56127108291158123, 4.000000000000014211, 0.000000000000000000 ) ) ;
#83451 = CIRCLE ( 'NONE', #26676, 7.000000000000024869 ) ;
#83452 = COLOUR_RGB ( '', 0.31764706, 0.68627451, 0.89019608) ;
#83453 = DIRECTION ( 'NONE',  ( -1.000000000000000000, -1.224606353822377258E-16, -0.000000000000000000 ) ) ;
#83454 =( GEOMETRIC_REPRESENTATION_CONTEXT ( 3 ) GLOBAL_UNCERTAINTY_ASSIGNED_CONTEXT ( ( #53518 ) ) GLOBAL_UNIT_ASSIGNED_CONTEXT ( ( #26770, #35929, #101147 ) ) REPRESENTATION_CONTEXT ( 'NONE', 'WORKASPACE' ) );
#83455 = CARTESIAN_POINT ( 'NONE',  ( 85.62573226540682469, -39.27103144633588272, 185.8533192315640008 ) ) ;
#83456 = CARTESIAN_POINT ( 'NONE',  ( 16.83431405849833951, 36.36677671467317907, -24.30698433968626304 ) ) ;
#83457 = SURFACE_STYLE_USAGE ( .BOTH. , #50542 ) ;
#83458 = ORIENTED_EDGE ( 'NONE', *, *, #82849, .F. ) ;
#83459 =( GEOMETRIC_REPRESENTATION_CONTEXT ( 3 ) GLOBAL_UNCERTAINTY_ASSIGNED_CONTEXT ( ( #75705 ) ) GLOBAL_UNIT_ASSIGNED_CONTEXT ( ( #15752, #25482, #82071 ) ) REPRESENTATION_CONTEXT ( 'NONE', 'WORKASPACE' ) );
#83460 = CARTESIAN_POINT ( 'NONE',  ( 94.64336416359569171, -57.65696167691804419, -9.478012974654758338 ) ) ;
#83461 = DIRECTION ( 'NONE',  ( -1.000000000000000000, -0.000000000000000000, -0.000000000000000000 ) ) ;
#83462 = CARTESIAN_POINT ( 'NONE',  ( 16.42263527633062026, 34.33311419812763177, -24.27358441403828948 ) ) ;
#83463 = CARTESIAN_POINT ( 'NONE',  ( 0.05533025579362068486, 4.993776679985853839, 4.350525068611871049 ) ) ;
#83464 = CARTESIAN_POINT ( 'NONE',  ( -81.25802617709217657, -30.00000000000000711, -10.90515713852204271 ) ) ;
#83465 = ADVANCED_FACE ( 'NONE', ( #91048 ), #43017, .T. ) ;
#83466 = DIRECTION ( 'NONE',  ( 0.000000000000000000, -0.8660254037844380415, 0.5000000000000009992 ) ) ;
#83467 = CARTESIAN_POINT ( 'NONE',  ( 58.18888888888888999, 3.309500000000014541, 4.052968581778174646E-16 ) ) ;
#83468 = LINE ( 'NONE', #385, #77386 ) ;
#83469 = ADVANCED_FACE ( 'NONE', ( #61338 ), #10628, .F. ) ;
#83471 = CARTESIAN_POINT ( 'NONE',  ( 34.88900972249397370, 464.6206820655982028, 18.69027339340997784 ) ) ;
#83470 = CARTESIAN_POINT ( 'NONE',  ( 35.77017041476860015, 490.7753167606494458, 12.37440192957616070 ) ) ;
#83472 = DIRECTION ( 'NONE',  ( 0.000000000000000000, 1.000000000000000000, 0.000000000000000000 ) ) ;
#83473 = DIRECTION ( 'NONE',  ( 0.5735764363510554853, 0.8191520442889852482, 0.000000000000000000 ) ) ;
#83474 = CARTESIAN_POINT ( 'NONE',  ( 14.33580413386840213, 42.00000000000000000, -89.41414995614803729 ) ) ;
#83475 = CARTESIAN_POINT ( 'NONE',  ( 5.647817967127097383, -81.54873593471207016, -2.038183545141173614 ) ) ;
#83476 = CARTESIAN_POINT ( 'NONE',  ( 0.7145311798161616545, -4.618802153517262532, -8.000000000000001776 ) ) ;
#83477 = CARTESIAN_POINT ( 'NONE',  ( 96.86866073052655679, 1.030564683017419500E-14, 0.000000000000000000 ) ) ;
#83478 = CARTESIAN_POINT ( 'NONE',  ( 68.12539969591429667, -29.92624738978073751, -21.66398342862366988 ) ) ;
#83479 = ORIENTED_EDGE ( 'NONE', *, *, #3266, .T. ) ;
#83480 = CARTESIAN_POINT ( 'NONE',  ( 6.984126283073807784, 9.027603028764220383, -0.5389771161762282325 ) ) ;
#83481 = CARTESIAN_POINT ( 'NONE',  ( -7.002990960197238657, 83.94733181616544471, 3.868040364119522234 ) ) ;
#83482 = CARTESIAN_POINT ( 'NONE',  ( -41.71284618355627316, -25.37309400074422072, -29.93689894554868758 ) ) ;
#83483 = CIRCLE ( 'NONE', #50746, 1.999999999999998668 ) ;
#83485 = CARTESIAN_POINT ( 'NONE',  ( -15.00099999999999767, 12.99999999999999289, -4.000000000000000000 ) ) ;
#83484 = CARTESIAN_POINT ( 'NONE',  ( 89.06666666666666288, 1.023464760207051730E-14, 0.000000000000000000 ) ) ;
#83486 = EDGE_CURVE ( 'NONE', #61806, #99054, #74530, .T. ) ;
#83487 = CARTESIAN_POINT ( 'NONE',  ( 7.270302578000916505, -3.659675574284731780, -18.03744543698569203 ) ) ;
#83488 = ORIENTED_EDGE ( 'NONE', *, *, #34418, .F. ) ;
#83489 = DIRECTION ( 'NONE',  ( 0.000000000000000000, -1.000000000000000000, 0.000000000000000000 ) ) ;
#83490 = ORIENTED_EDGE ( 'NONE', *, *, #73557, .T. ) ;
#83491 = CARTESIAN_POINT ( 'NONE',  ( -26.01822098816688467, 35.07276571059547621, 8.183900759913079526 ) ) ;
#83492 = CARTESIAN_POINT ( 'NONE',  ( 15.36292483821380372, 2.971926847719377651, 2.727430453976030122 ) ) ;
#83493 = ADVANCED_FACE ( 'NONE', ( #36029 ), #105563, .T. ) ;
#83494 = CARTESIAN_POINT ( 'NONE',  ( -50.02737965620911353, -60.00000000000000711, -37.89930100465098661 ) ) ;
#83495 = ORIENTED_EDGE ( 'NONE', *, *, #27851, .T. ) ;
#83496 = CARTESIAN_POINT ( 'NONE',  ( 15.05785784214676326, 3.824195276769950969, 4.604276673498415740 ) ) ;
#83497 = CARTESIAN_POINT ( 'NONE',  ( 101.9301734557807322, -60.21151021950694116, 194.2770710414559687 ) ) ;
#83499 = CARTESIAN_POINT ( 'NONE',  ( -7.344361273354514275, -7.554394694114762387, -3.175733139645582792 ) ) ;
#83498 = CARTESIAN_POINT ( 'NONE',  ( 9.789044728060087408, 294.6486233851415477, -2.043184600578025201 ) ) ;
#83500 = ORIENTED_EDGE ( 'NONE', *, *, #76541, .T. ) ;
#83501 = ORIENTED_EDGE ( 'NONE', *, *, #16156, .T. ) ;
#83502 = EDGE_LOOP ( 'NONE', ( #10146, #82488, #99262, #103830 ) ) ;
#83503 = CARTESIAN_POINT ( 'NONE',  ( 29.35230083617101116, 317.9833937185579202, 13.40910235493362634 ) ) ;
#83504 = CARTESIAN_POINT ( 'NONE',  ( -13.49999999999999822, 1.319989657865599186, -12.97199716660744961 ) ) ;
#83505 = CARTESIAN_POINT ( 'NONE',  ( 43.30868969682389036, 5.000000000000015099, 6.123233995736782060E-16 ) ) ;
#83507 = EDGE_CURVE ( 'NONE', #78511, #72914, #43547, .T. ) ;
#83506 = ORIENTED_EDGE ( 'NONE', *, *, #51604, .T. ) ;
#83508 = AXIS2_PLACEMENT_3D ( 'NONE', #10830, #43751, #76643 ) ;
#83509 = CARTESIAN_POINT ( 'NONE',  ( 0.000000000000000000, 152.0000000000000000, -5.000000000000000000 ) ) ;
#83510 = DIRECTION ( 'NONE',  ( 0.000000000000000000, 1.000000000000000000, 0.000000000000000000 ) ) ;
#83511 = B_SPLINE_CURVE_WITH_KNOTS ( 'NONE', 3,
 ( #8254, #7718, #48178, #64913, #72981, #105887 ),
 .UNSPECIFIED., .F., .F.,
 ( 4, 2, 4 ),
 ( 8.673617379884035472E-19, 0.0003910247833730961706, 0.0007820495667461914739 ),
 .UNSPECIFIED. ) ;
#83512 = DIRECTION ( 'NONE',  ( -1.000000000000000000, -1.224606353822377258E-16, -0.000000000000000000 ) ) ;
#83513 = CARTESIAN_POINT ( 'NONE',  ( -22.17556693859086536, -57.67274538812966256, 42.55074624272938877 ) ) ;
#83514 = DIRECTION ( 'NONE',  ( -1.000000000000000000, -1.224606353822377258E-16, -0.000000000000000000 ) ) ;
#83515 = CARTESIAN_POINT ( 'NONE',  ( 0.000000000000000000, 4.898587196589413815E-16, -4.000000000000000888 ) ) ;
#83516 = CARTESIAN_POINT ( 'NONE',  ( -6.542885568110277106, 41.77240995323538897, -59.03854211387476880 ) ) ;
#83517 = CARTESIAN_POINT ( 'NONE',  ( -94.55497525217361954, -59.99999999999993605, 22.39874202688834615 ) ) ;
#83518 = CARTESIAN_POINT ( 'NONE',  ( -51.04693240308429125, -29.11976890750409197, 48.95828090291404067 ) ) ;
#83519 = CARTESIAN_POINT ( 'NONE',  ( 4.010857135589731489E-16, 21.85270131633359014, 7.000000000000016875 ) ) ;
#83520 = PRESENTATION_LAYER_ASSIGNMENT (  '', '', ( #790 ) ) ;
#83521 = VERTEX_POINT ( 'NONE', #103378 ) ;
#83522 = CARTESIAN_POINT ( 'NONE',  ( -96.70315692490667914, -60.36316151395556773, 196.8125950864377387 ) ) ;
#83523 = STYLED_ITEM ( 'NONE', ( #61517 ), #56475 ) ;
#83524 = DIRECTION ( 'NONE',  ( -0.5735764363510494901, -0.8191520442889894671, 0.000000000000000000 ) ) ;
#83525 = CARTESIAN_POINT ( 'NONE',  ( 0.000000000000000000, 0.000000000000000000, 4.000000000000000888 ) ) ;
#83526 = ORIENTED_EDGE ( 'NONE', *, *, #57983, .T. ) ;
#83527 = CARTESIAN_POINT ( 'NONE',  ( 9.500000000000003553, -5.000000000000000000, -68.91429205785459544 ) ) ;
#83528 = AXIS2_PLACEMENT_3D ( 'NONE', #67369, #41482, #51155 ) ;
#83529 = CARTESIAN_POINT ( 'NONE',  ( 80.86154658310535126, -38.83032902587230950, 194.4093053065819845 ) ) ;
#83530 = DIRECTION ( 'NONE',  ( 0.000000000000000000, -1.000000000000000000, 0.000000000000000000 ) ) ;
#83531 = CARTESIAN_POINT ( 'NONE',  ( -11.28790243858421327, -9.071383756617098726, -12.46447053051440790 ) ) ;
#83532 = AXIS2_PLACEMENT_3D ( 'NONE', #37340, #13004, #96074 ) ;
#83533 = CARTESIAN_POINT ( 'NONE',  ( 93.08106583031154457, -30.00000000000000000, 191.1326281931611106 ) ) ;
#83534 = B_SPLINE_CURVE_WITH_KNOTS ( 'NONE', 3,
 ( #86336, #29188, #76608, #2722, #28641, #43718, #37797, #69078 ),
 .UNSPECIFIED., .F., .F.,
 ( 4, 2, 2, 4 ),
 ( 0.004673709593152147040, 0.005837709341827638197, 0.007001709090503129354, 0.009329708587854111668 ),
 .UNSPECIFIED. ) ;
#83535 = DIRECTION ( 'NONE',  ( 0.5735764363510462704, 0.8191520442889915765, 0.000000000000000000 ) ) ;
#83536 = DIRECTION ( 'NONE',  ( -0.000000000000000000, -1.000000000000000000, -0.000000000000000000 ) ) ;
#83537 = EDGE_CURVE ( 'NONE', #78767, #79890, #71075, .T. ) ;
#83538 = CARTESIAN_POINT ( 'NONE',  ( 42.98746414932995208, -5.000000000000000000, 6.123233995736768255E-16 ) ) ;
#83539 = ORIENTED_EDGE ( 'NONE', *, *, #59716, .T. ) ;
#83540 = ORIENTED_EDGE ( 'NONE', *, *, #63991, .T. ) ;
#83541 = CARTESIAN_POINT ( 'NONE',  ( 53.38895677506906168, -25.63475069958329655, 51.75996385648595322 ) ) ;
#83542 = CARTESIAN_POINT ( 'NONE',  ( 5.398220238549152228, 41.68867471179443385, -58.74408635829322378 ) ) ;
#83543 = CARTESIAN_POINT ( 'NONE',  ( -5.500000000000006217, 42.00000000000000000, -58.09827136975972905 ) ) ;
#83544 = EDGE_CURVE ( 'NONE', #80206, #6993, #102310, .T. ) ;
#83545 = EDGE_LOOP ( 'NONE', ( #64796, #61814 ) ) ;
#83546 = CARTESIAN_POINT ( 'NONE',  ( -90.72424882750010511, -38.34306975412113161, 6.969030681448126430 ) ) ;
#83547 = EDGE_LOOP ( 'NONE', ( #97570, #9322 ) ) ;
#83548 = CARTESIAN_POINT ( 'NONE',  ( 14.58597127886924483, 5.499146323186232088, 6.679532531465572909 ) ) ;
#83549 = CARTESIAN_POINT ( 'NONE',  ( 110.3706048748884427, -38.35605039672871186, 158.9118694323576619 ) ) ;
#83550 = CARTESIAN_POINT ( 'NONE',  ( 11.83150069961154216, 21.33506542399163664, -7.411767003152391453 ) ) ;
#83551 = CARTESIAN_POINT ( 'NONE',  ( 86.61308833284006425, -45.28267297219348819, 48.35240368102819986 ) ) ;
#83552 = CARTESIAN_POINT ( 'NONE',  ( 1.719443193058131758, -4.999999999998633093, -17.47055129848030219 ) ) ;
#83553 = CARTESIAN_POINT ( 'NONE',  ( -1.308996938995748982, -3.000000000000001776, -75.00000000000000000 ) ) ;
#83554 = CARTESIAN_POINT ( 'NONE',  ( 74.76516655405903578, -59.99999999999997868, 179.4311784582239682 ) ) ;
#83555 = CARTESIAN_POINT ( 'NONE',  ( -2.500000000000000888, -17.18734298064772759, 25.31896405944760531 ) ) ;
#83556 = EDGE_CURVE ( 'NONE', #101661, #49207, #52130, .T. ) ;
#83557 =( BOUNDED_SURFACE ( )  B_SPLINE_SURFACE ( 2, 3, ( 
 ( #62155, #21700, #95048, #63737, #11973, #62672, #46476, #38923, #63200, #79364 ),
 ( #96091, #30854, #96620, #49102, #56666, #65835, #31385, #89059, #98715, #90111 ),
 ( #32437, #7058, #47522, #82002, #105757, #89590, #48042, #72337, #98197, #105241 ) ),
 .UNSPECIFIED., .F., .F., .F. ) 
 B_SPLINE_SURFACE_WITH_KNOTS ( ( 3, 3 ),
 ( 4, 2, 2, 2, 4 ),
 ( 0.000000000000000000, 1.000000000000000000 ),
 ( 0.000000000000000000, 0.001626978433639921342, 0.003253956867279842683, 0.004880935300919764241, 0.006507913734559685366 ),
 .UNSPECIFIED. ) 
 GEOMETRIC_REPRESENTATION_ITEM ( )  RATIONAL_B_SPLINE_SURFACE ( (
 ( 1.000000000000000000, 1.000000000000000000, 1.000000000000000000, 1.000000000000000000, 1.000000000000000000, 1.000000000000000000, 1.000000000000000000, 1.000000000000000000, 1.000000000000000000, 1.000000000000000000),
 ( 1.857142857142858317, 1.857142857142858317, 1.857142857142858317, 1.857142857142858317, 1.857142857142858317, 1.857142857142858317, 1.857142857142858317, 1.857142857142858317, 1.857142857142858317, 1.857142857142858317),
 ( 1.000000000000000000, 1.000000000000000000, 1.000000000000000000, 1.000000000000000000, 1.000000000000000000, 1.000000000000000000, 1.000000000000000000, 1.000000000000000000, 1.000000000000000000, 1.000000000000000000) ) ) 
 REPRESENTATION_ITEM ( '' )  SURFACE ( )  );
#83558 = AXIS2_PLACEMENT_3D ( 'NONE', #67958, #91709, #99238 ) ;
#83559 = CARTESIAN_POINT ( 'NONE',  ( -43.63911886418856767, 435.1012159695318360, 10.95008075558104110 ) ) ;
#83560 = ORIENTED_EDGE ( 'NONE', *, *, #63720, .T. ) ;
#83561 = CARTESIAN_POINT ( 'NONE',  ( 63.02317967037522806, -22.10708017086810173, 71.83048262152487951 ) ) ;
#83562 = LINE ( 'NONE', #10205, #91012 ) ;
#83563 = CARTESIAN_POINT ( 'NONE',  ( -38.47428897412110160, 485.7788508071988076, -4.770630528146475591 ) ) ;
#83564 = CARTESIAN_POINT ( 'NONE',  ( -42.74672710594789748, 418.3108395146689418, 19.64234251677965659 ) ) ;
#83565 = CARTESIAN_POINT ( 'NONE',  ( 18.86650669486618881, 1.474610560812782335E-15, 0.000000000000000000 ) ) ;
#83566 = CARTESIAN_POINT ( 'NONE',  ( 5.000000000000000000, 6.123233995736766282E-16, -4.289342857142857568 ) ) ;
#83567 = CARTESIAN_POINT ( 'NONE',  ( 7.999999999999998224, -29.09374999999999289, 3.313708498984766493 ) ) ;
#83568 = CARTESIAN_POINT ( 'NONE',  ( 16.64348903516512834, 43.75610143575153899, -4.157797401561768247 ) ) ;
#83569 = ORIENTED_EDGE ( 'NONE', *, *, #77768, .T. ) ;
#83570 = CARTESIAN_POINT ( 'NONE',  ( 83.03373258142163138, -46.50209328944929865, 179.9266600372746723 ) ) ;
#83571 = CARTESIAN_POINT ( 'NONE',  ( -37.88465841952032065, 27.77130359203633958, 10.98700391011192679 ) ) ;
#83572 = CONICAL_SURFACE ( 'NONE', #37124, 13.50000000000000178, 1.047197551196596077 ) ;
#83573 = CARTESIAN_POINT ( 'NONE',  ( -8.000000000000001776, -8.843750004096769146, 3.313708498984759387 ) ) ;
#83574 = VERTEX_POINT ( 'NONE', #78557 ) ;
#83575 = CARTESIAN_POINT ( 'NONE',  ( 10.59999999999999609, -3.309499999999999886, 4.475777889183790779E-16 ) ) ;
#83576 = CARTESIAN_POINT ( 'NONE',  ( 9.060614273895151172, -4.999999999999968914, -17.33913672110647752 ) ) ;
#83577 =( NAMED_UNIT ( * ) PLANE_ANGLE_UNIT ( ) SI_UNIT ( $, .RADIAN. ) );
#83578 =( NAMED_UNIT ( * ) PLANE_ANGLE_UNIT ( ) SI_UNIT ( $, .RADIAN. ) );
#83579 = CARTESIAN_POINT ( 'NONE',  ( -8.857351009234111672, -3.000000000000002665, -97.18047212222559494 ) ) ;
#83580 = CARTESIAN_POINT ( 'NONE',  ( -21.34091502998213485, -26.33362732275400475, -38.46055773294248326 ) ) ;
#83581 = EDGE_CURVE ( 'NONE', #23780, #74084, #68903, .T. ) ;
#83582 = PRESENTATION_STYLE_ASSIGNMENT (( #41540 ) ) ;
#83583 = CARTESIAN_POINT ( 'NONE',  ( 47.45147319089161897, -60.00000000000002132, 65.78626815950619289 ) ) ;
#83584 = CARTESIAN_POINT ( 'NONE',  ( 6.944371705245971249, 105.5389969142454731, -3.972324460300566962 ) ) ;
#83585 = CARTESIAN_POINT ( 'NONE',  ( 8.695822068310066655, -13.47502420773152920, 31.95796511938647200 ) ) ;
#83586 = ADVANCED_FACE ( 'NONE', ( #27943 ), #69950, .F. ) ;
#83587 = EDGE_CURVE ( 'NONE', #11120, #92773, #28460, .T. ) ;
#83589 = CARTESIAN_POINT ( 'NONE',  ( -15.54016792948419656, 22.94944790772357024, -1.155673903705213057 ) ) ;
#83588 = CARTESIAN_POINT ( 'NONE',  ( -12.03844305070917997, -21.14040406273131012, 35.57043951055553066 ) ) ;
#83590 = CARTESIAN_POINT ( 'NONE',  ( 0.000000000000000000, -8.000000000000000000, 0.000000000000000000 ) ) ;
#83591 = CARTESIAN_POINT ( 'NONE',  ( 45.29905483467455696, 497.0732240353902398, -8.041250874568902418 ) ) ;
#83592 = CARTESIAN_POINT ( 'NONE',  ( -37.56673239365849781, -1.200000000000000030E-05, 12.20617127781066102 ) ) ;
#83593 = CONICAL_SURFACE ( 'NONE', #80134, 4.172000000000009479, 0.9599310885968813656 ) ;
#83594 = AXIS2_PLACEMENT_3D ( 'NONE', #7892, #14922, #57502 ) ;
#83595 = CARTESIAN_POINT ( 'NONE',  ( -2.623433461001182021, 7.604994000793857012, -7.633824513837113024 ) ) ;
#83596 = CONICAL_SURFACE ( 'NONE', #105997, 5.000000000000010658, 0.9599310885968697082 ) ;
#83597 = ORIENTED_EDGE ( 'NONE', *, *, #23335, .F. ) ;
#83598 = CARTESIAN_POINT ( 'NONE',  ( -2.965789724133574889, -21.40052483609195022, -38.55044985044033012 ) ) ;
#83599 = PRODUCT_DEFINITION_SHAPE ( 'NONE', 'NONE',  #106796 ) ;
#83600 = CARTESIAN_POINT ( 'NONE',  ( -17.49999999999841904, 48.26617306480387981, 62.61753806995410088 ) ) ;
#83601 = CARTESIAN_POINT ( 'NONE',  ( -12.39875862467593848, -3.846090740250397655, 20.49813959098556282 ) ) ;
#83602 = STYLED_ITEM ( 'NONE', ( #58386 ), #13526 ) ;
#83604 = CARTESIAN_POINT ( 'NONE',  ( 28.05109246044522564, -21.77036439436171023, -28.92073443998052795 ) ) ;
#83603 = CARTESIAN_POINT ( 'NONE',  ( 52.81650669486619165, 4.898587196589294500E-16, -4.000000000000007105 ) ) ;
#83605 = ADVANCED_FACE ( 'NONE', ( #11688 ), #54126, .F. ) ;
#83606 = VERTEX_POINT ( 'NONE', #95820 ) ;
#83607 = CARTESIAN_POINT ( 'NONE',  ( -5.477432325710316796, -88.16479535570472592, 2.459915882346686899 ) ) ;
#83608 = CARTESIAN_POINT ( 'NONE',  ( -4.277917525292022738, 52.15487555894509342, 6.542882894562609408 ) ) ;
#83609 = VERTEX_POINT ( 'NONE', #13811 ) ;
#83610 = CARTESIAN_POINT ( 'NONE',  ( 6.123233995736763324E-16, 48.00000000000000000, -95.00000000000000000 ) ) ;
#83611 = CARTESIAN_POINT ( 'NONE',  ( 45.94900261086841198, 1.482358050883964840E-15, 0.000000000000000000 ) ) ;
#83612 = CARTESIAN_POINT ( 'NONE',  ( -17.66057173557561910, 41.94261100565687883, -82.88176911731406449 ) ) ;
#83613 = CARTESIAN_POINT ( 'NONE',  ( -98.25489335440740035, -60.00000000000000711, 70.49837245525611706 ) ) ;
#83614 = SURFACE_STYLE_USAGE ( .BOTH. , #52315 ) ;
#83615 = CARTESIAN_POINT ( 'NONE',  ( 26.11923076923076792, 4.172000000000003261, 0.000000000000000000 ) ) ;
#83616 = CARTESIAN_POINT ( 'NONE',  ( 31.00389226642222340, 485.8187364282109115, 14.27494812388583512 ) ) ;
#83617 = CARTESIAN_POINT ( 'NONE',  ( 41.18500240986835337, 460.1236783698127510, 2.133705300515011061 ) ) ;
#83619 = CARTESIAN_POINT ( 'NONE',  ( -15.46209624076597144, 2.722175477911281671, -1.608330402066967979 ) ) ;
#83618 = CARTESIAN_POINT ( 'NONE',  ( -35.12011055360168399, 436.4929263758896809, 6.579006402756536254 ) ) ;
#83620 = CARTESIAN_POINT ( 'NONE',  ( -83.42161577068522149, -39.47582673691351829, 173.7517446053938102 ) ) ;
#83621 = ORIENTED_EDGE ( 'NONE', *, *, #102523, .T. ) ;
#83623 = FACE_OUTER_BOUND ( 'NONE', #23076, .T. ) ;
#83622 = B_SPLINE_CURVE_WITH_KNOTS ( 'NONE', 3,
 ( #26613, #41166, #16348, #41689 ),
 .UNSPECIFIED., .F., .F.,
 ( 4, 4 ),
 ( 1.734723475976806902E-18, 0.0001919544104626820578 ),
 .UNSPECIFIED. ) ;
#83624 = ORIENTED_EDGE ( 'NONE', *, *, #35490, .F. ) ;
#83625 = CIRCLE ( 'NONE', #30308, 10.12668159690567649 ) ;
#83626 = ORIENTED_EDGE ( 'NONE', *, *, #65477, .F. ) ;
#83627 = CARTESIAN_POINT ( 'NONE',  ( -4.506266729858579012, -1.182839587743470977, 104.3949571352749643 ) ) ;
#83628 = CARTESIAN_POINT ( 'NONE',  ( -3.605819256461556543E-15, 5.788408252967900403, 2.974182810908597929 ) ) ;
#83629 = ORIENTED_EDGE ( 'NONE', *, *, #66345, .T. ) ;
#83630 = CARTESIAN_POINT ( 'NONE',  ( -73.50473004590615744, -60.00000000000000000, -24.84693947030580574 ) ) ;
#83631 = DIRECTION ( 'NONE',  ( 0.000000000000000000, -1.000000000000000000, 0.000000000000000000 ) ) ;
#83632 = CARTESIAN_POINT ( 'NONE',  ( 12.61650669486618881, 4.898587196589411843E-16, -4.000000000000000888 ) ) ;
#83633 = CARTESIAN_POINT ( 'NONE',  ( -3.584918491109374106, 16.05929873264827279, 6.013529126027898464 ) ) ;
#83634 = CARTESIAN_POINT ( 'NONE',  ( -1.250712992818178160, 53.76598346644076543, 9.153008886931235821 ) ) ;
#83635 = LINE ( 'NONE', #93349, #101901 ) ;
#83636 = CARTESIAN_POINT ( 'NONE',  ( 87.30924545702741568, -14.21045842199429998, 28.19131950638903206 ) ) ;
#83637 = CARTESIAN_POINT ( 'NONE',  ( -80.26890325034752038, -59.99999999999982947, 200.1011331233653721 ) ) ;
#83638 = CARTESIAN_POINT ( 'NONE',  ( -57.23881194926001115, -42.96809999363954091, 66.85320747466838043 ) ) ;
#83639 = ORIENTED_EDGE ( 'NONE', *, *, #22779, .T. ) ;
#83640 = CARTESIAN_POINT ( 'NONE',  ( -0.7521598668867096604, 300.0000000000000000, 9.936704142777553983 ) ) ;
#83641 = CARTESIAN_POINT ( 'NONE',  ( 92.57024406876091405, -60.00000000000966338, -19.13806900009738499 ) ) ;
#83642 = ORIENTED_EDGE ( 'NONE', *, *, #88658, .F. ) ;
#83643 = CARTESIAN_POINT ( 'NONE',  ( 7.155655305952319800, -42.95360862942818159, 31.03894574562138686 ) ) ;
#83644 = CARTESIAN_POINT ( 'NONE',  ( -104.6942319917173450, -60.15544093628119526, 188.9572098072957829 ) ) ;
#83645 = EDGE_LOOP ( 'NONE', ( #45081, #71886, #99352, #57498, #98318 ) ) ;
#83646 = CARTESIAN_POINT ( 'NONE',  ( -46.00000000000000711, 488.2671786690042950, 2.798715677624241671 ) ) ;
#83647 = CARTESIAN_POINT ( 'NONE',  ( -80.26108746176230113, -60.00000000000001421, 196.3255223119888342 ) ) ;
#83648 = LINE ( 'NONE', #9760, #45039 ) ;
#83649 = CARTESIAN_POINT ( 'NONE',  ( 5.082755093536325930, -22.34375000204838457, -5.082755093536325042 ) ) ;
#83650 = FACE_OUTER_BOUND ( 'NONE', #26255, .T. ) ;
#83651 = FACE_OUTER_BOUND ( 'NONE', #32118, .T. ) ;
#83652 = CARTESIAN_POINT ( 'NONE',  ( 5.483224646671643221, 0.000000000000000000, 16.14659623658214116 ) ) ;
#83653 = FACE_OUTER_BOUND ( 'NONE', #78811, .T. ) ;
#83654 = CARTESIAN_POINT ( 'NONE',  ( 24.60488647473181345, 306.9835580411500473, 10.41807558718820914 ) ) ;
#83655 = CARTESIAN_POINT ( 'NONE',  ( 12.57292557173279590, -10.06217675253460975, 11.13464401508594115 ) ) ;
#83656 = CYLINDRICAL_SURFACE ( 'NONE', #78840, 1.250000000000001110 ) ;
#83657 = ADVANCED_FACE ( 'NONE', ( #14335 ), #60904, .T. ) ;
#83658 = AXIS2_PLACEMENT_3D ( 'NONE', #22044, #47871, #29621 ) ;
#83659 = LINE ( 'NONE', #59, #48257 ) ;
#83660 = UNCERTAINTY_MEASURE_WITH_UNIT (LENGTH_MEASURE( 1.000000000000000082E-05 ), #67984, 'distance_accuracy_value', 'NONE');
#83661 = CARTESIAN_POINT ( 'NONE',  ( -32.52340609234104107, -56.84855274590991314, 37.29694331777213279 ) ) ;
#83662 = CARTESIAN_POINT ( 'NONE',  ( -1.909182100399782422, -49.86416495494171386, 102.2488568920577734 ) ) ;
#83663 = CARTESIAN_POINT ( 'NONE',  ( 46.32781807547821984, -46.43946234991636857, 47.27666961722683681 ) ) ;
#83664 = FILL_AREA_STYLE_COLOUR ( '', #16217 ) ;
#83665 = ORIENTED_EDGE ( 'NONE', *, *, #15313, .T. ) ;
#83666 = ADVANCED_FACE ( 'NONE', ( #89314 ), #105613, .F. ) ;
#83667 = CARTESIAN_POINT ( 'NONE',  ( 43.71789550056999474, 434.9437403290091879, 13.92762231526894112 ) ) ;
#83668 = EDGE_CURVE ( 'NONE', #25032, #76997, #100407, .T. ) ;
#83669 = CARTESIAN_POINT ( 'NONE',  ( -78.44477202083649559, -38.62748133887316015, 189.5277942107175306 ) ) ;
#83670 = AXIS2_PLACEMENT_3D ( 'NONE', #48234, #65502, #6729 ) ;
#83671 = ORIENTED_EDGE ( 'NONE', *, *, #17733, .T. ) ;
#83673 = CARTESIAN_POINT ( 'NONE',  ( 40.95595929481465447, 405.2208686710653183, 27.85131585683114963 ) ) ;
#83672 = CARTESIAN_POINT ( 'NONE',  ( 42.55893460000645234, 435.1566242046030766, 18.92048169488380083 ) ) ;
#83674 = DIRECTION ( 'NONE',  ( 0.000000000000000000, -1.000000000000000000, 0.000000000000000000 ) ) ;
#83675 = CARTESIAN_POINT ( 'NONE',  ( -7.417433415418480003, 41.15875677289866985, -59.49136428978601998 ) ) ;
#83676 = AXIS2_PLACEMENT_3D ( 'NONE', #48644, #72408, #81016 ) ;
#83677 = AXIS2_PLACEMENT_3D ( 'NONE', #38449, #86997, #31430 ) ;
#83678 = CARTESIAN_POINT ( 'NONE',  ( 34.67805467039151779, 461.9798124557175356, 4.171311676497361454 ) ) ;
#83679 = DIRECTION ( 'NONE',  ( 0.000000000000000000, 0.000000000000000000, -1.000000000000000000 ) ) ;
#83680 = STYLED_ITEM ( 'NONE', ( #96398 ), #36367 ) ;
#83681 = CARTESIAN_POINT ( 'NONE',  ( 5.000000000000000000, -42.29200263518463032, 4.347328673565829860 ) ) ;
#83682 = DIRECTION ( 'NONE',  ( -1.000000000000000000, -1.224606353822377258E-16, -0.000000000000000000 ) ) ;
#83683 = CARTESIAN_POINT ( 'NONE',  ( 108.9316662144759817, -60.00000000000001421, 135.4909546950748904 ) ) ;
#83684 = DIRECTION ( 'NONE',  ( 0.000000000000000000, -1.000000000000000000, 0.000000000000000000 ) ) ;
#83685 = ADVANCED_FACE ( 'NONE', ( #1870 ), #16478, .F. ) ;
#83686 = AXIS2_PLACEMENT_3D ( 'NONE', #40107, #89194, #41692 ) ;
#83687 = CARTESIAN_POINT ( 'NONE',  ( 4.898587196589412829E-16, -21.12499999999999289, -8.000000000000000000 ) ) ;
#83688 = ORIENTED_EDGE ( 'NONE', *, *, #39815, .T. ) ;
#83689 = B_SPLINE_CURVE_WITH_KNOTS ( 'NONE', 3,
 ( #22681, #97059, #63660, #7502, #15079, #89514 ),
 .UNSPECIFIED., .F., .F.,
 ( 4, 2, 4 ),
 ( 0.000000000000000000, 0.001990940508721407518, 0.003981881017442815036 ),
 .UNSPECIFIED. ) ;
#83690 = CARTESIAN_POINT ( 'NONE',  ( -96.41186482556817339, -29.99999999999981526, 191.2305605891251901 ) ) ;
#83691 = ORIENTED_EDGE ( 'NONE', *, *, #94481, .T. ) ;
#83692 = CARTESIAN_POINT ( 'NONE',  ( 26.01879166445673874, 37.20103050938880784, -8.182916409703022254 ) ) ;
#83693 = DIRECTION ( 'NONE',  ( 0.000000000000000000, 0.000000000000000000, -1.000000000000000000 ) ) ;
#83694 = CYLINDRICAL_SURFACE ( 'NONE', #75924, 1.250000000000000000 ) ;
#83695 = LINE ( 'NONE', #76138, #83339 ) ;
#83696 = CARTESIAN_POINT ( 'NONE',  ( -5.082755093536325042, -21.96875000204838457, -5.082755093536325930 ) ) ;
#83697 = CARTESIAN_POINT ( 'NONE',  ( -3.702395615612349200, -1.049538900538678154, 103.3251893371222536 ) ) ;
#83698 = UNCERTAINTY_MEASURE_WITH_UNIT (LENGTH_MEASURE( 1.000000000000000082E-05 ), #44970, 'distance_accuracy_value', 'NONE');
#83699 = CARTESIAN_POINT ( 'NONE',  ( 1.132798289211301501E-15, -15.00000000000000000, 9.000000000000000000 ) ) ;
#83700 = ORIENTED_EDGE ( 'NONE', *, *, #48658, .F. ) ;
#83701 = CARTESIAN_POINT ( 'NONE',  ( 84.31892941953071841, -22.12908237796155220, 154.7626912266840975 ) ) ;
#83702 = CARTESIAN_POINT ( 'NONE',  ( -51.48757442383523397, 38.95383793070303113, -37.45149417477429665 ) ) ;
#83703 = CYLINDRICAL_SURFACE ( 'NONE', #71255, 1.250000000000000222 ) ;
#83704 = ORIENTED_EDGE ( 'NONE', *, *, #22824, .T. ) ;
#83705 = CYLINDRICAL_SURFACE ( 'NONE', #106454, 8.000000000000000000 ) ;
#83706 = CARTESIAN_POINT ( 'NONE',  ( 89.99999999999997158, -52.00000000000000000, 198.0238439516549818 ) ) ;
#83707 = CARTESIAN_POINT ( 'NONE',  ( -1.841875822471433519E-14, -3.000000000000002665, -70.00227127314062159 ) ) ;
#83708 = CARTESIAN_POINT ( 'NONE',  ( 32.21290004233850368, 485.9817488811997350, 5.040586218672359564 ) ) ;
#83709 = CIRCLE ( 'NONE', #73373, 4.000000000000000888 ) ;
#83710 = CARTESIAN_POINT ( 'NONE',  ( -5.191144708981720868, 252.6403008552126721, 3.015512395308842297 ) ) ;
#83711 = CARTESIAN_POINT ( 'NONE',  ( 11.04468709431039564, 45.87751353276773614, 13.15154111190456021 ) ) ;
#83712 = DIRECTION ( 'NONE',  ( 0.000000000000000000, -1.000000000000000000, 0.000000000000000000 ) ) ;
#83713 = EDGE_LOOP ( 'NONE', ( #10351, #25368, #47088, #40715 ) ) ;
#83714 = EDGE_CURVE ( 'NONE', #61003, #31318, #83166, .T. ) ;
#83715 = CARTESIAN_POINT ( 'NONE',  ( 0.000000000000000000, 0.000000000000000000, 0.000000000000000000 ) ) ;
#83716 = CARTESIAN_POINT ( 'NONE',  ( -5.000000000005067946, -59.33879011280326665, 7.480853745603068816 ) ) ;
#83717 = CARTESIAN_POINT ( 'NONE',  ( 87.30971457308248773, -31.67967750561784968, 188.1757596176438199 ) ) ;
#83718 = EDGE_CURVE ( 'NONE', #18153, #68507, #64620, .T. ) ;
#83719 = ADVANCED_FACE ( 'NONE', ( #101116 ), #82292, .F. ) ;
#83720 = CARTESIAN_POINT ( 'NONE',  ( 94.84444444444443434, 1.023464760207051730E-14, 0.000000000000000000 ) ) ;
#83721 = CARTESIAN_POINT ( 'NONE',  ( 2.977408999572651815, -32.93750000204839523, 7.188101187500000933 ) ) ;
#83722 = CARTESIAN_POINT ( 'NONE',  ( 17.47322663601547177, 294.5877948852590293, -2.055689749307683112 ) ) ;
#83723 = CARTESIAN_POINT ( 'NONE',  ( -14.95520043898599738, 4.194724623223834215, 5.164345506907288552 ) ) ;
#83724 = CARTESIAN_POINT ( 'NONE',  ( 19.83349330513379982, 1.593028355512270567E-15, 0.000000000000000000 ) ) ;
#83725 = AXIS2_PLACEMENT_3D ( 'NONE', #1981, #11665, #83972 ) ;
#83726 = VERTEX_POINT ( 'NONE', #101654 ) ;
#83727 = DIRECTION ( 'NONE',  ( -0.000000000000000000, -1.000000000000000000, -0.000000000000000000 ) ) ;
#83728 = LINE ( 'NONE', #1745, #11851 ) ;
#83729 = CARTESIAN_POINT ( 'NONE',  ( -9.999497344918166775, 7.500719060599902122, -5.000000000000000888 ) ) ;
#83730 = FACE_OUTER_BOUND ( 'NONE', #106317, .T. ) ;
#83731 = AXIS2_PLACEMENT_3D ( 'NONE', #65155, #80802, #8508 ) ;
#83732 = EDGE_LOOP ( 'NONE', ( #82844, #10223 ) ) ;
#83733 = DIRECTION ( 'NONE',  ( 0.000000000000000000, 0.000000000000000000, -1.000000000000000000 ) ) ;
#83734 = DIRECTION ( 'NONE',  ( 0.000000000000000000, -1.000000000000000000, -0.000000000000000000 ) ) ;
#83735 = CONICAL_SURFACE ( 'NONE', #28921, 2747.477419454587107, 1.221730476396026610 ) ;
#83736 = CARTESIAN_POINT ( 'NONE',  ( 31.61469319755823193, 437.7834757340932583, 21.48356015851413048 ) ) ;
#83737 = SURFACE_SIDE_STYLE ('',( #91847 ) ) ;
#83738 = LINE ( 'NONE', #58423, #2823 ) ;
#83739 = PRESENTATION_LAYER_ASSIGNMENT (  '', '', ( #85466 ) ) ;
#83740 =( GEOMETRIC_REPRESENTATION_CONTEXT ( 3 ) GLOBAL_UNCERTAINTY_ASSIGNED_CONTEXT ( ( #4891 ) ) GLOBAL_UNIT_ASSIGNED_CONTEXT ( ( #30005, #69913, #95258 ) ) REPRESENTATION_CONTEXT ( 'NONE', 'WORKASPACE' ) );
#83741 = CARTESIAN_POINT ( 'NONE',  ( 37.56673239365870387, 25.75719283951018923, 10.95617127780998956 ) ) ;
#83742 = CARTESIAN_POINT ( 'NONE',  ( -83.39409730309102997, -59.99999999999998579, 199.1218053928312770 ) ) ;
#83743 = AXIS2_PLACEMENT_3D ( 'NONE', #45640, #78516, #4649 ) ;
#83744 = AXIS2_PLACEMENT_3D ( 'NONE', #9889, #60078, #92942 ) ;
#83745 = AXIS2_PLACEMENT_3D ( 'NONE', #50331, #1227, #57355 ) ;
#83746 = CARTESIAN_POINT ( 'NONE',  ( 44.17836536378482748, 435.2619773020558682, 14.65562696767865170 ) ) ;
#83747 = ADVANCED_FACE ( 'NONE', ( #45555 ), #19717, .T. ) ;
#83748 = DIRECTION ( 'NONE',  ( 0.000000000000000000, 0.000000000000000000, -1.000000000000000000 ) ) ;
#83749 = CARTESIAN_POINT ( 'NONE',  ( -86.01685430178015679, -24.89350102973689971, 179.1283417026938878 ) ) ;
#83750 = ORIENTED_EDGE ( 'NONE', *, *, #92257, .F. ) ;
#83751 = VECTOR ( 'NONE', #103631, 1000.000000000000000 ) ;
#83752 = CIRCLE ( 'NONE', #100940, 1.999999999999999334 ) ;
#83753 = VERTEX_POINT ( 'NONE', #28325 ) ;
#83754 = CARTESIAN_POINT ( 'NONE',  ( 16.01428880459198467, 3.811183212004471521, -1.301242280779890681 ) ) ;
#83755 = DIRECTION ( 'NONE',  ( 0.000000000000000000, -1.000000000000000000, 0.000000000000000000 ) ) ;
#83756 = CARTESIAN_POINT ( 'NONE',  ( -84.49387577902174939, -45.26915323538062808, -6.724149892752078195 ) ) ;
#83757 = B_SPLINE_CURVE_WITH_KNOTS ( 'NONE', 3,
 ( #68611, #102554, #51328, #35190 ),
 .UNSPECIFIED., .F., .F.,
 ( 4, 4 ),
 ( 5.791482857413889982E-16, 0.0001919544104619767843 ),
 .UNSPECIFIED. ) ;
#83758 =( NAMED_UNIT ( * ) PLANE_ANGLE_UNIT ( ) SI_UNIT ( $, .RADIAN. ) );
#83759 = CARTESIAN_POINT ( 'NONE',  ( 17.50000000000002842, 50.00000000000000000, 100.0000000000000000 ) ) ;
#83760 = DIRECTION ( 'NONE',  ( 1.000000000000000000, 1.224606353822377258E-16, 0.000000000000000000 ) ) ;
#83761 = DIRECTION ( 'NONE',  ( -1.000000000000000000, -1.224606353822377258E-16, -0.000000000000000000 ) ) ;
#83762 = CARTESIAN_POINT ( 'NONE',  ( -55.65414010186731986, 42.00000000000000000, 72.41885610124127481 ) ) ;
#83763 = CARTESIAN_POINT ( 'NONE',  ( -22.13642162920451639, 27.78492472323463502, 32.60352800065667367 ) ) ;
#83764 = CARTESIAN_POINT ( 'NONE',  ( 74.10901235487826000, -60.00000000000013500, 189.8092491115571647 ) ) ;
#83765 = CARTESIAN_POINT ( 'NONE',  ( 5.799999999999999822, -4.618802153517009401, -8.000000000000001776 ) ) ;
#83766 = CARTESIAN_POINT ( 'NONE',  ( -56.79577812574758156, -14.21045842199439591, -31.02744264688941556 ) ) ;
#83767 = CARTESIAN_POINT ( 'NONE',  ( -68.46050526737764130, -22.10827440420577616, 87.18976234775816181 ) ) ;
#83768 = ORIENTED_EDGE ( 'NONE', *, *, #40564, .T. ) ;
#83769 = CARTESIAN_POINT ( 'NONE',  ( 78.18398495971976558, -30.00000000000001421, 185.0784753857526539 ) ) ;
#83770 = CARTESIAN_POINT ( 'NONE',  ( -23.30914976775985537, 40.83761692952442957, 60.74960289684516113 ) ) ;
#83771 = CARTESIAN_POINT ( 'NONE',  ( 94.37133057941774439, -57.65304023162428138, -12.34840853396864269 ) ) ;
#83772 = ORIENTED_EDGE ( 'NONE', *, *, #83587, .T. ) ;
#83773 = CARTESIAN_POINT ( 'NONE',  ( 14.85870402376584742, -6.955274255831150221, 13.29338602724358509 ) ) ;
#83774 = B_SPLINE_CURVE_WITH_KNOTS ( 'NONE', 3,
 ( #13892, #87816, #79704, #21505, #54341, #61025, #2759, #101991, #36249, #11371, #18999, #28149, #46810, #38735, #22028, #6329, #104508, #31197, #13362, #96440 ),
 .UNSPECIFIED., .F., .F.,
 ( 4, 2, 2, 2, 2, 2, 2, 2, 2, 4 ),
 ( 0.007065883224795808069, 0.007569382595898239974, 0.008072881967000671011, 0.008576381338103105517, 0.008828131023654322770, 0.009079880709205540024, 0.009583380080307965856, 0.01008687945141039342, 0.01059037882251281926, 0.01109387819361524682 ),
 .UNSPECIFIED. ) ;
#83775 = CARTESIAN_POINT ( 'NONE',  ( 0.000000000000000000, 0.000000000000000000, 0.000000000000000000 ) ) ;
#83776 = ORIENTED_EDGE ( 'NONE', *, *, #37754, .F. ) ;
#83777 = COLOUR_RGB ( '', 0.40784314, 0.44705882, 0.49803922) ;
#83778 = CYLINDRICAL_SURFACE ( 'NONE', #71584, 2.000000000000000444 ) ;
#83779 = CARTESIAN_POINT ( 'NONE',  ( -3.222962768498216414E-17, 13.85270131633358304, -7.000000000000011546 ) ) ;
#83780 = DIRECTION ( 'NONE',  ( 1.000000000000000000, 0.000000000000000000, 0.000000000000000000 ) ) ;
#83781 = CARTESIAN_POINT ( 'NONE',  ( 31.40588807316546038, 312.3426313771107061, -8.004124503849919137 ) ) ;
#83782 = CARTESIAN_POINT ( 'NONE',  ( 5.082755093536325930, -15.96875000204838635, -5.082755093536325042 ) ) ;
#83783 = CARTESIAN_POINT ( 'NONE',  ( -48.80564935039983965, 14.82671221253059279, 14.61894534951832192 ) ) ;
#83784 = VECTOR ( 'NONE', #68431, 1000.000000000000000 ) ;
#83785 = CARTESIAN_POINT ( 'NONE',  ( 1.459339698542529762, -0.03374778880127472791, 101.6368042612139249 ) ) ;
#83786 = CARTESIAN_POINT ( 'NONE',  ( 3.566423465315838204, -49.06946792773464239, 103.5097305745183434 ) ) ;
#83787 = CARTESIAN_POINT ( 'NONE',  ( 6.750000000000017764, 11.69134295108991317, -13.00000000000000000 ) ) ;
#83788 = CARTESIAN_POINT ( 'NONE',  ( -12.48743925095353191, -3.519139377062180607, -13.73189632760026058 ) ) ;
#83789 = CARTESIAN_POINT ( 'NONE',  ( 0.000000000000000000, 0.000000000000000000, -13.00000000000000000 ) ) ;
#83790 = ADVANCED_FACE ( 'NONE', ( #4021 ), #78074, .F. ) ;
#83791 = VERTEX_POINT ( 'NONE', #100578 ) ;
#83792 = CARTESIAN_POINT ( 'NONE',  ( -7.445751637708186266, 40.55658532066092903, -70.17153985021506912 ) ) ;
#83794 = CARTESIAN_POINT ( 'NONE',  ( 32.17265427855518567, -49.90131150188997822, 35.87558796595580901 ) ) ;
#83793 = CARTESIAN_POINT ( 'NONE',  ( 90.51111111111110574, 1.023464760207051730E-14, 0.000000000000000000 ) ) ;
#83795 = CARTESIAN_POINT ( 'NONE',  ( 35.49387599962324202, 421.8708178829924691, 6.500313947379569690 ) ) ;
#83796 = VERTEX_POINT ( 'NONE', #59613 ) ;
#83797 = EDGE_CURVE ( 'NONE', #45699, #75687, #83227, .T. ) ;
#83798 = SURFACE_STYLE_FILL_AREA ( #96939 ) ;
#83799 = ADVANCED_FACE ( 'NONE', ( #76834 ), #20255, .T. ) ;
#83800 = UNCERTAINTY_MEASURE_WITH_UNIT (LENGTH_MEASURE( 1.000000000000000082E-05 ), #3972, 'distance_accuracy_value', 'NONE');
#83801 = ORIENTED_EDGE ( 'NONE', *, *, #88658, .T. ) ;
#83803 = CARTESIAN_POINT ( 'NONE',  ( -10.00012749751951446, -4.999999999999999112, 1.308371270542952658 ) ) ;
#83802 = CARTESIAN_POINT ( 'NONE',  ( 0.4033376246892514394, -7.198601258566903915, 0.5316568767328679890 ) ) ;
#83804 = DIRECTION ( 'NONE',  ( 0.000000000000000000, 1.000000000000000000, 0.000000000000000000 ) ) ;
#83805 = CARTESIAN_POINT ( 'NONE',  ( -43.68959978692321044, 484.5138553196954376, 2.648407630516707023 ) ) ;
#83806 = APPLICATION_CONTEXT ( 'automotive_design' ) ;
#83807 = CARTESIAN_POINT ( 'NONE',  ( 10.28624191511840458, 43.25714326066859172, 15.40779740156149202 ) ) ;
#83808 = CARTESIAN_POINT ( 'NONE',  ( 33.00000000000000000, 450.0000000000002274, 28.20242257375372219 ) ) ;
#83809 = CARTESIAN_POINT ( 'NONE',  ( 0.8444424525834832718, 13.67360963902750903, -51.42495577429150444 ) ) ;
#83810 = ORIENTED_EDGE ( 'NONE', *, *, #45983, .F. ) ;
#83811 = CARTESIAN_POINT ( 'NONE',  ( 91.38620944121281298, -60.00000000000000711, -15.95155868622245521 ) ) ;
#83812 = PRESENTATION_LAYER_ASSIGNMENT (  '', '', ( #13126 ) ) ;
#83813 = CARTESIAN_POINT ( 'NONE',  ( 32.89532852795907303, 465.6911463857187528, 10.83018753746880236 ) ) ;
#83814 = CARTESIAN_POINT ( 'NONE',  ( -15.89515006508820960, -2.031693691641069055, 14.86243156795516640 ) ) ;
#83815 = EDGE_CURVE ( 'NONE', #93278, #77883, #27813, .T. ) ;
#83816 = CARTESIAN_POINT ( 'NONE',  ( 39.19378338565743292, 489.8656698032318104, 11.78649807965894603 ) ) ;
#83817 = CARTESIAN_POINT ( 'NONE',  ( 57.70539558375507738, 6.856755485862130937E-15, 0.000000000000000000 ) ) ;
#83818 = ORIENTED_EDGE ( 'NONE', *, *, #34199, .T. ) ;
#83819 = FACE_OUTER_BOUND ( 'NONE', #11193, .T. ) ;
#83820 = VERTEX_POINT ( 'NONE', #52554 ) ;
#83821 = ORIENTED_EDGE ( 'NONE', *, *, #74472, .T. ) ;
#83822 = CARTESIAN_POINT ( 'NONE',  ( 7.618844049274130725, 81.82764101070543461, 2.450177051822845620 ) ) ;
#83823 = CARTESIAN_POINT ( 'NONE',  ( 6.289692432696806890, -5.239086202715462548, -4.583616368338172542 ) ) ;
#83824 = CARTESIAN_POINT ( 'NONE',  ( -16.42642030348412518, 34.33441478758428644, -24.26661104398729663 ) ) ;
#83825 = CARTESIAN_POINT ( 'NONE',  ( 0.000000000000000000, 0.000000000000000000, -4.814498510800145681 ) ) ;
#83827 = CARTESIAN_POINT ( 'NONE',  ( 82.19860323403510449, -37.81518911496591784, -13.38202468312296389 ) ) ;
#83826 = AXIS2_PLACEMENT_3D ( 'NONE', #88416, #6406, #104049 ) ;
#83828 = AXIS2_PLACEMENT_3D ( 'NONE', #91990, #2442, #75260 ) ;
#83829 = CARTESIAN_POINT ( 'NONE',  ( -41.09174544714365851, 313.3976221602537180, -5.572537511513111497 ) ) ;
#83830 = DIRECTION ( 'NONE',  ( 0.000000000000000000, 1.000000000000000000, 0.000000000000000000 ) ) ;
#83831 = CARTESIAN_POINT ( 'NONE',  ( 12.50000000000000711, 34.80611260448990407, -54.08410186685180321 ) ) ;
#83832 = ORIENTED_EDGE ( 'NONE', *, *, #14482, .F. ) ;
#83833 = CARTESIAN_POINT ( 'NONE',  ( 30.59999999999999787, 3.309500000000003439, 0.000000000000000000 ) ) ;
#83834 = ORIENTED_EDGE ( 'NONE', *, *, #9827, .T. ) ;
#83835 = CARTESIAN_POINT ( 'NONE',  ( 9.182800793770848458, 51.37232910640911854, -3.876820685372471154 ) ) ;
#83836 = CARTESIAN_POINT ( 'NONE',  ( 3.801077171203065319, -48.88909605940821734, 104.1059035333590828 ) ) ;
#83837 = AXIS2_PLACEMENT_3D ( 'NONE', #70716, #86391, #4921 ) ;
#83838 = VECTOR ( 'NONE', #104564, 1000.000000000000227 ) ;
#83839 = AXIS2_PLACEMENT_3D ( 'NONE', #93475, #79919, #79395 ) ;
#83841 = ORIENTED_EDGE ( 'NONE', *, *, #58259, .T. ) ;
#83840 = LINE ( 'NONE', #101632, #78645 ) ;
#83842 = CARTESIAN_POINT ( 'NONE',  ( 71.46833319993017142, -32.53831864036357047, 102.5522570331628458 ) ) ;
#83843 = AXIS2_PLACEMENT_3D ( 'NONE', #48869, #32192, #97420 ) ;
#83844 = ORIENTED_EDGE ( 'NONE', *, *, #52739, .F. ) ;
#83845 = CARTESIAN_POINT ( 'NONE',  ( 4.999999999999995559, -46.00000000000000000, 42.58845726811990318 ) ) ;
#83847 = CARTESIAN_POINT ( 'NONE',  ( 0.000000000000000000, 50.00000000000000000, 0.000000000000000000 ) ) ;
#83846 = COLOUR_RGB ( '', 0.72549020, 0.75294118, 0.79215686) ;
#83848 = CARTESIAN_POINT ( 'NONE',  ( -7.188101187500000933, -23.00000000204839523, -2.977408999572651371 ) ) ;
#83849 = CARTESIAN_POINT ( 'NONE',  ( -93.81425292840387442, -57.67376786465794680, 13.59058164905135513 ) ) ;
#83850 = EDGE_LOOP ( 'NONE', ( #55935, #52885, #34291, #22018, #78186, #71661 ) ) ;
#83851 = CARTESIAN_POINT ( 'NONE',  ( -37.50059943756144776, 490.7879993827797307, 12.38039871356719246 ) ) ;
#83852 = CARTESIAN_POINT ( 'NONE',  ( 104.7030407962678282, -52.71701985175332794, 182.7871775134649113 ) ) ;
#83853 = CARTESIAN_POINT ( 'NONE',  ( -32.84237740334621236, 485.2251842821281116, 5.746442123025396143 ) ) ;
#83854 = EDGE_CURVE ( 'NONE', #26294, #63024, #29906, .T. ) ;
#83855 = DIRECTION ( 'NONE',  ( -1.000000000000000000, -0.000000000000000000, -0.000000000000000000 ) ) ;
#83856 = CARTESIAN_POINT ( 'NONE',  ( -3.313708498984760720, -25.71875000409677625, -8.000000000000000000 ) ) ;
#83857 = DIRECTION ( 'NONE',  ( 0.000000000000000000, -1.000000000000000000, 0.000000000000000000 ) ) ;
#83858 = DIRECTION ( 'NONE',  ( -1.000000000000000000, -1.224606353822377258E-16, -0.000000000000000000 ) ) ;
#83859 = CARTESIAN_POINT ( 'NONE',  ( 83.86866073052654258, 1.030564683017419500E-14, 0.000000000000000000 ) ) ;
#83860 = AXIS2_PLACEMENT_3D ( 'NONE', #25049, #26138, #74091 ) ;
#83861 = CARTESIAN_POINT ( 'NONE',  ( -36.97266421102955292, 437.4722577378113328, 4.366281382744582551 ) ) ;
#83862 = FACE_OUTER_BOUND ( 'NONE', #101146, .T. ) ;
#83863 = DIRECTION ( 'NONE',  ( 0.000000000000000000, 0.000000000000000000, 1.000000000000000000 ) ) ;
#83864 = DIRECTION ( 'NONE',  ( 0.000000000000000000, 1.000000000000000000, -0.000000000000000000 ) ) ;
#83865 = ORIENTED_EDGE ( 'NONE', *, *, #88264, .T. ) ;
#83866 = CARTESIAN_POINT ( 'NONE',  ( 82.42421628608209971, 5.000000000000021316, 0.000000000000000000 ) ) ;
#83867 = FACE_OUTER_BOUND ( 'NONE', #94852, .T. ) ;
#83868 = MECHANICAL_DESIGN_GEOMETRIC_PRESENTATION_REPRESENTATION (  '', ( #37339 ), #104501 ) ;
#83869 = CARTESIAN_POINT ( 'NONE',  ( 0.9981243769357334150, 8.900829104547275605, 51.25576959928475418 ) ) ;
#83870 = CARTESIAN_POINT ( 'NONE',  ( -84.25106516082894359, -30.00000000000000355, 163.2648472752855184 ) ) ;
#83871 = ORIENTED_EDGE ( 'NONE', *, *, #7144, .T. ) ;
#83872 = ORIENTED_EDGE ( 'NONE', *, *, #31727, .F. ) ;
#83873 = CARTESIAN_POINT ( 'NONE',  ( 37.72778265019833555, 25.42095348269468857, -13.45617127781092215 ) ) ;
#83874 = CARTESIAN_POINT ( 'NONE',  ( 67.63584330748660989, -57.68118349180133464, 139.1929817678663994 ) ) ;
#83876 = CARTESIAN_POINT ( 'NONE',  ( -8.719197186943313582, 53.90628269159294206, 1.531152949374563699 ) ) ;
#83875 = CARTESIAN_POINT ( 'NONE',  ( -15.45341029905986829, 2.829415941280664981, -2.060260514156198486 ) ) ;
#83877 = CARTESIAN_POINT ( 'NONE',  ( 46.71504066713215053, -34.79384376595470485, -36.65170777883916031 ) ) ;
#83878 =( NAMED_UNIT ( * ) PLANE_ANGLE_UNIT ( ) SI_UNIT ( $, .RADIAN. ) );
#83879 = CARTESIAN_POINT ( 'NONE',  ( -43.53171589075616055, -60.00000000000002132, 57.82064124434394614 ) ) ;
#83880 = PRESENTATION_LAYER_ASSIGNMENT (  '', '', ( #77035 ) ) ;
#83881 = CARTESIAN_POINT ( 'NONE',  ( 60.14984002819952025, 4.000000000000015099, 4.898587196589422689E-16 ) ) ;
#83882 = EDGE_CURVE ( 'NONE', #74417, #39260, #11872, .T. ) ;
#83883 = CONICAL_SURFACE ( 'NONE', #82109, 22.55262289886175964, 1.221730476396026388 ) ;
#83884 = CARTESIAN_POINT ( 'NONE',  ( -86.68224123219718535, -24.39526350757373052, 184.9923197224934484 ) ) ;
#83885 = VERTEX_POINT ( 'NONE', #103769 ) ;
#83886 = CARTESIAN_POINT ( 'NONE',  ( 30.74966693359977299, 13.13370859069518204, 41.50962874632922706 ) ) ;
#83887 = CARTESIAN_POINT ( 'NONE',  ( -1.994277754766871968, -29.03106682059618748, 28.72592687327638217 ) ) ;
#83888 = DIRECTION ( 'NONE',  ( 0.000000000000000000, 0.000000000000000000, 1.000000000000000000 ) ) ;
#83889 = CARTESIAN_POINT ( 'NONE',  ( -3.454253436624922458, -49.15858197120396511, 103.7259032015043090 ) ) ;
#83890 =( BOUNDED_SURFACE ( )  B_SPLINE_SURFACE ( 2, 3, ( 
 ( #3326, #36273, #20093, #27647, #93410, #84777, #51863, #52395, #100952, #19560, #2240, #11395, #77753, #93936, #3864, #28704, #61585, #94479, #27109, #34668, #102012, #85308, #1715, #60001, #36796, #69662, #19024, #10862, #67540, #44320, #78792, #37326, #31354, #70719 ),
 ( #62123, #29242, #53980, #70186, #95013, #30277, #38373, #64233, #96591, #38890, #22727, #47484, #23246, #21148, #103611, #22190, #71237, #104132, #55564, #45392, #12462, #78272, #79331, #103093, #79856, #97105, #86918, #88500, #6494, #14578, #80382, #21664, #12989, #45915 ),
 ( #4926, #63164, #39426, #37858, #72301, #29760, #46956, #5964, #105207, #96060, #5452, #54501, #87445, #55040, #62635, #46442, #95523, #87972, #86396, #30820, #63706, #4385, #13523, #14052, #71758, #104667, #82519, #106781, #74939, #40464, #50144, #489, #25380, #32402 ) ),
 .UNSPECIFIED., .F., .T., .F. ) 
 B_SPLINE_SURFACE_WITH_KNOTS ( ( 3, 3 ),
 ( 4, 2, 2, 2, 2, 2, 2, 2, 2, 2, 2, 2, 2, 2, 2, 2, 4 ),
 ( 0.000000000000000000, 1.000000000000000000 ),
 ( 0.000000000000000000, 0.3926990816987241395, 0.7853981633974482790, 1.178097245096172418, 1.570796326794896558, 1.963495408493620697, 2.356194490192344837, 2.748893571891068976, 3.141592653589793116, 3.534291735288517255, 3.926990816987241395, 4.319689898685965090, 4.712388980384689674, 5.105088062083414258, 5.497787143782137953, 5.890486225480861648, 6.283185307179586232 ),
 .UNSPECIFIED. ) 
 GEOMETRIC_REPRESENTATION_ITEM ( )  RATIONAL_B_SPLINE_SURFACE ( (
 ( 1.000000000000000000, 1.000000000000000000, 1.000000000000000000, 1.000000000000000000, 1.000000000000000000, 1.000000000000000000, 1.000000000000000000, 1.000000000000000000, 1.000000000000000000, 1.000000000000000000, 1.000000000000000000, 1.000000000000000000, 1.000000000000000000, 1.000000000000000000, 1.000000000000000000, 1.000000000000000000, 1.000000000000000000, 1.000000000000000000, 1.000000000000000000, 1.000000000000000000, 1.000000000000000000, 1.000000000000000000, 1.000000000000000000, 1.000000000000000000, 1.000000000000000000, 1.000000000000000000, 1.000000000000000000, 1.000000000000000000, 1.000000000000000000, 1.000000000000000000, 1.000000000000000000, 1.000000000000000000, 1.000000000000000000, 1.000000000000000000),
 ( 1.857142857142858317, 1.857142857142858317, 1.857142857142858317, 1.857142857142858317, 1.857142857142858317, 1.857142857142858317, 1.857142857142858317, 1.857142857142858317, 1.857142857142858317, 1.857142857142858317, 1.857142857142858317, 1.857142857142858317, 1.857142857142858317, 1.857142857142858317, 1.857142857142858317, 1.857142857142858317, 1.857142857142858317, 1.857142857142858317, 1.857142857142858317, 1.857142857142858317, 1.857142857142858317, 1.857142857142858317, 1.857142857142858317, 1.857142857142858317, 1.857142857142858317, 1.857142857142858317, 1.857142857142858317, 1.857142857142858317, 1.857142857142858317, 1.857142857142858317, 1.857142857142858317, 1.857142857142858317, 1.857142857142858317, 1.857142857142858317),
 ( 1.000000000000000000, 1.000000000000000000, 1.000000000000000000, 1.000000000000000000, 1.000000000000000000, 1.000000000000000000, 1.000000000000000000, 1.000000000000000000, 1.000000000000000000, 1.000000000000000000, 1.000000000000000000, 1.000000000000000000, 1.000000000000000000, 1.000000000000000000, 1.000000000000000000, 1.000000000000000000, 1.000000000000000000, 1.000000000000000000, 1.000000000000000000, 1.000000000000000000, 1.000000000000000000, 1.000000000000000000, 1.000000000000000000, 1.000000000000000000, 1.000000000000000000, 1.000000000000000000, 1.000000000000000000, 1.000000000000000000, 1.000000000000000000, 1.000000000000000000, 1.000000000000000000, 1.000000000000000000, 1.000000000000000000, 1.000000000000000000) ) ) 
 REPRESENTATION_ITEM ( '' )  SURFACE ( )  );
#83892 = CARTESIAN_POINT ( 'NONE',  ( 5.795768137672492770, -65.04849424565485094, 14.25540627950699246 ) ) ;
#83891 = CARTESIAN_POINT ( 'NONE',  ( 33.74271564777244237, 484.1802673187708592, 2.058285076122321922 ) ) ;
#83893 = ORIENTED_EDGE ( 'NONE', *, *, #30394, .F. ) ;
#83894 = CARTESIAN_POINT ( 'NONE',  ( -36.29465277445844151, 352.4908535429611902, 1.226005505992772804 ) ) ;
#83895 = CARTESIAN_POINT ( 'NONE',  ( 0.5680194430980197717, 28.15644683432188700, 38.38337714611267870 ) ) ;
#83896 = DIRECTION ( 'NONE',  ( -1.000000000000000000, -0.000000000000000000, 0.000000000000000000 ) ) ;
#83897 = VECTOR ( 'NONE', #36060, 1000.000000000000000 ) ;
#83898 = CARTESIAN_POINT ( 'NONE',  ( 23.63566405412713323, 303.4845845294884725, -9.864010225974007895 ) ) ;
#83899 = CARTESIAN_POINT ( 'NONE',  ( 30.95643954367146833, 313.8918926584737505, -7.857037206977866006 ) ) ;
#83900 = FILL_AREA_STYLE ('',( #26251 ) ) ;
#83901 = CARTESIAN_POINT ( 'NONE',  ( 0.000000000000000000, -3.331654917651224235, 0.000000000000000000 ) ) ;
#83902 = CARTESIAN_POINT ( 'NONE',  ( 114.5100518737696689, -60.00000000000002132, 177.0882855716755557 ) ) ;
#83903 = CARTESIAN_POINT ( 'NONE',  ( -83.89923350218229814, -18.67999242611703536, 147.1925220706413597 ) ) ;
#83904 = ORIENTED_EDGE ( 'NONE', *, *, #77608, .F. ) ;
#83905 = CARTESIAN_POINT ( 'NONE',  ( -4.852941176470598528, -3.000000000000002665, -70.80672828634229177 ) ) ;
#83906 = CARTESIAN_POINT ( 'NONE',  ( 0.000000000000000000, 0.000000000000000000, 0.000000000000000000 ) ) ;
#83907 = AXIS2_PLACEMENT_3D ( 'NONE', #105203, #24315, #46438 ) ;
#83908 = CARTESIAN_POINT ( 'NONE',  ( 43.00000000000000000, 484.2804969086081996, -2.982821241663323075 ) ) ;
#83909 = AXIS2_PLACEMENT_3D ( 'NONE', #31765, #24217, #66229 ) ;
#83910 = AXIS2_PLACEMENT_3D ( 'NONE', #104605, #15593, #49009 ) ;
#83911 = CARTESIAN_POINT ( 'NONE',  ( 6.463178677061754307, -2.643201791673487122, -6.839998497243183095 ) ) ;
#83912 = CARTESIAN_POINT ( 'NONE',  ( 2.869469304594349790, 64.67108097164965841, -5.000000000000001776 ) ) ;
#83913 = FACE_OUTER_BOUND ( 'NONE', #100557, .T. ) ;
#83914 = ORIENTED_EDGE ( 'NONE', *, *, #76182, .F. ) ;
#83915 = UNCERTAINTY_MEASURE_WITH_UNIT (LENGTH_MEASURE( 1.000000000000000082E-05 ), #62526, 'distance_accuracy_value', 'NONE');
#83917 = AXIS2_PLACEMENT_3D ( 'NONE', #41048, #90662, #73931 ) ;
#83916 = CARTESIAN_POINT ( 'NONE',  ( -23.29322033388968904, 305.8372712004871801, 10.15257527089631751 ) ) ;
#83918 = ORIENTED_EDGE ( 'NONE', *, *, #25067, .F. ) ;
#83919 = CARTESIAN_POINT ( 'NONE',  ( 16.64348903516512834, -1.200000000000000030E-05, -5.407797401561770023 ) ) ;
#83920 = CIRCLE ( 'NONE', #51250, 4.250000000000000000 ) ;
#83921 = CARTESIAN_POINT ( 'NONE',  ( 0.7408669144222883585, 15.11700796859930307, 9.999999999997886135 ) ) ;
#83922 = CARTESIAN_POINT ( 'NONE',  ( 31.96903519139344141, 486.7815514870802076, 6.755070114929473846 ) ) ;
#83923 = CARTESIAN_POINT ( 'NONE',  ( -11.54772599577038505, 50.00000000000000000, 62.20121126512094634 ) ) ;
#83924 = CARTESIAN_POINT ( 'NONE',  ( 5.000000000000000000, -13.89959410954354802, 11.33893914917864087 ) ) ;
#83925 = CARTESIAN_POINT ( 'NONE',  ( 30.00000000000000000, 0.000000000000000000, 9.000000000000000000 ) ) ;
#83926 = EDGE_LOOP ( 'NONE', ( #96522, #95145, #2711, #56891 ) ) ;
#83927 = CARTESIAN_POINT ( 'NONE',  ( 97.11419591411292629, -60.00000000000001421, 63.44341482763463347 ) ) ;
#83929 = CARTESIAN_POINT ( 'NONE',  ( 21.04530086232624342, -29.03383587574997904, 29.34416034787003724 ) ) ;
#83928 = CARTESIAN_POINT ( 'NONE',  ( -78.42690035548760363, -14.21045842199427156, 178.5095186877798028 ) ) ;
#83930 = CARTESIAN_POINT ( 'NONE',  ( -1.145927044342081135E-15, 61.34242035161803841, 9.357204421225127078 ) ) ;
#83931 = LINE ( 'NONE', #49965, #25 ) ;
#83932 = CARTESIAN_POINT ( 'NONE',  ( -42.40463338888051226, -18.78660199041541290, 35.79879680396032171 ) ) ;
#83933 = CIRCLE ( 'NONE', #18514, 5.000000000000011546 ) ;
#83934 = CARTESIAN_POINT ( 'NONE',  ( 0.000000000000000000, 4.898587196589412829E-16, -4.000000000000000000 ) ) ;
#83935 = UNCERTAINTY_MEASURE_WITH_UNIT (LENGTH_MEASURE( 1.000000000000000082E-05 ), #104781, 'distance_accuracy_value', 'NONE');
#83936 = B_SPLINE_CURVE_WITH_KNOTS ( 'NONE', 3,
 ( #23878, #56722, #40030, #582, #89644, #66418, #15745, #65366, #48628, #106330, #24411, #90170, #82064, #10822, #84208, #43744, #2203, #67500, #101973, #42680, #52903, #28134, #26544, #93370, #17896, #60491, #35697, #76633, #51824, #85270 ),
 .UNSPECIFIED., .F., .F.,
 ( 4, 2, 2, 1, 1, 1, 2, 2, 2, 2, 2, 1, 2, 2, 2, 2, 4 ),
 ( 0.000000000000000000, 0.1249999999998845923, 0.1874999999998268885, 0.2187499999997968292, 0.2343749999997817579, 0.2421874999997729871, 0.2460937499997698230, 0.2499999999997666589, 0.3749999999998109290, 0.4374999999998330225, 0.4687499999998432365, 0.4843749999998492317, 0.4921874999998513966, 0.4999999999998535616, 0.6249999999998900879, 0.7499999999999267253, 1.000000000000000000 ),
 .UNSPECIFIED. ) ;
#83937 = ORIENTED_EDGE ( 'NONE', *, *, #24170, .F. ) ;
#83938 = CARTESIAN_POINT ( 'NONE',  ( -5.833333333333328596, -46.00000000000000000, 103.8776713793258608 ) ) ;
#83939 = CARTESIAN_POINT ( 'NONE',  ( 37.04388863813380794, 311.3287000699716032, 13.89786840526617517 ) ) ;
#83940 = LINE ( 'NONE', #76913, #52647 ) ;
#83941 = FACE_OUTER_BOUND ( 'NONE', #96681, .T. ) ;
#83942 = DIRECTION ( 'NONE',  ( -0.000000000000000000, -1.000000000000000000, -0.000000000000000000 ) ) ;
#83943 = ORIENTED_EDGE ( 'NONE', *, *, #10236, .F. ) ;
#83944 = CARTESIAN_POINT ( 'NONE',  ( -15.90885615318869029, 37.20836610827222302, -22.13023378396306384 ) ) ;
#83945 = ORIENTED_EDGE ( 'NONE', *, *, #40870, .T. ) ;
#83946 = CARTESIAN_POINT ( 'NONE',  ( 81.20719313386280191, -29.99999999999995026, 0.8620750168147771619 ) ) ;
#83947 = CARTESIAN_POINT ( 'NONE',  ( 47.29503607946699617, 13.12332669628137438, 14.58854632476099766 ) ) ;
#83948 = CARTESIAN_POINT ( 'NONE',  ( 44.46823338009918558, 1.482358050883964840E-15, 0.000000000000000000 ) ) ;
#83949 = CIRCLE ( 'NONE', #51128, 7.500000000000000000 ) ;
#83951 = EDGE_CURVE ( 'NONE', #23889, #1638, #8052, .T. ) ;
#83950 = LINE ( 'NONE', #74256, #51508 ) ;
#83952 = CARTESIAN_POINT ( 'NONE',  ( 81.50579677117252686, -29.99999999999999645, 28.64214509496276051 ) ) ;
#83953 = ADVANCED_FACE ( 'NONE', ( #55202 ), #24676, .F. ) ;
#83954 = CARTESIAN_POINT ( 'NONE',  ( -30.00226090868998696, 322.3790423074855198, 14.50231502595238453 ) ) ;
#83955 = ORIENTED_EDGE ( 'NONE', *, *, #24427, .F. ) ;
#83956 = EDGE_LOOP ( 'NONE', ( #46887, #24037, #40015, #49796 ) ) ;
#83957 = ORIENTED_EDGE ( 'NONE', *, *, #102543, .T. ) ;
#83958 =( GEOMETRIC_REPRESENTATION_CONTEXT ( 3 ) GLOBAL_UNCERTAINTY_ASSIGNED_CONTEXT ( ( #100913 ) ) GLOBAL_UNIT_ASSIGNED_CONTEXT ( ( #40443, #15101, #105186 ) ) REPRESENTATION_CONTEXT ( 'NONE', 'WORKASPACE' ) );
#83959 = CARTESIAN_POINT ( 'NONE',  ( -46.97231841192009227, 12.59348177918413825, -16.28806988207291440 ) ) ;
#83960 = CARTESIAN_POINT ( 'NONE',  ( -3.308895880083044805, 303.8518027751322848, 9.936999415074330599 ) ) ;
#83961 = DIRECTION ( 'NONE',  ( 1.000000000000000000, -0.000000000000000000, -0.000000000000000000 ) ) ;
#83962 = CARTESIAN_POINT ( 'NONE',  ( -31.15872997657971410, 428.0413696779457382, 24.54324983164422136 ) ) ;
#83963 = CARTESIAN_POINT ( 'NONE',  ( -3.400000000000000355, 4.163799117101001052E-16, -5.283275477074182547 ) ) ;
#83964 = CONICAL_SURFACE ( 'NONE', #30633, 5.000000000000001776, 0.9599310885968803664 ) ;
#83965 = EDGE_LOOP ( 'NONE', ( #72613, #5818, #81570, #78917, #94836 ) ) ;
#83966 = CARTESIAN_POINT ( 'NONE',  ( 8.737863884124120517, 49.99999999999999289, -90.03618980230058355 ) ) ;
#83967 = ORIENTED_EDGE ( 'NONE', *, *, #64618, .F. ) ;
#83968 = CARTESIAN_POINT ( 'NONE',  ( 33.07276483573531323, 438.9325140356083921, 23.89537236861360014 ) ) ;
#83969 = CARTESIAN_POINT ( 'NONE',  ( 76.07586837099985644, -38.38264828878220669, 178.9567494468272741 ) ) ;
#83970 = DIRECTION ( 'NONE',  ( -0.000000000000000000, -1.000000000000000000, -0.000000000000000000 ) ) ;
#83971 = CARTESIAN_POINT ( 'NONE',  ( 35.82669496149354416, 304.5988386916886839, 4.195970393794294928 ) ) ;
#83972 = DIRECTION ( 'NONE',  ( 0.000000000000000000, 0.000000000000000000, 1.000000000000000000 ) ) ;
#83973 = VECTOR ( 'NONE', #103097, 1000.000000000000000 ) ;
#83974 = VERTEX_POINT ( 'NONE', #13684 ) ;
#83975 = DIRECTION ( 'NONE',  ( 0.000000000000000000, -1.000000000000000000, 0.000000000000000000 ) ) ;
#83976 = CARTESIAN_POINT ( 'NONE',  ( -1.469576158976823947E-15, -10.06250000409677092, 8.000000000000000000 ) ) ;
#83977 = CARTESIAN_POINT ( 'NONE',  ( 89.64643850830432825, 1.030564683017419500E-14, 0.000000000000000000 ) ) ;
#83978 = DIRECTION ( 'NONE',  ( -1.000000000000000000, 0.000000000000000000, 0.000000000000000000 ) ) ;
#83979 = ORIENTED_EDGE ( 'NONE', *, *, #77049, .F. ) ;
#83981 = CARTESIAN_POINT ( 'NONE',  ( -21.88255344520474921, 294.9922948560505915, 9.966861928665570858 ) ) ;
#83980 = SURFACE_SIDE_STYLE ('',( #93144 ) ) ;
#83982 = CARTESIAN_POINT ( 'NONE',  ( 8.013529827547630546, 54.15025421630311087, -1.653736085047024851 ) ) ;
#83983 = UNCERTAINTY_MEASURE_WITH_UNIT (LENGTH_MEASURE( 1.000000000000000082E-05 ), #9844, 'distance_accuracy_value', 'NONE');
#83984 = CARTESIAN_POINT ( 'NONE',  ( 20.00000000000000000, 12.99999999999999289, 0.000000000000000000 ) ) ;
#83985 = CARTESIAN_POINT ( 'NONE',  ( -43.94956565205965404, 434.7294131184608545, 8.824837262795423243 ) ) ;
#83987 = FACE_OUTER_BOUND ( 'NONE', #27912, .T. ) ;
#83986 = AXIS2_PLACEMENT_3D ( 'NONE', #63096, #6963, #64170 ) ;
#83988 = FILL_AREA_STYLE_COLOUR ( '', #71957 ) ;
#83989 = EDGE_CURVE ( 'NONE', #14996, #91623, #45328, .T. ) ;
#83990 = AXIS2_PLACEMENT_3D ( 'NONE', #91848, #42762, #75653 ) ;
#83991 = CIRCLE ( 'NONE', #37534, 4.172000000000001485 ) ;
#83992 = DIRECTION ( 'NONE',  ( -0.5735764363510494901, -0.8191520442889894671, 0.000000000000000000 ) ) ;
#83993 = CIRCLE ( 'NONE', #97757, 1.999999999999998890 ) ;
#83994 = CARTESIAN_POINT ( 'NONE',  ( 84.61807758326956730, -53.82215636532191638, 190.0709679738065745 ) ) ;
#83995 = B_SPLINE_CURVE_WITH_KNOTS ( 'NONE', 3,
 ( #47640, #61746, #103245, #71932, #45552, #104837, #39586, #102711, #28875, #29390, #13146, #62275, #94644, #20788, #53622, #95162, #86557, #12615, #21295, #54131 ),
 .UNSPECIFIED., .F., .F.,
 ( 4, 2, 2, 2, 2, 2, 2, 2, 2, 4 ),
 ( 0.006339153383469499359, 0.006843475872017545751, 0.007347798360565592143, 0.007599959604839613171, 0.007852120849113634199, 0.008356443337661681459, 0.008860765826209728718, 0.009365088314757775978, 0.009869410803305823238, 0.01037373329185387050 ),
 .UNSPECIFIED. ) ;
#83996 = CARTESIAN_POINT ( 'NONE',  ( 4.898587196589412829E-16, -25.81250000409677270, -8.000000000000000000 ) ) ;
#83997 = CARTESIAN_POINT ( 'NONE',  ( -8.568812041302383165, 127.6722392238321078, 4.999999999999365841 ) ) ;
#83998 = ORIENTED_EDGE ( 'NONE', *, *, #79278, .T. ) ;
#83999 = CARTESIAN_POINT ( 'NONE',  ( 91.48116923616865392, -57.66238768136772563, -20.18913141313222681 ) ) ;
#84000 = CARTESIAN_POINT ( 'NONE',  ( 30.00000000000000000, 0.000000000000000000, -6.000000000000012434 ) ) ;
#84001 = CARTESIAN_POINT ( 'NONE',  ( 16.11237705540419185, 35.08085309292203391, -21.97963608747229358 ) ) ;
#84002 = CARTESIAN_POINT ( 'NONE',  ( -82.36074577633510785, -30.00000000000000355, 37.46041508329808778 ) ) ;
#84003 = EDGE_CURVE ( 'NONE', #66540, #82760, #32026, .T. ) ;
#84004 = EDGE_CURVE ( 'NONE', #23499, #18245, #91319, .T. ) ;
#84005 = CIRCLE ( 'NONE', #27231, 0.9999999999999992228 ) ;
#84006 = DIRECTION ( 'NONE',  ( -0.000000000000000000, -1.000000000000000000, -0.000000000000000000 ) ) ;
#84007 = CARTESIAN_POINT ( 'NONE',  ( -4.419133455862510829, 6.108866147517284517, -7.026396753507433424 ) ) ;
#84009 = CARTESIAN_POINT ( 'NONE',  ( -32.87494462546125362, 485.1684504739463932, 5.618872456255630254 ) ) ;
#84008 = CARTESIAN_POINT ( 'NONE',  ( 36.12276851866623417, 490.9183493301041494, 12.43853037509677151 ) ) ;
#84010 = CIRCLE ( 'NONE', #59941, 11.27631144943088337 ) ;
#84011 = CARTESIAN_POINT ( 'NONE',  ( 99.75754961941544252, -5.000000000000000000, 6.123233995736778115E-16 ) ) ;
#84012 = CARTESIAN_POINT ( 'NONE',  ( -19.67392556837618400, -25.14117008353909455, 28.53997366849857542 ) ) ;
#84013 = CARTESIAN_POINT ( 'NONE',  ( -37.67992928263237218, 491.6871197847713688, 12.48602433195068073 ) ) ;
#84014 = CARTESIAN_POINT ( 'NONE',  ( 5.093234209761996922, -82.55532226535090956, 3.176141468578046023 ) ) ;
#84015 = CARTESIAN_POINT ( 'NONE',  ( -22.45489971457653766, 25.48429075023468471, 32.95935593634655447 ) ) ;
#84016 = CARTESIAN_POINT ( 'NONE',  ( 4.449746416242592429E-16, -5.788408252967910173, -2.974182810908588603 ) ) ;
#84017 = CARTESIAN_POINT ( 'NONE',  ( 46.14432154257043806, -26.57843610561197423, -28.93710014874023528 ) ) ;
#84018 = CIRCLE ( 'NONE', #94354, 5.000000000000011546 ) ;
#84019 = EDGE_CURVE ( 'NONE', #45240, #89868, #6725, .T. ) ;
#84020 = CARTESIAN_POINT ( 'NONE',  ( -23.46199991564613896, -32.51939257062084465, 30.27833130048637855 ) ) ;
#84021 = ORIENTED_EDGE ( 'NONE', *, *, #85655, .T. ) ;
#84022 = CARTESIAN_POINT ( 'NONE',  ( 5.890693798151877658, 11.69020577517987114, 3.781785903083255018 ) ) ;
#84023 = CARTESIAN_POINT ( 'NONE',  ( -9.843039827103241990, 108.5908350250833649, -1.781495459429543127 ) ) ;
#84024 = DIRECTION ( 'NONE',  ( 0.000000000000000000, -1.000000000000000000, 0.000000000000000000 ) ) ;
#84025 = CARTESIAN_POINT ( 'NONE',  ( -63.85241486307079128, -29.65655549946883340, -23.53290650701330833 ) ) ;
#84026 = EDGE_CURVE ( 'NONE', #9728, #4234, #25548, .T. ) ;
#84028 = DIRECTION ( 'NONE',  ( -1.000000000000000000, -0.000000000000000000, -0.000000000000000000 ) ) ;
#84027 = CYLINDRICAL_SURFACE ( 'NONE', #69180, 1.250000000000001110 ) ;
#84029 = EDGE_LOOP ( 'NONE', ( #5629, #40189, #68775, #32236, #9756 ) ) ;
#84030 = CARTESIAN_POINT ( 'NONE',  ( 6.287679341995262128, -1.331405739688502399, -6.828854810278215837 ) ) ;
#84031 = ORIENTED_EDGE ( 'NONE', *, *, #6203, .T. ) ;
#84032 = DIRECTION ( 'NONE',  ( -0.000000000000000000, 1.000000000000000000, -0.000000000000000000 ) ) ;
#84033 = CIRCLE ( 'NONE', #73705, 55.00000000000000000 ) ;
#84034 = CARTESIAN_POINT ( 'NONE',  ( 15.91318055706407186, 3.411564560433875570, 2.528039842346805344 ) ) ;
#84035 = ADVANCED_FACE ( 'NONE', ( #87218 ), #52195, .T. ) ;
#84036 = CARTESIAN_POINT ( 'NONE',  ( -1.469576158976823947E-15, -23.56250000409677270, 8.000000000000000000 ) ) ;
#84037 = ORIENTED_EDGE ( 'NONE', *, *, #96914, .T. ) ;
#84038 = CARTESIAN_POINT ( 'NONE',  ( -7.577625347064596895, 54.07946387534607879, -3.571027979463019975 ) ) ;
#84039 = CARTESIAN_POINT ( 'NONE',  ( 99.38929497627960075, -45.26971556542965658, 193.0884266367296505 ) ) ;
#84040 = COLOUR_RGB ( '', 0.31764706, 0.68627451, 0.89019608) ;
#84042 = CARTESIAN_POINT ( 'NONE',  ( -4.225130582364203136, -1.061186173226825069, 104.4756880579355283 ) ) ;
#84041 = DIRECTION ( 'NONE',  ( 0.000000000000000000, 1.000000000000000000, 0.000000000000000000 ) ) ;
#84043 = AXIS2_PLACEMENT_3D ( 'NONE', #46715, #22999, #69940 ) ;
#84044 = ORIENTED_EDGE ( 'NONE', *, *, #104574, .F. ) ;
#84045 = ORIENTED_EDGE ( 'NONE', *, *, #106185, .F. ) ;
#84046 = VERTEX_POINT ( 'NONE', #95308 ) ;
#84047 = CARTESIAN_POINT ( 'NONE',  ( 30.95817488778657989, 357.0893258606180893, 21.51345825778299314 ) ) ;
#84048 = LINE ( 'NONE', #10671, #45670 ) ;
#84049 = CARTESIAN_POINT ( 'NONE',  ( 9.806233215530133052, 53.43715092910265696, 2.591038554327974364 ) ) ;
#84050 = ORIENTED_EDGE ( 'NONE', *, *, #33471, .F. ) ;
#84051 = DIRECTION ( 'NONE',  ( -0.000000000000000000, -0.000000000000000000, -1.000000000000000000 ) ) ;
#84052 = CARTESIAN_POINT ( 'NONE',  ( 6.683837171061806082, 7.911893696991934455, 7.436622852660996417E-19 ) ) ;
#84053 = CYLINDRICAL_SURFACE ( 'NONE', #54701, 4.000000000000000000 ) ;
#84054 = CARTESIAN_POINT ( 'NONE',  ( -26.05015581842503991, -57.67603816461070920, 43.50693983564572420 ) ) ;
#84055 = CARTESIAN_POINT ( 'NONE',  ( -30.10126468112073184, 13.03072330106369492, 42.03538192853101663 ) ) ;
#84056 = AXIS2_PLACEMENT_3D ( 'NONE', #101822, #3135, #86205 ) ;
#84057 = CARTESIAN_POINT ( 'NONE',  ( -35.76320840016588676, 388.4727839510825333, 5.610592865731860002 ) ) ;
#84058 =( GEOMETRIC_REPRESENTATION_CONTEXT ( 3 ) GLOBAL_UNCERTAINTY_ASSIGNED_CONTEXT ( ( #48054 ) ) GLOBAL_UNIT_ASSIGNED_CONTEXT ( ( #77020, #29962, #93210 ) ) REPRESENTATION_CONTEXT ( 'NONE', 'WORKASPACE' ) );
#84059 = CARTESIAN_POINT ( 'NONE',  ( -6.907083948287215058, 41.55068305711947829, -58.85924204532965831 ) ) ;
#84060 = CIRCLE ( 'NONE', #97829, 4.000000000000001776 ) ;
#84061 = CARTESIAN_POINT ( 'NONE',  ( -94.38155987036965655, -60.00000000000007105, 5.296623108471039565 ) ) ;
#84062 = CARTESIAN_POINT ( 'NONE',  ( 29.68315524077034695, -1.200000000000000030E-05, 40.85535821593451544 ) ) ;
#84063 = CARTESIAN_POINT ( 'NONE',  ( -50.96199133419289495, -32.58464942492616956, 49.99883352212385290 ) ) ;
#84064 = DIRECTION ( 'NONE',  ( 0.8191520442889884679, 0.000000000000000000, 0.5735764363510509334 ) ) ;
#84065 = ORIENTED_EDGE ( 'NONE', *, *, #4409, .F. ) ;
#84066 = FACE_OUTER_BOUND ( 'NONE', #81997, .T. ) ;
#84067 = VECTOR ( 'NONE', #31095, 1000.000000000000000 ) ;
#84068 = DIRECTION ( 'NONE',  ( -1.000000000000000000, -1.224606353822377258E-16, -0.000000000000000000 ) ) ;
#84069 = CARTESIAN_POINT ( 'NONE',  ( 9.300691195493925534, -2.624086112765174672, 14.76496043385272827 ) ) ;
#84070 = EDGE_LOOP ( 'NONE', ( #28299, #46964, #72670, #64414, #19892, #96197 ) ) ;
#84071 = CARTESIAN_POINT ( 'NONE',  ( 77.19326105945918925, -38.47784706899123819, 185.3049776433571765 ) ) ;
#84072 =( LENGTH_UNIT ( ) NAMED_UNIT ( * ) SI_UNIT ( .MILLI., .METRE. ) );
#84073 = LINE ( 'NONE', #10173, #43966 ) ;
#84074 = DIRECTION ( 'NONE',  ( -1.000000000000000000, -1.224606353822377258E-16, -0.000000000000000000 ) ) ;
#84075 = CARTESIAN_POINT ( 'NONE',  ( -42.48296590551735363, 485.4097859441482683, -3.498432987069644895 ) ) ;
#84076 = CARTESIAN_POINT ( 'NONE',  ( 86.97982282064982940, -29.99999999999999645, 183.6336763072494023 ) ) ;
#84077 = CARTESIAN_POINT ( 'NONE',  ( 43.72966438978044579, 434.3041953058477702, 13.93761445528211596 ) ) ;
#84078 = EDGE_CURVE ( 'NONE', #66630, #45380, #88403, .T. ) ;
#84079 = CYLINDRICAL_SURFACE ( 'NONE', #100076, 4.000000000000000000 ) ;
#84080 = AXIS2_PLACEMENT_3D ( 'NONE', #77799, #28758, #49381 ) ;
#84081 = ORIENTED_EDGE ( 'NONE', *, *, #14617, .F. ) ;
#84082 = VERTEX_POINT ( 'NONE', #69965 ) ;
#84083 = CARTESIAN_POINT ( 'NONE',  ( 51.23517877398742826, -42.97391562393161024, 54.09909760496220343 ) ) ;
#84084 = CARTESIAN_POINT ( 'NONE',  ( 5.666915313784246067, 41.34312547834939977, -58.37679883534556069 ) ) ;
#84085 = ADVANCED_FACE ( 'NONE', ( #103910 ), #47264, .T. ) ;
#84086 = CARTESIAN_POINT ( 'NONE',  ( 48.02835407290545078, 16.78162100668605206, 14.35535821593427386 ) ) ;
#84087 = B_SPLINE_CURVE_WITH_KNOTS ( 'NONE', 3,
 ( #80592, #5654, #22932, #38576, #21877, #14798, #87653, #31034, #79540, #47693 ),
 .UNSPECIFIED., .F., .F.,
 ( 4, 2, 2, 2, 4 ),
 ( 0.01051144076094937159, 0.01162027323572613347, 0.01272910571050289534, 0.01383793818527965722, 0.01494677066005641909 ),
 .UNSPECIFIED. ) ;
#84088 = EDGE_LOOP ( 'NONE', ( #72340, #81385, #89661, #44702 ) ) ;
#84089 = CARTESIAN_POINT ( 'NONE',  ( -90.00912977251989844, -38.39750930754247094, -15.99775578366946149 ) ) ;
#84090 = AXIS2_PLACEMENT_3D ( 'NONE', #103575, #47448, #29723 ) ;
#84091 = EDGE_LOOP ( 'NONE', ( #11506, #5368, #86628, #3645, #49776, #31253 ) ) ;
#84092 = CARTESIAN_POINT ( 'NONE',  ( 16.10173312979568649, 5.477053992168872121, 4.739458514412312695 ) ) ;
#84093 = CARTESIAN_POINT ( 'NONE',  ( 110.2760654704705416, -38.35601861863470674, 184.1510513626866441 ) ) ;
#84094 = CARTESIAN_POINT ( 'NONE',  ( 13.08928845638972049, 23.86133543384095645, 4.069885106817294762 ) ) ;
#84095 = CARTESIAN_POINT ( 'NONE',  ( 83.49139130404353182, -37.85069686451048909, 31.99470159126698121 ) ) ;
#84096 = FACE_OUTER_BOUND ( 'NONE', #60314, .T. ) ;
#84097 = CARTESIAN_POINT ( 'NONE',  ( -25.74409405560901476, 306.5801223853982833, -9.620750498333789480 ) ) ;
#84098 = CARTESIAN_POINT ( 'NONE',  ( 3.717184411742878503, -9.782292260247256621, -11.42823731287383637 ) ) ;
#84099 = ADVANCED_FACE ( 'NONE', ( #22508 ), #91983, .F. ) ;
#84100 = AXIS2_PLACEMENT_3D ( 'NONE', #60890, #100264, #59292 ) ;
#84101 = CARTESIAN_POINT ( 'NONE',  ( -23.38332460214670050, 25.95229859289731422, -30.70617127781034483 ) ) ;
#84102 = CARTESIAN_POINT ( 'NONE',  ( 13.37207953394533355, -5.000000000000000000, 6.123233995736768255E-16 ) ) ;
#84103 = EDGE_LOOP ( 'NONE', ( #62886, #92984, #83104, #69006, #28484 ) ) ;
#84104 = CARTESIAN_POINT ( 'NONE',  ( 60.69206503066401126, -60.33900397284496364, 84.28633839224548296 ) ) ;
#84105 = EDGE_CURVE ( 'NONE', #23997, #60854, #37727, .T. ) ;
#84106 = CARTESIAN_POINT ( 'NONE',  ( 5.974456367264334036E-20, 45.30391365246044444, -18.75000000000000355 ) ) ;
#84107 = CARTESIAN_POINT ( 'NONE',  ( 33.58349330513380693, 1.593028355512270962E-15, 0.000000000000000000 ) ) ;
#84108 = ORIENTED_EDGE ( 'NONE', *, *, #17746, .F. ) ;
#84109 = CARTESIAN_POINT ( 'NONE',  ( -36.24643790419225553, 484.5338396111271777, -2.428444667542725810 ) ) ;
#84110 = STYLED_ITEM ( 'NONE', ( #99800 ), #76156 ) ;
#84111 = CARTESIAN_POINT ( 'NONE',  ( -40.94836816866144602, 406.2627700906166979, 27.72596324573498805 ) ) ;
#84112 = DIRECTION ( 'NONE',  ( -1.000000000000000000, -0.000000000000000000, -0.000000000000000000 ) ) ;
#84113 = CARTESIAN_POINT ( 'NONE',  ( 0.000000000000000000, 4.898587196589412829E-16, -4.000000000000000000 ) ) ;
#84114 = CARTESIAN_POINT ( 'NONE',  ( -8.000000000000000000, -26.74999999999999645, -9.797174393178825657E-16 ) ) ;
#84115 = CARTESIAN_POINT ( 'NONE',  ( 24.08218120605116397, -18.86977045670454700, 31.47062207553021906 ) ) ;
#84116 = COLOUR_RGB ( '', 0.40784314, 0.44705882, 0.49803922) ;
#84117 = EDGE_CURVE ( 'NONE', #20022, #27771, #2292, .T. ) ;
#84118 = CARTESIAN_POINT ( 'NONE',  ( -10.00000000000000178, 16.00000000000000000, -4.582575694955835388 ) ) ;
#84119 = CIRCLE ( 'NONE', #104831, 60.00000000000000000 ) ;
#84120 = ORIENTED_EDGE ( 'NONE', *, *, #21994, .F. ) ;
#84121 = CARTESIAN_POINT ( 'NONE',  ( 84.23407561538746791, -35.92907227037686368, 175.7388898281075740 ) ) ;
#84122 = CONICAL_SURFACE ( 'NONE', #66883, 7.500000000000000888, 0.8594454914424817238 ) ;
#84123 = DIRECTION ( 'NONE',  ( 0.000000000000000000, 0.000000000000000000, 1.000000000000000000 ) ) ;
#84124 = ORIENTED_EDGE ( 'NONE', *, *, #99395, .T. ) ;
#84125 = LINE ( 'NONE', #87193, #73810 ) ;
#84126 = CARTESIAN_POINT ( 'NONE',  ( 5.074712500031950846, -4.333244529504593601, -17.09696852381403431 ) ) ;
#84127 = CARTESIAN_POINT ( 'NONE',  ( 11.46641754970693228, -3.000000000000002665, -75.26692388747142104 ) ) ;
#84128 = CARTESIAN_POINT ( 'NONE',  ( -14.92666003045043510, -3.000000000000002665, -87.00284506551274433 ) ) ;
#84129 = CARTESIAN_POINT ( 'NONE',  ( -18.81654674752487821, -25.40603723063000530, -38.49895005552811256 ) ) ;
#84130 = EDGE_CURVE ( 'NONE', #60249, #160, #69464, .T. ) ;
#84131 = APPLICATION_PROTOCOL_DEFINITION ( 'draft international standard', 'automotive_design', 1998, #89957 ) ;
#84132 = B_SPLINE_CURVE_WITH_KNOTS ( 'NONE', 3,
 ( #18516, #1756, #51375, #34713, #74589, #665, #67587, #91849, #34177, #67055 ),
 .UNSPECIFIED., .F., .F.,
 ( 4, 2, 2, 2, 4 ),
 ( 0.001128025973688894868, 0.01055240993440221230, 0.01526460191475887199, 0.01762069790493720617, 0.01997679389511553688 ),
 .UNSPECIFIED. ) ;
#84133 = CARTESIAN_POINT ( 'NONE',  ( 47.86266428647820703, -60.00000000000000000, 66.71390725780067044 ) ) ;
#84134 = AXIS2_PLACEMENT_3D ( 'NONE', #56854, #64447, #97320 ) ;
#84135 = CARTESIAN_POINT ( 'NONE',  ( 35.96520222810764267, -36.00751560667545448, 45.14789304285356053 ) ) ;
#84136 = CIRCLE ( 'NONE', #9373, 11.00000000000001066 ) ;
#84137 = CARTESIAN_POINT ( 'NONE',  ( 0.000000000000000000, 0.000000000000000000, 4.000000000000000000 ) ) ;
#84138 = CARTESIAN_POINT ( 'NONE',  ( 20.76631208310896781, -17.42254526309043072, 31.47037444563865449 ) ) ;
#84139 = AXIS2_PLACEMENT_3D ( 'NONE', #71228, #4916, #21138 ) ;
#84141 = CARTESIAN_POINT ( 'NONE',  ( -12.60307481242552896, 22.93430151644087189, -5.613563419561906187 ) ) ;
#84140 = CARTESIAN_POINT ( 'NONE',  ( -38.04692939061810364, -36.94347500124628425, 47.39189219977645706 ) ) ;
#84142 = DIRECTION ( 'NONE',  ( 0.000000000000000000, -0.000000000000000000, 1.000000000000000000 ) ) ;
#84143 = CARTESIAN_POINT ( 'NONE',  ( -7.188101187500001821, -9.500000002048386349, -2.977408999572651371 ) ) ;
#84144 = CYLINDRICAL_SURFACE ( 'NONE', #83558, 4.000000000000000000 ) ;
#84145 = AXIS2_PLACEMENT_3D ( 'NONE', #99345, #91299, #7690 ) ;
#84146 = LINE ( 'NONE', #91710, #5303 ) ;
#84147 = EDGE_LOOP ( 'NONE', ( #103808, #27635, #39162, #23449, #77490, #106592 ) ) ;
#84148 = CARTESIAN_POINT ( 'NONE',  ( -6.928203230275508773, -65.00000000000000000, 4.000000000000002665 ) ) ;
#84149 = DIRECTION ( 'NONE',  ( 0.000000000000000000, -1.000000000000000000, 0.000000000000000000 ) ) ;
#84150 = CARTESIAN_POINT ( 'NONE',  ( 37.85084083633361729, 438.0234350436310820, 4.171260309356161322 ) ) ;
#84151 = EDGE_CURVE ( 'NONE', #82792, #36789, #100709, .T. ) ;
#84153 = CARTESIAN_POINT ( 'NONE',  ( 48.31748088701653643, -60.22827261165075896, -32.41382024327764100 ) ) ;
#84152 = SURFACE_STYLE_FILL_AREA ( #10251 ) ;
#84154 = ORIENTED_EDGE ( 'NONE', *, *, #2931, .T. ) ;
#84155 = AXIS2_PLACEMENT_3D ( 'NONE', #12509, #70763, #22239 ) ;
#84156 = CARTESIAN_POINT ( 'NONE',  ( 27.42283046010333436, 36.77223446253648120, 7.587737780918474506 ) ) ;
#84157 = CARTESIAN_POINT ( 'NONE',  ( -4.205845516828716768, 51.73505483899108981, 7.923285039163679322 ) ) ;
#84158 = ORIENTED_EDGE ( 'NONE', *, *, #17456, .F. ) ;
#84159 = EDGE_CURVE ( 'NONE', #103417, #43619, #15170, .T. ) ;
#84160 = ADVANCED_FACE ( 'NONE', ( #56682 ), #46458, .F. ) ;
#84161 = DIRECTION ( 'NONE',  ( 0.000000000000000000, 0.000000000000000000, -1.000000000000000000 ) ) ;
#84162 = CIRCLE ( 'NONE', #15257, 0.5000000000000004441 ) ;
#84163 = DIRECTION ( 'NONE',  ( 0.000000000000000000, -1.000000000000000000, 0.000000000000000000 ) ) ;
#84164 = AXIS2_PLACEMENT_3D ( 'NONE', #104843, #78963, #14747 ) ;
#84165 = DIRECTION ( 'NONE',  ( 1.150791560227848544E-16, -0.3420201433256727652, 0.9396926207859068736 ) ) ;
#84166 = CARTESIAN_POINT ( 'NONE',  ( -102.5570158079410135, -60.00000000000000711, 95.99420030246923830 ) ) ;
#84167 = DIRECTION ( 'NONE',  ( 0.000000000000000000, 1.000000000000000000, 0.000000000000000000 ) ) ;
#84168 = CARTESIAN_POINT ( 'NONE',  ( 6.289692432696784685, 1.244805614057421469E-13, 6.828989928337167115 ) ) ;
#84169 = CARTESIAN_POINT ( 'NONE',  ( 35.74483125092430669, 413.6409941285803598, 6.029078300230034770 ) ) ;
#84170 = CARTESIAN_POINT ( 'NONE',  ( 41.17144925627759022, 461.2585203975962713, 2.461466063511514424 ) ) ;
#84172 = DIRECTION ( 'NONE',  ( 4.738110706560371839E-17, -0.9221233147934838614, 0.3868961001538753219 ) ) ;
#84171 = CYLINDRICAL_SURFACE ( 'NONE', #100840, 7.000000000000011546 ) ;
#84173 = CARTESIAN_POINT ( 'NONE',  ( -82.08609670664580449, -49.97993307730780543, 177.5978396368247729 ) ) ;
#84174 = ORIENTED_EDGE ( 'NONE', *, *, #11163, .T. ) ;
#84175 = CARTESIAN_POINT ( 'NONE',  ( 6.057904175366206623, 41.61856606260997893, -70.65344123640606711 ) ) ;
#84176 = EDGE_CURVE ( 'NONE', #10644, #45933, #78456, .T. ) ;
#84177 = ORIENTED_EDGE ( 'NONE', *, *, #38114, .T. ) ;
#84178 = ORIENTED_EDGE ( 'NONE', *, *, #49857, .F. ) ;
#84179 = DIRECTION ( 'NONE',  ( -0.000000000000000000, 1.000000000000000000, -0.000000000000000000 ) ) ;
#84180 = DIRECTION ( 'NONE',  ( 0.9736964118521804767, 0.000000000000000000, -0.2278492869117413333 ) ) ;
#84181 = EDGE_LOOP ( 'NONE', ( #80310, #38106 ) ) ;
#84182 = DIRECTION ( 'NONE',  ( 1.000000000000000000, 0.000000000000000000, -0.000000000000000000 ) ) ;
#84183 = FACE_OUTER_BOUND ( 'NONE', #40123, .T. ) ;
#84184 = DIRECTION ( 'NONE',  ( 0.000000000000000000, -1.000000000000000000, 0.000000000000000000 ) ) ;
#84185 = AXIS2_PLACEMENT_3D ( 'NONE', #72951, #49209, #82108 ) ;
#84186 = CARTESIAN_POINT ( 'NONE',  ( 30.56153846153846132, 1.411358822780289120E-15, 0.000000000000000000 ) ) ;
#84187 = CARTESIAN_POINT ( 'NONE',  ( -0.1698863216407462684, 53.40045558394650982, 10.24124536584039902 ) ) ;
#84188 = FACE_OUTER_BOUND ( 'NONE', #5580, .T. ) ;
#84189 = DIRECTION ( 'NONE',  ( 0.000000000000000000, 0.000000000000000000, 1.000000000000000000 ) ) ;
#84190 = CARTESIAN_POINT ( 'NONE',  ( 102.0720237449618679, -14.21045842199434439, 125.2221798637976349 ) ) ;
#84191 = CARTESIAN_POINT ( 'NONE',  ( -72.11328378729270128, -60.00000000000007816, 177.1367255069332316 ) ) ;
#84192 = CARTESIAN_POINT ( 'NONE',  ( -59.49377889082170867, -56.86590393334827098, 79.18203250951856376 ) ) ;
#84193 = VERTEX_POINT ( 'NONE', #29935 ) ;
#84194 = CARTESIAN_POINT ( 'NONE',  ( 6.999814028509887542, 16.99967454973588943, 0.2742116757349301048 ) ) ;
#84195 = ORIENTED_EDGE ( 'NONE', *, *, #77802, .F. ) ;
#84196 = CARTESIAN_POINT ( 'NONE',  ( -102.7734312727401829, -37.82045702703825185, 170.2527634601842976 ) ) ;
#84197 = CARTESIAN_POINT ( 'NONE',  ( 7.188101187500000933, -10.43750000204838457, -2.977408999572650483 ) ) ;
#84198 = CARTESIAN_POINT ( 'NONE',  ( 8.349999999999999645, 1.411358822780289120E-15, 0.000000000000000000 ) ) ;
#84199 = VECTOR ( 'NONE', #73514, 1000.000000000000000 ) ;
#84200 = ORIENTED_EDGE ( 'NONE', *, *, #15042, .T. ) ;
#84201 = CARTESIAN_POINT ( 'NONE',  ( 7.421727621019012844, -2.999999999999999112, -70.37058875308096617 ) ) ;
#84202 = CARTESIAN_POINT ( 'NONE',  ( -71.67561706003607469, -60.00000000000001421, 151.8435231814522126 ) ) ;
#84203 = CARTESIAN_POINT ( 'NONE',  ( 37.56673239365841255, 25.47613764497371136, -13.45617127781092215 ) ) ;
#84204 = CARTESIAN_POINT ( 'NONE',  ( 5.082755093536324154, -22.71875000204838457, 5.082755093536326818 ) ) ;
#84205 = CARTESIAN_POINT ( 'NONE',  ( -0.3375803178940949278, 36.31236650232811769, -29.71517349513863948 ) ) ;
#84206 =( BOUNDED_CURVE ( )  B_SPLINE_CURVE ( 2, ( #34281, #67154, #8898 ),
 .UNSPECIFIED., .F., .F. ) 
 B_SPLINE_CURVE_WITH_KNOTS ( ( 3, 3 ),
 ( 0.000000000000000000, 1.000000000000000000 ),
 .UNSPECIFIED. ) 
 CURVE ( )  GEOMETRIC_REPRESENTATION_ITEM ( )  RATIONAL_B_SPLINE_CURVE ( ( 1.000000000000000000, 1.857142857142858317, 1.000000000000000000 ) ) 
 REPRESENTATION_ITEM ( '' )  );
#84207 = CARTESIAN_POINT ( 'NONE',  ( 10.38441970550273119, 0.000000000000000000, -13.52487676487348978 ) ) ;
#84208 = CARTESIAN_POINT ( 'NONE',  ( -11.30963196869130449, -4.963880803831879795, -12.57418315201559800 ) ) ;
#84209 = FILL_AREA_STYLE ('',( #85824 ) ) ;
#84210 = CARTESIAN_POINT ( 'NONE',  ( 9.478973614161615657, -11.83509979120333178, 9.222223356601535471 ) ) ;
#84211 = CARTESIAN_POINT ( 'NONE',  ( -8.000000000000001776, -14.84375000409677092, 3.313708498984759387 ) ) ;
#84212 = EDGE_CURVE ( 'NONE', #52196, #22409, #74904, .T. ) ;
#84213 = CARTESIAN_POINT ( 'NONE',  ( 37.85084083633365282, 438.0234350436313093, 4.171260309356235929 ) ) ;
#84214 = CARTESIAN_POINT ( 'NONE',  ( -30.28151271900150832, -49.91080145115500244, 35.08722031216328929 ) ) ;
#84215 = CARTESIAN_POINT ( 'NONE',  ( 3.484468584683845460, 19.88498498222627831, 6.075777484465951339 ) ) ;
#84216 = CARTESIAN_POINT ( 'NONE',  ( 45.70191470550344093, -60.25745932227290069, 50.30639238928311130 ) ) ;
#84217 = CARTESIAN_POINT ( 'NONE',  ( -32.72014288347608613, 485.4774019869826134, 6.282418260599838433 ) ) ;
#84218 = AXIS2_PLACEMENT_3D ( 'NONE', #91031, #10611, #9544 ) ;
#84219 = ADVANCED_FACE ( 'NONE', ( #67459 ), #90660, .T. ) ;
#84220 = CARTESIAN_POINT ( 'NONE',  ( -0.6419814643516539299, 45.36335988269765807, 18.57571296656996296 ) ) ;
#84221 = CARTESIAN_POINT ( 'NONE',  ( -93.08574300709510396, -38.49591865938590729, 201.1221301499342360 ) ) ;
#84222 = VERTEX_POINT ( 'NONE', #10263 ) ;
#84224 = CARTESIAN_POINT ( 'NONE',  ( 40.73878143178837519, 486.4834083601638213, 16.46716573231486436 ) ) ;
#84223 = CARTESIAN_POINT ( 'NONE',  ( -16.14595037822616419, 20.23371447306202597, -4.922994507635920947 ) ) ;
#84225 = CARTESIAN_POINT ( 'NONE',  ( 22.91543575571316183, -60.00000000000000711, 34.83253428109101435 ) ) ;
#84226 = CARTESIAN_POINT ( 'NONE',  ( -10.00000000000000178, -15.00000000000000000, -9.999999999999998224 ) ) ;
#84227 = CARTESIAN_POINT ( 'NONE',  ( -7.423110184046854521, 40.85353637179369457, -59.12022309273985599 ) ) ;
#84228 = CIRCLE ( 'NONE', #4998, 15.00000000000000711 ) ;
#84229 = CARTESIAN_POINT ( 'NONE',  ( 6.642722263319527087, 41.46658730130243953, -70.60825968728163105 ) ) ;
#84230 = LINE ( 'NONE', #59979, #72151 ) ;
#84231 = CARTESIAN_POINT ( 'NONE',  ( 43.18591170615831487, 464.9496799542843064, 14.54256400178507747 ) ) ;
#84232 = CARTESIAN_POINT ( 'NONE',  ( 10.59999999999999609, 1.533819458162526451E-15, 0.000000000000000000 ) ) ;
#84233 = CARTESIAN_POINT ( 'NONE',  ( 102.1238087080854626, -60.00000000000000000, 93.46745215179672073 ) ) ;
#84234 = DIRECTION ( 'NONE',  ( 0.000000000000000000, 1.000000000000000000, 0.000000000000000000 ) ) ;
#84235 = CARTESIAN_POINT ( 'NONE',  ( 0.000000000000000000, -78.00000000000000000, 37.00000000000000000 ) ) ;
#84236 = ORIENTED_EDGE ( 'NONE', *, *, #106117, .T. ) ;
#84237 = CARTESIAN_POINT ( 'NONE',  ( 34.47678062874019389, 437.1474145881098821, 5.468662283308706407 ) ) ;
#84238 = AXIS2_PLACEMENT_3D ( 'NONE', #78067, #94807, #38180 ) ;
#84239 = CARTESIAN_POINT ( 'NONE',  ( 0.000000000000000000, 0.000000000000000000, 0.000000000000000000 ) ) ;
#84240 = EDGE_LOOP ( 'NONE', ( #19912, #102507, #103307, #90547 ) ) ;
#84241 = DIRECTION ( 'NONE',  ( 0.000000000000000000, -1.000000000000000000, 0.000000000000000000 ) ) ;
#84242 = FACE_OUTER_BOUND ( 'NONE', #2498, .T. ) ;
#84243 = CARTESIAN_POINT ( 'NONE',  ( 30.00000000000000000, 0.000000000000000000, 9.000000000000000000 ) ) ;
#84244 = CARTESIAN_POINT ( 'NONE',  ( 2.977408999572650927, -22.25000000204839168, -7.188101187500001821 ) ) ;
#84245 = CARTESIAN_POINT ( 'NONE',  ( -3.750000000000004441, -6.495190528383288253, 1.734723475976807094E-15 ) ) ;
#84246 = CONICAL_SURFACE ( 'NONE', #13548, 4.172000000000009479, 0.9599310885968813656 ) ;
#84247 = CARTESIAN_POINT ( 'NONE',  ( 65.52222222222222570, 6.915964383211875250E-15, 0.000000000000000000 ) ) ;
#84248 = CONICAL_SURFACE ( 'NONE', #92860, 3.309499999999999886, 0.7853981633974710386 ) ;
#84250 = EDGE_LOOP ( 'NONE', ( #43063, #28335, #87773, #72546, #61728 ) ) ;
#84249 = CYLINDRICAL_SURFACE ( 'NONE', #99421, 4.000000000000000000 ) ;
#84251 = CARTESIAN_POINT ( 'NONE',  ( 81.09979694935459804, -49.92208873302202221, 168.6177104633348449 ) ) ;
#84252 = CARTESIAN_POINT ( 'NONE',  ( -46.00000000000000000, 461.1597079622330284, 8.544206286659692395 ) ) ;
#84253 = DIRECTION ( 'NONE',  ( 0.000000000000000000, 0.000000000000000000, 1.000000000000000000 ) ) ;
#84254 = ORIENTED_EDGE ( 'NONE', *, *, #106341, .F. ) ;
#84255 = LINE ( 'NONE', #35743, #18749 ) ;
#84256 = CARTESIAN_POINT ( 'NONE',  ( -0.7711376685623203553, 18.23545326243540643, -49.51189540388887877 ) ) ;
#84257 = CARTESIAN_POINT ( 'NONE',  ( 37.56673239365841255, 27.88554838446202311, -10.95617127781092037 ) ) ;
#84258 = CARTESIAN_POINT ( 'NONE',  ( 6.162888688655347558, -7.505553499465142053, -3.129864801432410934E-16 ) ) ;
#84259 = CARTESIAN_POINT ( 'NONE',  ( -27.99999999999999645, 0.000000000000000000, 0.000000000000000000 ) ) ;
#84260 = CARTESIAN_POINT ( 'NONE',  ( -25.40129139438734285, 304.9292372608223900, 10.39962324656867843 ) ) ;
#84261 = B_SPLINE_SURFACE_WITH_KNOTS ( 'NONE', 1, 3, ( 
 ( #76869, #102216, #86061, #27315, #50985, #34329, #52590, #11059, #44525, #77412, #83899, #1365, #51529, #28363, #2445, #42919, #27847, #93603, #10538, #60718, #2981, #84446, #68808, #52060, #100613, #75811, #43455, #85516 ),
 ( #1906, #60197, #59113, #68262, #18129, #35935, #34860, #101153, #53142, #12134, #75267, #67728, #19755, #59645, #19230, #11595, #93064, #84975, #26775, #3529, #92521, #101688, #18675, #76333, #36468, #35393, #69336, #61241 ) ),
 .UNSPECIFIED., .F., .F., .F.,
 ( 2, 2 ),
 ( 4, 2, 2, 2, 2, 2, 2, 2, 2, 2, 2, 2, 2, 4 ),
 ( 0.000000000000000000, 1.000000000000000000 ),
 ( 0.08901491201581737678, 0.1032490540155679704, 0.1174831960153185778, 0.1317173380150691853, 0.1459514800148197788, 0.1744197640143299588, 0.2028880480138401388, 0.2598246160128514504, 0.3167611840118632616, 0.4306343200098861623, 0.5445074560079088410, 0.6583805920059359051, 0.7722537280039543095, 1.000000000000000000 ),
 .UNSPECIFIED. ) ;
#84262 = VERTEX_POINT ( 'NONE', #83615 ) ;
#84263 = SHAPE_DEFINITION_REPRESENTATION ( #76508, #69581 ) ;
#84264 = CARTESIAN_POINT ( 'NONE',  ( 90.51111111111110574, 1.023464760207051730E-14, 0.000000000000000000 ) ) ;
#84265 = VECTOR ( 'NONE', #50852, 1000.000000000000000 ) ;
#84266 = SURFACE_STYLE_USAGE ( .BOTH. , #91309 ) ;
#84267 = CARTESIAN_POINT ( 'NONE',  ( 86.77293047539107818, -57.38694033980660691, 193.7425620307543284 ) ) ;
#84268 = DIRECTION ( 'NONE',  ( -1.000000000000000000, -0.000000000000000000, -0.000000000000000000 ) ) ;
#84269 = CARTESIAN_POINT ( 'NONE',  ( 7.188101187500000044, -28.15625000204838813, 0.000000000000000000 ) ) ;
#84270 = CARTESIAN_POINT ( 'NONE',  ( -42.19618372163272113, 487.7264399052817794, 8.629926728125361990 ) ) ;
#84271 = CIRCLE ( 'NONE', #86000, 8.000000000000000000 ) ;
#84272 = CARTESIAN_POINT ( 'NONE',  ( 8.012708964559053015, 52.02215964811360038, 1.654162217208905883 ) ) ;
#84273 = VECTOR ( 'NONE', #54012, 1000.000000000000000 ) ;
#84274 = LINE ( 'NONE', #10369, #61506 ) ;
#84275 = ORIENTED_EDGE ( 'NONE', *, *, #100836, .F. ) ;
#84276 = CARTESIAN_POINT ( 'NONE',  ( 1.098491644507098242, 43.84235381817760668, 16.88236719228266125 ) ) ;
#84277 = DIRECTION ( 'NONE',  ( 0.000000000000000000, 0.000000000000000000, -1.000000000000000000 ) ) ;
#84278 = CARTESIAN_POINT ( 'NONE',  ( -5.952234287511010358, 4.563574555944671651, -5.000000000000000000 ) ) ;
#84279 = LINE ( 'NONE', #26096, #20517 ) ;
#84280 = EDGE_CURVE ( 'NONE', #80639, #17581, #15687, .T. ) ;
#84281 = ORIENTED_EDGE ( 'NONE', *, *, #91606, .F. ) ;
#84282 = EDGE_CURVE ( 'NONE', #26965, #71171, #4019, .T. ) ;
#84283 = CARTESIAN_POINT ( 'NONE',  ( 0.000000000000000000, 29.56666008184760130, 0.000000000000000000 ) ) ;
#84284 = CARTESIAN_POINT ( 'NONE',  ( -4.852941176470593199, 44.25000000000000000, -70.80672828634229177 ) ) ;
#84285 = AXIS2_PLACEMENT_3D ( 'NONE', #94209, #12210, #39168 ) ;
#84286 = EDGE_CURVE ( 'NONE', #93427, #71455, #17807, .T. ) ;
#84287 = CARTESIAN_POINT ( 'NONE',  ( 32.04707041935533596, 435.9091500956466234, 19.86198171785667554 ) ) ;
#84288 =( LENGTH_UNIT ( ) NAMED_UNIT ( * ) SI_UNIT ( .MILLI., .METRE. ) );
#84289 = CARTESIAN_POINT ( 'NONE',  ( 9.989435848181784650, 101.0261970747157250, -0.5278651953176017875 ) ) ;
#84290 = CARTESIAN_POINT ( 'NONE',  ( 28.50099738913158376, -5.000000000000000000, 0.000000000000000000 ) ) ;
#84291 = CARTESIAN_POINT ( 'NONE',  ( -90.18900329953886796, -59.99999999999999289, 202.0050657913863574 ) ) ;
#84292 = VECTOR ( 'NONE', #29278, 1000.000000000000000 ) ;
#84293 = ADVANCED_FACE ( 'NONE', ( #34588 ), #17850, .T. ) ;
#84294 = COLOUR_RGB ( '', 0.66274510, 0.83137255, 0.94901961) ;
#84295 = CARTESIAN_POINT ( 'NONE',  ( -7.500000000000002665, 4.320742148886547618, -27.76523484934600816 ) ) ;
#84296 = CARTESIAN_POINT ( 'NONE',  ( 26.36650669486618881, 4.898587196589413815E-16, -4.000000000000000888 ) ) ;
#84297 = CARTESIAN_POINT ( 'NONE',  ( -85.78622453063103137, -28.51040679079540396, 180.2837960777752926 ) ) ;
#84298 = PRESENTATION_STYLE_ASSIGNMENT (( #2293 ) ) ;
#84299 = EDGE_CURVE ( 'NONE', #84731, #4022, #103935, .T. ) ;
#84300 = ORIENTED_EDGE ( 'NONE', *, *, #41675, .T. ) ;
#84301 = CARTESIAN_POINT ( 'NONE',  ( -16.04671841158817358, 302.5605069650110863, 9.875078356356782550 ) ) ;
#84302 = CARTESIAN_POINT ( 'NONE',  ( 3.358578016107284014, -0.9723468250019194903, 104.2746939430690389 ) ) ;
#84303 = CARTESIAN_POINT ( 'NONE',  ( -82.89586554537308416, -37.82252042144357773, 0.5134924856167544238 ) ) ;
#84304 = AXIS2_PLACEMENT_3D ( 'NONE', #31146, #96912, #72096 ) ;
#84305 = CARTESIAN_POINT ( 'NONE',  ( -6.708832649680421589, -13.06702039274563454, -7.389177399647482325 ) ) ;
#84306 = DIRECTION ( 'NONE',  ( 1.000000000000000000, 1.224606353822377258E-16, 0.000000000000000000 ) ) ;
#84307 = CIRCLE ( 'NONE', #37856, 33.82893434829263413 ) ;
#84308 = CARTESIAN_POINT ( 'NONE',  ( -15.42152358372385557, 44.08893209364050136, 5.095058633600949349 ) ) ;
#84309 = CARTESIAN_POINT ( 'NONE',  ( -8.188359067971299865, -12.25820946039680592, 8.650503056542792280 ) ) ;
#84310 = CARTESIAN_POINT ( 'NONE',  ( -6.594225035609122543, -11.92007582869070426, 9.808253832663700322 ) ) ;
#84311 = CARTESIAN_POINT ( 'NONE',  ( -22.19860641359375819, 28.18788469371687455, 31.21259335822219683 ) ) ;
#84312 = CARTESIAN_POINT ( 'NONE',  ( 70.38659604113041723, -14.21045842199445808, 117.5484250040930050 ) ) ;
#84313 = VECTOR ( 'NONE', #61068, 1000.000000000000000 ) ;
#84314 = CARTESIAN_POINT ( 'NONE',  ( -89.90470572912276737, -30.00000000000002842, -11.15078749779565825 ) ) ;
#84315 = CARTESIAN_POINT ( 'NONE',  ( -73.44956775615928279, -36.01767715975007178, 111.7754548667898860 ) ) ;
#84316 = ORIENTED_EDGE ( 'NONE', *, *, #50736, .T. ) ;
#84317 = CARTESIAN_POINT ( 'NONE',  ( 73.11766847789152735, -30.00000000000003197, 143.8471250665463117 ) ) ;
#84318 = CARTESIAN_POINT ( 'NONE',  ( 2.971737004093363499, 40.83778713800185756, 64.99968649108126328 ) ) ;
#84319 = VERTEX_POINT ( 'NONE', #25431 ) ;
#84320 = CARTESIAN_POINT ( 'NONE',  ( 30.73846156699857346, -57.67116533035498094, -42.81922766351370058 ) ) ;
#84321 = ORIENTED_EDGE ( 'NONE', *, *, #86794, .T. ) ;
#84322 = CARTESIAN_POINT ( 'NONE',  ( 7.799693306582752506, 52.08906168172599394, -1.774544900689356774 ) ) ;
#84323 = CARTESIAN_POINT ( 'NONE',  ( -5.082755093536325042, -23.46875000204838457, -5.082755093536325930 ) ) ;
#84324 = CIRCLE ( 'NONE', #82634, 7.500000000000000000 ) ;
#84325 = CARTESIAN_POINT ( 'NONE',  ( -1.219019397738882127, 27.86094505705872137, -39.18046835220320645 ) ) ;
#84326 = ORIENTED_EDGE ( 'NONE', *, *, #92223, .F. ) ;
#84327 = SURFACE_SIDE_STYLE ('',( #100498 ) ) ;
#84328 = ORIENTED_EDGE ( 'NONE', *, *, #59971, .F. ) ;
#84329 = DIRECTION ( 'NONE',  ( 0.000000000000000000, 0.000000000000000000, 1.000000000000000000 ) ) ;
#84330 = DIRECTION ( 'NONE',  ( 0.000000000000000000, 0.000000000000000000, -1.000000000000000000 ) ) ;
#84331 = CARTESIAN_POINT ( 'NONE',  ( 27.24240537402066309, 306.4001577942659651, -9.435465325163482575 ) ) ;
#84332 = CARTESIAN_POINT ( 'NONE',  ( -7.188101187500000044, -12.40625000204838635, -8.802885111219163269E-16 ) ) ;
#84333 = CARTESIAN_POINT ( 'NONE',  ( -32.15166163075724626, 486.0589784586660471, 5.199393881400879103 ) ) ;
#84334 = DIRECTION ( 'NONE',  ( -0.5735764363510497121, 0.8191520442889892450, 1.003171929053521665E-16 ) ) ;
#84335 = DIRECTION ( 'NONE',  ( 0.000000000000000000, -1.000000000000000000, 0.000000000000000000 ) ) ;
#84336 = CARTESIAN_POINT ( 'NONE',  ( -12.49701543487590705, -3.281887186806090373, -14.00878883702671018 ) ) ;
#84337 = CARTESIAN_POINT ( 'NONE',  ( 0.000000000000000000, 15.00000000000000000, 0.000000000000000000 ) ) ;
#84338 = EDGE_CURVE ( 'NONE', #73270, #87270, #18388, .T. ) ;
#84339 = UNCERTAINTY_MEASURE_WITH_UNIT (LENGTH_MEASURE( 1.000000000000000082E-05 ), #55653, 'distance_accuracy_value', 'NONE');
#84340 = B_SPLINE_CURVE_WITH_KNOTS ( 'NONE', 3,
 ( #90699, #49148, #15201, #48089, #106318, #16263, #73964, #44, #33017, #65883, #98764, #24917, #57771, #33536, #101965, #26534, #18423, #100896, #69091, #85260, #84730, #35688 ),
 .UNSPECIFIED., .F., .F.,
 ( 4, 2, 2, 2, 2, 2, 2, 2, 2, 2, 4 ),
 ( 2.543397799394530001E-16, 0.001421275008199062145, 0.002842550016397869719, 0.003553187520497273506, 0.004263825024596677726, 0.005685100032795484433, 0.007106375040994290272, 0.007817012545093694059, 0.008527650049193096979, 0.009948925057391901083, 0.01137020006559070519 ),
 .UNSPECIFIED. ) ;
#84341 = AXIS2_PLACEMENT_3D ( 'NONE', #11018, #21287, #53616 ) ;
#84342 = EDGE_LOOP ( 'NONE', ( #41869, #69842, #106770, #100075, #102149 ) ) ;
#84343 = CARTESIAN_POINT ( 'NONE',  ( 3.857142857142854986, -1.200583151104943624, 103.1763305333244176 ) ) ;
#84345 = CARTESIAN_POINT ( 'NONE',  ( 31.94500641777023375, -39.48962315678958390, 33.87780594823525604 ) ) ;
#84344 = SURFACE_SIDE_STYLE ('',( #18568 ) ) ;
#84346 = CARTESIAN_POINT ( 'NONE',  ( -25.22241582816893413, -4.285714285714285587, 3.301606509427073455 ) ) ;
#84347 = ORIENTED_EDGE ( 'NONE', *, *, #63394, .F. ) ;
#84348 = EDGE_CURVE ( 'NONE', #79201, #23775, #13211, .T. ) ;
#84349 = EDGE_CURVE ( 'NONE', #26769, #65192, #65985, .T. ) ;
#84350 = CARTESIAN_POINT ( 'NONE',  ( -22.45608800630787627, 25.48376296471925073, -32.96030118683280108 ) ) ;
#84351 = ORIENTED_EDGE ( 'NONE', *, *, #56578, .F. ) ;
#84353 = DIRECTION ( 'NONE',  ( 1.000000000000000000, 0.000000000000000000, 0.000000000000000000 ) ) ;
#84352 = CARTESIAN_POINT ( 'NONE',  ( -27.02532652597945884, 34.78626739604272444, -7.556984339685866026 ) ) ;
#84354 = CARTESIAN_POINT ( 'NONE',  ( 0.000000000000000000, 80.00000000000000000, 0.000000000000000000 ) ) ;
#84355 = CARTESIAN_POINT ( 'NONE',  ( 4.000000000000000000, 17.85270131633358304, -10.00000000000000178 ) ) ;
#84356 = DIRECTION ( 'NONE',  ( -0.5735764363510461594, 0.8191520442889916875, 1.003171929053524870E-16 ) ) ;
#84357 = CARTESIAN_POINT ( 'NONE',  ( 43.10000000000000142, 3.309500000000003439, 0.000000000000000000 ) ) ;
#84358 = LINE ( 'NONE', #77327, #33223 ) ;
#84359 = ORIENTED_EDGE ( 'NONE', *, *, #30428, .T. ) ;
#84360 = AXIS2_PLACEMENT_3D ( 'NONE', #76330, #102212, #93601 ) ;
#84361 = CARTESIAN_POINT ( 'NONE',  ( 87.53966758494706824, -59.99999999999999289, -22.09775139173853731 ) ) ;
#84362 = FILL_AREA_STYLE ('',( #51973 ) ) ;
#84363 = FILL_AREA_STYLE_COLOUR ( '', #75485 ) ;
#84364 = DIRECTION ( 'NONE',  ( -1.000000000000000000, -1.224606353822377258E-16, -0.000000000000000000 ) ) ;
#84365 = CARTESIAN_POINT ( 'NONE',  ( -16.14595037822616419, 12.99999999999999467, -8.749999999999921840 ) ) ;
#84366 = EDGE_LOOP ( 'NONE', ( #55508, #6790, #87272, #55355, #64657, #104279 ) ) ;
#84367 = EDGE_CURVE ( 'NONE', #91522, #63934, #17051, .T. ) ;
#84368 = CARTESIAN_POINT ( 'NONE',  ( -43.03357534758885095, 463.2291678140052227, 4.675918524150252331 ) ) ;
#84369 = ORIENTED_EDGE ( 'NONE', *, *, #35845, .T. ) ;
#84370 = ORIENTED_EDGE ( 'NONE', *, *, #59475, .F. ) ;
#84371 = CARTESIAN_POINT ( 'NONE',  ( 7.896571385775229324, 81.21002000654247865, 1.305932416347436620 ) ) ;
#84372 = DIRECTION ( 'NONE',  ( -1.000000000000000000, -0.000000000000000000, -0.000000000000000000 ) ) ;
#84373 = CARTESIAN_POINT ( 'NONE',  ( -16.42070475374124783, 35.05495340490914913, -21.83980561103319218 ) ) ;
#84374 = DIRECTION ( 'NONE',  ( 0.000000000000000000, -1.000000000000000000, 0.000000000000000000 ) ) ;
#84375 = CARTESIAN_POINT ( 'NONE',  ( 85.54848234686721753, -60.20738201045722349, -15.09784675847152613 ) ) ;
#84376 = CARTESIAN_POINT ( 'NONE',  ( -38.72759624817576452, 310.1070778200068503, 1.620604754975068174 ) ) ;
#84377 = DIRECTION ( 'NONE',  ( -0.5735764363510512664, 0.8191520442889881348, 1.003171929053520309E-16 ) ) ;
#84378 = CIRCLE ( 'NONE', #37897, 4.000000000000007105 ) ;
#84379 = CARTESIAN_POINT ( 'NONE',  ( -16.91669820832276727, 34.22140543898331799, 24.30698433968612804 ) ) ;
#84380 = VERTEX_POINT ( 'NONE', #18940 ) ;
#84381 = EDGE_CURVE ( 'NONE', #32853, #75707, #99353, .T. ) ;
#84382 = CARTESIAN_POINT ( 'NONE',  ( -6.499999999999999112, 4.076783350660889482, -6.121918786669028556 ) ) ;
#84383 = VERTEX_POINT ( 'NONE', #74984 ) ;
#84384 = CARTESIAN_POINT ( 'NONE',  ( 49.26574068698166542, 8.068653426789120786, -15.39376958037598619 ) ) ;
#84385 = DIRECTION ( 'NONE',  ( 0.000000000000000000, -1.000000000000000000, 0.000000000000000000 ) ) ;
#84386 = EDGE_CURVE ( 'NONE', #75403, #71690, #12616, .T. ) ;
#84388 = ORIENTED_EDGE ( 'NONE', *, *, #2403, .T. ) ;
#84387 = CARTESIAN_POINT ( 'NONE',  ( 5.415856237588537958, 41.85405046271414875, -58.97635192936115800 ) ) ;
#84389 = CARTESIAN_POINT ( 'NONE',  ( 77.90007794136121788, -29.08184770833722865, 125.1920107075117983 ) ) ;
#84390 = ORIENTED_EDGE ( 'NONE', *, *, #58112, .T. ) ;
#84391 = CARTESIAN_POINT ( 'NONE',  ( 4.165510012636465476, -48.44870269470101221, 43.44044287971949103 ) ) ;
#84392 = DIRECTION ( 'NONE',  ( 0.000000000000000000, 0.000000000000000000, 1.000000000000000000 ) ) ;
#84393 = CARTESIAN_POINT ( 'NONE',  ( 5.082755093536325930, -24.96875000204838813, -5.082755093536325042 ) ) ;
#84394 = CARTESIAN_POINT ( 'NONE',  ( -91.87475470944771416, -57.66094841159801376, -19.53952869114660373 ) ) ;
#84395 = VERTEX_POINT ( 'NONE', #78193 ) ;
#84396 = DIRECTION ( 'NONE',  ( -1.000000000000000000, 0.000000000000000000, 0.000000000000000000 ) ) ;
#84397 = VECTOR ( 'NONE', #59611, 1000.000000000000000 ) ;
#84398 = CARTESIAN_POINT ( 'NONE',  ( 102.2581492532549419, -37.84842508405214545, 182.3710817063251568 ) ) ;
#84399 = AXIS2_PLACEMENT_3D ( 'NONE', #17166, #1474, #50037 ) ;
#84400 = CARTESIAN_POINT ( 'NONE',  ( -32.87547266101557852, 465.6993878536674742, 10.91512469976539279 ) ) ;
#84401 = CARTESIAN_POINT ( 'NONE',  ( 2.503857664561936320E-16, -8.660254037844401509, -10.00000000000000000 ) ) ;
#84402 = CARTESIAN_POINT ( 'NONE',  ( -3.313708498984760720, -19.71875000409677270, -8.000000000000000000 ) ) ;
#84403 = CARTESIAN_POINT ( 'NONE',  ( 10.73176661990081371, 1.340359594676612611E-15, 0.000000000000000000 ) ) ;
#84404 = CARTESIAN_POINT ( 'NONE',  ( 68.70539558375507738, -1.232595164407830946E-29, 4.000000000000007105 ) ) ;
#84405 = AXIS2_PLACEMENT_3D ( 'NONE', #106199, #65234, #24274 ) ;
#84406 = DIRECTION ( 'NONE',  ( -0.000000000000000000, 1.000000000000000000, -0.000000000000000000 ) ) ;
#84407 = DIRECTION ( 'NONE',  ( -0.000000000000000000, -0.000000000000000000, -1.000000000000000000 ) ) ;
#84408 = CARTESIAN_POINT ( 'NONE',  ( 10.50000000000000355, -5.000000000000000000, -34.12705335492802305 ) ) ;
#84409 = DIRECTION ( 'NONE',  ( 1.000000000000000000, 6.938893903907228378E-18, 5.551115123125782702E-17 ) ) ;
#84410 = CARTESIAN_POINT ( 'NONE',  ( 0.2291258134149000425, -29.99999999999999645, -7.774924953687139428 ) ) ;
#84411 = LINE ( 'NONE', #83866, #9177 ) ;
#84412 = PRESENTATION_STYLE_ASSIGNMENT (( #82809 ) ) ;
#84413 = CARTESIAN_POINT ( 'NONE',  ( 0.9524862760789143401, 8.765895626014080122, 51.31327605337367714 ) ) ;
#84414 = CIRCLE ( 'NONE', #75781, 5.000000000000003553 ) ;
#84415 = CARTESIAN_POINT ( 'NONE',  ( -89.14411627724076936, -30.00000000000000711, 188.9134825190658944 ) ) ;
#84416 = EDGE_CURVE ( 'NONE', #17545, #105603, #72896, .T. ) ;
#84417 = ORIENTED_EDGE ( 'NONE', *, *, #50847, .F. ) ;
#84418 = AXIS2_PLACEMENT_3D ( 'NONE', #59479, #92344, #100976 ) ;
#84419 = DIRECTION ( 'NONE',  ( -1.000000000000000000, 0.000000000000000000, -0.000000000000000000 ) ) ;
#84420 = CARTESIAN_POINT ( 'NONE',  ( 72.55415673912993668, -57.66409419474867093, 177.4493738948018233 ) ) ;
#84422 = CARTESIAN_POINT ( 'NONE',  ( 42.61650669486618881, 1.474610560812782335E-15, 0.000000000000000000 ) ) ;
#84421 = DIRECTION ( 'NONE',  ( 0.000000000000000000, -1.000000000000000000, 0.000000000000000000 ) ) ;
#84423 = EDGE_CURVE ( 'NONE', #16221, #87702, #12911, .T. ) ;
#84424 = ADVANCED_FACE ( 'NONE', ( #93323 ), #100471, .T. ) ;
#84426 = CARTESIAN_POINT ( 'NONE',  ( 46.69156559559471731, -34.78800018587544685, -36.65496307456758984 ) ) ;
#84425 = AXIS2_PLACEMENT_3D ( 'NONE', #85312, #28174, #11398 ) ;
#84427 = CARTESIAN_POINT ( 'NONE',  ( 38.81358894280276672, 485.1131561813238591, -4.191378885298274959 ) ) ;
#84428 = CARTESIAN_POINT ( 'NONE',  ( -36.18825654482056819, -59.99999999999999289, 47.53788091366800472 ) ) ;
#84429 = DIRECTION ( 'NONE',  ( 0.000000000000000000, 0.000000000000000000, 1.000000000000000000 ) ) ;
#84430 = EDGE_CURVE ( 'NONE', #7161, #42192, #79760, .T. ) ;
#84431 = AXIS2_PLACEMENT_3D ( 'NONE', #29430, #69853, #71966 ) ;
#84432 = CARTESIAN_POINT ( 'NONE',  ( -43.69716417794982277, 48.00000000000000000, 48.48761666242421597 ) ) ;
#84433 = CARTESIAN_POINT ( 'NONE',  ( -86.45107053092409899, -35.49386078015379553, 186.8406724003439763 ) ) ;
#84434 = VERTEX_POINT ( 'NONE', #87362 ) ;
#84435 = CARTESIAN_POINT ( 'NONE',  ( 29.85995211472236832, 18.03913124950667424, 39.60535821593451544 ) ) ;
#84436 = CARTESIAN_POINT ( 'NONE',  ( -3.964250166353671112, -18.58602789357551544, 26.98074317074543416 ) ) ;
#84437 = ADVANCED_FACE ( 'NONE', ( #37777, #70104, #103011, #45312, #36191 ), #40267, .F. ) ;
#84438 = CARTESIAN_POINT ( 'NONE',  ( -42.60801251486928720, 467.2312078438266099, 12.94848564814438419 ) ) ;
#84440 = CARTESIAN_POINT ( 'NONE',  ( -7.943938681556293346, 53.91044595262783901, 3.880671334416982976 ) ) ;
#84439 = CARTESIAN_POINT ( 'NONE',  ( -21.19348424345033521, 294.8901562694577478, 1.945151701991089332 ) ) ;
#84441 = ORIENTED_EDGE ( 'NONE', *, *, #8892, .F. ) ;
#84442 = CARTESIAN_POINT ( 'NONE',  ( 1.220173976448186481, 27.62999424518777047, 39.81527922047737889 ) ) ;
#84443 = CARTESIAN_POINT ( 'NONE',  ( -30.29801405241517998, 7.759806510565432802, -41.94638970127596878 ) ) ;
#84444 = CIRCLE ( 'NONE', #79275, 2.000000000000000000 ) ;
#84445 = CARTESIAN_POINT ( 'NONE',  ( 17.59235505452603832, 49.99999999999999289, 62.71843377526943897 ) ) ;
#84446 = CARTESIAN_POINT ( 'NONE',  ( 35.76482652855951017, 405.2378813769876729, 6.148826621638260548 ) ) ;
#84447 = DIRECTION ( 'NONE',  ( 1.000000000000000000, 1.224606353822377258E-16, 0.000000000000000000 ) ) ;
#84448 = DIRECTION ( 'NONE',  ( 0.000000000000000000, -1.000000000000000000, 0.000000000000000000 ) ) ;
#84449 = CARTESIAN_POINT ( 'NONE',  ( 100.7779335074592524, -14.21045842199434084, 117.1442511085924565 ) ) ;
#84450 = CARTESIAN_POINT ( 'NONE',  ( -80.99376376317795234, -36.03179907666569193, 148.3448988380689286 ) ) ;
#84451 = ORIENTED_EDGE ( 'NONE', *, *, #96728, .T. ) ;
#84452 = DIRECTION ( 'NONE',  ( -1.000000000000000000, -1.224606353822377258E-16, -0.000000000000000000 ) ) ;
#84453 = CARTESIAN_POINT ( 'NONE',  ( 5.093082057083956116, 252.4444620642155996, -3.176439207277734766 ) ) ;
#84454 = CARTESIAN_POINT ( 'NONE',  ( 49.85179264443584657, -57.67837586547972961, 76.80686450657027819 ) ) ;
#84455 = APPLICATION_CONTEXT ( 'automotive_design' ) ;
#84456 = CARTESIAN_POINT ( 'NONE',  ( -32.88333705524179607, 439.7317646416724415, 24.13381181826117583 ) ) ;
#84457 = CARTESIAN_POINT ( 'NONE',  ( 45.47623700953192127, 382.7937029844407562, 7.371119132332191626 ) ) ;
#84458 = CARTESIAN_POINT ( 'NONE',  ( 43.72734063489998846, 464.0947689350302880, 7.873621169229567229 ) ) ;
#84459 = ORIENTED_EDGE ( 'NONE', *, *, #5205, .F. ) ;
#84460 = CARTESIAN_POINT ( 'NONE',  ( 31.43086057969960478, 439.6979630470218581, 23.48915592383433193 ) ) ;
#84461 = ORIENTED_EDGE ( 'NONE', *, *, #73204, .T. ) ;
#84462 = FILL_AREA_STYLE_COLOUR ( '', #49840 ) ;
#84463 = PLANE ( 'NONE',  #17041 ) ;
#84464 = CARTESIAN_POINT ( 'NONE',  ( 7.069742150690448312, 41.66287055390499461, -69.58314084581829206 ) ) ;
#84465 = CARTESIAN_POINT ( 'NONE',  ( -42.35263604938428017, 50.00000000000000000, 46.99568999588436924 ) ) ;
#84466 = CARTESIAN_POINT ( 'NONE',  ( 6.073384266099709272, -15.26795065999747436, 14.38582946077996283 ) ) ;
#84467 = VECTOR ( 'NONE', #46922, 1000.000000000000000 ) ;
#84468 = VERTEX_POINT ( 'NONE', #44786 ) ;
#84469 = CARTESIAN_POINT ( 'NONE',  ( 111.1380688386296356, -59.99999999999998579, 186.6089157120882192 ) ) ;
#84471 = CARTESIAN_POINT ( 'NONE',  ( 24.22882282971767864, -56.87184356490050163, 34.54272924709754733 ) ) ;
#84470 = CARTESIAN_POINT ( 'NONE',  ( -75.52856519143354319, -59.99999999999994316, 193.8568173627997737 ) ) ;
#84473 = CARTESIAN_POINT ( 'NONE',  ( 33.95156263172584943, 464.5083255208626838, 6.608064661821377861 ) ) ;
#84472 = UNCERTAINTY_MEASURE_WITH_UNIT (LENGTH_MEASURE( 1.000000000000000082E-05 ), #56380, 'distance_accuracy_value', 'NONE');
#84474 = CARTESIAN_POINT ( 'NONE',  ( 37.46478434938782698, 360.1732274943323659, 2.822779564172262390 ) ) ;
#84475 = AXIS2_PLACEMENT_3D ( 'NONE', #22895, #47128, #46609 ) ;
#84476 = EDGE_CURVE ( 'NONE', #91694, #6703, #67772, .T. ) ;
#84477 = CARTESIAN_POINT ( 'NONE',  ( -41.77985743548467923, -29.15823557948370492, 37.78287941733934474 ) ) ;
#84478 = CARTESIAN_POINT ( 'NONE',  ( -38.38499389483345681, 18.64284798593159564, 1.874612472308246902 ) ) ;
#84479 = UNCERTAINTY_MEASURE_WITH_UNIT (LENGTH_MEASURE( 1.000000000000000082E-05 ), #77512, 'distance_accuracy_value', 'NONE');
#84480 = ORIENTED_EDGE ( 'NONE', *, *, #104587, .T. ) ;
#84481 = DIRECTION ( 'NONE',  ( -0.000000000000000000, 1.000000000000000000, -0.000000000000000000 ) ) ;
#84482 = CARTESIAN_POINT ( 'NONE',  ( 7.482955433003800394, 54.13148333495901454, 3.437080708373401183 ) ) ;
#84483 = DIRECTION ( 'NONE',  ( -1.000000000000000000, -0.000000000000000000, -0.000000000000000000 ) ) ;
#84484 = CARTESIAN_POINT ( 'NONE',  ( 6.400000000000000355, 9.237604307034018802, 0.000000000000000000 ) ) ;
#84485 = CARTESIAN_POINT ( 'NONE',  ( 7.618844049274132502, -61.82764101070539908, 2.450177051822849617 ) ) ;
#84486 = CARTESIAN_POINT ( 'NONE',  ( -36.14398083585128774, 461.0280587598256261, 3.026911855274814656 ) ) ;
#84487 = ORIENTED_EDGE ( 'NONE', *, *, #56365, .F. ) ;
#84488 = CARTESIAN_POINT ( 'NONE',  ( -16.42383576958760472, 37.18011179812618394, -21.84794872343122307 ) ) ;
#84489 = ORIENTED_EDGE ( 'NONE', *, *, #46317, .T. ) ;
#84490 = CARTESIAN_POINT ( 'NONE',  ( 101.0624751218346660, -29.99999999999999289, 167.4344596707726680 ) ) ;
#84491 = CARTESIAN_POINT ( 'NONE',  ( 33.07092925538307782, 40.70022578739308727, -62.17362998248158590 ) ) ;
#84493 = CARTESIAN_POINT ( 'NONE',  ( -4.696906829037973630, -83.56001852512108030, -3.734050370377307360 ) ) ;
#84492 = PRESENTATION_LAYER_ASSIGNMENT (  '', '', ( #24219 ) ) ;
#84494 = CARTESIAN_POINT ( 'NONE',  ( 81.97181451191005408, -30.00000000000001066, 33.65921166970361611 ) ) ;
#84495 = AXIS2_PLACEMENT_3D ( 'NONE', #35716, #27629, #93395 ) ;
#84496 = EDGE_CURVE ( 'NONE', #84500, #79406, #31012, .T. ) ;
#84497 = CARTESIAN_POINT ( 'NONE',  ( -32.13416116311759652, 374.4058483644059265, 24.05691306682159336 ) ) ;
#84498 = VERTEX_POINT ( 'NONE', #101418 ) ;
#84499 = AXIS2_PLACEMENT_3D ( 'NONE', #101785, #44090, #27953 ) ;
#84500 = VERTEX_POINT ( 'NONE', #20012 ) ;
#84501 = EDGE_LOOP ( 'NONE', ( #40437, #56870, #48876, #58593 ) ) ;
#84503 = VERTEX_POINT ( 'NONE', #11856 ) ;
#84502 = CARTESIAN_POINT ( 'NONE',  ( -47.44481056709870614, 11.19259812317955927, -16.71748578406464958 ) ) ;
#84504 = DIRECTION ( 'NONE',  ( -1.000000000000000000, 0.000000000000000000, 0.000000000000000000 ) ) ;
#84505 = DIRECTION ( 'NONE',  ( -1.000000000000000000, 0.000000000000000000, 0.000000000000000000 ) ) ;
#84506 = CARTESIAN_POINT ( 'NONE',  ( 39.75151623530055645, 438.7665981957342751, 23.14798673880785529 ) ) ;
#84507 = CARTESIAN_POINT ( 'NONE',  ( -31.18704516878236177, 357.2439419286618545, 20.55224204967724688 ) ) ;
#84508 = CARTESIAN_POINT ( 'NONE',  ( -8.000000000000000000, 0.000000000000000000, -7.424942857142857733 ) ) ;
#84509 = ORIENTED_EDGE ( 'NONE', *, *, #55410, .T. ) ;
#84510 = CARTESIAN_POINT ( 'NONE',  ( -6.043427762771305112, 50.00000000000000000, -74.51456333905269958 ) ) ;
#84511 = AXIS2_PLACEMENT_3D ( 'NONE', #65186, #98080, #89993 ) ;
#84512 = B_SPLINE_CURVE_WITH_KNOTS ( 'NONE', 3,
 ( #103619, #39952, #72824, #105215, #97630, #56095, #63173, #105729, #5459, #55570, #31361, #14584, #70725, #79339, #89031, #47493, #23794, #45924 ),
 .UNSPECIFIED., .F., .F.,
 ( 4, 2, 2, 2, 2, 2, 2, 2, 4 ),
 ( 0.007150400357696743217, 0.007655146576508041652, 0.008159892795319340086, 0.008664639014130639388, 0.009169385232941936956, 0.009674131451753234523, 0.01017887767056453382, 0.01068362388937583313, 0.01118837010818713069 ),
 .UNSPECIFIED. ) ;
#84513 = ORIENTED_EDGE ( 'NONE', *, *, #76103, .F. ) ;
#84514 = CARTESIAN_POINT ( 'NONE',  ( 75.45453868462554681, -38.35108631456310491, 173.7963811085962789 ) ) ;
#84515 = CARTESIAN_POINT ( 'NONE',  ( 35.59999999999999432, 3.309500000000003439, 0.000000000000000000 ) ) ;
#84516 = CARTESIAN_POINT ( 'NONE',  ( 25.67326358033849942, 305.2097782842129732, 10.46538467574003839 ) ) ;
#84517 = EDGE_CURVE ( 'NONE', #81365, #9776, #14378, .T. ) ;
#84518 = VECTOR ( 'NONE', #80845, 1000.000000000000341 ) ;
#84519 = LINE ( 'NONE', #86662, #18326 ) ;
#84520 = PRODUCT ( '2. Holder', '2. Holder', '', ( #56794 ) ) ;
#84521 = VERTEX_POINT ( 'NONE', #102476 ) ;
#84522 = CARTESIAN_POINT ( 'NONE',  ( 28.71516359314587064, 10.50242333429324582, -41.65501769021862799 ) ) ;
#84523 = CARTESIAN_POINT ( 'NONE',  ( -16.14595037822616419, 12.99999999999999289, 0.000000000000000000 ) ) ;
#84524 = CARTESIAN_POINT ( 'NONE',  ( 27.63977025857940717, 296.6218385434618767, 2.321776652389909490 ) ) ;
#84525 = FACE_OUTER_BOUND ( 'NONE', #54666, .T. ) ;
#84526 = CARTESIAN_POINT ( 'NONE',  ( -5.656854249492381470, -20.56249999999999289, 5.656854249492379694 ) ) ;
#84527 = ORIENTED_EDGE ( 'NONE', *, *, #106672, .T. ) ;
#84529 =( NAMED_UNIT ( * ) SI_UNIT ( $, .STERADIAN. ) SOLID_ANGLE_UNIT ( ) );
#84528 =( LENGTH_UNIT ( ) NAMED_UNIT ( * ) SI_UNIT ( .MILLI., .METRE. ) );
#84530 = DIRECTION ( 'NONE',  ( 0.000000000000000000, 0.000000000000000000, 1.000000000000000000 ) ) ;
#84531 = PLANE ( 'NONE',  #84959 ) ;
#84532 = CARTESIAN_POINT ( 'NONE',  ( 6.646227138586374927, 302.7439599329172779, 9.914178426197896243 ) ) ;
#84533 =( GEOMETRIC_REPRESENTATION_CONTEXT ( 3 ) GLOBAL_UNCERTAINTY_ASSIGNED_CONTEXT ( ( #88461 ) ) GLOBAL_UNIT_ASSIGNED_CONTEXT ( ( #31891, #64259, #104160 ) ) REPRESENTATION_CONTEXT ( 'NONE', 'WORKASPACE' ) );
#84534 = CARTESIAN_POINT ( 'NONE',  ( -7.003653396366579464, 103.9429379444032264, -3.866846144092870752 ) ) ;
#84535 = CIRCLE ( 'NONE', #55174, 0.9999999999999996669 ) ;
#84536 = PRODUCT_RELATED_PRODUCT_CATEGORY ( 'part', '', ( #28705 ) ) ;
#84537 = CARTESIAN_POINT ( 'NONE',  ( -37.56673239365849781, 27.60449318992554169, 13.45617127781067168 ) ) ;
#84538 = CARTESIAN_POINT ( 'NONE',  ( 86.39088408274903941, -17.34302421594473742, 179.9388769400421779 ) ) ;
#84539 = CARTESIAN_POINT ( 'NONE',  ( 24.34999999999999787, 3.309500000000003439, 0.000000000000000000 ) ) ;
#84540 = CARTESIAN_POINT ( 'NONE',  ( -8.971954110056353571, 136.3305255231049671, -1.734723475998474934E-15 ) ) ;
#84541 = EDGE_LOOP ( 'NONE', ( #6282, #91559, #42133, #30141, #28495 ) ) ;
#84542 = CARTESIAN_POINT ( 'NONE',  ( 5.615325946863288564, -57.67109132440626240, -44.55232355965021185 ) ) ;
#84543 = DIRECTION ( 'NONE',  ( 0.000000000000000000, -1.000000000000000000, 0.000000000000000000 ) ) ;
#84544 = DIRECTION ( 'NONE',  ( -0.000000000000000000, -1.000000000000000000, -0.000000000000000000 ) ) ;
#84545 =( BOUNDED_SURFACE ( )  B_SPLINE_SURFACE ( 3, 2, ( 
 ( #59657, #74744, #92537 ),
 ( #48871, #81762, #32739 ),
 ( #65607, #98492, #24644 ),
 ( #57492, #99012, #90417 ),
 ( #16520, #53157, #77426 ),
 ( #29447, #84458, #3542 ),
 ( #52072, #11608, #101700 ),
 ( #62319, #86074, #36480 ),
 ( #93075, #20842, #68272 ),
 ( #103301, #102227, #20309 ) ),
 .UNSPECIFIED., .F., .F., .F. ) 
 B_SPLINE_SURFACE_WITH_KNOTS ( ( 4, 2, 2, 2, 4 ),
 ( 3, 3 ),
 ( 6.505213034913026604E-19, 0.002844712610137182639, 0.003555890762671477974, 0.004267068915205773742, 0.005689425220274364411 ),
 ( 0.000000000000000000, 1.000000000000000000 ),
 .UNSPECIFIED. ) 
 GEOMETRIC_REPRESENTATION_ITEM ( )  RATIONAL_B_SPLINE_SURFACE ( (
 ( 1.000000000000000000, 0.8258027051680146835, 1.000000000000000000),
 ( 1.000000000000000000, 0.8423184768582745452, 1.000000000000000000),
 ( 1.000000000000000000, 0.8479189272860049309, 1.000000000000000000),
 ( 1.000000000000000000, 0.8482780919516984541, 1.000000000000000000),
 ( 1.000000000000000000, 0.8479712937334785705, 1.000000000000000000),
 ( 1.000000000000000000, 0.8466356411039382968, 1.000000000000000000),
 ( 1.000000000000000000, 0.8456087446180271527, 1.000000000000000000),
 ( 1.000000000000000000, 0.8414089630397959541, 1.000000000000000000),
 ( 1.000000000000000000, 0.8371477558891856630, 1.000000000000000000),
 ( 1.000000000000000000, 0.8308329163120958816, 1.000000000000000000) ) ) 
 REPRESENTATION_ITEM ( '' )  SURFACE ( )  );
#84546 = CARTESIAN_POINT ( 'NONE',  ( -94.02980808522455902, -30.00000000000000711, 112.1455996697054900 ) ) ;
#84547 = AXIS2_PLACEMENT_3D ( 'NONE', #70564, #5297, #88343 ) ;
#84548 = DIRECTION ( 'NONE',  ( 0.000000000000000000, 0.000000000000000000, -1.000000000000000000 ) ) ;
#84549 = CARTESIAN_POINT ( 'NONE',  ( -2.558993250146713638, 7.638875775588015671, -7.593821156097209979 ) ) ;
#84551 = SURFACE_STYLE_FILL_AREA ( #3633 ) ;
#84550 = CARTESIAN_POINT ( 'NONE',  ( -9.842473135306432752, 246.4106818288640568, 1.785129593756279220 ) ) ;
#84552 = EDGE_CURVE ( 'NONE', #28621, #85839, #91939, .T. ) ;
#84553 = DIRECTION ( 'NONE',  ( 0.000000000000000000, 0.000000000000000000, 1.000000000000000000 ) ) ;
#84554 = CARTESIAN_POINT ( 'NONE',  ( -32.00612393675804412, -31.56328806623667660, 32.42231260273467086 ) ) ;
#84555 = CARTESIAN_POINT ( 'NONE',  ( -19.32515916410156009, 49.99999999999999289, 60.14378497377332167 ) ) ;
#84556 = CARTESIAN_POINT ( 'NONE',  ( -43.52560348121802747, 486.7876442849098453, 7.034435017230201481 ) ) ;
#84557 = LINE ( 'NONE', #26361, #8070 ) ;
#84558 = B_SPLINE_CURVE_WITH_KNOTS ( 'NONE', 3,
 ( #64023, #81219, #7336, #71543, #63486, #88806, #88283, #80693, #40245, #104445, #72612, #103916, #72085, #104992, #30597, #6270 ),
 .UNSPECIFIED., .F., .F.,
 ( 4, 2, 2, 2, 2, 2, 2, 4 ),
 ( 2.478060227011367563E-17, 0.0007707015628690528459, 0.001156052344303514163, 0.001541403125737975371, 0.001926753907172436579, 0.002312104688606898221, 0.002697455470041359212, 0.003082806251475820637 ),
 .UNSPECIFIED. ) ;
#84559 = CARTESIAN_POINT ( 'NONE',  ( 56.43757173888357670, -28.73354875062528890, -26.14196234985615064 ) ) ;
#84560 = CARTESIAN_POINT ( 'NONE',  ( -26.15948994066758715, -25.57049903555443748, 29.61355792721284175 ) ) ;
#84561 = CONICAL_SURFACE ( 'NONE', #8782, 4.172000000000001485, 0.9599310885968750373 ) ;
#84562 = CIRCLE ( 'NONE', #27792, 3.309500000000001663 ) ;
#84563 = ORIENTED_EDGE ( 'NONE', *, *, #84496, .F. ) ;
#84564 = CARTESIAN_POINT ( 'NONE',  ( 6.704772934685585994, 9.540285309610183617, -2.024104295774001194 ) ) ;
#84565 = CYLINDRICAL_SURFACE ( 'NONE', #15949, 5.000000000000002665 ) ;
#84566 = CARTESIAN_POINT ( 'NONE',  ( -16.83015825594305426, -42.95785322665913952, 31.29329447951673870 ) ) ;
#84567 = EDGE_CURVE ( 'NONE', #93427, #19599, #4307, .T. ) ;
#84568 = CARTESIAN_POINT ( 'NONE',  ( -60.15663760392290982, -29.26964696484472483, -24.92025292455906893 ) ) ;
#84569 = CONICAL_SURFACE ( 'NONE', #77635, 3.309500000000007880, 0.9599310885968770357 ) ;
#84570 = EDGE_CURVE ( 'NONE', #37991, #31075, #61503, .T. ) ;
#84572 = CARTESIAN_POINT ( 'NONE',  ( -64.94678499638771996, -34.58945069958795671, -23.72257533880744873 ) ) ;
#84571 = CARTESIAN_POINT ( 'NONE',  ( 9.833493305133801599, 1.593028355512270567E-15, 0.000000000000000000 ) ) ;
#84573 = ORIENTED_EDGE ( 'NONE', *, *, #105601, .T. ) ;
#84574 = AXIS2_PLACEMENT_3D ( 'NONE', #50962, #17570, #50431 ) ;
#84575 = CARTESIAN_POINT ( 'NONE',  ( -35.86608289195888233, 437.2866345698543569, 4.452337163522260610 ) ) ;
#84576 = ORIENTED_EDGE ( 'NONE', *, *, #72468, .T. ) ;
#84577 = AXIS2_PLACEMENT_3D ( 'NONE', #47939, #87902, #46890 ) ;
#84578 = CIRCLE ( 'NONE', #38117, 4.000000000000001776 ) ;
#84579 = CARTESIAN_POINT ( 'NONE',  ( 24.83349330513380337, 4.000000000000002665, 0.000000000000000000 ) ) ;
#84580 = ORIENTED_EDGE ( 'NONE', *, *, #36564, .F. ) ;
#84581 =( NAMED_UNIT ( * ) SI_UNIT ( $, .STERADIAN. ) SOLID_ANGLE_UNIT ( ) );
#84582 = CARTESIAN_POINT ( 'NONE',  ( 101.0491831504412659, -52.74036209462195046, 193.3224896004936681 ) ) ;
#84584 = CARTESIAN_POINT ( 'NONE',  ( -7.213352437320215138, -7.981635269923192055, -3.463014597543478512 ) ) ;
#84583 = CARTESIAN_POINT ( 'NONE',  ( 8.922146979286338819, -20.27139005636187008, 27.26475389761597512 ) ) ;
#84585 = ORIENTED_EDGE ( 'NONE', *, *, #38069, .F. ) ;
#84586 = VERTEX_POINT ( 'NONE', #94397 ) ;
#84587 = ORIENTED_EDGE ( 'NONE', *, *, #78451, .F. ) ;
#84588 = CARTESIAN_POINT ( 'NONE',  ( 27.67623204030578421, 310.9913909337609539, 11.64485516987953240 ) ) ;
#84589 = DIRECTION ( 'NONE',  ( 1.000000000000000000, 0.000000000000000000, 0.000000000000000000 ) ) ;
#84590 = CARTESIAN_POINT ( 'NONE',  ( 15.39075092899655317, 46.20845424323130146, 5.262406961020114515 ) ) ;
#84591 = ORIENTED_EDGE ( 'NONE', *, *, #61037, .T. ) ;
#84592 = CARTESIAN_POINT ( 'NONE',  ( 0.000000000000000000, 0.000000000000000000, 0.000000000000000000 ) ) ;
#84593 = FILL_AREA_STYLE ('',( #42522 ) ) ;
#84594 = DIRECTION ( 'NONE',  ( 0.000000000000000000, 0.000000000000000000, 1.000000000000000000 ) ) ;
#84596 = CARTESIAN_POINT ( 'NONE',  ( -101.3184166277729048, -59.99999999996092725, 74.64939812631605776 ) ) ;
#84595 =( GEOMETRIC_REPRESENTATION_CONTEXT ( 3 ) GLOBAL_UNCERTAINTY_ASSIGNED_CONTEXT ( ( #40760 ) ) GLOBAL_UNIT_ASSIGNED_CONTEXT ( ( #47275, #28094, #60450 ) ) REPRESENTATION_CONTEXT ( 'NONE', 'WORKASPACE' ) );
#84597 = LINE ( 'NONE', #3139, #49459 ) ;
#84598 = CARTESIAN_POINT ( 'NONE',  ( -32.54922218626916930, 319.8023524069591303, -6.363686095274232457 ) ) ;
#84599 = CARTESIAN_POINT ( 'NONE',  ( -6.641837642500876271, 41.74662713182689089, -59.04567091375639620 ) ) ;
#84600 = CARTESIAN_POINT ( 'NONE',  ( -85.55948822751662419, -29.99999999999991829, -20.40846083852196813 ) ) ;
#84601 = EDGE_CURVE ( 'NONE', #94586, #3543, #82936, .T. ) ;
#84602 = CARTESIAN_POINT ( 'NONE',  ( -50.14550149790785838, -42.97898697507390153, 52.14561158908378502 ) ) ;
#84603 = AXIS2_PLACEMENT_3D ( 'NONE', #9530, #17655, #74797 ) ;
#84604 = ORIENTED_EDGE ( 'NONE', *, *, #40202, .T. ) ;
#84605 = DIRECTION ( 'NONE',  ( 0.000000000000000000, 0.000000000000000000, 1.000000000000000000 ) ) ;
#84606 = ORIENTED_EDGE ( 'NONE', *, *, #72848, .F. ) ;
#84607 = DIRECTION ( 'NONE',  ( -1.000000000000000000, -0.000000000000000000, -0.000000000000000000 ) ) ;
#84608 = CARTESIAN_POINT ( 'NONE',  ( -9.407137736701065123, 302.6622268194199705, -10.04029227552683068 ) ) ;
#84609 = DIRECTION ( 'NONE',  ( -1.000000000000000000, -0.000000000000000000, -0.000000000000000000 ) ) ;
#84610 = EDGE_LOOP ( 'NONE', ( #98394, #60703, #24283, #51161, #65056, #105 ) ) ;
#84611 = CARTESIAN_POINT ( 'NONE',  ( 105.4486652112230018, -38.38584500015401346, 197.0171471424765173 ) ) ;
#84612 = CARTESIAN_POINT ( 'NONE',  ( 3.841398122528194126, -48.92777529680783033, 104.5835869663331579 ) ) ;
#84613 = CARTESIAN_POINT ( 'NONE',  ( -19.15465222815915070, 294.6774222264219247, 1.900466129964910378 ) ) ;
#84614 = CARTESIAN_POINT ( 'NONE',  ( 79.13121736040859844, 42.00000000000000000, -45.60838156035022450 ) ) ;
#84615 = CARTESIAN_POINT ( 'NONE',  ( 87.76354976536211439, -30.00000000000000711, 186.1681723011733993 ) ) ;
#84616 = CARTESIAN_POINT ( 'NONE',  ( -10.61258144643682577, 43.90877112545464911, -12.94048881062180811 ) ) ;
#84617 = ADVANCED_FACE ( 'NONE', ( #45836 ), #94934, .F. ) ;
#84618 = FACE_OUTER_BOUND ( 'NONE', #46541, .T. ) ;
#84619 = VECTOR ( 'NONE', #38101, 1000.000000000000000 ) ;
#84620 = EDGE_LOOP ( 'NONE', ( #4065, #7170, #85935, #37365, #62457 ) ) ;
#84621 = VERTEX_POINT ( 'NONE', #57087 ) ;
#84622 = CARTESIAN_POINT ( 'NONE',  ( 51.80856163756618571, -22.18394510151134469, 47.83007306119799296 ) ) ;
#84623 = CARTESIAN_POINT ( 'NONE',  ( -46.00000000000000000, 437.9173578870133952, 12.34179081168478298 ) ) ;
#84624 = DIRECTION ( 'NONE',  ( 0.000000000000000000, 0.000000000000000000, 1.000000000000000000 ) ) ;
#84625 = VERTEX_POINT ( 'NONE', #38809 ) ;
#84626 = CARTESIAN_POINT ( 'NONE',  ( -85.43130989759367822, -38.35985338504925579, -22.45028662619849058 ) ) ;
#84627 = ORIENTED_EDGE ( 'NONE', *, *, #57313, .F. ) ;
#84628 = CARTESIAN_POINT ( 'NONE',  ( 106.8950603560237482, -38.36540817785023449, 195.0234272126446342 ) ) ;
#84629 = CARTESIAN_POINT ( 'NONE',  ( 12.42199367956279765, 22.57433134022317844, -6.088470440402769412 ) ) ;
#84630 = CARTESIAN_POINT ( 'NONE',  ( 87.99907843909515748, -45.28282746162219752, 58.11307062178342875 ) ) ;
#84631 =( NAMED_UNIT ( * ) SI_UNIT ( $, .STERADIAN. ) SOLID_ANGLE_UNIT ( ) );
#84632 = CARTESIAN_POINT ( 'NONE',  ( -20.95526673416674868, 304.9223276462623744, -8.985009476610910539 ) ) ;
#84633 = CARTESIAN_POINT ( 'NONE',  ( 6.708832649680419813, -13.06702039274575888, -7.389177399647247846 ) ) ;
#84634 = EDGE_CURVE ( 'NONE', #90543, #85237, #9198, .T. ) ;
#84635 = DIRECTION ( 'NONE',  ( 0.000000000000000000, -1.000000000000000000, 0.000000000000000000 ) ) ;
#84636 = AXIS2_PLACEMENT_3D ( 'NONE', #105083, #40334, #39821 ) ;
#84637 = LINE ( 'NONE', #35051, #95691 ) ;
#84638 = AXIS2_PLACEMENT_3D ( 'NONE', #21793, #64360, #88618 ) ;
#84639 = CARTESIAN_POINT ( 'NONE',  ( 2.955796066023812063, 53.34212538443676976, 5.000000000000000000 ) ) ;
#84640 = ORIENTED_EDGE ( 'NONE', *, *, #97910, .F. ) ;
#84641 = EDGE_CURVE ( 'NONE', #68930, #4192, #88486, .T. ) ;
#84642 = CARTESIAN_POINT ( 'NONE',  ( 44.78945892759311675, 1.340359594676612611E-15, 0.000000000000000000 ) ) ;
#84643 = DIRECTION ( 'NONE',  ( -1.000000000000000000, 0.000000000000000000, 0.000000000000000000 ) ) ;
#84644 = LINE ( 'NONE', #53339, #28195 ) ;
#84645 = CONICAL_SURFACE ( 'NONE', #91502, 4.172000000000009479, 0.9599310885968813656 ) ;
#84646 = VERTEX_POINT ( 'NONE', #97025 ) ;
#84647 = CARTESIAN_POINT ( 'NONE',  ( -34.55934088217597377, 338.7551446543786824, -0.7819439798765525085 ) ) ;
#84648 = CARTESIAN_POINT ( 'NONE',  ( -37.13583097524582399, 311.9121134930005610, 14.04606923393727058 ) ) ;
#84649 = CARTESIAN_POINT ( 'NONE',  ( -12.10346316003903056, -4.692865865568782269, -76.82923406330107241 ) ) ;
#84650 = CARTESIAN_POINT ( 'NONE',  ( 20.11650669486618881, 1.474610560812782335E-15, 0.000000000000000000 ) ) ;
#84651 = CARTESIAN_POINT ( 'NONE',  ( 5.656854249492380582, -25.81249999999999645, -5.656854249492379694 ) ) ;
#84652 = CARTESIAN_POINT ( 'NONE',  ( 50.79025413206112205, -29.86198917105789619, 47.81129180970600601 ) ) ;
#84653 = CIRCLE ( 'NONE', #41597, 4.000000000000000888 ) ;
#84654 = DIRECTION ( 'NONE',  ( 0.5735764363510490460, 0.8191520442889896891, 0.000000000000000000 ) ) ;
#84655 = VERTEX_POINT ( 'NONE', #95980 ) ;
#84656 = CARTESIAN_POINT ( 'NONE',  ( 83.72818806616849940, -42.97983555213142637, 180.3459984342655957 ) ) ;
#84657 = EDGE_CURVE ( 'NONE', #77405, #6205, #7847, .T. ) ;
#84658 = CARTESIAN_POINT ( 'NONE',  ( -16.48303619537882625, 45.94111582078982536, 4.157797401561652784 ) ) ;
#84659 = ORIENTED_EDGE ( 'NONE', *, *, #86522, .F. ) ;
#84660 = EDGE_CURVE ( 'NONE', #65653, #18077, #52273, .T. ) ;
#84661 = CARTESIAN_POINT ( 'NONE',  ( -100.3578242334469337, -52.71019514449881882, 125.2399389498935136 ) ) ;
#84662 = FACE_OUTER_BOUND ( 'NONE', #106086, .T. ) ;
#84663 = CARTESIAN_POINT ( 'NONE',  ( -14.73122683063112603, -3.000000000000002665, -81.05502296678270113 ) ) ;
#84664 = CARTESIAN_POINT ( 'NONE',  ( 46.00000000000000000, 450.0000000000002274, 13.20242257375370976 ) ) ;
#84665 = CARTESIAN_POINT ( 'NONE',  ( -18.18925383356936720, -25.18032758874422683, -38.50619832935123554 ) ) ;
#84666 = CARTESIAN_POINT ( 'NONE',  ( 41.57491510848411309, -60.00000000000000000, 54.47207502686755021 ) ) ;
#84667 = PRESENTATION_LAYER_ASSIGNMENT (  '', '', ( #74333 ) ) ;
#84668 = CARTESIAN_POINT ( 'NONE',  ( 27.30418487774501202, -30.61949767632602715, 39.20238763744198707 ) ) ;
#84669 = CARTESIAN_POINT ( 'NONE',  ( 7.801777176595949825, 108.5882798581263131, -1.786991866639918936 ) ) ;
#84670 = CARTESIAN_POINT ( 'NONE',  ( 19.73225841471719022, -16.99122103950224627, 31.48169930546135120 ) ) ;
#84672 = CARTESIAN_POINT ( 'NONE',  ( -12.85466265431899124, 23.42010317047945378, 4.868175573428279890 ) ) ;
#84671 = CARTESIAN_POINT ( 'NONE',  ( -35.29827408586819359, -35.67579097495918461, 44.48726958153784494 ) ) ;
#84673 = CIRCLE ( 'NONE', #31265, 4.000000000000000888 ) ;
#84674 = CARTESIAN_POINT ( 'NONE',  ( 2.435618412119228804, 294.8338784867337381, -9.717600221945083661 ) ) ;
#84675 = CARTESIAN_POINT ( 'NONE',  ( 37.51854390953261742, 313.5286481325095451, 14.45587837336505999 ) ) ;
#84676 = DIRECTION ( 'NONE',  ( 0.000000000000000000, 1.000000000000000000, -0.000000000000000000 ) ) ;
#84677 = DIRECTION ( 'NONE',  ( 1.000000000000000000, 0.000000000000000000, 0.000000000000000000 ) ) ;
#84678 = ORIENTED_EDGE ( 'NONE', *, *, #54066, .T. ) ;
#84679 = CARTESIAN_POINT ( 'NONE',  ( 0.000000000000000000, 4.898587196589413815E-16, -4.000000000000000888 ) ) ;
#84680 = CARTESIAN_POINT ( 'NONE',  ( -17.49999999999995381, 51.97748320727993843, 60.75044042984304582 ) ) ;
#84681 = FILL_AREA_STYLE ('',( #2143 ) ) ;
#84682 = CARTESIAN_POINT ( 'NONE',  ( -41.85455215201762513, 465.6883253721317146, 15.30917575692330246 ) ) ;
#84683 = EDGE_CURVE ( 'NONE', #22906, #82852, #104012, .T. ) ;
#84684 = CARTESIAN_POINT ( 'NONE',  ( 38.79056939014538585, -60.22819850092196958, -34.02320223531833676 ) ) ;
#84685 = ORIENTED_EDGE ( 'NONE', *, *, #55535, .T. ) ;
#84686 = CARTESIAN_POINT ( 'NONE',  ( 0.000000000000000000, 300.0000000000000000, 0.000000000000000000 ) ) ;
#84687 = DIRECTION ( 'NONE',  ( -0.000000000000000000, -0.000000000000000000, -1.000000000000000000 ) ) ;
#84688 = ORIENTED_EDGE ( 'NONE', *, *, #105904, .F. ) ;
#84689 = EDGE_CURVE ( 'NONE', #106204, #99028, #12704, .T. ) ;
#84690 = SHAPE_REPRESENTATION ( '8. Bar', ( #10728 ), #90114 ) ;
#84691 = DIRECTION ( 'NONE',  ( 0.000000000000000000, 0.000000000000000000, -1.000000000000000000 ) ) ;
#84692 = DIRECTION ( 'NONE',  ( 0.000000000000000000, -1.000000000000000000, 0.000000000000000000 ) ) ;
#84693 = DIRECTION ( 'NONE',  ( 0.000000000000000000, 0.000000000000000000, 1.000000000000000000 ) ) ;
#84694 = CARTESIAN_POINT ( 'NONE',  ( -92.06170028002134131, -60.00000000000000000, 19.77329225891599407 ) ) ;
#84695 = DIRECTION ( 'NONE',  ( 0.000000000000000000, -3.700743415417185576E-15, -1.000000000000000000 ) ) ;
#84696 = CARTESIAN_POINT ( 'NONE',  ( 4.613983237546153582, -6.452243898629819618, -7.591546097228406786 ) ) ;
#84697 = CARTESIAN_POINT ( 'NONE',  ( 21.23684446602550935, 304.9566545053270943, -9.977713076987674512 ) ) ;
#84698 = CARTESIAN_POINT ( 'NONE',  ( 40.53119313125029066, 460.3380581626494745, 2.322614769220080699 ) ) ;
#84699 = CARTESIAN_POINT ( 'NONE',  ( -9.999999999999992895, -3.000000000000002665, -83.69100306252320820 ) ) ;
#84700 = CARTESIAN_POINT ( 'NONE',  ( -81.96316505919669737, -49.96949351764808256, 176.6395136813214606 ) ) ;
#84701 = VERTEX_POINT ( 'NONE', #104053 ) ;
#84702 = CYLINDRICAL_SURFACE ( 'NONE', #66071, 1.249999999999999778 ) ;
#84703 =( GEOMETRIC_REPRESENTATION_CONTEXT ( 3 ) GLOBAL_UNCERTAINTY_ASSIGNED_CONTEXT ( ( #68297 ) ) GLOBAL_UNIT_ASSIGNED_CONTEXT ( ( #102024, #28185, #53991 ) ) REPRESENTATION_CONTEXT ( 'NONE', 'WORKASPACE' ) );
#84704 = EDGE_LOOP ( 'NONE', ( #33178, #41697, #2065, #17660 ) ) ;
#84705 = EDGE_LOOP ( 'NONE', ( #36328, #49038, #99938, #11660 ) ) ;
#84706 = CARTESIAN_POINT ( 'NONE',  ( -4.284822031654928587, -1.092833614412262122, 104.4267991316945370 ) ) ;
#84707 = CARTESIAN_POINT ( 'NONE',  ( -3.631902923573203879, -4.332661967060489339, 17.83376356531591611 ) ) ;
#84708 = CARTESIAN_POINT ( 'NONE',  ( 29.00000000000001066, 1.102182119232617714E-15, -9.000000000000000000 ) ) ;
#84709 = EDGE_LOOP ( 'NONE', ( #52198, #35592, #24236, #49319 ) ) ;
#84710 = DIRECTION ( 'NONE',  ( 0.000000000000000000, 0.000000000000000000, 1.000000000000000000 ) ) ;
#84711 = CARTESIAN_POINT ( 'NONE',  ( -95.04855897266367037, -57.67186573470212352, 33.03592761066350647 ) ) ;
#84712 = CARTESIAN_POINT ( 'NONE',  ( -23.21751746555244722, 25.25267828308493634, 33.20617127781060418 ) ) ;
#84713 = LINE ( 'NONE', #41062, #75407 ) ;
#84714 = CARTESIAN_POINT ( 'NONE',  ( 10.73176661990081371, 0.000000000000000000, 5.000000000000002665 ) ) ;
#84715 = CARTESIAN_POINT ( 'NONE',  ( 44.35000000000000142, 1.533819458162526451E-15, 0.000000000000000000 ) ) ;
#84716 = CARTESIAN_POINT ( 'NONE',  ( -5.000000000000000000, -14.21727251091160404, 9.320362779991915758 ) ) ;
#84717 = CONICAL_SURFACE ( 'NONE', #45162, 3.309500000000001663, 0.9599310885968770357 ) ;
#84718 = CARTESIAN_POINT ( 'NONE',  ( 94.55541571559547265, -59.99999999999990763, 22.40038052076814878 ) ) ;
#84719 = CIRCLE ( 'NONE', #81228, 4.171999999999999709 ) ;
#84720 = CARTESIAN_POINT ( 'NONE',  ( -75.43392636619238090, -30.00000000000003553, 160.3050061908775206 ) ) ;
#84721 = ADVANCED_FACE ( 'NONE', ( #40383 ), #29993, .T. ) ;
#84722 = CARTESIAN_POINT ( 'NONE',  ( -57.28148858968405222, -56.86046258776218565, 73.21236583999979075 ) ) ;
#84723 = EDGE_LOOP ( 'NONE', ( #46230, #67989 ) ) ;
#84724 = SURFACE_SIDE_STYLE ('',( #59943 ) ) ;
#84725 = VERTEX_POINT ( 'NONE', #87890 ) ;
#84726 = CARTESIAN_POINT ( 'NONE',  ( -101.5550978881653776, -37.82069211984403978, 186.3190918155810891 ) ) ;
#84727 = SURFACE_STYLE_USAGE ( .BOTH. , #44817 ) ;
#84728 = DIRECTION ( 'NONE',  ( 0.000000000000000000, -1.000000000000000000, 0.000000000000000000 ) ) ;
#84729 = EDGE_CURVE ( 'NONE', #92720, #10253, #86416, .T. ) ;
#84730 = CARTESIAN_POINT ( 'NONE',  ( 1.435596609963271764, -30.00000000000001066, 7.059243743694297635 ) ) ;
#84731 = VERTEX_POINT ( 'NONE', #413 ) ;
#84732 = CARTESIAN_POINT ( 'NONE',  ( 9.500000000000003553, -4.999999999999998224, -68.91429205785459544 ) ) ;
#84733 = CARTESIAN_POINT ( 'NONE',  ( -74.98993051287176570, -60.00000000000002132, 181.2383444034526292 ) ) ;
#84734 = CARTESIAN_POINT ( 'NONE',  ( 36.39102669964498915, 25.97871626027877667, -12.63845754337161864 ) ) ;
#84735 = CARTESIAN_POINT ( 'NONE',  ( -7.188101187500001821, -23.37500000204839168, -2.977408999572651371 ) ) ;
#84736 = DIRECTION ( 'NONE',  ( 0.000000000000000000, 0.000000000000000000, 1.000000000000000000 ) ) ;
#84737 = DIRECTION ( 'NONE',  ( 0.000000000000000000, -1.000000000000000000, 0.000000000000000000 ) ) ;
#84738 = CARTESIAN_POINT ( 'NONE',  ( 16.46939662768644652, -0.000000000000000000, -4.418225343323719301 ) ) ;
#84739 = CARTESIAN_POINT ( 'NONE',  ( -23.61963550967466574, 306.0340374937824777, 10.19690224617928287 ) ) ;
#84740 = FILL_AREA_STYLE_COLOUR ( '', #21517 ) ;
#84741 = EDGE_CURVE ( 'NONE', #92807, #27686, #18211, .T. ) ;
#84742 = DIRECTION ( 'NONE',  ( -0.000000000000000000, 1.000000000000000000, 0.000000000000000000 ) ) ;
#84743 = UNCERTAINTY_MEASURE_WITH_UNIT (LENGTH_MEASURE( 1.000000000000000082E-05 ), #47502, 'distance_accuracy_value', 'NONE');
#84744 = CARTESIAN_POINT ( 'NONE',  ( -30.11975150981648852, -60.33646582423781979, 36.84978483557001994 ) ) ;
#84745 = B_SPLINE_CURVE_WITH_KNOTS ( 'NONE', 3,
 ( #30049, #12763, #64009, #96373, #4698, #54814, #13824, #8392, #16490, #65039, #32159, #73102, #56928, #42356 ),
 .UNSPECIFIED., .F., .F.,
 ( 4, 2, 2, 2, 2, 2, 4 ),
 ( 2.602085213965210642E-18, 0.001035928240051109178, 0.001553892360076662574, 0.002071856480102215754, 0.002589820600127769150, 0.003107784720153322546, 0.004143712960204457528 ),
 .UNSPECIFIED. ) ;
#84746 = CARTESIAN_POINT ( 'NONE',  ( 2.020820481867037888, 21.31435198444414070, 6.705773521646341884 ) ) ;
#84747 = UNCERTAINTY_MEASURE_WITH_UNIT (LENGTH_MEASURE( 1.000000000000000082E-05 ), #70043, 'distance_accuracy_value', 'NONE');
#84748 = CARTESIAN_POINT ( 'NONE',  ( 45.39934709178754701, -29.15827231024250921, 41.32491508119058210 ) ) ;
#84749 =( GEOMETRIC_REPRESENTATION_CONTEXT ( 3 ) GLOBAL_UNCERTAINTY_ASSIGNED_CONTEXT ( ( #16144 ) ) GLOBAL_UNIT_ASSIGNED_CONTEXT ( ( #22431, #69494, #28532 ) ) REPRESENTATION_CONTEXT ( 'NONE', 'WORKASPACE' ) );
#84750 = CARTESIAN_POINT ( 'NONE',  ( -32.78741055188836384, 485.3331003366710092, 5.977022408746766047 ) ) ;
#84751 = CARTESIAN_POINT ( 'NONE',  ( -5.744562646538029504, 13.27102973350405080, 4.000000000000000000 ) ) ;
#84752 = CARTESIAN_POINT ( 'NONE',  ( -85.96729481479134449, -38.64372570064532653, 199.0413494251739337 ) ) ;
#84753 = ORIENTED_EDGE ( 'NONE', *, *, #99432, .T. ) ;
#84755 = DIRECTION ( 'NONE',  ( 0.000000000000000000, 0.000000000000000000, 1.000000000000000000 ) ) ;
#84754 = CARTESIAN_POINT ( 'NONE',  ( 84.55232465008280940, -38.35844130464479207, -23.23874272793522877 ) ) ;
#84756 = CARTESIAN_POINT ( 'NONE',  ( 38.00499196079799447, -59.99999999999999289, 41.32896168422335847 ) ) ;
#84757 = DIRECTION ( 'NONE',  ( -1.000000000000000000, -1.224606353822377258E-16, -0.000000000000000000 ) ) ;
#84758 = CARTESIAN_POINT ( 'NONE',  ( -7.090506018371190322, 41.24767894959148151, -58.61600934880981839 ) ) ;
#84759 = CARTESIAN_POINT ( 'NONE',  ( 7.036764706176849238, 40.29466777802799271, -71.06385277369803077 ) ) ;
#84760 = DIRECTION ( 'NONE',  ( -1.000000000000000000, -1.224606353822377258E-16, -0.000000000000000000 ) ) ;
#84761 = CARTESIAN_POINT ( 'NONE',  ( -23.95966359935239609, 306.2573737793246664, 9.247948789945837689 ) ) ;
#84762 = CARTESIAN_POINT ( 'NONE',  ( 6.936184427528457874, 0.000000000000000000, 0.000000000000000000 ) ) ;
#84763 = CARTESIAN_POINT ( 'NONE',  ( 112.2172298700076283, -60.00000000000000711, 170.6121558011703598 ) ) ;
#84764 = CARTESIAN_POINT ( 'NONE',  ( 5.819846122303831137, -6.321060697774819381, 2.051601713727242426 ) ) ;
#84765 = DIRECTION ( 'NONE',  ( -1.000000000000000000, -0.000000000000000000, -0.000000000000000000 ) ) ;
#84766 = VERTEX_POINT ( 'NONE', #42508 ) ;
#84767 = EDGE_CURVE ( 'NONE', #67620, #23775, #28224, .T. ) ;
#84768 = CARTESIAN_POINT ( 'NONE',  ( 1.276500347551263737, -50.00000000000000000, 101.3106844269525340 ) ) ;
#84769 = CYLINDRICAL_SURFACE ( 'NONE', #91749, 11.27631144943088515 ) ;
#84770 = ORIENTED_EDGE ( 'NONE', *, *, #36687, .F. ) ;
#84772 = FACE_OUTER_BOUND ( 'NONE', #103918, .T. ) ;
#84771 =( NAMED_UNIT ( * ) PLANE_ANGLE_UNIT ( ) SI_UNIT ( $, .RADIAN. ) );
#84773 = PRESENTATION_STYLE_ASSIGNMENT (( #33579 ) ) ;
#84774 =( NAMED_UNIT ( * ) SI_UNIT ( $, .STERADIAN. ) SOLID_ANGLE_UNIT ( ) );
#84775 = CARTESIAN_POINT ( 'NONE',  ( 89.99999999999997158, -60.00000000000000000, 194.0238439516549818 ) ) ;
#84776 = CARTESIAN_POINT ( 'NONE',  ( -5.082755093536325042, -20.46875000204838813, -5.082755093536325930 ) ) ;
#84777 = CARTESIAN_POINT ( 'NONE',  ( 9.596002107493083244, -5.000000000000002665, -77.62543935902139935 ) ) ;
#84778 = EDGE_CURVE ( 'NONE', #89053, #96664, #14342, .T. ) ;
#84779 = UNCERTAINTY_MEASURE_WITH_UNIT (LENGTH_MEASURE( 1.000000000000000082E-05 ), #24041, 'distance_accuracy_value', 'NONE');
#84780 = FACE_OUTER_BOUND ( 'NONE', #105450, .T. ) ;
#84781 = ORIENTED_EDGE ( 'NONE', *, *, #57496, .T. ) ;
#84782 = CARTESIAN_POINT ( 'NONE',  ( 83.05514034890428832, -36.01272047364142992, 164.7561459065111364 ) ) ;
#84783 = CARTESIAN_POINT ( 'NONE',  ( -3.454253436624934004, -0.8414180287960428828, 103.7259032015043232 ) ) ;
#84784 = B_SPLINE_CURVE_WITH_KNOTS ( 'NONE', 3,
 ( #101526, #37356, #69697, #4418, #52426, #2272, #43812, #3895, #69175, #70220, #103121, #53505, #29272, #62152, #102043, #27143 ),
 .UNSPECIFIED., .F., .F.,
 ( 4, 2, 2, 2, 2, 2, 2, 4 ),
 ( 7.196489415735148522E-17, 0.0007700875212649647061, 0.001155131281897411009, 0.001540175042529857421, 0.001925218803162303833, 0.002310262563794750028, 0.002695306324427196656, 0.003080350085059642851 ),
 .UNSPECIFIED. ) ;
#84785 = PLANE ( 'NONE',  #28269 ) ;
#84786 = ORIENTED_EDGE ( 'NONE', *, *, #40352, .F. ) ;
#84787 = AXIS2_PLACEMENT_3D ( 'NONE', #86412, #37338, #62136 ) ;
#84788 = CARTESIAN_POINT ( 'NONE',  ( 65.03872891708842019, 4.898587196589294500E-16, -4.000000000000007105 ) ) ;
#84789 = EDGE_CURVE ( 'NONE', #105857, #37936, #10912, .T. ) ;
#84790 = SURFACE_STYLE_FILL_AREA ( #27661 ) ;
#84791 = CYLINDRICAL_SURFACE ( 'NONE', #90349, 3.400000000000000355 ) ;
#84792 = CARTESIAN_POINT ( 'NONE',  ( -10.00000000000000355, 15.00000000000000000, -10.00000000000000000 ) ) ;
#84793 = CIRCLE ( 'NONE', #17585, 4.172000000000001485 ) ;
#84794 = CARTESIAN_POINT ( 'NONE',  ( -6.000208918519490453, 254.0003133778996300, -0.2646532170642417747 ) ) ;
#84795 = CARTESIAN_POINT ( 'NONE',  ( 16.64348903516524203, 43.75610143575153188, 4.157797401561407646 ) ) ;
#84796 = CARTESIAN_POINT ( 'NONE',  ( 9.081552814318261113, -1.588707212875608343, 15.49454491418383739 ) ) ;
#84797 = VERTEX_POINT ( 'NONE', #58711 ) ;
#84798 = UNCERTAINTY_MEASURE_WITH_UNIT (LENGTH_MEASURE( 1.000000000000000082E-05 ), #28863, 'distance_accuracy_value', 'NONE');
#84799 = FACE_OUTER_BOUND ( 'NONE', #9527, .T. ) ;
#84800 = CARTESIAN_POINT ( 'NONE',  ( -5.000000000000000000, -68.02685735654881682, 16.47960771717093209 ) ) ;
#84801 = CARTESIAN_POINT ( 'NONE',  ( 86.36684635806597043, -61.01915684967102038, 194.5641491802014968 ) ) ;
#84802 = AXIS2_PLACEMENT_3D ( 'NONE', #46212, #103900, #13818 ) ;
#84803 = FACE_OUTER_BOUND ( 'NONE', #78871, .T. ) ;
#84804 = CARTESIAN_POINT ( 'NONE',  ( 4.401442555609581635E-16, -23.28125000204838457, -7.188101187500000044 ) ) ;
#84805 = CARTESIAN_POINT ( 'NONE',  ( -41.59000009475712289, 487.6876459975654825, 9.910902919395237376 ) ) ;
#84806 = DIRECTION ( 'NONE',  ( 0.000000000000000000, 0.000000000000000000, -1.000000000000000000 ) ) ;
#84807 = CARTESIAN_POINT ( 'NONE',  ( 14.44768974034866993, 5.957293599828272335, 7.129930386717071578 ) ) ;
#84808 = ITEM_DEFINED_TRANSFORMATION ( 'NONE', 'NONE', #54143,  #10728 ) ;
#84809 = ORIENTED_EDGE ( 'NONE', *, *, #34277, .F. ) ;
#84810 = CARTESIAN_POINT ( 'NONE',  ( -10.04799450895599122, 7.431456737699883242, 0.000000000000000000 ) ) ;
#84811 = AXIS2_PLACEMENT_3D ( 'NONE', #626, #66468, #34676 ) ;
#84812 = DIRECTION ( 'NONE',  ( -1.000000000000000000, 0.000000000000000000, 0.000000000000000000 ) ) ;
#84813 = EDGE_CURVE ( 'NONE', #40814, #70795, #32855, .T. ) ;
#84814 = STYLED_ITEM ( 'NONE', ( #48936 ), #43474 ) ;
#84815 = VERTEX_POINT ( 'NONE', #43055 ) ;
#84816 = CARTESIAN_POINT ( 'NONE',  ( 34.85314611530805706, 481.9558839989245485, 14.52857051749963091 ) ) ;
#84817 = CARTESIAN_POINT ( 'NONE',  ( -9.312033689600580644, 50.00000000000000000, -94.29807022305314490 ) ) ;
#84818 = MECHANICAL_DESIGN_GEOMETRIC_PRESENTATION_REPRESENTATION (  '', ( #2111 ), #77897 ) ;
#84819 = ORIENTED_EDGE ( 'NONE', *, *, #93623, .F. ) ;
#84820 = ADVANCED_FACE ( 'NONE', ( #41974 ), #26536, .T. ) ;
#84821 = DIRECTION ( 'NONE',  ( 0.000000000000000000, 0.000000000000000000, -1.000000000000000000 ) ) ;
#84822 = CARTESIAN_POINT ( 'NONE',  ( -1.160479916384425936, 11.83769311796837975, -50.01979920269963742 ) ) ;
#84823 = DIRECTION ( 'NONE',  ( 0.000000000000000000, 0.000000000000000000, 1.000000000000000000 ) ) ;
#84824 = DIRECTION ( 'NONE',  ( -0.000000000000000000, 1.000000000000000000, 0.000000000000000000 ) ) ;
#84825 = CARTESIAN_POINT ( 'NONE',  ( -106.0920714368447193, -60.00000000000001421, 198.1769906956861860 ) ) ;
#84826 = DIRECTION ( 'NONE',  ( 0.000000000000000000, -1.000000000000000000, 0.000000000000000000 ) ) ;
#84828 = AXIS2_PLACEMENT_3D ( 'NONE', #94735, #4648, #28971 ) ;
#84827 = CARTESIAN_POINT ( 'NONE',  ( 62.33904886068935980, -4.000000000000000000, 4.898587196589421703E-16 ) ) ;
#84829 =( NAMED_UNIT ( * ) PLANE_ANGLE_UNIT ( ) SI_UNIT ( $, .RADIAN. ) );
#84830 = CARTESIAN_POINT ( 'NONE',  ( 0.000000000000000000, 0.000000000000000000, 0.000000000000000000 ) ) ;
#84831 = CARTESIAN_POINT ( 'NONE',  ( -85.93749938942525546, -24.97245962735015112, 178.1374030527065599 ) ) ;
#84832 = ORIENTED_EDGE ( 'NONE', *, *, #12483, .T. ) ;
#84833 = CARTESIAN_POINT ( 'NONE',  ( -19.18365999306769609, 302.7119710974035343, 9.907277072326611034 ) ) ;
#84834 = EDGE_CURVE ( 'NONE', #74736, #16354, #98611, .T. ) ;
#84835 = DIRECTION ( 'NONE',  ( -1.000000000000000000, -1.224606353822377258E-16, -0.000000000000000000 ) ) ;
#84836 = CARTESIAN_POINT ( 'NONE',  ( -82.65196724022408148, -37.83200599901501704, 4.245451695380549673 ) ) ;
#84837 = DIRECTION ( 'NONE',  ( 0.000000000000000000, -1.000000000000000000, 0.000000000000000000 ) ) ;
#84838 = CARTESIAN_POINT ( 'NONE',  ( -15.89310649718362534, 43.76126840433826004, 6.420194468478833905 ) ) ;
#84839 = CARTESIAN_POINT ( 'NONE',  ( -7.599068113629535937, -12.41377559130418717, 8.423488589708485463 ) ) ;
#84840 = CARTESIAN_POINT ( 'NONE',  ( -14.91271302809441401, 41.98564543112699710, -86.62215342991694911 ) ) ;
#84841 = CARTESIAN_POINT ( 'NONE',  ( -59.23741894013591036, 42.00000000000000711, 7.754160006507077263 ) ) ;
#84842 = CARTESIAN_POINT ( 'NONE',  ( 67.91784306603950938, -14.21045842199442077, 108.3249851056250321 ) ) ;
#84843 = PRESENTATION_STYLE_ASSIGNMENT (( #44935 ) ) ;
#84844 = CARTESIAN_POINT ( 'NONE',  ( -79.45587154498480231, -59.99999999999991473, -31.00068500363164858 ) ) ;
#84845 = CARTESIAN_POINT ( 'NONE',  ( -72.65146387209594536, -46.43774402763246911, 115.6314650919494511 ) ) ;
#84846 = EDGE_LOOP ( 'NONE', ( #21919, #7860, #28126, #13914 ) ) ;
#84847 = CARTESIAN_POINT ( 'NONE',  ( 99.17368802223589341, -30.00000000000007816, 199.4946398670649046 ) ) ;
#84848 = CARTESIAN_POINT ( 'NONE',  ( 23.32150899776524966, 40.83761553963523028, 60.74500979864502881 ) ) ;
#84849 = CARTESIAN_POINT ( 'NONE',  ( 40.27502314868564071, -59.99999999999023714, 56.79790577732133272 ) ) ;
#84850 = ORIENTED_EDGE ( 'NONE', *, *, #83815, .F. ) ;
#84851 = CARTESIAN_POINT ( 'NONE',  ( 10.90053399926999766, -11.19007817188768072, 9.996270789008875113 ) ) ;
#84852 = CARTESIAN_POINT ( 'NONE',  ( -7.188101187500000933, -27.87500000204838457, -2.977408999572651371 ) ) ;
#84853 = PRESENTATION_LAYER_ASSIGNMENT (  '', '', ( #71067 ) ) ;
#84854 = CARTESIAN_POINT ( 'NONE',  ( -4.905018583967756030, -7.976400143203195903, -3.459768807258288170 ) ) ;
#84855 = EDGE_LOOP ( 'NONE', ( #84938, #104633, #71390, #90524 ) ) ;
#84856 = DIRECTION ( 'NONE',  ( 0.000000000000000000, -1.000000000000000000, 0.000000000000000000 ) ) ;
#84857 = VERTEX_POINT ( 'NONE', #102883 ) ;
#84858 = DIRECTION ( 'NONE',  ( 0.8191520442889975717, 1.003171929053531773E-16, -0.5735764363510378328 ) ) ;
#84859 = AXIS2_PLACEMENT_3D ( 'NONE', #906, #92617, #82934 ) ;
#84860 = CYLINDRICAL_SURFACE ( 'NONE', #88534, 7.500000000000000000 ) ;
#84861 = CARTESIAN_POINT ( 'NONE',  ( -44.56219100001479205, -59.99999999999020162, 65.08294012514838300 ) ) ;
#84862 = LINE ( 'NONE', #100502, #20974 ) ;
#84863 = CARTESIAN_POINT ( 'NONE',  ( 4.401442555609581635E-16, -11.28125000204838457, -7.188101187500000044 ) ) ;
#84864 = CARTESIAN_POINT ( 'NONE',  ( -8.000000000000000000, -18.03125000409677270, -3.313708498984762496 ) ) ;
#84865 = AXIS2_PLACEMENT_3D ( 'NONE', #52176, #102330, #19871 ) ;
#84866 = DIRECTION ( 'NONE',  ( 0.000000000000000000, 0.000000000000000000, 1.000000000000000000 ) ) ;
#84867 = CARTESIAN_POINT ( 'NONE',  ( 6.837824896291514243, 3.947820044545422569, -6.564402953523715389 ) ) ;
#84868 = CARTESIAN_POINT ( 'NONE',  ( -12.50000000000000000, -3.000000000000003109, -14.34180675897363599 ) ) ;
#84869 = EDGE_CURVE ( 'NONE', #24875, #8448, #6507, .T. ) ;
#84870 = CARTESIAN_POINT ( 'NONE',  ( -32.85155332502864667, 463.8111683108725174, 7.359358840565846549 ) ) ;
#84871 = ORIENTED_EDGE ( 'NONE', *, *, #74452, .T. ) ;
#84872 = CARTESIAN_POINT ( 'NONE',  ( 4.725902370230581795, -2.526352736915794761, 103.4500010546506559 ) ) ;
#84873 = AXIS2_PLACEMENT_3D ( 'NONE', #101604, #3440, #21251 ) ;
#84875 = CARTESIAN_POINT ( 'NONE',  ( 31.71202031379651842, -18.67338479681879448, 29.92500649697927528 ) ) ;
#84874 = DIRECTION ( 'NONE',  ( 1.000000000000000000, 0.000000000000000000, 0.000000000000000000 ) ) ;
#84876 = CARTESIAN_POINT ( 'NONE',  ( 6.601913983210295100, -4.285714285714226079, 24.56594385547514747 ) ) ;
#84877 = ORIENTED_EDGE ( 'NONE', *, *, #48546, .T. ) ;
#84878 = CARTESIAN_POINT ( 'NONE',  ( -8.737863883542575039, 48.00000000000000000, -90.03618980370900715 ) ) ;
#84879 = ORIENTED_EDGE ( 'NONE', *, *, #55932, .T. ) ;
#84881 = DIRECTION ( 'NONE',  ( 0.000000000000000000, 1.000000000000000000, 0.000000000000000000 ) ) ;
#84880 = CARTESIAN_POINT ( 'NONE',  ( 32.28930913498017929, 488.2717154064768579, 9.213726894932253941 ) ) ;
#84882 = CARTESIAN_POINT ( 'NONE',  ( 0.000000000000000000, 303.8518027762758038, -10.00000000000000355 ) ) ;
#84883 = CARTESIAN_POINT ( 'NONE',  ( 5.656854249492378806, -23.37500000409677270, 5.656854249492381470 ) ) ;
#84884 = CARTESIAN_POINT ( 'NONE',  ( 4.699999999999999289, -3.752776749732553707, 6.499999999999998224 ) ) ;
#84885 = DIRECTION ( 'NONE',  ( -0.8257009859296325915, 0.000000000000000000, -0.5641080409237514415 ) ) ;
#84886 = CARTESIAN_POINT ( 'NONE',  ( -19.70764564238371719, 304.7954121406193622, 9.925013215726785631 ) ) ;
#84887 = VERTEX_POINT ( 'NONE', #43576 ) ;
#84888 = CARTESIAN_POINT ( 'NONE',  ( 92.42023922870691877, -60.00000000000000000, -0.1265986644637803749 ) ) ;
#84889 = FACE_OUTER_BOUND ( 'NONE', #84501, .T. ) ;
#84890 = FILL_AREA_STYLE ('',( #84363 ) ) ;
#84891 = FACE_OUTER_BOUND ( 'NONE', #104908, .T. ) ;
#84892 =( GEOMETRIC_REPRESENTATION_CONTEXT ( 3 ) GLOBAL_UNCERTAINTY_ASSIGNED_CONTEXT ( ( #2785 ) ) GLOBAL_UNIT_ASSIGNED_CONTEXT ( ( #98574, #7429, #75361 ) ) REPRESENTATION_CONTEXT ( 'NONE', 'WORKASPACE' ) );
#84893 = CARTESIAN_POINT ( 'NONE',  ( -6.455412923701131511, 41.05104862138563249, -71.04266226920890404 ) ) ;
#84894 = CARTESIAN_POINT ( 'NONE',  ( -46.79057916015437257, 18.53868985150237236, -15.81409158839457518 ) ) ;
#84895 = ORIENTED_EDGE ( 'NONE', *, *, #89055, .F. ) ;
#84896 = ADVANCED_FACE ( 'NONE', ( #35523 ), #54029, .T. ) ;
#84897 = MECHANICAL_DESIGN_GEOMETRIC_PRESENTATION_REPRESENTATION (  '', ( #90042 ), #79645 ) ;
#84898 = CARTESIAN_POINT ( 'NONE',  ( -108.5592049839054454, -29.99999999999999289, 186.0944184388078781 ) ) ;
#84899 = ORIENTED_EDGE ( 'NONE', *, *, #42627, .T. ) ;
#84900 = VERTEX_POINT ( 'NONE', #68399 ) ;
#84901 = CARTESIAN_POINT ( 'NONE',  ( 7.896165657598944065, 81.21088868628027058, -1.307894402814552937 ) ) ;
#84902 = CYLINDRICAL_SURFACE ( 'NONE', #71807, 5.000000000000001776 ) ;
#84903 = CARTESIAN_POINT ( 'NONE',  ( 0.000000000000000000, 0.000000000000000000, -6.235812796514431433 ) ) ;
#84904 = DIRECTION ( 'NONE',  ( 0.000000000000000000, 0.000000000000000000, 1.000000000000000000 ) ) ;
#84905 = CARTESIAN_POINT ( 'NONE',  ( 85.19561819474900233, -60.19663697381487566, -15.74138277301408451 ) ) ;
#84906 = CIRCLE ( 'NONE', #90046, 4.000000000000007105 ) ;
#84907 = CARTESIAN_POINT ( 'NONE',  ( -39.04768082253571748, 311.1420226168212366, 1.880774019654843254 ) ) ;
#84908 = DIRECTION ( 'NONE',  ( -1.000000000000000000, -1.224606353822377258E-16, -0.000000000000000000 ) ) ;
#84909 = CARTESIAN_POINT ( 'NONE',  ( 30.59999999999999787, -3.309499999999999886, 4.475777889183790779E-16 ) ) ;
#84910 = VERTEX_POINT ( 'NONE', #78068 ) ;
#84912 = EDGE_CURVE ( 'NONE', #72931, #2343, #5772, .T. ) ;
#84911 = CARTESIAN_POINT ( 'NONE',  ( -6.838249472399976270, -3.995156693690935956, -6.573189567101946018 ) ) ;
#84913 = ORIENTED_EDGE ( 'NONE', *, *, #19619, .F. ) ;
#84914 = CARTESIAN_POINT ( 'NONE',  ( 49.27910061723706292, 7.914421806211205279, -15.56686240200417259 ) ) ;
#84915 = DIRECTION ( 'NONE',  ( -1.000000000000000000, -1.224606353822377258E-16, -0.000000000000000000 ) ) ;
#84917 = ORIENTED_EDGE ( 'NONE', *, *, #51750, .T. ) ;
#84916 = DIRECTION ( 'NONE',  ( 0.000000000000000000, 0.000000000000000000, 1.000000000000000000 ) ) ;
#84918 = CARTESIAN_POINT ( 'NONE',  ( 75.11061747473844719, -39.49004629203866301, 121.1523287295283779 ) ) ;
#84919 = ORIENTED_EDGE ( 'NONE', *, *, #85517, .F. ) ;
#84920 = EDGE_CURVE ( 'NONE', #74067, #81365, #77004, .T. ) ;
#84921 = CARTESIAN_POINT ( 'NONE',  ( 1.625799246043344359, -50.01537087125233683, 40.95671946476290515 ) ) ;
#84922 = CARTESIAN_POINT ( 'NONE',  ( 104.9555555555555486, 1.023464760207051730E-14, 0.000000000000000000 ) ) ;
#84923 = CARTESIAN_POINT ( 'NONE',  ( 2.977408999572650927, -24.87500000204838813, -7.188101187500000933 ) ) ;
#84924 = CARTESIAN_POINT ( 'NONE',  ( -72.68483858684419374, -57.66063987133676960, 178.6659478268091163 ) ) ;
#84925 = ORIENTED_EDGE ( 'NONE', *, *, #93629, .T. ) ;
#84926 = B_SPLINE_CURVE_WITH_KNOTS ( 'NONE', 3,
 ( #83229, #27700, #44375, #76723, #68107, #101005, #20144, #52445, #85363, #3383, #27163, #2834, #11452, #67062, #60055, #28225, #75663, #10391 ),
 .UNSPECIFIED., .F., .F.,
 ( 4, 2, 2, 2, 2, 2, 2, 2, 4 ),
 ( 0.002862744142489912630, 0.003367451191158993620, 0.003619804715493535850, 0.003872158239828078080, 0.004376865288497162540, 0.004881572337166247000, 0.005890986434504425460, 0.006395693483173519461, 0.006900400531842612595 ),
 .UNSPECIFIED. ) ;
#84927 = CARTESIAN_POINT ( 'NONE',  ( -29.08775742405871867, 43.32034978114150903, -70.51094494232118848 ) ) ;
#84928 = CARTESIAN_POINT ( 'NONE',  ( 101.6546115610671563, -37.84847036870517911, 185.8343739213452466 ) ) ;
#84929 = CARTESIAN_POINT ( 'NONE',  ( -32.84951609414347473, 478.7804999730025202, 7.701738758140129093 ) ) ;
#84930 = CARTESIAN_POINT ( 'NONE',  ( 41.36650669486618881, -3.999999999999998224, 0.000000000000000000 ) ) ;
#84931 = CARTESIAN_POINT ( 'NONE',  ( 7.999999999999998224, -20.28125000409677625, 3.313708498984766493 ) ) ;
#84932 = CARTESIAN_POINT ( 'NONE',  ( 16.36650669486618881, 0.000000000000000000, 4.000000000000000888 ) ) ;
#84933 = CARTESIAN_POINT ( 'NONE',  ( 9.381593208289393360, 247.9856136188048765, -3.465401811657803144 ) ) ;
#84934 = CIRCLE ( 'NONE', #52191, 5.000000000000000888 ) ;
#84935 = CARTESIAN_POINT ( 'NONE',  ( 0.000000000000000000, 34.08768991669519721, 0.000000000000000000 ) ) ;
#84936 = DIRECTION ( 'NONE',  ( 1.000000000000000000, 0.000000000000000000, 0.000000000000000000 ) ) ;
#84937 = CARTESIAN_POINT ( 'NONE',  ( 32.85155332502866798, 463.8111683108725174, 7.359358840565819904 ) ) ;
#84938 = ORIENTED_EDGE ( 'NONE', *, *, #88910, .T. ) ;
#84939 = CARTESIAN_POINT ( 'NONE',  ( 43.61214829175436591, 434.3223057887385608, 14.49707129802061800 ) ) ;
#84940 = CARTESIAN_POINT ( 'NONE',  ( 12.22950890273489755, -4.580576956131391597, -12.66933385000445611 ) ) ;
#84941 = CIRCLE ( 'NONE', #34995, 5.000000000000002665 ) ;
#84942 = CARTESIAN_POINT ( 'NONE',  ( -7.500000000000003553, -3.000000000000000888, -36.97043916959992771 ) ) ;
#84943 = CARTESIAN_POINT ( 'NONE',  ( -86.32322474925454969, -30.00000000000000711, 180.5646619429487316 ) ) ;
#84944 = EDGE_CURVE ( 'NONE', #66879, #73917, #37120, .T. ) ;
#84945 = EDGE_LOOP ( 'NONE', ( #35769, #101221, #50391, #73963 ) ) ;
#84946 = CARTESIAN_POINT ( 'NONE',  ( -17.11334244688239536, -4.333298119783949964, -5.314533759433560434 ) ) ;
#84947 = AXIS2_PLACEMENT_3D ( 'NONE', #89422, #105585, #57549 ) ;
#84948 = CARTESIAN_POINT ( 'NONE',  ( 83.05975511330255756, -57.53496370214478617, 201.2049058628653597 ) ) ;
#84950 = CARTESIAN_POINT ( 'NONE',  ( 80.00000000000000000, -52.00000000000000000, -23.09707704303352926 ) ) ;
#84949 = CARTESIAN_POINT ( 'NONE',  ( 32.04230769230768772, -4.171999999999999709, 5.616230220889763424E-16 ) ) ;
#84951 = ADVANCED_FACE ( 'NONE', ( #101811 ), #27975, .T. ) ;
#84952 = ADVANCED_FACE ( 'NONE', ( #14372 ), #7531, .T. ) ;
#84953 = CARTESIAN_POINT ( 'NONE',  ( 28.54446013220072942, -29.03608049721292517, -38.24221999424131013 ) ) ;
#84954 =( NAMED_UNIT ( * ) PLANE_ANGLE_UNIT ( ) SI_UNIT ( $, .RADIAN. ) );
#84955 = CARTESIAN_POINT ( 'NONE',  ( -29.92793289100823984, -60.00000000000000711, 42.99008754467271842 ) ) ;
#84956 = CARTESIAN_POINT ( 'NONE',  ( -50.94745919686192082, 50.00000000000000000, -37.05882352941185331 ) ) ;
#84957 = SURFACE_SIDE_STYLE ('',( #18660 ) ) ;
#84958 = CARTESIAN_POINT ( 'NONE',  ( -86.49309358683535720, -20.77578434039007149, 183.3212683181210707 ) ) ;
#84960 = EDGE_LOOP ( 'NONE', ( #11267, #42977, #62502, #36174 ) ) ;
#84959 = AXIS2_PLACEMENT_3D ( 'NONE', #34415, #60279, #17142 ) ;
#84961 = CARTESIAN_POINT ( 'NONE',  ( 30.25727950662361820, 17.21737621059157064, 39.73669541984489229 ) ) ;
#84962 = CARTESIAN_POINT ( 'NONE',  ( -4.998953709602685258, -25.54932396112263859, 28.13843181039721131 ) ) ;
#84963 = FILL_AREA_STYLE_COLOUR ( '', #106571 ) ;
#84964 = CARTESIAN_POINT ( 'NONE',  ( 8.000000000000000000, 0.000000000000000000, -13.00000000000000000 ) ) ;
#84965 = AXIS2_PLACEMENT_3D ( 'NONE', #72972, #15816, #10241 ) ;
#84966 = CARTESIAN_POINT ( 'NONE',  ( -42.69336147150778515, 372.1122575306994236, 17.99588274971726420 ) ) ;
#84967 = ORIENTED_EDGE ( 'NONE', *, *, #29080, .T. ) ;
#84968 = EDGE_CURVE ( 'NONE', #57077, #106280, #105005, .T. ) ;
#84969 =( GEOMETRIC_REPRESENTATION_CONTEXT ( 3 ) GLOBAL_UNCERTAINTY_ASSIGNED_CONTEXT ( ( #65576 ) ) GLOBAL_UNIT_ASSIGNED_CONTEXT ( ( #85460, #13672, #44469 ) ) REPRESENTATION_CONTEXT ( 'NONE', 'WORKASPACE' ) );
#84970 = CARTESIAN_POINT ( 'NONE',  ( -3.313708498984746065, -29.46874999999999645, 8.000000000000017764 ) ) ;
#84971 = DIRECTION ( 'NONE',  ( -0.5735764363510494901, -0.8191520442889894671, 0.000000000000000000 ) ) ;
#84972 = CARTESIAN_POINT ( 'NONE',  ( -30.90685644053160885, 9.526079354490862627, -40.57200395206852050 ) ) ;
#84973 = AXIS2_PLACEMENT_3D ( 'NONE', #84107, #26444, #36136 ) ;
#84974 = CARTESIAN_POINT ( 'NONE',  ( 23.94432778666880068, 303.5797213061153457, -9.843316957413865254 ) ) ;
#84975 = CARTESIAN_POINT ( 'NONE',  ( 45.17824257314219949, 354.4244853104167987, 3.762393652172960845 ) ) ;
#84976 = EDGE_CURVE ( 'NONE', #10091, #35053, #67835, .T. ) ;
#84977 = SURFACE_SIDE_STYLE ('',( #59646 ) ) ;
#84978 = CARTESIAN_POINT ( 'NONE',  ( 9.627423004282553265, 53.53986113459780682, -2.126428460392088216 ) ) ;
#84979 = CARTESIAN_POINT ( 'NONE',  ( 97.09801539114592117, -30.00000000000000711, 79.69841507686976456 ) ) ;
#84980 = CARTESIAN_POINT ( 'NONE',  ( -78.28590395464601670, -60.31583579356012592, 158.4450162056950262 ) ) ;
#84981 = ORIENTED_EDGE ( 'NONE', *, *, #95077, .F. ) ;
#84982 = CARTESIAN_POINT ( 'NONE',  ( 85.31310517497098544, 1.030564683017419500E-14, 0.000000000000000000 ) ) ;
#84983 = DIRECTION ( 'NONE',  ( 0.000000000000000000, 0.000000000000000000, -1.000000000000000000 ) ) ;
#84984 = CARTESIAN_POINT ( 'NONE',  ( 30.05171975993012623, -57.68438312713176686, 45.30126411961221322 ) ) ;
#84985 = CARTESIAN_POINT ( 'NONE',  ( 18.00000000000000355, 12.99999999999999289, 0.000000000000000000 ) ) ;
#84986 = CARTESIAN_POINT ( 'NONE',  ( 41.00553391478180032, 320.1856813797184600, 4.158943489448629904 ) ) ;
#84987 = FACE_OUTER_BOUND ( 'NONE', #89746, .T. ) ;
#84988 = ORIENTED_EDGE ( 'NONE', *, *, #90808, .F. ) ;
#84989 = CARTESIAN_POINT ( 'NONE',  ( 4.957729184102722009, 53.54793516222699878, -8.497043709396882250 ) ) ;
#84990 = CARTESIAN_POINT ( 'NONE',  ( 55.74444444444444713, -3.309500000000000774, 4.475777889183797681E-16 ) ) ;
#84991 = CARTESIAN_POINT ( 'NONE',  ( 7.188101187499999156, -31.25000000204838813, 2.977408999572654924 ) ) ;
#84992 = VERTEX_POINT ( 'NONE', #22525 ) ;
#84993 = FACE_OUTER_BOUND ( 'NONE', #97974, .T. ) ;
#84994 = CARTESIAN_POINT ( 'NONE',  ( 3.409011323177081998, 15.24615751665884922, 9.403185743875308589 ) ) ;
#84995 = CARTESIAN_POINT ( 'NONE',  ( 4.966176485634620441, 41.64999999999997726, -70.47555195150160046 ) ) ;
#84996 = CARTESIAN_POINT ( 'NONE',  ( 58.76133767613618630, 50.00000000000000000, 23.44026136864407306 ) ) ;
#84997 = CARTESIAN_POINT ( 'NONE',  ( 1.678729582439481227, -5.952306540456972606, -13.77787289860723696 ) ) ;
#84998 = DIRECTION ( 'NONE',  ( -0.000000000000000000, 1.000000000000000000, -0.000000000000000000 ) ) ;
#84999 = ORIENTED_EDGE ( 'NONE', *, *, #28229, .F. ) ;
#85000 = CARTESIAN_POINT ( 'NONE',  ( 0.7145311798163271888, -9.237604307034018802, 8.246630900752838649E-17 ) ) ;
#85002 = CARTESIAN_POINT ( 'NONE',  ( 20.16305471169097174, -39.47376339469866480, 30.99867996556357141 ) ) ;
#85001 = CARTESIAN_POINT ( 'NONE',  ( -78.54456454054628978, -14.21045842199430709, 165.9065210845421348 ) ) ;
#85003 = CARTESIAN_POINT ( 'NONE',  ( 1.202368250414458695E-14, 27.55047179872464724, -49.09040922050319011 ) ) ;
#85004 = ADVANCED_FACE ( 'NONE', ( #79125 ), #5849, .T. ) ;
#85005 = CARTESIAN_POINT ( 'NONE',  ( -38.66081106768926645, -29.14070258423828719, 35.42311757073793643 ) ) ;
#85006 = UNCERTAINTY_MEASURE_WITH_UNIT (LENGTH_MEASURE( 1.000000000000000082E-05 ), #82207, 'distance_accuracy_value', 'NONE');
#85007 = ORIENTED_EDGE ( 'NONE', *, *, #9184, .F. ) ;
#85008 = DIRECTION ( 'NONE',  ( -1.000000000000000000, -1.224606353822377258E-16, -0.000000000000000000 ) ) ;
#85009 = CARTESIAN_POINT ( 'NONE',  ( -2.499999999999996003, -8.000000000000000000, -4.679304766526493044E-16 ) ) ;
#85010 = CARTESIAN_POINT ( 'NONE',  ( -13.83891950279925354, -57.46707097098471451, 29.12888379965242081 ) ) ;
#85011 = CARTESIAN_POINT ( 'NONE',  ( 0.000000000000000000, 0.000000000000000000, 1.734723475976807094E-15 ) ) ;
#85012 = CARTESIAN_POINT ( 'NONE',  ( 7.934883677559680493, -61.13160822062448574, 1.051380792122691421 ) ) ;
#85013 = CARTESIAN_POINT ( 'NONE',  ( 12.41665141885566470, -3.617041646665052568, 20.56186768168683088 ) ) ;
#85014 = ORIENTED_EDGE ( 'NONE', *, *, #31479, .F. ) ;
#85015 = CARTESIAN_POINT ( 'NONE',  ( -15.99452815637125447, 36.61440916976220450, -24.05462502184712648 ) ) ;
#85016 = ORIENTED_EDGE ( 'NONE', *, *, #46986, .F. ) ;
#85017 = CARTESIAN_POINT ( 'NONE',  ( 94.81216642829221541, -30.00000000000000000, 191.3357916152312725 ) ) ;
#85018 = CARTESIAN_POINT ( 'NONE',  ( -13.70721846773710695, 3.095425950693140749, -6.047708547295085779 ) ) ;
#85019 = PRESENTATION_LAYER_ASSIGNMENT (  '', '', ( #24743 ) ) ;
#85020 = UNCERTAINTY_MEASURE_WITH_UNIT (LENGTH_MEASURE( 1.000000000000000082E-05 ), #62566, 'distance_accuracy_value', 'NONE');
#85021 = CARTESIAN_POINT ( 'NONE',  ( -4.472135954999577834, -84.72670096487358649, -4.000000000000002665 ) ) ;
#85022 = CARTESIAN_POINT ( 'NONE',  ( 82.04623972355572903, -30.00000000000000000, 34.40552157734605032 ) ) ;
#85023 = AXIS2_PLACEMENT_3D ( 'NONE', #89880, #7880, #40787 ) ;
#85024 = CARTESIAN_POINT ( 'NONE',  ( 4.678819457397440651, 8.078722181090837395, 0.000000000000000000 ) ) ;
#85025 = VERTEX_POINT ( 'NONE', #88297 ) ;
#85026 = EDGE_CURVE ( 'NONE', #40074, #28791, #15448, .T. ) ;
#85027 = ORIENTED_EDGE ( 'NONE', *, *, #90517, .T. ) ;
#85028 = ORIENTED_EDGE ( 'NONE', *, *, #38768, .F. ) ;
#85029 = CARTESIAN_POINT ( 'NONE',  ( -32.77384846114340888, 465.0024891621177403, 11.55799621384033671 ) ) ;
#85030 = FACE_OUTER_BOUND ( 'NONE', #63012, .T. ) ;
#85031 = AXIS2_PLACEMENT_3D ( 'NONE', #102683, #95137, #94613 ) ;
#85032 = CARTESIAN_POINT ( 'NONE',  ( 1.530808498934191324E-16, -1.200000000000000030E-05, 7.749999999999999112 ) ) ;
#85033 = CARTESIAN_POINT ( 'NONE',  ( 38.67540923711027290, 439.2245545847551398, 23.63822418690137539 ) ) ;
#85034 = CARTESIAN_POINT ( 'NONE',  ( -31.01628821198604768, 439.2628560410439604, 22.57312827278326495 ) ) ;
#85035 = CARTESIAN_POINT ( 'NONE',  ( -7.986539162393897939, -88.97327171057455075, -0.5321833565149911571 ) ) ;
#85036 = EDGE_CURVE ( 'NONE', #98784, #53610, #96707, .T. ) ;
#85037 = CARTESIAN_POINT ( 'NONE',  ( 19.00000000000000711, 5.000000000000000888, 25.00000000000000000 ) ) ;
#85038 = ORIENTED_EDGE ( 'NONE', *, *, #29149, .T. ) ;
#85040 = ADVANCED_FACE ( 'NONE', ( #46762 ), #38689, .F. ) ;
#85039 = CARTESIAN_POINT ( 'NONE',  ( 1.570796324976846403, 50.00000000000000000, -73.00000000000001421 ) ) ;
#85041 = ORIENTED_EDGE ( 'NONE', *, *, #19266, .T. ) ;
#85042 = CARTESIAN_POINT ( 'NONE',  ( 73.58237775803615932, -38.32580639661416200, 156.7707483651560949 ) ) ;
#85043 = CARTESIAN_POINT ( 'NONE',  ( 7.086921372259695358E-15, 43.00000000000000000, -57.86910460382442523 ) ) ;
#85044 = CARTESIAN_POINT ( 'NONE',  ( 24.47931459791210429, 295.5124831337354863, 2.078786121475366677 ) ) ;
#85045 = ADVANCED_FACE ( 'NONE', ( #13316 ), #45535, .T. ) ;
#85046 = DIRECTION ( 'NONE',  ( -1.000000000000000000, 0.000000000000000000, 0.000000000000000000 ) ) ;
#85047 = AXIS2_PLACEMENT_3D ( 'NONE', #7562, #73357, #24332 ) ;
#85048 = ORIENTED_EDGE ( 'NONE', *, *, #93560, .F. ) ;
#85049 = EDGE_CURVE ( 'NONE', #95748, #18245, #95475, .T. ) ;
#85050 = CARTESIAN_POINT ( 'NONE',  ( 29.50913623581959300, 8.560131685753185948, -42.09559527950068514 ) ) ;
#85051 = CARTESIAN_POINT ( 'NONE',  ( 9.035703905990985163, -10.37169118567828185, -12.88508357975250185 ) ) ;
#85052 = CARTESIAN_POINT ( 'NONE',  ( -2.100000000000004530, 0.000000000000000000, 0.000000000000000000 ) ) ;
#85053 =( GEOMETRIC_REPRESENTATION_CONTEXT ( 3 ) GLOBAL_UNCERTAINTY_ASSIGNED_CONTEXT ( ( #84779 ) ) GLOBAL_UNIT_ASSIGNED_CONTEXT ( ( #24041, #56882, #24569 ) ) REPRESENTATION_CONTEXT ( 'NONE', 'WORKASPACE' ) );
#85054 = DIRECTION ( 'NONE',  ( 0.000000000000000000, 0.000000000000000000, -1.000000000000000000 ) ) ;
#85056 = ORIENTED_EDGE ( 'NONE', *, *, #19724, .T. ) ;
#85055 = COLOUR_RGB ( '', 0.72549020, 0.75294118, 0.79215686) ;
#85058 = CARTESIAN_POINT ( 'NONE',  ( 30.00000000000000000, 461.8887775513396150, 11.55279652844105698 ) ) ;
#85057 = FILL_AREA_STYLE ('',( #83444 ) ) ;
#85059 = CARTESIAN_POINT ( 'NONE',  ( -4.999999999999993783, -3.723962137281044971, 102.2532056551910529 ) ) ;
#85060 = DIRECTION ( 'NONE',  ( 1.000000000000000000, 0.000000000000000000, -0.000000000000000000 ) ) ;
#85061 = CARTESIAN_POINT ( 'NONE',  ( 42.64966854229459869, 465.0854819100619011, 13.23715615004964086 ) ) ;
#85062 = DIRECTION ( 'NONE',  ( -1.000000000000000000, -1.224606353822377258E-16, -0.000000000000000000 ) ) ;
#85063 = DIRECTION ( 'NONE',  ( 0.000000000000000000, -1.000000000000000000, -0.000000000000000000 ) ) ;
#85064 = CARTESIAN_POINT ( 'NONE',  ( 11.84999999999999787, 3.309500000000003439, 0.000000000000000000 ) ) ;
#85065 = CARTESIAN_POINT ( 'NONE',  ( 84.61252253634089016, -61.08059672144357677, 193.0962152012025683 ) ) ;
#85066 = CARTESIAN_POINT ( 'NONE',  ( 16.75187969033441604, 36.38380281757147827, -24.30698433969211791 ) ) ;
#85067 = CARTESIAN_POINT ( 'NONE',  ( -8.568812041277357849, 127.6722392238329462, 0.000000000000000000 ) ) ;
#85068 = EDGE_LOOP ( 'NONE', ( #74250, #4056 ) ) ;
#85069 = DIRECTION ( 'NONE',  ( 1.000000000000000000, -0.000000000000000000, -0.000000000000000000 ) ) ;
#85070 = CARTESIAN_POINT ( 'NONE',  ( 30.59999999999999787, 1.533819458162526451E-15, 0.000000000000000000 ) ) ;
#85071 = DIRECTION ( 'NONE',  ( 1.000000000000000000, -0.000000000000000000, -0.000000000000000000 ) ) ;
#85072 = CARTESIAN_POINT ( 'NONE',  ( 3.313708498984800688, -18.78124999999998934, 7.999999999999960032 ) ) ;
#85073 = CARTESIAN_POINT ( 'NONE',  ( -86.16358238103411793, -30.00000000000000000, 65.24097969989436763 ) ) ;
#85074 = AXIS2_PLACEMENT_3D ( 'NONE', #4339, #40284, #73160 ) ;
#85075 = CARTESIAN_POINT ( 'NONE',  ( -29.68315524076956535, 13.47185074185901499, 42.10535821593508388 ) ) ;
#85076 = CARTESIAN_POINT ( 'NONE',  ( 33.19742037143350188, -57.69209351129511987, 47.48252466582053444 ) ) ;
#85078 = CARTESIAN_POINT ( 'NONE',  ( 0.000000000000000000, 29.56666008184760130, 0.000000000000000000 ) ) ;
#85077 = CARTESIAN_POINT ( 'NONE',  ( -9.948561005166148163, 246.1300972625179782, -1.045755304005127062 ) ) ;
#85079 = EDGE_CURVE ( 'NONE', #44667, #33604, #31307, .T. ) ;
#85080 = CARTESIAN_POINT ( 'NONE',  ( -48.44486512746869522, 38.95340677903534754, -41.63464568442791602 ) ) ;
#85081 = CARTESIAN_POINT ( 'NONE',  ( -18.51494887344581741, -24.53949113939198412, 28.33608110197982555 ) ) ;
#85082 = LINE ( 'NONE', #19864, #60156 ) ;
#85083 = CARTESIAN_POINT ( 'NONE',  ( -42.72730916064396212, 485.8496625310939976, 7.279181987618908778 ) ) ;
#85084 = CARTESIAN_POINT ( 'NONE',  ( 44.49616249768619269, 470.0858613617913306, 4.037852223137175400 ) ) ;
#85085 = CONICAL_SURFACE ( 'NONE', #78145, 5.000000000000001776, 0.9599310885968803664 ) ;
#85086 = CARTESIAN_POINT ( 'NONE',  ( 39.41494875793583930, -24.69103780450011598, -30.41528609289981944 ) ) ;
#85087 = COLOUR_RGB ( '', 0.31764706, 0.68627451, 0.89019608) ;
#85088 = CARTESIAN_POINT ( 'NONE',  ( -24.52207515261177662, -29.04217159202778831, 29.86984086181256970 ) ) ;
#85089 = ORIENTED_EDGE ( 'NONE', *, *, #3865, .F. ) ;
#85090 = CARTESIAN_POINT ( 'NONE',  ( 5.744562646538029504, 12.99999999999999112, -4.000000000000000000 ) ) ;
#85091 = CARTESIAN_POINT ( 'NONE',  ( -16.44160279200490749, -22.06944590909828818, 27.77945804026875010 ) ) ;
#85092 = CARTESIAN_POINT ( 'NONE',  ( 39.29343254467229940, 485.1983557762937949, -4.348408391708091791 ) ) ;
#85093 = ORIENTED_EDGE ( 'NONE', *, *, #48383, .F. ) ;
#85094 = CARTESIAN_POINT ( 'NONE',  ( -36.60690515392210642, 437.5575915073889632, 4.269387481551378372 ) ) ;
#85095 = VERTEX_POINT ( 'NONE', #10021 ) ;
#85096 = CARTESIAN_POINT ( 'NONE',  ( 0.000000000000000000, 0.000000000000000000, 4.000000000000000000 ) ) ;
#85097 = EDGE_CURVE ( 'NONE', #49781, #22579, #74747, .T. ) ;
#85098 = CARTESIAN_POINT ( 'NONE',  ( 22.61650669486618526, 4.000000000000003553, 4.898587196589414801E-16 ) ) ;
#85099 = VERTEX_POINT ( 'NONE', #16517 ) ;
#85100 = CARTESIAN_POINT ( 'NONE',  ( 0.000000000000000000, 0.000000000000000000, 0.000000000000000000 ) ) ;
#85101 = CARTESIAN_POINT ( 'NONE',  ( 10.47796581435196472, 50.00000000000001421, -78.93819186518393849 ) ) ;
#85102 = CARTESIAN_POINT ( 'NONE',  ( 103.9186714964248637, -60.15547946887917874, 191.0484277881152195 ) ) ;
#85104 = CARTESIAN_POINT ( 'NONE',  ( 56.48317336153285595, 6.856755485862130937E-15, 0.000000000000000000 ) ) ;
#85103 = CARTESIAN_POINT ( 'NONE',  ( 7.904834542844216827, 294.7031450397155368, -6.150931456888534044 ) ) ;
#85105 = ADVANCED_FACE ( 'NONE', ( #41323 ), #92002, .F. ) ;
#85106 = VERTEX_POINT ( 'NONE', #32736 ) ;
#85107 = AXIS2_PLACEMENT_3D ( 'NONE', #101777, #36030, #68363 ) ;
#85108 = ORIENTED_EDGE ( 'NONE', *, *, #37199, .T. ) ;
#85109 = ORIENTED_EDGE ( 'NONE', *, *, #56945, .F. ) ;
#85110 = CARTESIAN_POINT ( 'NONE',  ( 23.64531383863861436, 306.0645085318336100, 10.20398222576348957 ) ) ;
#85111 = CIRCLE ( 'NONE', #38639, 3.400000000000000355 ) ;
#85112 = CARTESIAN_POINT ( 'NONE',  ( -5.000000000000000000, -15.62228920881132765, 12.61250543006183911 ) ) ;
#85113 = DIRECTION ( 'NONE',  ( 0.000000000000000000, -0.7633528697427716114, -0.6459817305895541040 ) ) ;
#85114 = ORIENTED_EDGE ( 'NONE', *, *, #73491, .T. ) ;
#85115 = MECHANICAL_DESIGN_GEOMETRIC_PRESENTATION_REPRESENTATION (  '', ( #73001 ), #12740 ) ;
#85116 = CARTESIAN_POINT ( 'NONE',  ( 45.36923076923077502, 1.411358822780289120E-15, 0.000000000000000000 ) ) ;
#85117 = CARTESIAN_POINT ( 'NONE',  ( -6.921856738059537051, 41.59435685020018525, -70.13580383255585105 ) ) ;
#85118 =( GEOMETRIC_REPRESENTATION_CONTEXT ( 3 ) GLOBAL_UNCERTAINTY_ASSIGNED_CONTEXT ( ( #10308 ) ) GLOBAL_UNIT_ASSIGNED_CONTEXT ( ( #12986, #103608, #63162 ) ) REPRESENTATION_CONTEXT ( 'NONE', 'WORKASPACE' ) );
#85119 = CARTESIAN_POINT ( 'NONE',  ( 7.500000000000007105, 39.99999999999998579, -68.91429205785453860 ) ) ;
#85120 = CARTESIAN_POINT ( 'NONE',  ( -95.13513732309382931, -60.00000000000000000, -7.455916306700166807 ) ) ;
#85121 = DIRECTION ( 'NONE',  ( 0.000000000000000000, -1.000000000000000000, 0.000000000000000000 ) ) ;
#85122 = CARTESIAN_POINT ( 'NONE',  ( -30.12932728364529922, 334.4140447340107585, 17.11298374841474867 ) ) ;
#85123 = CARTESIAN_POINT ( 'NONE',  ( -6.578491659837745864, 41.30621945901641112, -58.38226164895504411 ) ) ;
#85124 = CARTESIAN_POINT ( 'NONE',  ( -88.18129031808710749, -59.99999999999997158, -24.85705915495453411 ) ) ;
#85125 = CARTESIAN_POINT ( 'NONE',  ( 72.50181414422412729, -37.99999999999997868, -21.26202816386757277 ) ) ;
#85126 = CARTESIAN_POINT ( 'NONE',  ( -48.25703249655036586, -49.90483171777201932, 51.25166225055939151 ) ) ;
#85127 = EDGE_LOOP ( 'NONE', ( #54206, #2167, #30059, #54329 ) ) ;
#85128 = LINE ( 'NONE', #35551, #16016 ) ;
#85129 = ORIENTED_EDGE ( 'NONE', *, *, #41488, .F. ) ;
#85130 = DIRECTION ( 'NONE',  ( 1.000000000000000000, 1.224606353822377258E-16, 0.000000000000000000 ) ) ;
#85131 = CARTESIAN_POINT ( 'NONE',  ( -9.218636978381848479, 294.6649786875596533, -3.878494680342783774 ) ) ;
#85132 = CARTESIAN_POINT ( 'NONE',  ( 5.382057749264598456, -7.001732015960572042, -2.659775980967105991 ) ) ;
#85133 = ORIENTED_EDGE ( 'NONE', *, *, #36116, .F. ) ;
#85134 = CARTESIAN_POINT ( 'NONE',  ( 5.999787407977320797, 246.0003188881554763, 0.2740427891042969688 ) ) ;
#85135 = CARTESIAN_POINT ( 'NONE',  ( 88.86616235159861787, -30.00000000000552802, -15.15331224089027806 ) ) ;
#85136 = CARTESIAN_POINT ( 'NONE',  ( 49.28001195564470294, 13.04047724765487537, 15.62422648183673957 ) ) ;
#85137 = CARTESIAN_POINT ( 'NONE',  ( 3.349796915291911148, -48.86785030187898826, 104.5044954676193214 ) ) ;
#85138 = CARTESIAN_POINT ( 'NONE',  ( 6.771436162406291537, 41.75941402238878197, -59.18670940897492727 ) ) ;
#85139 = CARTESIAN_POINT ( 'NONE',  ( 37.36680950585426331, 18.64316884707256605, -10.04205104291870398 ) ) ;
#85140 = CARTESIAN_POINT ( 'NONE',  ( 85.96440179497020040, -30.00000000000000000, 178.3523970025662493 ) ) ;
#85141 = CARTESIAN_POINT ( 'NONE',  ( 0.000000000000000000, 0.000000000000000000, 4.000000000000000888 ) ) ;
#85142 = CARTESIAN_POINT ( 'NONE',  ( -1.011281213726471728, 37.02243808088083199, 27.74757158266077539 ) ) ;
#85143 = EDGE_CURVE ( 'NONE', #87161, #32332, #67737, .T. ) ;
#85144 = VERTEX_POINT ( 'NONE', #73682 ) ;
#85145 = ORIENTED_EDGE ( 'NONE', *, *, #131, .T. ) ;
#85146 = CARTESIAN_POINT ( 'NONE',  ( 55.56247616277558876, -22.15090731089991039, 54.53775895343569147 ) ) ;
#85147 = CARTESIAN_POINT ( 'NONE',  ( 6.736687879933906942, 41.36687664139658693, -58.48851407026759830 ) ) ;
#85148 = CARTESIAN_POINT ( 'NONE',  ( -7.500000000000008882, 42.00000000000000711, -72.67206406577980715 ) ) ;
#85149 = EDGE_CURVE ( 'NONE', #78613, #9645, #61005, .T. ) ;
#85150 = ORIENTED_EDGE ( 'NONE', *, *, #28397, .F. ) ;
#85152 = ADVANCED_FACE ( 'NONE', ( #99009 ), #58587, .F. ) ;
#85151 = CARTESIAN_POINT ( 'NONE',  ( -85.10638907240416984, -38.35927573440125116, -22.75109318859258067 ) ) ;
#85153 = ORIENTED_EDGE ( 'NONE', *, *, #60456, .T. ) ;
#85154 =( NAMED_UNIT ( * ) SI_UNIT ( $, .STERADIAN. ) SOLID_ANGLE_UNIT ( ) );
#85155 = CARTESIAN_POINT ( 'NONE',  ( 110.2617929913287185, -38.35601522437976740, 184.2502704656793640 ) ) ;
#85156 = CARTESIAN_POINT ( 'NONE',  ( 14.42243728958148807, 21.45411286276491936, 5.348240395882925213 ) ) ;
#85157 = CIRCLE ( 'NONE', #61069, 12.00000000000001066 ) ;
#85158 = CARTESIAN_POINT ( 'NONE',  ( 86.34280695398143735, -60.13066267512422058, 4.659422765642229791 ) ) ;
#85159 = CARTESIAN_POINT ( 'NONE',  ( -1.013051998863770953, 45.47574100367069150, -18.25019877145031799 ) ) ;
#85160 = CARTESIAN_POINT ( 'NONE',  ( -26.60412269428898924, 307.1936361343147155, -9.480968390364807874 ) ) ;
#85161 = CIRCLE ( 'NONE', #38669, 4.000000000000000888 ) ;
#85162 = CARTESIAN_POINT ( 'NONE',  ( 4.962899348968470292, -12.37352932398349381, -8.506080509221449759 ) ) ;
#85163 = CARTESIAN_POINT ( 'NONE',  ( -23.62769831312177971, 25.18629417231644396, -33.13992749466611798 ) ) ;
#85164 =( GEOMETRIC_REPRESENTATION_CONTEXT ( 3 ) GLOBAL_UNCERTAINTY_ASSIGNED_CONTEXT ( ( #42270 ) ) GLOBAL_UNIT_ASSIGNED_CONTEXT ( ( #5767, #6824, #21984 ) ) REPRESENTATION_CONTEXT ( 'NONE', 'WORKASPACE' ) );
#85165 = ADVANCED_FACE ( 'NONE', ( #75276 ), #93334, .T. ) ;
#85166 = DIRECTION ( 'NONE',  ( 0.5735764363510470476, -0.8191520442889911324, 1.003171929053524007E-16 ) ) ;
#85167 = CARTESIAN_POINT ( 'NONE',  ( 7.849086896557445847, 70.34805173277894141, 0.000000000000000000 ) ) ;
#85169 = ORIENTED_EDGE ( 'NONE', *, *, #20511, .T. ) ;
#85168 =( BOUNDED_SURFACE ( )  B_SPLINE_SURFACE ( 3, 2, ( 
 ( #11560, #103771, #37489 ),
 ( #20257, #36434, #45029 ),
 ( #62796, #4023, #103249 ),
 ( #13686, #70352, #12620 ),
 ( #77378, #95685, #52556 ),
 ( #87604, #45557, #4550 ),
 ( #54667, #95166, #44491 ),
 ( #29394, #36950, #78427 ),
 ( #69304, #46596, #21299 ),
 ( #54136, #2945, #87077 ),
 ( #13150, #35899, #68776 ),
 ( #78961, #101656, #27815 ),
 ( #60684, #93571, #19719 ),
 ( #53104, #102178, #28327 ),
 ( #69818, #86027, #61204 ),
 ( #12097, #102715, #94648 ),
 ( #28879, #61750, #15290 ),
 ( #80016, #7187, #22885 ),
 ( #64390, #56254, #40102 ),
 ( #81076, #97266, #88132 ),
 ( #55722, #23411, #48175 ),
 ( #89188, #71936, #14214 ),
 ( #31509, #48701, #47644 ),
 ( #64908, #63863, #6126 ) ),
 .UNSPECIFIED., .F., .F., .F. ) 
 B_SPLINE_SURFACE_WITH_KNOTS ( ( 4, 2, 2, 2, 2, 2, 2, 2, 2, 2, 2, 4 ),
 ( 3, 3 ),
 ( 0.005037129470918477389, 0.006635042084548149581, 0.007433998391362986111, 0.008232954698177821773, 0.009830867311807493097, 0.01062982361862232876, 0.01142877992543716442, 0.01302669253906683575, 0.01462460515269650881, 0.01542356145951134447, 0.01622251776632618187, 0.01782043037995585319 ),
 ( 0.000000000000000000, 1.000000000000000000 ),
 .UNSPECIFIED. ) 
 GEOMETRIC_REPRESENTATION_ITEM ( )  RATIONAL_B_SPLINE_SURFACE ( (
 ( 1.000000000000000000, 0.7071067811865475727, 1.000000000000000000),
 ( 1.000000000000000000, 0.7084299270926217584, 1.000000000000000000),
 ( 1.000000000000000000, 0.7118707319821261370, 1.000000000000000000),
 ( 1.000000000000000000, 0.7196931121702430101, 1.000000000000000000),
 ( 1.000000000000000000, 0.7227437164891366006, 1.000000000000000000),
 ( 1.000000000000000000, 0.7296388212890008163, 1.000000000000000000),
 ( 1.000000000000000000, 0.7334745704062100025, 1.000000000000000000),
 ( 1.000000000000000000, 0.7457129707556888754, 1.000000000000000000),
 ( 1.000000000000000000, 0.7549127490209673885, 1.000000000000000000),
 ( 1.000000000000000000, 0.7694591811115146784, 1.000000000000000000),
 ( 1.000000000000000000, 0.7744510510067527109, 1.000000000000000000),
 ( 1.000000000000000000, 0.7843714700247860216, 1.000000000000000000),
 ( 1.000000000000000000, 0.7893201836189067677, 1.000000000000000000),
 ( 1.000000000000000000, 0.8039615404448176017, 1.000000000000000000),
 ( 1.000000000000000000, 0.8134756678392851548, 1.000000000000000000),
 ( 1.000000000000000000, 0.8310114419075367298, 1.000000000000000000),
 ( 1.000000000000000000, 0.8387987601958035722, 1.000000000000000000),
 ( 1.000000000000000000, 0.8485725036619826689, 1.000000000000000000),
 ( 1.000000000000000000, 0.8515123028897164659, 1.000000000000000000),
 ( 1.000000000000000000, 0.8566700882282884955, 1.000000000000000000),
 ( 1.000000000000000000, 0.8588953665494961642, 1.000000000000000000),
 ( 1.000000000000000000, 0.8642157076431438156, 1.000000000000000000),
 ( 1.000000000000000000, 0.8660228936532952115, 1.000000000000000000),
 ( 1.000000000000000000, 0.8660254037844388186, 1.000000000000000000) ) ) 
 REPRESENTATION_ITEM ( '' )  SURFACE ( )  );
#85170 = CARTESIAN_POINT ( 'NONE',  ( 20.00000000000000711, 5.000000000000000888, 25.00000000000000000 ) ) ;
#85171 = CARTESIAN_POINT ( 'NONE',  ( 15.49776003472984343, 37.05489105806098138, -22.93080861416551031 ) ) ;
#85172 = DIRECTION ( 'NONE',  ( 0.000000000000000000, -1.000000000000000000, 0.000000000000000000 ) ) ;
#85173 = EDGE_LOOP ( 'NONE', ( #65756, #66678 ) ) ;
#85174 = CARTESIAN_POINT ( 'NONE',  ( -30.05061994666513314, 312.1672957118879026, -7.283488774298362500 ) ) ;
#85175 = CARTESIAN_POINT ( 'NONE',  ( -38.82405594768357560, 321.9282899208834579, 16.54806888951848265 ) ) ;
#85176 = DIRECTION ( 'NONE',  ( -1.000000000000000000, -1.224606353822377258E-16, -0.000000000000000000 ) ) ;
#85177 = DIRECTION ( 'NONE',  ( -1.000000000000000000, -0.000000000000000000, -0.000000000000000000 ) ) ;
#85178 = CARTESIAN_POINT ( 'NONE',  ( 3.313708498984762052, -19.71874999999999645, -8.000000000000000000 ) ) ;
#85179 = CARTESIAN_POINT ( 'NONE',  ( 6.499001506047761723, -13.07634269194914722, 32.05319514180078500 ) ) ;
#85180 = DIRECTION ( 'NONE',  ( -0.000000000000000000, -1.000000000000000000, -0.000000000000000000 ) ) ;
#85181 = ORIENTED_EDGE ( 'NONE', *, *, #94297, .F. ) ;
#85182 = CARTESIAN_POINT ( 'NONE',  ( 85.89771287621293538, -25.01010825923657777, 177.6372282980652813 ) ) ;
#85183 = DIRECTION ( 'NONE',  ( -1.000000000000000000, 0.000000000000000000, 0.000000000000000000 ) ) ;
#85184 = CARTESIAN_POINT ( 'NONE',  ( 5.947762761376476526, 4.378239541354660425, -5.416666666666668739 ) ) ;
#85185 = EDGE_LOOP ( 'NONE', ( #56771, #52122, #33427, #98754, #43209 ) ) ;
#85186 = MECHANICAL_DESIGN_GEOMETRIC_PRESENTATION_REPRESENTATION (  '', ( #24920 ), #14560 ) ;
#85187 = CARTESIAN_POINT ( 'NONE',  ( -87.30325485981414602, -45.26540918670090718, 53.23313115482674363 ) ) ;
#85188 = CARTESIAN_POINT ( 'NONE',  ( 0.5805565836007648972, -7.505553499465138501, -1.190388518514737689E-16 ) ) ;
#85189 = CARTESIAN_POINT ( 'NONE',  ( 9.937561876413942841, -5.000000000000002665, -76.56466736914200055 ) ) ;
#85190 = DIRECTION ( 'NONE',  ( 1.000000000000000000, -0.000000000000000000, -0.000000000000000000 ) ) ;
#85191 = CARTESIAN_POINT ( 'NONE',  ( -36.90887455182773635, -31.96477001361924764, -37.72354277451468363 ) ) ;
#85192 = VECTOR ( 'NONE', #44879, 1000.000000000000000 ) ;
#85193 = AXIS2_PLACEMENT_3D ( 'NONE', #91034, #76412, #78544 ) ;
#85194 = CIRCLE ( 'NONE', #57601, 4.000000000000007105 ) ;
#85195 = CARTESIAN_POINT ( 'NONE',  ( 13.45774757525579268, -59.99999999999997158, 39.73009970327057516 ) ) ;
#85196 = CARTESIAN_POINT ( 'NONE',  ( 28.93001008276146635, -31.73066402266886499, 39.98636524211740806 ) ) ;
#85197 = FACE_OUTER_BOUND ( 'NONE', #31151, .T. ) ;
#85199 = CARTESIAN_POINT ( 'NONE',  ( -13.74817541072891736, 20.46283863168138240, 6.678757362012751386 ) ) ;
#85198 = CARTESIAN_POINT ( 'NONE',  ( -29.97844425214491082, -32.43635721192953270, 40.56189535855136796 ) ) ;
#85200 = EDGE_CURVE ( 'NONE', #1, #12726, #12686, .T. ) ;
#85201 = CARTESIAN_POINT ( 'NONE',  ( 5.515535885521446247, 296.1986775320684728, -10.01281319186619001 ) ) ;
#85202 = CARTESIAN_POINT ( 'NONE',  ( -4.413590570192278406, -9.188952443232103917, 5.751919616880371677 ) ) ;
#85203 = CARTESIAN_POINT ( 'NONE',  ( 35.62336637792430594, 303.3604247956168365, -0.04934908291839113642 ) ) ;
#85204 = CARTESIAN_POINT ( 'NONE',  ( 32.33349330513380693, -3.851859888774471706E-31, 4.000000000000001776 ) ) ;
#85205 = ORIENTED_EDGE ( 'NONE', *, *, #38258, .T. ) ;
#85206 = DIRECTION ( 'NONE',  ( 0.000000000000000000, 1.000000000000000000, 0.000000000000000000 ) ) ;
#85207 = VERTEX_POINT ( 'NONE', #78490 ) ;
#85208 = CARTESIAN_POINT ( 'NONE',  ( 0.3157512944565053492, -3.097794232830064498, 7.999999999999998224 ) ) ;
#85209 = CARTESIAN_POINT ( 'NONE',  ( 32.61650669486618881, 0.000000000000000000, 4.000000000000000888 ) ) ;
#85210 = CARTESIAN_POINT ( 'NONE',  ( 5.190609988845225509, -62.36077713256408828, -3.016375611400011092 ) ) ;
#85211 = EDGE_CURVE ( 'NONE', #24805, #6815, #28540, .T. ) ;
#85213 = CARTESIAN_POINT ( 'NONE',  ( -15.98142407300128021, -47.40881529994586430, -34.25628805530171661 ) ) ;
#85212 =( NAMED_UNIT ( * ) SI_UNIT ( $, .STERADIAN. ) SOLID_ANGLE_UNIT ( ) );
#85214 = AXIS2_PLACEMENT_3D ( 'NONE', #31982, #30396, #64857 ) ;
#85215 = ORIENTED_EDGE ( 'NONE', *, *, #27984, .F. ) ;
#85216 = DIRECTION ( 'NONE',  ( 0.000000000000000000, -1.000000000000000000, 0.000000000000000000 ) ) ;
#85217 = CARTESIAN_POINT ( 'NONE',  ( 16.33361799548379523, -5.000000000000000000, 6.123233995736768255E-16 ) ) ;
#85218 = ORIENTED_EDGE ( 'NONE', *, *, #54768, .T. ) ;
#85219 = DIRECTION ( 'NONE',  ( -1.000000000000000000, 0.000000000000000000, 0.000000000000000000 ) ) ;
#85220 = CARTESIAN_POINT ( 'NONE',  ( 53.29999999999999716, 6.915964383211875250E-15, 0.000000000000000000 ) ) ;
#85221 = DIRECTION ( 'NONE',  ( -1.000000000000000000, -1.224606353822377258E-16, -0.000000000000000000 ) ) ;
#85222 = CARTESIAN_POINT ( 'NONE',  ( -91.87273713405024012, -60.00000000000000000, 10.11626477920355249 ) ) ;
#85223 = CARTESIAN_POINT ( 'NONE',  ( -5.656854249492379694, -25.43749999999999645, -5.656854249492380582 ) ) ;
#85224 =( GEOMETRIC_REPRESENTATION_CONTEXT ( 3 ) GLOBAL_UNCERTAINTY_ASSIGNED_CONTEXT ( ( #97862 ) ) GLOBAL_UNIT_ASSIGNED_CONTEXT ( ( #68842, #28950, #12695 ) ) REPRESENTATION_CONTEXT ( 'NONE', 'WORKASPACE' ) );
#85225 = CARTESIAN_POINT ( 'NONE',  ( -8.000000000000000000, -11.84374999999999289, -3.313708498984762496 ) ) ;
#85226 = CIRCLE ( 'NONE', #19842, 0.5000000000000000000 ) ;
#85227 = CIRCLE ( 'NONE', #36999, 12.00000000000000711 ) ;
#85229 = CARTESIAN_POINT ( 'NONE',  ( 5.000000000000002665, 152.0000000000000000, 5.000000000000000000 ) ) ;
#85228 = CARTESIAN_POINT ( 'NONE',  ( 8.737863884125493641, -3.000000000000002665, -79.96381019769830800 ) ) ;
#85230 = EDGE_CURVE ( 'NONE', #60761, #22594, #101183, .T. ) ;
#85231 = CARTESIAN_POINT ( 'NONE',  ( -82.72299685417047499, -39.49295184692452665, 167.2469102829343797 ) ) ;
#85232 = EDGE_LOOP ( 'NONE', ( #77289, #41967, #19469, #101174 ) ) ;
#85233 = STYLED_ITEM ( 'NONE', ( #101590 ), #85431 ) ;
#85234 = CARTESIAN_POINT ( 'NONE',  ( -43.61209369432236826, 434.3223138618526491, 14.49730483407481785 ) ) ;
#85235 = VERTEX_POINT ( 'NONE', #85000 ) ;
#85236 = STYLED_ITEM ( 'NONE', ( #71486 ), #13091 ) ;
#85237 = VERTEX_POINT ( 'NONE', #11084 ) ;
#85238 = DIRECTION ( 'NONE',  ( 0.000000000000000000, 0.000000000000000000, 1.000000000000000000 ) ) ;
#85239 = CARTESIAN_POINT ( 'NONE',  ( -7.012902693339047921, -4.999999999999998224, 16.13291991228729572 ) ) ;
#85240 = EDGE_CURVE ( 'NONE', #16503, #64476, #76048, .T. ) ;
#85241 =( NAMED_UNIT ( * ) PLANE_ANGLE_UNIT ( ) SI_UNIT ( $, .RADIAN. ) );
#85242 =( LENGTH_UNIT ( ) NAMED_UNIT ( * ) SI_UNIT ( .MILLI., .METRE. ) );
#85243 = ORIENTED_EDGE ( 'NONE', *, *, #67703, .F. ) ;
#85244 =( NAMED_UNIT ( * ) SI_UNIT ( $, .STERADIAN. ) SOLID_ANGLE_UNIT ( ) );
#85245 = CARTESIAN_POINT ( 'NONE',  ( -94.41342216801938036, -57.67108681604360498, -0.2751897739404595700 ) ) ;
#85246 = CARTESIAN_POINT ( 'NONE',  ( 27.10511071441197117, -1.200000000000000030E-05, 10.05698433968570704 ) ) ;
#85247 = CARTESIAN_POINT ( 'NONE',  ( 0.000000000000000000, 0.000000000000000000, 5.000000000000000888 ) ) ;
#85248 = CARTESIAN_POINT ( 'NONE',  ( -9.165151389911679658, 104.9999999999999858, -4.000000000000001776 ) ) ;
#85249 = FACE_OUTER_BOUND ( 'NONE', #60146, .T. ) ;
#85250 = DIRECTION ( 'NONE',  ( 0.000000000000000000, 0.000000000000000000, 1.000000000000000000 ) ) ;
#85251 = CARTESIAN_POINT ( 'NONE',  ( 91.97789438503755832, -14.21045842199438880, 64.70176211216229945 ) ) ;
#85252 = CARTESIAN_POINT ( 'NONE',  ( -97.13635602990564166, -30.00000000000002842, 199.9106954788804842 ) ) ;
#85253 = CARTESIAN_POINT ( 'NONE',  ( -56.51892958678620715, -56.85846262883293178, 71.22199430594528735 ) ) ;
#85254 = EDGE_LOOP ( 'NONE', ( #1294, #27351, #61603, #18072, #1495 ) ) ;
#85255 = DIRECTION ( 'NONE',  ( -1.000000000000000000, -1.224606353822377258E-16, -0.000000000000000000 ) ) ;
#85256 = EDGE_LOOP ( 'NONE', ( #52721, #8761, #17186, #17886, #6822 ) ) ;
#85257 = CARTESIAN_POINT ( 'NONE',  ( -102.2780374498291849, -45.26529867060920509, 188.3692498935314177 ) ) ;
#85258 = DIRECTION ( 'NONE',  ( 0.000000000000000000, -0.000000000000000000, 1.000000000000000000 ) ) ;
#85259 = CARTESIAN_POINT ( 'NONE',  ( -6.308794298586568594, 51.28513677629712220, 8.024939188852076910 ) ) ;
#85260 = CARTESIAN_POINT ( 'NONE',  ( 1.899847863968399331, -30.00000000000001066, 6.948366715868964150 ) ) ;
#85261 = ORIENTED_EDGE ( 'NONE', *, *, #25660, .F. ) ;
#85262 = CARTESIAN_POINT ( 'NONE',  ( 19.49496444267845519, 49.99961719514236336, 60.01447535217918983 ) ) ;
#85263 = SURFACE_SIDE_STYLE ('',( #77708 ) ) ;
#85264 = DIRECTION ( 'NONE',  ( 0.000000000000000000, -1.000000000000000000, 0.000000000000000000 ) ) ;
#85265 = CARTESIAN_POINT ( 'NONE',  ( 2.977408999572651815, -15.31250000204838457, 7.188101187500000933 ) ) ;
#85266 = CARTESIAN_POINT ( 'NONE',  ( -1.012588390450172460, 36.47564902558247013, -29.25078143156558141 ) ) ;
#85267 = DIRECTION ( 'NONE',  ( 0.000000000000000000, -0.3420201433256725987, -0.9396926207859068736 ) ) ;
#85268 = CONICAL_SURFACE ( 'NONE', #64559, 3.400000000000000355, 0.9599310885968748153 ) ;
#85269 = CARTESIAN_POINT ( 'NONE',  ( 7.896571385775229324, -81.21002000654247865, 1.305932416347435732 ) ) ;
#85270 = CARTESIAN_POINT ( 'NONE',  ( -12.34835181856066555, -4.332967528434497062, -12.86601580078907148 ) ) ;
#85271 = FACE_OUTER_BOUND ( 'NONE', #72103, .T. ) ;
#85272 = CARTESIAN_POINT ( 'NONE',  ( -6.928203230275507885, -85.00000000000000000, -4.000000000000001776 ) ) ;
#85273 =( NAMED_UNIT ( * ) SI_UNIT ( $, .STERADIAN. ) SOLID_ANGLE_UNIT ( ) );
#85274 = PRODUCT_DEFINITION_FORMATION_WITH_SPECIFIED_SOURCE ( 'ANY', '', #63166, .NOT_KNOWN. ) ;
#85275 = CARTESIAN_POINT ( 'NONE',  ( -30.74555747973485964, -46.43642797045591664, 34.64107672549393158 ) ) ;
#85276 = LINE ( 'NONE', #68025, #86950 ) ;
#85277 = CARTESIAN_POINT ( 'NONE',  ( 45.65249901139200261, -53.34829274510006769, 48.30469018026722239 ) ) ;
#85278 = CARTESIAN_POINT ( 'NONE',  ( -32.67430661331354713, 485.6291057174253751, 6.589190333393256438 ) ) ;
#85279 = CARTESIAN_POINT ( 'NONE',  ( 5.000000000000002665, 152.0000000000000000, -5.000000000000000000 ) ) ;
#85280 = CARTESIAN_POINT ( 'NONE',  ( -98.93768687063476364, -38.47564685778473148, 200.7974262912544816 ) ) ;
#85281 = ORIENTED_EDGE ( 'NONE', *, *, #70058, .F. ) ;
#85283 = CARTESIAN_POINT ( 'NONE',  ( 21.08349330513380693, 1.593028355512270962E-15, 0.000000000000000000 ) ) ;
#85282 = CARTESIAN_POINT ( 'NONE',  ( 84.45160259173304951, -38.35831399414499998, -23.32470882673439405 ) ) ;
#85284 = CARTESIAN_POINT ( 'NONE',  ( 81.19995102473650661, -60.00000000000004974, 183.8609189267522481 ) ) ;
#85285 = CARTESIAN_POINT ( 'NONE',  ( -19.07987706826217789, 49.64660923895987565, 61.77383235656444072 ) ) ;
#85286 = CARTESIAN_POINT ( 'NONE',  ( -7.039599673380882550, 41.52217312180329856, -58.93052077570905567 ) ) ;
#85287 = CARTESIAN_POINT ( 'NONE',  ( 5.273744720368365613, 41.55406131380648560, -70.69180554715100584 ) ) ;
#85288 = DIRECTION ( 'NONE',  ( 0.000000000000000000, 1.000000000000000000, 0.000000000000000000 ) ) ;
#85289 = CARTESIAN_POINT ( 'NONE',  ( 42.19180677453719142, 462.2931784592651638, 3.389262873192005809 ) ) ;
#85290 = CARTESIAN_POINT ( 'NONE',  ( 8.572527594031464315E-16, 61.50000000000000000, -6.999999999999992895 ) ) ;
#85291 = CARTESIAN_POINT ( 'NONE',  ( 106.9310636521288558, -60.00000000000000711, 197.1921110703508191 ) ) ;
#85292 = B_SPLINE_CURVE_WITH_KNOTS ( 'NONE', 3,
 ( #84203, #51819, #61007, #51282, #93891, #43213, #85819, #84734, #18428, #10817, #11896, #35692, #44823, #77709, #34093, #1668, #34625, #66966, #67496, #59410, #92274, #78746, #4344, #4880 ),
 .UNSPECIFIED., .F., .F.,
 ( 4, 2, 2, 2, 2, 2, 2, 2, 2, 2, 2, 4 ),
 ( 0.007801886282271855259, 0.008306033261743405588, 0.008810180241214956784, 0.009314327220686507980, 0.009566400710422282710, 0.009818474200158055706, 0.01007054768989382870, 0.01032262117962960343, 0.01057469466936537643, 0.01082676815910114942, 0.01133091513857269715, 0.01183506211804424488 ),
 .UNSPECIFIED. ) ;
#85293 = CIRCLE ( 'NONE', #90674, 5.000000000000000888 ) ;
#85294 = EDGE_CURVE ( 'NONE', #19286, #22326, #43810, .T. ) ;
#85295 = DIRECTION ( 'NONE',  ( 1.000000000000000000, 0.000000000000000000, 0.000000000000000000 ) ) ;
#85296 = VERTEX_POINT ( 'NONE', #64450 ) ;
#85297 = EDGE_CURVE ( 'NONE', #32332, #25223, #31750, .T. ) ;
#85298 = PRESENTATION_STYLE_ASSIGNMENT (( #18463 ) ) ;
#85299 = PRESENTATION_LAYER_ASSIGNMENT (  '', '', ( #2587 ) ) ;
#85300 = CARTESIAN_POINT ( 'NONE',  ( -80.75557906412130649, -30.00000000000003197, -12.51863527975343438 ) ) ;
#85301 = ORIENTED_EDGE ( 'NONE', *, *, #18794, .T. ) ;
#85303 = CARTESIAN_POINT ( 'NONE',  ( 32.03491031660919219, 464.8549693818604851, 13.92556383226224526 ) ) ;
#85302 = CARTESIAN_POINT ( 'NONE',  ( -74.65037011510671050, -38.33113839674835788, 166.1707960067358272 ) ) ;
#85304 = DIRECTION ( 'NONE',  ( -1.000000000000000000, -0.000000000000000000, -0.000000000000000000 ) ) ;
#85305 = LINE ( 'NONE', #45388, #62175 ) ;
#85306 = FACE_OUTER_BOUND ( 'NONE', #91882, .T. ) ;
#85307 = CARTESIAN_POINT ( 'NONE',  ( 7.188101187499999156, -13.62500000204838457, 2.977408999572654924 ) ) ;
#85309 = EDGE_CURVE ( 'NONE', #87052, #73379, #15348, .T. ) ;
#85308 = CARTESIAN_POINT ( 'NONE',  ( -9.596002107494335576, -5.000000000000002665, -92.37456064099097830 ) ) ;
#85310 =( GEOMETRIC_REPRESENTATION_CONTEXT ( 3 ) GLOBAL_UNCERTAINTY_ASSIGNED_CONTEXT ( ( #10953 ) ) GLOBAL_UNIT_ASSIGNED_CONTEXT ( ( #79380, #30325, #22242 ) ) REPRESENTATION_CONTEXT ( 'NONE', 'WORKASPACE' ) );
#85311 = MECHANICAL_DESIGN_GEOMETRIC_PRESENTATION_REPRESENTATION (  '', ( #83523 ), #31890 ) ;
#85312 = CARTESIAN_POINT ( 'NONE',  ( 38.54515645702225868, 1.482358050883964840E-15, 0.000000000000000000 ) ) ;
#85313 = STYLED_ITEM ( 'NONE', ( #61778 ), #35241 ) ;
#85315 = ORIENTED_EDGE ( 'NONE', *, *, #54559, .F. ) ;
#85314 = FACE_OUTER_BOUND ( 'NONE', #55401, .T. ) ;
#85316 = CARTESIAN_POINT ( 'NONE',  ( 83.84610521665520366, -35.96948417761220185, 172.3088706270825696 ) ) ;
#85317 = DIRECTION ( 'NONE',  ( -1.000000000000000000, 0.000000000000000000, 0.000000000000000000 ) ) ;
#85318 = CONICAL_SURFACE ( 'NONE', #49096, 3.309500000000007880, 0.9599310885968770357 ) ;
#85319 = CARTESIAN_POINT ( 'NONE',  ( 9.537927238823508347, 87.64626857118182102, -3.010735687602429156 ) ) ;
#85320 = VERTEX_POINT ( 'NONE', #13214 ) ;
#85321 = CARTESIAN_POINT ( 'NONE',  ( 42.51086551946173131, 484.3281707585954905, -1.915972276551562548 ) ) ;
#85322 = CARTESIAN_POINT ( 'NONE',  ( -47.90320435033602564, 17.06740859345675787, 14.35535821593516559 ) ) ;
#85323 = CARTESIAN_POINT ( 'NONE',  ( 37.72605696939957909, 27.54990033529972138, -13.45617127781096123 ) ) ;
#85324 = LINE ( 'NONE', #86930, #38305 ) ;
#85325 = CARTESIAN_POINT ( 'NONE',  ( -5.910690929868577470, 253.8649590609318807, -1.065041252563913465 ) ) ;
#85326 = CARTESIAN_POINT ( 'NONE',  ( 0.7723747150160921171, 18.23314980831915122, 49.51284287117157135 ) ) ;
#85327 = DIRECTION ( 'NONE',  ( 0.000000000000000000, 0.000000000000000000, 1.000000000000000000 ) ) ;
#85328 = EDGE_LOOP ( 'NONE', ( #98988, #40154, #46101, #94926 ) ) ;
#85329 = SURFACE_SIDE_STYLE ('',( #36292 ) ) ;
#85330 = CARTESIAN_POINT ( 'NONE',  ( -7.152384844127436025, 296.5444182697836482, 6.994491946633746515 ) ) ;
#85331 = CARTESIAN_POINT ( 'NONE',  ( 17.34830914839334781, 18.64284798592843373, 34.29224544877874337 ) ) ;
#85332 = CARTESIAN_POINT ( 'NONE',  ( 87.07023238404832455, -24.31684118448634280, 186.7349181601837245 ) ) ;
#85334 = CARTESIAN_POINT ( 'NONE',  ( -13.27507766870887451, 3.850002543425556034, -6.914036890321489714 ) ) ;
#85333 = DIRECTION ( 'NONE',  ( 0.000000000000000000, -1.000000000000000000, 0.000000000000000000 ) ) ;
#85335 = ADVANCED_FACE ( 'NONE', ( #21890 ), #105780, .T. ) ;
#85336 = CARTESIAN_POINT ( 'NONE',  ( 7.188101187500001821, -26.56250000204838457, -2.977408999572650483 ) ) ;
#85337 = DIRECTION ( 'NONE',  ( 0.9735618822052786170, 0.000000000000000000, -0.2284234259372612819 ) ) ;
#85338 = CARTESIAN_POINT ( 'NONE',  ( 30.59999999999999787, 3.309500000000003439, 4.052968581778167743E-16 ) ) ;
#85339 = ITEM_DEFINED_TRANSFORMATION ( 'NONE', 'NONE', #24934,  #10728 ) ;
#85340 = ORIENTED_EDGE ( 'NONE', *, *, #105016, .T. ) ;
#85341 = CARTESIAN_POINT ( 'NONE',  ( 40.66024587926714418, 485.8034863302610233, -4.843677042987392767 ) ) ;
#85342 = FACE_OUTER_BOUND ( 'NONE', #20519, .T. ) ;
#85343 = CARTESIAN_POINT ( 'NONE',  ( -9.998567040938999284, 7.502056690389962590, 0.000000000000000000 ) ) ;
#85344 = ADVANCED_FACE ( 'NONE', ( #80604 ), #9838, .F. ) ;
#85345 = DIRECTION ( 'NONE',  ( 0.000000000000000000, 0.000000000000000000, 1.000000000000000000 ) ) ;
#85346 = EDGE_CURVE ( 'NONE', #8297, #62772, #11071, .T. ) ;
#85347 = EDGE_LOOP ( 'NONE', ( #60957, #100537, #77793, #89532 ) ) ;
#85348 = CARTESIAN_POINT ( 'NONE',  ( -8.235963203755042983, 51.66292127458935823, -4.031152949374507521 ) ) ;
#85349 = CARTESIAN_POINT ( 'NONE',  ( 2.040829700809986047, 50.00000000000000000, -98.00000000000000000 ) ) ;
#85350 = ORIENTED_EDGE ( 'NONE', *, *, #94422, .F. ) ;
#85351 =( NAMED_UNIT ( * ) SI_UNIT ( $, .STERADIAN. ) SOLID_ANGLE_UNIT ( ) );
#85352 = CARTESIAN_POINT ( 'NONE',  ( -8.000000000000001776, -22.34375000409677270, 3.313708498984759387 ) ) ;
#85353 = CARTESIAN_POINT ( 'NONE',  ( 32.78741055188847042, 485.3331003366707819, 5.977022408747033388 ) ) ;
#85354 =( NAMED_UNIT ( * ) PLANE_ANGLE_UNIT ( ) SI_UNIT ( $, .RADIAN. ) );
#85355 = CARTESIAN_POINT ( 'NONE',  ( -94.68332376739145673, -60.00000000000000000, 202.5677762804762949 ) ) ;
#85356 = CARTESIAN_POINT ( 'NONE',  ( 18.97029851426021096, 49.42830426956580681, 61.97293826772167336 ) ) ;
#85357 = CARTESIAN_POINT ( 'NONE',  ( 16.36650669486618881, 1.474610560812782335E-15, 0.000000000000000000 ) ) ;
#85358 = CARTESIAN_POINT ( 'NONE',  ( 0.000000000000000000, -78.00000000000000000, 27.00000000000000000 ) ) ;
#85359 = CYLINDRICAL_SURFACE ( 'NONE', #40487, 5.000000000000000000 ) ;
#85360 = EDGE_CURVE ( 'NONE', #9600, #40876, #55798, .T. ) ;
#85361 = CARTESIAN_POINT ( 'NONE',  ( -84.83234346679212479, -39.37621439949131030, 182.9386712835791116 ) ) ;
#85362 = VECTOR ( 'NONE', #36951, 1000.000000000000000 ) ;
#85363 = CARTESIAN_POINT ( 'NONE',  ( -4.181427851358347603, 54.26024483359611139, -6.680433775739387237 ) ) ;
#85364 = ORIENTED_EDGE ( 'NONE', *, *, #11292, .T. ) ;
#85365 = CARTESIAN_POINT ( 'NONE',  ( -9.508921847869125088, 46.21454289499524037, -13.17524946764681282 ) ) ;
#85366 = EDGE_CURVE ( 'NONE', #7404, #57904, #100628, .T. ) ;
#85368 = CARTESIAN_POINT ( 'NONE',  ( 16.65484354297773351, 1.340359594676612611E-15, 0.000000000000000000 ) ) ;
#85367 = TOROIDAL_SURFACE ( 'NONE', #33729, 10.00000000000000000, 0.5000000000000000000 ) ;
#85369 = CARTESIAN_POINT ( 'NONE',  ( -82.98397381039904985, -37.81828557849092221, -0.6893747078036359666 ) ) ;
#85370 = CYLINDRICAL_SURFACE ( 'NONE', #80504, 1.999999999999998224 ) ;
#85371 = FILL_AREA_STYLE ('',( #19623 ) ) ;
#85372 = MECHANICAL_DESIGN_GEOMETRIC_PRESENTATION_REPRESENTATION (  '', ( #30275 ), #24282 ) ;
#85373 = CIRCLE ( 'NONE', #52648, 3.309500000000001663 ) ;
#85374 = CARTESIAN_POINT ( 'NONE',  ( 7.849086896557461834, 81.65194826718307297, 2.456708681988599773E-12 ) ) ;
#85375 = CARTESIAN_POINT ( 'NONE',  ( -6.033336773385747698, -14.92884390011200502, 14.31563199681415632 ) ) ;
#85376 = CARTESIAN_POINT ( 'NONE',  ( -15.50526908257195835, 42.00000000000000000, -57.69562748404377572 ) ) ;
#85377 = EDGE_CURVE ( 'NONE', #31057, #105843, #189, .T. ) ;
#85378 = CARTESIAN_POINT ( 'NONE',  ( 78.26152162121309175, -14.21045842199439946, 161.8191806974193696 ) ) ;
#85379 =( NAMED_UNIT ( * ) PLANE_ANGLE_UNIT ( ) SI_UNIT ( $, .RADIAN. ) );
#85380 = CARTESIAN_POINT ( 'NONE',  ( -89.53165980454747341, -30.00000000000000000, -13.19740150267569767 ) ) ;
#85381 = CARTESIAN_POINT ( 'NONE',  ( -69.47164100847101054, -60.33650507013528852, 112.5478477857417232 ) ) ;
#85382 = AXIS2_PLACEMENT_3D ( 'NONE', #9072, #84041, #74860 ) ;
#85383 = ORIENTED_EDGE ( 'NONE', *, *, #90298, .F. ) ;
#85384 = CARTESIAN_POINT ( 'NONE',  ( 108.4902253387283793, -59.99999999999992184, 199.0859659658876524 ) ) ;
#85385 = CARTESIAN_POINT ( 'NONE',  ( 14.00414139509130784, -57.67120807224324608, -44.20775937555332291 ) ) ;
#85386 = ADVANCED_FACE ( 'NONE', ( #6185 ), #70563, .T. ) ;
#85387 = CIRCLE ( 'NONE', #68132, 10.00000000000000000 ) ;
#85389 = ORIENTED_EDGE ( 'NONE', *, *, #58533, .T. ) ;
#85388 = AXIS2_PLACEMENT_3D ( 'NONE', #87250, #27985, #85660 ) ;
#85390 = CARTESIAN_POINT ( 'NONE',  ( 13.98725534264629466, -57.97295057622655179, 27.65002740835610240 ) ) ;
#85391 = CARTESIAN_POINT ( 'NONE',  ( -5.082755093536326818, -27.59375000204838813, 5.082755093536325042 ) ) ;
#85392 = CARTESIAN_POINT ( 'NONE',  ( -1.099210409027892466, 27.97021247871829175, -38.88368413723794959 ) ) ;
#85393 = ORIENTED_EDGE ( 'NONE', *, *, #37845, .F. ) ;
#85394 = VERTEX_POINT ( 'NONE', #68708 ) ;
#85395 = CARTESIAN_POINT ( 'NONE',  ( 46.77666182531591943, 18.74137236369644910, -15.58806238568051228 ) ) ;
#85396 = CARTESIAN_POINT ( 'NONE',  ( -24.04720975275586881, -60.00000000000493827, 43.35146360697347490 ) ) ;
#85397 = CARTESIAN_POINT ( 'NONE',  ( 28.56029514625197052, 307.6844803076128869, -9.136023263255507842 ) ) ;
#85398 = CARTESIAN_POINT ( 'NONE',  ( 7.188101187500000044, -30.03125000204838813, 0.000000000000000000 ) ) ;
#85399 = CARTESIAN_POINT ( 'NONE',  ( -48.02835407290516656, 16.78162100668608048, 14.35535821593516559 ) ) ;
#85400 = AXIS2_PLACEMENT_3D ( 'NONE', #65425, #30967, #98321 ) ;
#85401 = CARTESIAN_POINT ( 'NONE',  ( 2.109839796630671227, -0.2109020744221661026, 102.5367317923686556 ) ) ;
#85402 = DIRECTION ( 'NONE',  ( -1.000000000000000000, -1.224606353822377258E-16, -0.000000000000000000 ) ) ;
#85403 = CARTESIAN_POINT ( 'NONE',  ( -10.48543666094731464, 50.00000000000000000, -91.04342776276725147 ) ) ;
#85404 = FACE_OUTER_BOUND ( 'NONE', #15309, .T. ) ;
#85405 = CARTESIAN_POINT ( 'NONE',  ( 41.15811204217011010, 436.5847606186501366, 6.466625614333893601 ) ) ;
#85406 = B_SPLINE_CURVE_WITH_KNOTS ( 'NONE', 3,
 ( #32083, #54195, #95222, #87134, #46137, #104349, #79024, #5142 ),
 .UNSPECIFIED., .F., .F.,
 ( 4, 2, 2, 4 ),
 ( 1.734723475976807094E-18, 0.002725205121551986433, 0.004087807682327984637, 0.005450410243103983275 ),
 .UNSPECIFIED. ) ;
#85407 = UNCERTAINTY_MEASURE_WITH_UNIT (LENGTH_MEASURE( 1.000000000000000082E-05 ), #54293, 'distance_accuracy_value', 'NONE');
#85408 = ORIENTED_EDGE ( 'NONE', *, *, #79227, .T. ) ;
#85409 = CARTESIAN_POINT ( 'NONE',  ( 5.833333333333327708, -4.000000000000004441, 103.8776713793258608 ) ) ;
#85411 = CARTESIAN_POINT ( 'NONE',  ( 31.12421421041707248, -18.66565208751482174, 29.72625561025419572 ) ) ;
#85410 = CYLINDRICAL_SURFACE ( 'NONE', #1028, 5.000000000000002665 ) ;
#85412 = CARTESIAN_POINT ( 'NONE',  ( 6.601913983208107517, -4.285714285714895766, -24.56594385547655790 ) ) ;
#85413 = ORIENTED_EDGE ( 'NONE', *, *, #18875, .F. ) ;
#85414 = CARTESIAN_POINT ( 'NONE',  ( -9.999999999999994671, 48.00000000000000000, -86.30899693899574743 ) ) ;
#85416 = CARTESIAN_POINT ( 'NONE',  ( -5.500000000000006217, 42.00000000000000000, -59.88032989329961708 ) ) ;
#85415 = CARTESIAN_POINT ( 'NONE',  ( -26.94599015477662363, 34.53165509030868918, -10.05698433968608896 ) ) ;
#85417 = CARTESIAN_POINT ( 'NONE',  ( 0.000000000000000000, 4.898587196589412829E-16, -4.000000000000000000 ) ) ;
#85418 = CARTESIAN_POINT ( 'NONE',  ( 25.21823338009918203, -5.000000000000000888, 6.123233995736769241E-16 ) ) ;
#85419 = PRESENTATION_STYLE_ASSIGNMENT (( #77855 ) ) ;
#85420 = CARTESIAN_POINT ( 'NONE',  ( -19.99999999999999289, 5.000000000000000888, 25.00000000000000000 ) ) ;
#85421 = CARTESIAN_POINT ( 'NONE',  ( 37.38561277374697056, 1.340359594676612611E-15, 0.000000000000000000 ) ) ;
#85422 = ORIENTED_EDGE ( 'NONE', *, *, #67133, .T. ) ;
#85423 = CARTESIAN_POINT ( 'NONE',  ( 91.85465987230205087, -59.99999999999999289, 11.69882378743306717 ) ) ;
#85424 =( LENGTH_UNIT ( ) NAMED_UNIT ( * ) SI_UNIT ( .MILLI., .METRE. ) );
#85425 = DIRECTION ( 'NONE',  ( -1.000000000000000000, -0.000000000000000000, -0.000000000000000000 ) ) ;
#85426 = CARTESIAN_POINT ( 'NONE',  ( -35.48030077899827006, 426.7164938744821825, 6.204872843841080510 ) ) ;
#85427 = AXIS2_PLACEMENT_3D ( 'NONE', #42610, #2676, #1055 ) ;
#85428 = CARTESIAN_POINT ( 'NONE',  ( -4.852941176476488927, 40.28748004600674903, -70.80672828634432392 ) ) ;
#85429 = DIRECTION ( 'NONE',  ( 0.000000000000000000, 0.000000000000000000, -1.000000000000000000 ) ) ;
#85430 = ORIENTED_EDGE ( 'NONE', *, *, #21730, .T. ) ;
#85431 = ADVANCED_FACE ( 'NONE', ( #36369 ), #34781, .F. ) ;
#85432 = CARTESIAN_POINT ( 'NONE',  ( -109.4058916485573576, -30.00000000000661871, 179.3849327511039178 ) ) ;
#85433 = EDGE_LOOP ( 'NONE', ( #41003, #32862, #89878 ) ) ;
#85434 = DIRECTION ( 'NONE',  ( 0.000000000000000000, -1.000000000000000000, 0.000000000000000000 ) ) ;
#85435 = CARTESIAN_POINT ( 'NONE',  ( 3.898086217683916832, -13.33789614101576682, -12.77952306666688109 ) ) ;
#85436 = DIRECTION ( 'NONE',  ( 0.000000000000000000, 0.000000000000000000, 1.000000000000000000 ) ) ;
#85437 = CARTESIAN_POINT ( 'NONE',  ( 16.11715839250286919, 21.56713793043144278, -2.163674775856062826 ) ) ;
#85438 = CARTESIAN_POINT ( 'NONE',  ( 83.86240317988412585, -45.27766788077440197, -12.38235677868432205 ) ) ;
#85439 = CARTESIAN_POINT ( 'NONE',  ( -30.80797925829203976, 309.0763670535902179, -8.567432199028438333 ) ) ;
#85440 = CARTESIAN_POINT ( 'NONE',  ( 13.09999999999999787, 3.309500000000003439, 4.052968581778167743E-16 ) ) ;
#85442 = EDGE_CURVE ( 'NONE', #27490, #72526, #13085, .T. ) ;
#85441 = CYLINDRICAL_SURFACE ( 'NONE', #65695, 5.000000000000000888 ) ;
#85443 = CARTESIAN_POINT ( 'NONE',  ( 72.51657123412842054, -41.65836498953471079, -21.93284144621084053 ) ) ;
#85444 = VERTEX_POINT ( 'NONE', #71860 ) ;
#85445 = CARTESIAN_POINT ( 'NONE',  ( -43.58525199864187272, 435.7810069860521480, 17.82023302324694569 ) ) ;
#85446 = ORIENTED_EDGE ( 'NONE', *, *, #90712, .T. ) ;
#85447 = DIRECTION ( 'NONE',  ( 1.000000000000000000, 1.224606353822377258E-16, 0.000000000000000000 ) ) ;
#85448 =( LENGTH_UNIT ( ) NAMED_UNIT ( * ) SI_UNIT ( .MILLI., .METRE. ) );
#85450 = ORIENTED_EDGE ( 'NONE', *, *, #33854, .T. ) ;
#85449 = CARTESIAN_POINT ( 'NONE',  ( -2.324561895696642773E-13, 53.39766064372246746, 10.25000000000230038 ) ) ;
#85451 = CARTESIAN_POINT ( 'NONE',  ( 74.24571010611629163, -49.90480856335479132, 125.1173812749847514 ) ) ;
#85452 = MECHANICAL_DESIGN_GEOMETRIC_PRESENTATION_REPRESENTATION (  '', ( #42389 ), #44098 ) ;
#85453 = ORIENTED_EDGE ( 'NONE', *, *, #32427, .T. ) ;
#85454 = CARTESIAN_POINT ( 'NONE',  ( 6.354875581175684296, -49.58570828476184289, 39.47587273802374597 ) ) ;
#85455 = CARTESIAN_POINT ( 'NONE',  ( -7.188101187500002709, -21.31250000204838813, 2.977408999572647819 ) ) ;
#85456 = CARTESIAN_POINT ( 'NONE',  ( -101.2734545671114290, -57.63007487344309254, 203.5435050992661843 ) ) ;
#85457 = EDGE_CURVE ( 'NONE', #83726, #68935, #21523, .T. ) ;
#85458 = AXIS2_PLACEMENT_3D ( 'NONE', #86280, #102439, #87329 ) ;
#85459 = ORIENTED_EDGE ( 'NONE', *, *, #53888, .T. ) ;
#85460 =( LENGTH_UNIT ( ) NAMED_UNIT ( * ) SI_UNIT ( .MILLI., .METRE. ) );
#85461 = CARTESIAN_POINT ( 'NONE',  ( -31.76732676843110781, 43.01778740796270029, -66.82714613718027863 ) ) ;
#85462 = CARTESIAN_POINT ( 'NONE',  ( 106.4261979399583993, -60.15152501556619313, 168.2421470263708159 ) ) ;
#85463 = CARTESIAN_POINT ( 'NONE',  ( -9.165151389911679658, 85.00000000000000000, 4.000000000000000000 ) ) ;
#85464 = CARTESIAN_POINT ( 'NONE',  ( 95.42421628608209971, -5.000000000000000888, 6.123233995736779101E-16 ) ) ;
#85465 = ADVANCED_FACE ( 'NONE', ( #38466 ), #20940, .T. ) ;
#85466 = STYLED_ITEM ( 'NONE', ( #85298 ), #89040 ) ;
#85467 = CARTESIAN_POINT ( 'NONE',  ( 8.000000000000000000, -17.18750000409676915, 0.000000000000000000 ) ) ;
#85468 = CONICAL_SURFACE ( 'NONE', #76826, 4.172000000000009479, 0.9599310885968813656 ) ;
#85469 = CARTESIAN_POINT ( 'NONE',  ( -41.60704211633953520, -27.00187119801606173, 37.06697387215593409 ) ) ;
#85470 = CIRCLE ( 'NONE', #99217, 4.000000000000000888 ) ;
#85471 = CARTESIAN_POINT ( 'NONE',  ( -37.24861026655265306, 25.58887987570736655, 13.42549399110521335 ) ) ;
#85472 = VECTOR ( 'NONE', #71422, 1000.000000000000000 ) ;
#85473 = CARTESIAN_POINT ( 'NONE',  ( -46.00000000000000000, 488.7535717825852544, 4.225312566738604225 ) ) ;
#85474 = CARTESIAN_POINT ( 'NONE',  ( 0.000000000000000000, 0.000000000000000000, -7.657127082228716297 ) ) ;
#85475 = CARTESIAN_POINT ( 'NONE',  ( 97.48272865599727766, -52.68889013459489945, 195.2151372445526647 ) ) ;
#85476 = CARTESIAN_POINT ( 'NONE',  ( 33.78291765283140080, 183.1183258647170362, 182.1969486012845891 ) ) ;
#85477 = CARTESIAN_POINT ( 'NONE',  ( 6.643741133345863581, -29.99999999999999645, -3.073381310751047035 ) ) ;
#85478 = VERTEX_POINT ( 'NONE', #21762 ) ;
#85479 =( NAMED_UNIT ( * ) PLANE_ANGLE_UNIT ( ) SI_UNIT ( $, .RADIAN. ) );
#85480 = LINE ( 'NONE', #13152, #85362 ) ;
#85482 = CARTESIAN_POINT ( 'NONE',  ( 0.000000000000000000, -30.00000000000000000, 8.000000000000000000 ) ) ;
#85481 =( BOUNDED_SURFACE ( )  B_SPLINE_SURFACE ( 2, 3, ( 
 ( #78367, #10961, #37426, #101593, #44421, #69240, #20190, #102654, #84346, #61693, #53044, #103189, #44966, #27750, #94584, #69759, #68712, #29333, #85412, #51432, #36892, #10440, #43355, #60623, #11494, #12037, #77847, #76239, #2348, #3961, #19123, #84876, #77316, #68157 ),
 ( #101052, #27208, #92962, #51960, #76772, #54599, #22822, #95623, #95107, #56184, #46017, #54075, #78898, #105304, #79951, #6062, #79430, #104229, #5024, #87017, #55656, #81008, #30917, #29856, #21242, #63798, #96161, #46536, #62734, #38988, #15222, #6592, #47051, #31447 ),
 ( #5542, #30376, #37957, #13088, #88593, #7124, #96685, #21764, #38468, #71862, #63266, #88069, #22293, #104768, #71335, #40038, #47581, #70818, #13621, #87540, #72913, #72398, #14674, #64328, #80476, #55139, #14148, #39523, #97199, #23344, #89123, #48107, #103709, #105822 ) ),
 .UNSPECIFIED., .F., .T., .F. ) 
 B_SPLINE_SURFACE_WITH_KNOTS ( ( 3, 3 ),
 ( 4, 2, 2, 2, 2, 2, 2, 2, 2, 2, 2, 2, 2, 2, 2, 2, 4 ),
 ( 0.000000000000000000, 1.000000000000000000 ),
 ( -3.141592653589793116, -2.748893571891068976, -2.356194490192344837, -1.963495408493620697, -1.570796326794896558, -1.178097245096172418, -0.7853981633974482790, -0.3926990816987241395, 0.000000000000000000, 0.3926990816987241395, 0.7853981633974482790, 1.178097245096172418, 1.570796326794896558, 1.963495408493620697, 2.356194490192344837, 2.748893571891068976, 3.141592653589793116 ),
 .UNSPECIFIED. ) 
 GEOMETRIC_REPRESENTATION_ITEM ( )  RATIONAL_B_SPLINE_SURFACE ( (
 ( 1.000000000000000000, 1.000000000000000000, 1.000000000000000000, 1.000000000000000000, 1.000000000000000000, 1.000000000000000000, 1.000000000000000000, 1.000000000000000000, 1.000000000000000000, 1.000000000000000000, 1.000000000000000000, 1.000000000000000000, 1.000000000000000000, 1.000000000000000000, 1.000000000000000000, 1.000000000000000000, 1.000000000000000000, 1.000000000000000000, 1.000000000000000000, 1.000000000000000000, 1.000000000000000000, 1.000000000000000000, 1.000000000000000000, 1.000000000000000000, 1.000000000000000000, 1.000000000000000000, 1.000000000000000000, 1.000000000000000000, 1.000000000000000000, 1.000000000000000000, 1.000000000000000000, 1.000000000000000000, 1.000000000000000000, 1.000000000000000000),
 ( 1.857142857142858317, 1.857142857142858317, 1.857142857142858317, 1.857142857142858317, 1.857142857142858317, 1.857142857142858317, 1.857142857142858317, 1.857142857142858317, 1.857142857142858317, 1.857142857142858317, 1.857142857142858317, 1.857142857142858317, 1.857142857142858317, 1.857142857142858317, 1.857142857142858317, 1.857142857142858317, 1.857142857142858317, 1.857142857142858317, 1.857142857142858317, 1.857142857142858317, 1.857142857142858317, 1.857142857142858317, 1.857142857142858317, 1.857142857142858317, 1.857142857142858317, 1.857142857142858317, 1.857142857142858317, 1.857142857142858317, 1.857142857142858317, 1.857142857142858317, 1.857142857142858317, 1.857142857142858317, 1.857142857142858317, 1.857142857142858317),
 ( 1.000000000000000000, 1.000000000000000000, 1.000000000000000000, 1.000000000000000000, 1.000000000000000000, 1.000000000000000000, 1.000000000000000000, 1.000000000000000000, 1.000000000000000000, 1.000000000000000000, 1.000000000000000000, 1.000000000000000000, 1.000000000000000000, 1.000000000000000000, 1.000000000000000000, 1.000000000000000000, 1.000000000000000000, 1.000000000000000000, 1.000000000000000000, 1.000000000000000000, 1.000000000000000000, 1.000000000000000000, 1.000000000000000000, 1.000000000000000000, 1.000000000000000000, 1.000000000000000000, 1.000000000000000000, 1.000000000000000000, 1.000000000000000000, 1.000000000000000000, 1.000000000000000000, 1.000000000000000000, 1.000000000000000000, 1.000000000000000000) ) ) 
 REPRESENTATION_ITEM ( '' )  SURFACE ( )  );
#85483 = CARTESIAN_POINT ( 'NONE',  ( 17.78280590860698140, -20.33637464548202445, -37.74591371100264325 ) ) ;
#85484 = CARTESIAN_POINT ( 'NONE',  ( -86.31380317257726631, -29.99999999999999645, 180.5119918063797115 ) ) ;
#85485 = EDGE_CURVE ( 'NONE', #28024, #104209, #61076, .T. ) ;
#85486 = B_SPLINE_CURVE_WITH_KNOTS ( 'NONE', 3,
 ( #48715, #56266, #57335, #81092, #90258, #71951, #96769, #105383, #16360, #7730, #15302, #71408, #22376, #40113, #79510, #38543, #89203, #5620 ),
 .UNSPECIFIED., .F., .F.,
 ( 4, 2, 2, 2, 2, 2, 2, 2, 4 ),
 ( 0.5000000000001136868, 0.5625000000000994760, 0.6250000000000852651, 0.6875000000000711653, 0.7500000000000569544, 0.8125000000000427436, 0.8750000000000284217, 0.9375000000000142109, 1.000000000000000000 ),
 .UNSPECIFIED. ) ;
#85487 = ORIENTED_EDGE ( 'NONE', *, *, #96766, .T. ) ;
#85488 = VECTOR ( 'NONE', #95927, 1000.000000000000000 ) ;
#85489 = CARTESIAN_POINT ( 'NONE',  ( -26.78474277083682864, 36.99592048761888208, -7.587964203663859486 ) ) ;
#85490 = CARTESIAN_POINT ( 'NONE',  ( 86.18040502910800171, -57.57669570564139860, 202.7805009680767512 ) ) ;
#85491 = CARTESIAN_POINT ( 'NONE',  ( 6.123233995736763324E-16, 48.00000000000000000, -75.00000000000001421 ) ) ;
#85492 = CARTESIAN_POINT ( 'NONE',  ( 60.34209228246672296, -37.37745114556734194, -34.08145293111767415 ) ) ;
#85493 = PRESENTATION_STYLE_ASSIGNMENT (( #28340 ) ) ;
#85494 = CARTESIAN_POINT ( 'NONE',  ( 8.737863883542575039, -3.000000000000003109, -90.03618980370902136 ) ) ;
#85495 = PRODUCT_DEFINITION_SHAPE ( 'NONE', 'NONE',  #105582 ) ;
#85496 = CARTESIAN_POINT ( 'NONE',  ( -61.30040684021128072, -60.00000000000001421, 104.8731119092859529 ) ) ;
#85497 = CARTESIAN_POINT ( 'NONE',  ( -37.46929538816834793, 50.00000000000000000, -55.58823529411764497 ) ) ;
#85498 = CIRCLE ( 'NONE', #35556, 4.172000000000009479 ) ;
#85499 = CARTESIAN_POINT ( 'NONE',  ( -86.74136516792933094, -31.76096988859487169, 186.6536333241581644 ) ) ;
#85500 = ORIENTED_EDGE ( 'NONE', *, *, #65697, .F. ) ;
#85501 = CARTESIAN_POINT ( 'NONE',  ( 34.83349330513380693, 4.000000000000003553, 0.000000000000000000 ) ) ;
#85502 = CARTESIAN_POINT ( 'NONE',  ( -5.016449219528405834, -29.03096582929385505, 28.71858016739311381 ) ) ;
#85503 = AXIS2_PLACEMENT_3D ( 'NONE', #9348, #90290, #74621 ) ;
#85504 = CARTESIAN_POINT ( 'NONE',  ( -5.767825830945890964, 42.00032026480481306, -59.73203846925512295 ) ) ;
#85505 = LINE ( 'NONE', #78460, #92532 ) ;
#85507 = CARTESIAN_POINT ( 'NONE',  ( 7.000000000000000000, 0.000000000000000000, -9.975036109638290682 ) ) ;
#85506 = CARTESIAN_POINT ( 'NONE',  ( -30.64820813098222985, 298.3937798550618936, 2.720202561658572105 ) ) ;
#85508 = EDGE_CURVE ( 'NONE', #96901, #91513, #734, .T. ) ;
#85509 = VERTEX_POINT ( 'NONE', #64325 ) ;
#85510 = CARTESIAN_POINT ( 'NONE',  ( -36.64823341582351901, 437.5392299810053487, 4.281405873620232505 ) ) ;
#85511 = CARTESIAN_POINT ( 'NONE',  ( 19.29515645702225868, 1.482358050883964840E-15, 0.000000000000000000 ) ) ;
#85512 =( LENGTH_UNIT ( ) NAMED_UNIT ( * ) SI_UNIT ( .MILLI., .METRE. ) );
#85513 = LINE ( 'NONE', #44521, #58491 ) ;
#85514 = EDGE_LOOP ( 'NONE', ( #89842, #102817, #3038, #5305, #98954, #47601 ) ) ;
#85515 = CARTESIAN_POINT ( 'NONE',  ( 27.33779175179976662, 296.2809847081317685, -9.691540634816723454 ) ) ;
#85516 = CARTESIAN_POINT ( 'NONE',  ( 35.56416567029047116, 496.2909070316903239, -10.19064917708978335 ) ) ;
#85517 = EDGE_CURVE ( 'NONE', #38940, #29831, #16852, .T. ) ;
#85518 = DIRECTION ( 'NONE',  ( -1.000000000000000000, -1.224606353822377258E-16, -0.000000000000000000 ) ) ;
#85519 = CARTESIAN_POINT ( 'NONE',  ( 19.86162800728184763, 303.8052307878185729, 8.927100233615687941 ) ) ;
#85520 = CARTESIAN_POINT ( 'NONE',  ( 94.33250250775739687, -60.00000000000007105, 18.12814013139226077 ) ) ;
#85521 = CARTESIAN_POINT ( 'NONE',  ( -82.11053578525284991, -36.02907692299217501, 156.5644557899646543 ) ) ;
#85522 = VERTEX_POINT ( 'NONE', #95105 ) ;
#85523 = CARTESIAN_POINT ( 'NONE',  ( 43.09948196127323428, 484.9577458347781089, -0.8563396247083570056 ) ) ;
#85524 = CARTESIAN_POINT ( 'NONE',  ( 4.815811321232740916, 251.8007670769736990, 3.581116321197037156 ) ) ;
#85525 = DIRECTION ( 'NONE',  ( 0.000000000000000000, 0.000000000000000000, -1.000000000000000000 ) ) ;
#85526 = CARTESIAN_POINT ( 'NONE',  ( 35.15748201403830109, 323.3744436496217531, -4.986382573361860082 ) ) ;
#85527 = CARTESIAN_POINT ( 'NONE',  ( 38.86575227086510154, 477.1840224093098186, -1.710886565985892505 ) ) ;
#85528 = EDGE_LOOP ( 'NONE', ( #38731, #2457 ) ) ;
#85530 = VECTOR ( 'NONE', #25795, 999.9999999999998863 ) ;
#85529 = B_SPLINE_CURVE_WITH_KNOTS ( 'NONE', 3,
 ( #14901, #29042, #20949, #103921, #62425, #38173, #22517, #13311, #30069, #12782, #94802, #96389, #47796, #71548, #70512 ),
 .UNSPECIFIED., .F., .F.,
 ( 4, 1, 1, 1, 1, 1, 1, 1, 2, 2, 4 ),
 ( 0.000000000000000000, 0.2500000000003557155, 0.3750000000005364043, 0.4375000000006320500, 0.4687500000006805667, 0.4843750000006981082, 0.4921875000007118750, 0.4960937500007114864, 0.4980468750007052692, 0.5000000000006989964, 1.000000000000000000 ),
 .UNSPECIFIED. ) ;
#85531 = CARTESIAN_POINT ( 'NONE',  ( -18.41162169223098033, 304.6294254666754568, 9.889731659030220001 ) ) ;
#85532 = EDGE_CURVE ( 'NONE', #66358, #30441, #35306, .T. ) ;
#85533 = CYLINDRICAL_SURFACE ( 'NONE', #43256, 5.000000000000000888 ) ;
#85534 = CARTESIAN_POINT ( 'NONE',  ( 4.401442555609581635E-16, -26.28125000204838813, -7.188101187500000044 ) ) ;
#85535 = EDGE_LOOP ( 'NONE', ( #41198, #30860, #99619, #43601, #36873 ) ) ;
#85536 = CARTESIAN_POINT ( 'NONE',  ( 13.50000000000000178, 0.000000000000000000, 0.000000000000000000 ) ) ;
#85537 = CARTESIAN_POINT ( 'NONE',  ( 5.788218731899625880, 41.97741539037772895, -69.85767741758428429 ) ) ;
#85538 = CONICAL_SURFACE ( 'NONE', #1090, 3.400000000000000355, 0.9599310885968748153 ) ;
#85539 = CARTESIAN_POINT ( 'NONE',  ( 63.25915952246698026, 50.00000000000000000, 0.7870165385177050332 ) ) ;
#85540 = CARTESIAN_POINT ( 'NONE',  ( -4.551587301587304957, -1.200583151104947843, 104.4018401814738155 ) ) ;
#85541 = FACE_OUTER_BOUND ( 'NONE', #8953, .T. ) ;
#85542 = ORIENTED_EDGE ( 'NONE', *, *, #77201, .T. ) ;
#85543 = CARTESIAN_POINT ( 'NONE',  ( 52.47548216836918300, -60.00000000000000000, -37.40658969025393787 ) ) ;
#85544 = COLOUR_RGB ( '', 0.08235294, 0.09019608, 0.10196078) ;
#85546 = CARTESIAN_POINT ( 'NONE',  ( 19.99411887364738050, -32.51301298576517240, 29.81229016983529689 ) ) ;
#85545 = CARTESIAN_POINT ( 'NONE',  ( -37.39630343064651186, -60.00000000000003553, 52.44675545814470041 ) ) ;
#85547 = CARTESIAN_POINT ( 'NONE',  ( 4.798419095149803646E-15, 57.18445727710329862, -19.59103268995865221 ) ) ;
#85548 = CARTESIAN_POINT ( 'NONE',  ( -34.03134722860705352, -49.90169853283954637, 36.80301113731194107 ) ) ;
#85549 = B_SPLINE_CURVE_WITH_KNOTS ( 'NONE', 3,
 ( #8067, #83960, #24295, #44039, #75870, #52646, #52117, #59705, #101216, #76390 ),
 .UNSPECIFIED., .F., .F.,
 ( 4, 2, 2, 2, 4 ),
 ( 1.498769063644528192E-28, 0.009926681031335791300, 0.01489002154700368868, 0.01737169180483764605, 0.01985336206267160342 ),
 .UNSPECIFIED. ) ;
#85550 = UNCERTAINTY_MEASURE_WITH_UNIT (LENGTH_MEASURE( 1.000000000000000082E-05 ), #100301, 'distance_accuracy_value', 'NONE');
#85551 = ORIENTED_EDGE ( 'NONE', *, *, #78889, .F. ) ;
#85552 = AXIS2_PLACEMENT_3D ( 'NONE', #41903, #68321, #101215 ) ;
#85553 = DIRECTION ( 'NONE',  ( -1.000000000000000000, -1.224606353822377258E-16, -0.000000000000000000 ) ) ;
#85554 = AXIS2_PLACEMENT_3D ( 'NONE', #70619, #102986, #94913 ) ;
#85555 = DIRECTION ( 'NONE',  ( 0.000000000000000000, 0.000000000000000000, -1.000000000000000000 ) ) ;
#85556 = CARTESIAN_POINT ( 'NONE',  ( -43.41041896072598405, 463.0441421612069917, 5.626145547246294676 ) ) ;
#85557 = AXIS2_PLACEMENT_3D ( 'NONE', #55940, #23104, #64609 ) ;
#85558 = CIRCLE ( 'NONE', #83839, 5.000000000000001776 ) ;
#85559 = PRESENTATION_STYLE_ASSIGNMENT (( #26811 ) ) ;
#85560 = CARTESIAN_POINT ( 'NONE',  ( 7.002641335706726977, -63.94912737319169338, 3.868676264653295949 ) ) ;
#85561 = CARTESIAN_POINT ( 'NONE',  ( 11.96163940603816123, -2.124851113821345727, 20.65895591259675612 ) ) ;
#85562 = ORIENTED_EDGE ( 'NONE', *, *, #45758, .T. ) ;
#85563 = FACE_OUTER_BOUND ( 'NONE', #361, .T. ) ;
#85564 = CARTESIAN_POINT ( 'NONE',  ( 18.91791044776121211, 45.90000000000000568, 62.18611311450882795 ) ) ;
#85565 = ORIENTED_EDGE ( 'NONE', *, *, #101208, .F. ) ;
#85566 = CARTESIAN_POINT ( 'NONE',  ( 91.51003720985690393, -29.99999999999987921, 190.7004568425288653 ) ) ;
#85567 = CARTESIAN_POINT ( 'NONE',  ( 23.97397358239886600, 41.62137230726112591, -74.34129542729060347 ) ) ;
#85568 = AXIS2_PLACEMENT_3D ( 'NONE', #5254, #12268, #94811 ) ;
#85569 = DIRECTION ( 'NONE',  ( 0.000000000000000000, -1.000000000000000000, 0.000000000000000000 ) ) ;
#85570 = MECHANICAL_DESIGN_GEOMETRIC_PRESENTATION_REPRESENTATION (  '', ( #73435 ), #99300 ) ;
#85571 = CARTESIAN_POINT ( 'NONE',  ( 76.82090249591115594, -29.99999999999999645, -16.77916451698828482 ) ) ;
#85572 = CARTESIAN_POINT ( 'NONE',  ( -28.53018783420407445, 313.9245910824191697, 12.38472899747105949 ) ) ;
#85573 = EDGE_LOOP ( 'NONE', ( #67904, #7458, #72061, #78003 ) ) ;
#85574 = EDGE_CURVE ( 'NONE', #86580, #63501, #104344, .T. ) ;
#85575 = ORIENTED_EDGE ( 'NONE', *, *, #11698, .T. ) ;
#85576 = ORIENTED_EDGE ( 'NONE', *, *, #95625, .F. ) ;
#85577 = CARTESIAN_POINT ( 'NONE',  ( -47.07447497471051889, 13.47837589781632417, -14.79567547011589923 ) ) ;
#85578 = DIRECTION ( 'NONE',  ( -0.000000000000000000, -0.000000000000000000, -1.000000000000000000 ) ) ;
#85579 = CARTESIAN_POINT ( 'NONE',  ( 8.000000000000000000, -15.49999999999999289, 0.000000000000000000 ) ) ;
#85580 = CARTESIAN_POINT ( 'NONE',  ( 4.496882872040836254, -10.53788665489624776, 3.972797206970396733 ) ) ;
#85581 = CARTESIAN_POINT ( 'NONE',  ( -16.64348903516521005, 43.47556584774768140, -6.657797401561535544 ) ) ;
#85582 = CYLINDRICAL_SURFACE ( 'NONE', #40721, 4.000000000000000000 ) ;
#85584 = EDGE_CURVE ( 'NONE', #10582, #105650, #57256, .T. ) ;
#85583 = CARTESIAN_POINT ( 'NONE',  ( 23.99113157954623432, 50.00000000000000000, -74.11764705887551941 ) ) ;
#85585 = EDGE_LOOP ( 'NONE', ( #74822, #102933, #14370, #92462, #18134 ) ) ;
#85586 = EDGE_LOOP ( 'NONE', ( #100991, #15586, #75888, #30923, #43234, #81242 ) ) ;
#85587 = CARTESIAN_POINT ( 'NONE',  ( -5.646888413699860720, -61.55025844029609772, 2.040714635159920576 ) ) ;
#85588 = CARTESIAN_POINT ( 'NONE',  ( 6.400000000000000355, 4.618802153517003184, -8.000000000000000000 ) ) ;
#85589 = DIRECTION ( 'NONE',  ( 1.000000000000000000, 0.000000000000000000, 0.000000000000000000 ) ) ;
#85590 = CARTESIAN_POINT ( 'NONE',  ( 24.36825887693873227, 295.5443735985305125, 10.08561002281235197 ) ) ;
#85591 = AXIS2_PLACEMENT_3D ( 'NONE', #2323, #35811, #86481 ) ;
#85592 = CARTESIAN_POINT ( 'NONE',  ( -4.472135954999577834, 249.7258814900167181, -4.000000000000002665 ) ) ;
#85593 = EDGE_LOOP ( 'NONE', ( #65049, #45843, #17260, #104506, #19548 ) ) ;
#85594 = CARTESIAN_POINT ( 'NONE',  ( 104.0908829527487711, -5.000000000000000888, 6.123233995736779101E-16 ) ) ;
#85595 = PRESENTATION_LAYER_ASSIGNMENT (  '', '', ( #37339 ) ) ;
#85596 = DIRECTION ( 'NONE',  ( -1.000000000000000000, -1.224606353822377258E-16, -0.000000000000000000 ) ) ;
#85597 = CARTESIAN_POINT ( 'NONE',  ( -8.559508646656389885, -1.200000000000000030E-05, -4.031152949374503081 ) ) ;
#85598 = CARTESIAN_POINT ( 'NONE',  ( -4.250000000000000000, 5.204748896376250699E-16, -4.814498510800145681 ) ) ;
#85599 = EDGE_CURVE ( 'NONE', #83606, #102396, #31961, .T. ) ;
#85600 = ORIENTED_EDGE ( 'NONE', *, *, #40940, .T. ) ;
#85602 = SURFACE_SIDE_STYLE ('',( #5582 ) ) ;
#85601 =( LENGTH_UNIT ( ) NAMED_UNIT ( * ) SI_UNIT ( .MILLI., .METRE. ) );
#85603 = CARTESIAN_POINT ( 'NONE',  ( 0.000000000000000000, 3.000000000000002665, 0.000000000000000000 ) ) ;
#85604 = CARTESIAN_POINT ( 'NONE',  ( 0.2595206531158521512, 2.531175536751809396, 6.499999999999995559 ) ) ;
#85605 =( NAMED_UNIT ( * ) PLANE_ANGLE_UNIT ( ) SI_UNIT ( $, .RADIAN. ) );
#85606 = CARTESIAN_POINT ( 'NONE',  ( 2.627664075538336252, 302.8385117092220185, 9.934221049389936553 ) ) ;
#85607 = CARTESIAN_POINT ( 'NONE',  ( 23.09999999999999432, -3.309499999999999886, 0.000000000000000000 ) ) ;
#85608 = LINE ( 'NONE', #86678, #17531 ) ;
#85609 = CARTESIAN_POINT ( 'NONE',  ( 86.53304295523901146, -28.12513539782037952, 185.0945772042086048 ) ) ;
#85610 = CARTESIAN_POINT ( 'NONE',  ( -5.293142421612902382, 18.41054814049272892, -37.78857195590732942 ) ) ;
#85611 = CARTESIAN_POINT ( 'NONE',  ( -8.420453562213536358, 123.3148673108814819, 0.000000000000000000 ) ) ;
#85612 = ORIENTED_EDGE ( 'NONE', *, *, #91290, .T. ) ;
#85613 = DIRECTION ( 'NONE',  ( 0.000000000000000000, -0.8660254037844381525, -0.5000000000000008882 ) ) ;
#85614 = CARTESIAN_POINT ( 'NONE',  ( 13.38905016575103168, -53.47246454263770943, 31.09099597011418226 ) ) ;
#85615 = FACE_OUTER_BOUND ( 'NONE', #106314, .T. ) ;
#85616 = CARTESIAN_POINT ( 'NONE',  ( -82.96469731869161990, -30.00000000000000355, 42.60355304050059289 ) ) ;
#85617 = CIRCLE ( 'NONE', #80418, 4.000000000000001776 ) ;
#85618 = AXIS2_PLACEMENT_3D ( 'NONE', #104323, #54166, #69852 ) ;
#85619 = CARTESIAN_POINT ( 'NONE',  ( 35.16921309548814634, -57.69533892213389947, 49.31795818493156958 ) ) ;
#85621 = DIRECTION ( 'NONE',  ( 0.000000000000000000, -1.000000000000000000, 0.000000000000000000 ) ) ;
#85620 = CARTESIAN_POINT ( 'NONE',  ( 37.02114271195448225, 490.9588991526813970, 12.45652432424409461 ) ) ;
#85622 = CARTESIAN_POINT ( 'NONE',  ( -6.500000000000000888, 0.000000000000000000, 1.734723475976807094E-15 ) ) ;
#85623 = DIRECTION ( 'NONE',  ( 0.000000000000000000, 0.000000000000000000, 1.000000000000000000 ) ) ;
#85624 = CARTESIAN_POINT ( 'NONE',  ( 40.66415791351412423, 490.1350948120814337, 11.30186264364121662 ) ) ;
#85625 = CARTESIAN_POINT ( 'NONE',  ( 7.101747359470936161, -4.047770588429664862, -17.37629258577382885 ) ) ;
#85626 = CARTESIAN_POINT ( 'NONE',  ( 44.10862079528723001, 485.7176850333829634, 3.977867558414246663 ) ) ;
#85627 = TOROIDAL_SURFACE ( 'NONE', #97599, 3.500000000000000000, 0.5000000000000000000 ) ;
#85628 = AXIS2_PLACEMENT_3D ( 'NONE', #91590, #41954, #74840 ) ;
#85629 = VECTOR ( 'NONE', #15060, 1000.000000000000000 ) ;
#85630 = CARTESIAN_POINT ( 'NONE',  ( 64.30247150797818279, -29.69425787713660014, -23.35221998356511364 ) ) ;
#85631 = CARTESIAN_POINT ( 'NONE',  ( -26.75657867810697965, -56.87252330840309611, 35.15284453816919097 ) ) ;
#85632 = CIRCLE ( 'NONE', #71819, 4.000000000000000888 ) ;
#85633 = EDGE_LOOP ( 'NONE', ( #19345, #53951, #62897, #61970, #50046 ) ) ;
#85634 = CARTESIAN_POINT ( 'NONE',  ( 41.31161337382093279, 484.8232235214512684, -3.619187650536324519 ) ) ;
#85635 = CARTESIAN_POINT ( 'NONE',  ( -9.333892298909264085, 106.7827573162503541, -3.590295303293453255 ) ) ;
#85636 = TOROIDAL_SURFACE ( 'NONE', #54560, 12.00000000000000000, 2.000000000000000000 ) ;
#85637 = CARTESIAN_POINT ( 'NONE',  ( -21.41503862012732640, -42.95838455524901178, 31.73348506666451385 ) ) ;
#85639 = CARTESIAN_POINT ( 'NONE',  ( -37.99667718823692297, 439.4681409270056065, 23.88471372786844071 ) ) ;
#85638 = CARTESIAN_POINT ( 'NONE',  ( -0.6447843993400577123, 28.14413779556368667, 38.41621468030491826 ) ) ;
#85640 = ADVANCED_FACE ( 'NONE', ( #34106 ), #45605, .T. ) ;
#85641 = EDGE_LOOP ( 'NONE', ( #20161, #97705, #105620, #87401 ) ) ;
#85642 = DIRECTION ( 'NONE',  ( 0.000000000000000000, -1.000000000000000000, 0.000000000000000000 ) ) ;
#85643 = EDGE_LOOP ( 'NONE', ( #37863, #66757, #86034, #71602, #76916 ) ) ;
#85644 = CARTESIAN_POINT ( 'NONE',  ( 4.046285834744535848, 49.99999999999999289, -97.52808355545833763 ) ) ;
#85645 = ADVANCED_FACE ( 'NONE', ( #589 ), #42295, .T. ) ;
#85646 = SURFACE_STYLE_USAGE ( .BOTH. , #19358 ) ;
#85647 = CARTESIAN_POINT ( 'NONE',  ( 19.83349330513379982, 1.593028355512270567E-15, 0.000000000000000000 ) ) ;
#85648 = VERTEX_POINT ( 'NONE', #16826 ) ;
#85649 = DIRECTION ( 'NONE',  ( 0.000000000000000000, 0.000000000000000000, 1.000000000000000000 ) ) ;
#85650 = CARTESIAN_POINT ( 'NONE',  ( 100.1894145001407708, -37.84390723933621103, 190.2404321465731982 ) ) ;
#85652 = CARTESIAN_POINT ( 'NONE',  ( -6.944031699373469202, -9.465393454438721932, 3.972913591453822502 ) ) ;
#85651 = DIRECTION ( 'NONE',  ( 0.000000000000000000, 0.000000000000000000, 1.000000000000000000 ) ) ;
#85653 = AXIS2_PLACEMENT_3D ( 'NONE', #23736, #41476, #49565 ) ;
#85654 = ORIENTED_EDGE ( 'NONE', *, *, #105400, .T. ) ;
#85655 = EDGE_CURVE ( 'NONE', #9366, #6102, #42107, .T. ) ;
#85656 = ORIENTED_EDGE ( 'NONE', *, *, #102003, .T. ) ;
#85657 = AXIS2_PLACEMENT_3D ( 'NONE', #30664, #64086, #23098 ) ;
#85658 = ORIENTED_EDGE ( 'NONE', *, *, #28865, .F. ) ;
#85659 = CARTESIAN_POINT ( 'NONE',  ( 22.31591624825033549, 305.3790487442428798, 10.05087283592891545 ) ) ;
#85660 = DIRECTION ( 'NONE',  ( 0.000000000000000000, 1.000000000000000000, 0.000000000000000000 ) ) ;
#85661 = CARTESIAN_POINT ( 'NONE',  ( 14.11571568429345724, 5.211159435664195705, -3.514002131771281068 ) ) ;
#85662 = ORIENTED_EDGE ( 'NONE', *, *, #56204, .T. ) ;
#85663 = CARTESIAN_POINT ( 'NONE',  ( 0.4053525175235886957, 3.145852061455926219, -6.500000000000000000 ) ) ;
#85664 = CARTESIAN_POINT ( 'NONE',  ( -5.313746993492887150, 41.99394904787047977, -69.45902141694074317 ) ) ;
#85665 = CARTESIAN_POINT ( 'NONE',  ( -94.48669138886810970, -60.00000000000000000, 3.951815744481825821 ) ) ;
#85666 = CARTESIAN_POINT ( 'NONE',  ( 8.000113193197769590, -69.00022638645862116, -0.2613481123984630061 ) ) ;
#85667 = CARTESIAN_POINT ( 'NONE',  ( 2.841596995776060286, -59.99999999999998579, 39.63907943748999685 ) ) ;
#85668 = CARTESIAN_POINT ( 'NONE',  ( 15.92648127229067612, -5.000000000000000000, 4.023271965934163141 ) ) ;
#85669 = CARTESIAN_POINT ( 'NONE',  ( -12.13034742782427777, 41.99999999999999289, -93.82352941176471006 ) ) ;
#85671 = CARTESIAN_POINT ( 'NONE',  ( 4.129220113709654250, -60.35881339298138926, 33.94144245523071390 ) ) ;
#85670 = CARTESIAN_POINT ( 'NONE',  ( -107.0562774193554816, -30.00000000000000355, 141.2195909136805767 ) ) ;
#85672 = CIRCLE ( 'NONE', #99406, 4.000000000000000888 ) ;
#85673 = CARTESIAN_POINT ( 'NONE',  ( -48.06896637034827791, -36.06506752110366421, 46.66918921588193570 ) ) ;
#85674 = ORIENTED_EDGE ( 'NONE', *, *, #90096, .F. ) ;
#85675 = CARTESIAN_POINT ( 'NONE',  ( -3.999999999999999112, 18.12277735230508213, 5.744562646538041051 ) ) ;
#85676 = EDGE_LOOP ( 'NONE', ( #16650, #25409, #60274, #33387, #54700, #60921, #58067, #72185 ) ) ;
#85677 = CARTESIAN_POINT ( 'NONE',  ( 35.47319904751531539, 436.4618060951635243, 5.062631899564591365 ) ) ;
#85678 = AXIS2_PLACEMENT_3D ( 'NONE', #67831, #65709, #74838 ) ;
#85679 = LINE ( 'NONE', #18294, #28873 ) ;
#85680 = CARTESIAN_POINT ( 'NONE',  ( 6.326195795702134639, 1.326139502404688697, 6.831522767507085980 ) ) ;
#85681 = ORIENTED_EDGE ( 'NONE', *, *, #92646, .F. ) ;
#85682 = CARTESIAN_POINT ( 'NONE',  ( 97.73333333333333428, 1.023464760207051730E-14, 0.000000000000000000 ) ) ;
#85683 = AXIS2_PLACEMENT_3D ( 'NONE', #82925, #898, #16597 ) ;
#85684 = EDGE_LOOP ( 'NONE', ( #55894, #46128, #53140, #76740 ) ) ;
#85685 = CARTESIAN_POINT ( 'NONE',  ( 103.9415641081996569, -29.99999999993293187, 120.1036003625780069 ) ) ;
#85686 = SURFACE_STYLE_USAGE ( .BOTH. , #105949 ) ;
#85687 = CARTESIAN_POINT ( 'NONE',  ( 6.678340154126256145, 41.85887555562482021, -59.41504759784768908 ) ) ;
#85688 = CARTESIAN_POINT ( 'NONE',  ( -1.905220702120325443E-14, 42.00000000000000711, -59.23741894013591036 ) ) ;
#85689 = CARTESIAN_POINT ( 'NONE',  ( 100.4127377726602219, -30.00000000000000000, 183.4147967980347858 ) ) ;
#85690 = CARTESIAN_POINT ( 'NONE',  ( 0.000000000000000000, 50.00000000000000000, 0.000000000000000000 ) ) ;
#85691 = ORIENTED_EDGE ( 'NONE', *, *, #35361, .F. ) ;
#85692 = EDGE_CURVE ( 'NONE', #99989, #50441, #77723, .T. ) ;
#85693 = B_SPLINE_CURVE_WITH_KNOTS ( 'NONE', 3,
 ( #3766, #46342, #4819, #21051, #38278, #4288, #37215, #22085 ),
 .UNSPECIFIED., .F., .F.,
 ( 4, 2, 2, 4 ),
 ( 5.204170427930421283E-18, 0.005696202229710471167, 0.008544303344565708919, 0.01139240445942094754 ),
 .UNSPECIFIED. ) ;
#85694 = ORIENTED_EDGE ( 'NONE', *, *, #46317, .F. ) ;
#85695 = ORIENTED_EDGE ( 'NONE', *, *, #78610, .T. ) ;
#85696 = CARTESIAN_POINT ( 'NONE',  ( 54.81643864070908734, -39.49759617041522830, 59.89540365714804437 ) ) ;
#85697 = AXIS2_PLACEMENT_3D ( 'NONE', #34734, #67605, #94412 ) ;
#85698 = CARTESIAN_POINT ( 'NONE',  ( 7.070595415630159586, 41.16321656043108135, -58.51508817460690182 ) ) ;
#85699 = CIRCLE ( 'NONE', #39189, 5.000000000000001776 ) ;
#85700 = CARTESIAN_POINT ( 'NONE',  ( 11.89131030317610183, 6.123233995736772199E-16, -5.000000000000001776 ) ) ;
#85701 = EDGE_CURVE ( 'NONE', #38733, #42532, #102412, .T. ) ;
#85702 = ADVANCED_FACE ( 'NONE', ( #100916 ), #76598, .F. ) ;
#85703 = ORIENTED_EDGE ( 'NONE', *, *, #39167, .T. ) ;
#85704 = CARTESIAN_POINT ( 'NONE',  ( -91.45944082887925219, -38.38696142436580061, -7.377240623632893346 ) ) ;
#85705 = VERTEX_POINT ( 'NONE', #20060 ) ;
#85706 = CARTESIAN_POINT ( 'NONE',  ( 110.9829524794310487, -38.35607303365373610, 174.7672866423136497 ) ) ;
#85707 = CARTESIAN_POINT ( 'NONE',  ( 10.61645511433041911, 13.94409384998177792, 9.960230482081710690 ) ) ;
#85709 = CARTESIAN_POINT ( 'NONE',  ( 82.48695905097841319, -37.86100049745743235, 8.080848905333057886 ) ) ;
#85708 = COLOUR_RGB ( '', 0.66274510, 0.83137255, 0.94901961) ;
#85710 = PRESENTATION_LAYER_ASSIGNMENT (  '', '', ( #61615 ) ) ;
#85711 = CIRCLE ( 'NONE', #40947, 7.000000000000000000 ) ;
#85712 = DIRECTION ( 'NONE',  ( 0.000000000000000000, -0.000000000000000000, 1.000000000000000000 ) ) ;
#85713 = STYLED_ITEM ( 'NONE', ( #47573 ), #38054 ) ;
#85714 = CARTESIAN_POINT ( 'NONE',  ( 4.524610880511400701, -11.34578236400706430, -9.835134842095726526 ) ) ;
#85715 = CARTESIAN_POINT ( 'NONE',  ( -24.35720706066873475, 25.22454029369766104, -32.47622240156568552 ) ) ;
#85716 = CARTESIAN_POINT ( 'NONE',  ( -19.50000000000000000, 12.99999999999999289, 0.000000000000000000 ) ) ;
#85717 = CARTESIAN_POINT ( 'NONE',  ( 3.996301576410518308, 136.8773085153401894, 5.000000000000000888 ) ) ;
#85718 = CIRCLE ( 'NONE', #68462, 3.400000000000000355 ) ;
#85719 = ORIENTED_EDGE ( 'NONE', *, *, #14219, .F. ) ;
#85720 = CARTESIAN_POINT ( 'NONE',  ( -16.14595037822616419, 12.99999999999999289, 0.000000000000000000 ) ) ;
#85721 = EDGE_CURVE ( 'NONE', #88346, #34066, #85276, .T. ) ;
#85722 = DIRECTION ( 'NONE',  ( -0.000000000000000000, -0.000000000000000000, -1.000000000000000000 ) ) ;
#85723 = DIRECTION ( 'NONE',  ( -1.000000000000000000, -0.000000000000000000, -0.000000000000000000 ) ) ;
#85724 = VERTEX_POINT ( 'NONE', #100389 ) ;
#85725 = AXIS2_PLACEMENT_3D ( 'NONE', #32435, #73372, #66360 ) ;
#85726 = DIRECTION ( 'NONE',  ( -1.000000000000000000, -1.224606353822377258E-16, -0.000000000000000000 ) ) ;
#85727 = CARTESIAN_POINT ( 'NONE',  ( -30.50310125412890372, 318.9373365299751981, 13.88874147237046763 ) ) ;
#85728 = CARTESIAN_POINT ( 'NONE',  ( 1.295095875561511761E-05, -30.00000000000000000, 37.00000000000000711 ) ) ;
#85729 = CARTESIAN_POINT ( 'NONE',  ( -14.75116205827941940, 43.55504283738518723, -90.22050498381219086 ) ) ;
#85730 = CARTESIAN_POINT ( 'NONE',  ( 5.656854249492380582, -21.31249999999999289, -5.656854249492379694 ) ) ;
#85731 = CARTESIAN_POINT ( 'NONE',  ( 5.618858407243280340, -12.94760482173810878, 32.08621218712340806 ) ) ;
#85732 = EDGE_CURVE ( 'NONE', #104354, #71702, #92827, .T. ) ;
#85733 = CIRCLE ( 'NONE', #23678, 4.000000000000000888 ) ;
#85734 = DIRECTION ( 'NONE',  ( 0.000000000000000000, -1.000000000000000000, 0.000000000000000000 ) ) ;
#85735 = ORIENTED_EDGE ( 'NONE', *, *, #51829, .T. ) ;
#85736 = CARTESIAN_POINT ( 'NONE',  ( 83.34476608070126247, -57.33726856256456728, 189.3581896335610111 ) ) ;
#85737 = EDGE_CURVE ( 'NONE', #97120, #65472, #28334, .T. ) ;
#85738 = AXIS2_PLACEMENT_3D ( 'NONE', #20983, #53816, #12819 ) ;
#85739 = B_SPLINE_CURVE_WITH_KNOTS ( 'NONE', 3,
 ( #100186, #66766, #86032, #36956, #16613, #99652, #99106, #25823, #18232, #9039 ),
 .UNSPECIFIED., .F., .F.,
 ( 4, 2, 2, 2, 4 ),
 ( 0.000000000000000000, 0.5000000000000000000, 0.7500000000000000000, 0.8750000000000000000, 1.000000000000000000 ),
 .UNSPECIFIED. ) ;
#85740 = DIRECTION ( 'NONE',  ( 0.000000000000000000, -1.000000000000000000, 0.000000000000000000 ) ) ;
#85741 = ORIENTED_EDGE ( 'NONE', *, *, #55180, .F. ) ;
#85742 = CARTESIAN_POINT ( 'NONE',  ( -87.58810446347557388, -37.82077815364313267, 63.64187444496401014 ) ) ;
#85743 = DIRECTION ( 'NONE',  ( -1.000000000000000000, -1.224606353822377258E-16, -0.000000000000000000 ) ) ;
#85744 = CARTESIAN_POINT ( 'NONE',  ( -15.17227823171696954, -5.000000000000002665, -86.54073391196325815 ) ) ;
#85745 = CARTESIAN_POINT ( 'NONE',  ( 12.49986889690059222, -3.000000000000002665, -76.70852482682694529 ) ) ;
#85746 = AXIS2_PLACEMENT_3D ( 'NONE', #67997, #34604, #1094 ) ;
#85747 = CARTESIAN_POINT ( 'NONE',  ( -4.121118778969612428, -21.54458145684739634, -38.54885555910615125 ) ) ;
#85748 =( NAMED_UNIT ( * ) SI_UNIT ( $, .STERADIAN. ) SOLID_ANGLE_UNIT ( ) );
#85749 = CARTESIAN_POINT ( 'NONE',  ( 21.93441337368819077, -59.99999999999999289, 40.50886425770784172 ) ) ;
#85750 = CARTESIAN_POINT ( 'NONE',  ( 20.11650669486618881, 4.000000000000003553, 4.898587196589414801E-16 ) ) ;
#85751 = CARTESIAN_POINT ( 'NONE',  ( 2.705399370281793114, -0.5466957599951438596, 103.4497616813456204 ) ) ;
#85752 = CARTESIAN_POINT ( 'NONE',  ( 46.00628356782431894, -28.63590054676348728, 41.16915987473818461 ) ) ;
#85753 = AXIS2_PLACEMENT_3D ( 'NONE', #35561, #68436, #94306 ) ;
#85755 = CARTESIAN_POINT ( 'NONE',  ( -13.23614406034744917, 22.05544707748403255, 4.271605316804893526 ) ) ;
#85754 = CARTESIAN_POINT ( 'NONE',  ( -31.50084319533580413, -33.43140129536075023, 41.49735270624054806 ) ) ;
#85756 = CARTESIAN_POINT ( 'NONE',  ( 1.050160786911071398, 296.8373249698643122, -10.00076906402473043 ) ) ;
#85757 = CARTESIAN_POINT ( 'NONE',  ( 43.74855578046756222, 328.6220886837048170, -1.765109843966993441 ) ) ;
#85758 = CARTESIAN_POINT ( 'NONE',  ( 43.35947070037873630, 356.1039901738380991, 11.86182662173998814 ) ) ;
#85759 = CARTESIAN_POINT ( 'NONE',  ( 67.22793774957824553, -4.000000000000000000, 4.898587196589421703E-16 ) ) ;
#85760 = ORIENTED_EDGE ( 'NONE', *, *, #26631, .T. ) ;
#85761 = CARTESIAN_POINT ( 'NONE',  ( 3.811597179862330709, -5.304926841629225898, -0.01956314070070098651 ) ) ;
#85762 = CIRCLE ( 'NONE', #49538, 4.000000000000000888 ) ;
#85763 = ORIENTED_EDGE ( 'NONE', *, *, #19278, .T. ) ;
#85764 = CARTESIAN_POINT ( 'NONE',  ( -13.08498522490498495, 1.516837759881986880, 14.92390867749982064 ) ) ;
#85765 = DIRECTION ( 'NONE',  ( 0.000000000000000000, 0.000000000000000000, 1.000000000000000000 ) ) ;
#85766 = CARTESIAN_POINT ( 'NONE',  ( -1.469576158976823947E-15, -29.56250000409677270, 8.000000000000000000 ) ) ;
#85768 = CARTESIAN_POINT ( 'NONE',  ( -22.67421649284328566, -60.22830675361940678, -35.89770680791995972 ) ) ;
#85767 = DIRECTION ( 'NONE',  ( 0.000000000000000000, 0.000000000000000000, -1.000000000000000000 ) ) ;
#85769 = EDGE_CURVE ( 'NONE', #29611, #11941, #88868, .T. ) ;
#85770 = ORIENTED_EDGE ( 'NONE', *, *, #45394, .T. ) ;
#85771 = CARTESIAN_POINT ( 'NONE',  ( 3.857142857142850101, -48.79941684889506348, 103.1763305333244176 ) ) ;
#85772 = CARTESIAN_POINT ( 'NONE',  ( -3.999994092537668244, -10.00072617203139380, 6.928206640937045080 ) ) ;
#85773 = CIRCLE ( 'NONE', #30730, 3.500000000000000000 ) ;
#85774 = AXIS2_PLACEMENT_3D ( 'NONE', #36207, #60983, #12929 ) ;
#85775 = EDGE_LOOP ( 'NONE', ( #25306, #80757, #60943, #8116, #14104 ) ) ;
#85776 = EDGE_CURVE ( 'NONE', #106205, #82529, #65716, .T. ) ;
#85777 = ADVANCED_FACE ( 'NONE', ( #50565 ), #90389, .T. ) ;
#85778 = CARTESIAN_POINT ( 'NONE',  ( 80.00000000000000000, -60.00000000000000000, -19.09707704303353282 ) ) ;
#85779 = CARTESIAN_POINT ( 'NONE',  ( 0.000000000000000000, 0.000000000000000000, 4.000000000000000000 ) ) ;
#85780 = CARTESIAN_POINT ( 'NONE',  ( -92.23326038059701659, -60.00000000000000711, 2.433354083156913816 ) ) ;
#85781 = ORIENTED_EDGE ( 'NONE', *, *, #46140, .T. ) ;
#85782 =( LENGTH_UNIT ( ) NAMED_UNIT ( * ) SI_UNIT ( .MILLI., .METRE. ) );
#85783 = DIRECTION ( 'NONE',  ( 0.000000000000000000, -1.000000000000000000, 0.000000000000000000 ) ) ;
#85784 = CIRCLE ( 'NONE', #1348, 3.309500000000001663 ) ;
#85785 = CARTESIAN_POINT ( 'NONE',  ( 7.439138809193584834, 41.00331669213974806, -59.84461289586582922 ) ) ;
#85786 = DIRECTION ( 'NONE',  ( -1.000000000000000000, -0.000000000000000000, -0.000000000000000000 ) ) ;
#85788 = DIRECTION ( 'NONE',  ( -0.3573389821873162453, -0.9339747597281914393, 0.000000000000000000 ) ) ;
#85787 = DIRECTION ( 'NONE',  ( -0.000000000000000000, -0.000000000000000000, -1.000000000000000000 ) ) ;
#85789 = CARTESIAN_POINT ( 'NONE',  ( -81.74441236244950915, -46.45436576172757270, 169.1830579053890347 ) ) ;
#85790 = VERTEX_POINT ( 'NONE', #73791 ) ;
#85791 = CARTESIAN_POINT ( 'NONE',  ( -13.52495681779062764, -0.000000000000000000, 10.38447319518036238 ) ) ;
#85792 = EDGE_CURVE ( 'NONE', #90051, #56071, #45143, .T. ) ;
#85793 = ORIENTED_EDGE ( 'NONE', *, *, #35676, .F. ) ;
#85794 = EDGE_CURVE ( 'NONE', #78701, #67484, #33472, .T. ) ;
#85795 = ORIENTED_EDGE ( 'NONE', *, *, #5591, .F. ) ;
#85796 = CARTESIAN_POINT ( 'NONE',  ( -9.479859806997659177, -5.000000000000000000, -13.37835090744192001 ) ) ;
#85797 = FACE_OUTER_BOUND ( 'NONE', #8981, .T. ) ;
#85798 = VERTEX_POINT ( 'NONE', #10130 ) ;
#85799 = AXIS2_PLACEMENT_3D ( 'NONE', #81868, #32304, #8525 ) ;
#85800 = FACE_OUTER_BOUND ( 'NONE', #92569, .T. ) ;
#85801 = CARTESIAN_POINT ( 'NONE',  ( -94.01586347659660703, -57.67588051021766660, 5.310313041227479935 ) ) ;
#85802 = CARTESIAN_POINT ( 'NONE',  ( 7.003653396366583905, -11.05706205559678068, -3.866846144092866311 ) ) ;
#85803 = CARTESIAN_POINT ( 'NONE',  ( 5.799999999999999822, 4.618802153517005848, 7.999999999999996447 ) ) ;
#85804 = CARTESIAN_POINT ( 'NONE',  ( -9.918325909156571640, 101.2076476829256819, 1.298699613733151015 ) ) ;
#85805 = CARTESIAN_POINT ( 'NONE',  ( -13.80753398876933247, -50.82042416759918524, 24.67600335260435074 ) ) ;
#85806 = CARTESIAN_POINT ( 'NONE',  ( -17.95946947111402991, 36.59397683629514830, -22.69701383365361380 ) ) ;
#85807 = CARTESIAN_POINT ( 'NONE',  ( 87.68135845022958108, -14.21045842199445275, 32.26523303912966156 ) ) ;
#85808 = CARTESIAN_POINT ( 'NONE',  ( -91.09862910994078788, -14.21045842199425380, 197.8399937059591309 ) ) ;
#85809 = CARTESIAN_POINT ( 'NONE',  ( -55.38459995159444560, -46.44143365808177037, 64.00544807844242712 ) ) ;
#85810 = EDGE_LOOP ( 'NONE', ( #9430, #4377, #41071, #3746 ) ) ;
#85811 = ORIENTED_EDGE ( 'NONE', *, *, #43835, .T. ) ;
#85812 = CARTESIAN_POINT ( 'NONE',  ( -106.5272989890566748, -60.15536930867855858, 172.9214709365080012 ) ) ;
#85813 = CARTESIAN_POINT ( 'NONE',  ( 0.000000000000000000, 0.000000000000000000, -2.716724522925831220 ) ) ;
#85814 = CARTESIAN_POINT ( 'NONE',  ( -15.00099999999999767, 12.99999999999999289, 0.000000000000000000 ) ) ;
#85815 = VECTOR ( 'NONE', #46289, 1000.000000000000000 ) ;
#85816 = ORIENTED_EDGE ( 'NONE', *, *, #86985, .T. ) ;
#85817 = CARTESIAN_POINT ( 'NONE',  ( 5.693345022498909280, -2.999999999999138467, -71.09407784968016131 ) ) ;
#85818 = SURFACE_SIDE_STYLE ('',( #28657 ) ) ;
#85819 = CARTESIAN_POINT ( 'NONE',  ( 36.49026554367495834, 25.91778114966158242, -12.86217455386831432 ) ) ;
#85820 = CARTESIAN_POINT ( 'NONE',  ( 5.082755093536325930, -16.34375000204838813, -5.082755093536325042 ) ) ;
#85821 = DIRECTION ( 'NONE',  ( -0.9508028509851098597, -0.1865215626109695546, 0.2473532802283995025 ) ) ;
#85822 = DIRECTION ( 'NONE',  ( 0.5735764363510468256, 0.8191520442889913545, 0.000000000000000000 ) ) ;
#85823 = CARTESIAN_POINT ( 'NONE',  ( -30.35537264529554946, 338.7115663565144246, 18.05293407820170515 ) ) ;
#85824 = FILL_AREA_STYLE_COLOUR ( '', #100185 ) ;
#85825 =( BOUNDED_SURFACE ( )  B_SPLINE_SURFACE ( 3, 2, ( 
 ( #40278, #55899, #30625 ),
 ( #22001, #6842, #13867 ),
 ( #56443, #23060, #64049 ),
 ( #63513, #96411, #71571 ),
 ( #5785, #87783, #54854 ),
 ( #38707, #22543, #13332 ),
 ( #80724, #46257, #88314 ),
 ( #97434, #103946, #79144 ),
 ( #5270, #14389, #96924 ),
 ( #88834, #39766, #46781 ) ),
 .UNSPECIFIED., .F., .F., .F. ) 
 B_SPLINE_SURFACE_WITH_KNOTS ( ( 4, 2, 2, 2, 4 ),
 ( 3, 3 ),
 ( 0.007162312563338129288, 0.008169815727934513425, 0.009177318892530896693, 0.01018482205712727996, 0.01119232522172366323 ),
 ( 0.1508783416922580001, 1.000000000000000000 ),
 .UNSPECIFIED. ) 
 GEOMETRIC_REPRESENTATION_ITEM ( )  RATIONAL_B_SPLINE_SURFACE ( (
 ( 0.9388230293412898053, 0.7972639082172212621, 1.000000000000000000),
 ( 0.9416444161515592493, 0.8066137816935087246, 1.000000000000000000),
 ( 0.9435088878518229638, 0.8127925071465851303, 1.000000000000000000),
 ( 0.9450395734671753756, 0.8178650894608657795, 1.000000000000000000),
 ( 0.9446996306686668010, 0.8167385434149065926, 1.000000000000000000),
 ( 0.9419800614655553517, 0.8077260861841054629, 1.000000000000000000),
 ( 0.9396107484148550348, 0.7998743527141916054, 1.000000000000000000),
 ( 0.9333151777508156277, 0.7790112831926551129, 1.000000000000000000),
 ( 0.9293941002835721665, 0.7660171137735573010, 1.000000000000000000),
 ( 0.9249525166718545188, 0.7512980243340108277, 1.000000000000000000) ) ) 
 REPRESENTATION_ITEM ( '' )  SURFACE ( )  );
#85826 = CARTESIAN_POINT ( 'NONE',  ( -7.873155740944470793, 63.95458188447780401, 0.000000000000000000 ) ) ;
#85827 = CARTESIAN_POINT ( 'NONE',  ( 37.61650669486618881, -3.999999999999998224, 0.000000000000000000 ) ) ;
#85828 = CARTESIAN_POINT ( 'NONE',  ( 37.20102314025923107, 438.1443282426988617, 4.012575796191242716 ) ) ;
#85829 = UNCERTAINTY_MEASURE_WITH_UNIT (LENGTH_MEASURE( 1.000000000000000082E-05 ), #18046, 'distance_accuracy_value', 'NONE');
#85830 = CARTESIAN_POINT ( 'NONE',  ( -27.77433481921273284, -22.10417860528052714, 29.38320212662867803 ) ) ;
#85831 = DIRECTION ( 'NONE',  ( 0.000000000000000000, 0.000000000000000000, 1.000000000000000000 ) ) ;
#85832 = AXIS2_PLACEMENT_3D ( 'NONE', #72852, #30314, #6004 ) ;
#85833 = CARTESIAN_POINT ( 'NONE',  ( 46.15439516824530841, -18.78259881707839796, 39.23926396323135890 ) ) ;
#85834 = CARTESIAN_POINT ( 'NONE',  ( -32.62376965138169993, 486.1221409277068801, 7.511474791651365557 ) ) ;
#85836 = CIRCLE ( 'NONE', #39319, 8.900000000000000355 ) ;
#85835 = CARTESIAN_POINT ( 'NONE',  ( -7.150053860865851263, 86.78265453913975591, 3.590189269391290239 ) ) ;
#85837 = EDGE_CURVE ( 'NONE', #74331, #35775, #9581, .T. ) ;
#85838 = CARTESIAN_POINT ( 'NONE',  ( -89.89686455004155619, -38.51728769248722983, 200.5441032878415797 ) ) ;
#85839 = VERTEX_POINT ( 'NONE', #400 ) ;
#85840 = CARTESIAN_POINT ( 'NONE',  ( 82.74320640397530724, -38.35695998739068102, -24.68618422736320994 ) ) ;
#85841 = CARTESIAN_POINT ( 'NONE',  ( 15.17271185359085983, 5.249115203880597491, -6.324282847316704981 ) ) ;
#85842 = CARTESIAN_POINT ( 'NONE',  ( -19.16002095161153918, 49.73805339712912144, 61.63562287024812036 ) ) ;
#85843 = FILL_AREA_STYLE_COLOUR ( '', #14343 ) ;
#85844 = CARTESIAN_POINT ( 'NONE',  ( 6.040960808745679422, 41.48433375008082180, -70.81801795692170742 ) ) ;
#85845 = CARTESIAN_POINT ( 'NONE',  ( -32.37479440661866192, 435.2079318469511691, 18.54001184198767760 ) ) ;
#85846 = CARTESIAN_POINT ( 'NONE',  ( 42.09158233638503077, 465.7816406625409513, 14.79318349170028668 ) ) ;
#85847 = CARTESIAN_POINT ( 'NONE',  ( 7.500000000000000000, 2.886751345948123770, -7.198902722707427593 ) ) ;
#85848 = CONICAL_SURFACE ( 'NONE', #72040, 5.000000000000010658, 0.9599310885968697082 ) ;
#85849 = CARTESIAN_POINT ( 'NONE',  ( 104.3686754364753853, -60.00000000000000711, 199.7312357621291596 ) ) ;
#85850 = AXIS2_PLACEMENT_3D ( 'NONE', #25400, #58260, #10754 ) ;
#85851 = B_SPLINE_CURVE_WITH_KNOTS ( 'NONE', 3,
 ( #71473, #21906, #81153, #80622, #14292, #73049 ),
 .UNSPECIFIED., .F., .F.,
 ( 4, 2, 4 ),
 ( 0.02035271886645138514, 0.03148701738111871901, 0.04262131589578604940 ),
 .UNSPECIFIED. ) ;
#85852 = CARTESIAN_POINT ( 'NONE',  ( -7.211357414135266097, -67.01146539934443069, 3.467230644691331687 ) ) ;
#85853 = VERTEX_POINT ( 'NONE', #33367 ) ;
#85854 = CARTESIAN_POINT ( 'NONE',  ( 35.07439070120019409, 437.8544070495369738, 4.397851634058062231 ) ) ;
#85855 = CARTESIAN_POINT ( 'NONE',  ( -79.59097844331863314, -29.99999999999999289, -14.32855134736868585 ) ) ;
#85856 = ORIENTED_EDGE ( 'NONE', *, *, #51143, .T. ) ;
#85858 = CARTESIAN_POINT ( 'NONE',  ( 5.254776564415823081, 11.34081578130501811, -31.40351826358976695 ) ) ;
#85857 = CARTESIAN_POINT ( 'NONE',  ( -70.02821094524227874, -38.33024996013831043, 134.5064181467811295 ) ) ;
#85859 = DIRECTION ( 'NONE',  ( 1.224646799147353454E-16, 0.000000000000000000, -1.000000000000000000 ) ) ;
#85860 = CARTESIAN_POINT ( 'NONE',  ( 6.902527771671632451, 4.675077770780898589, -0.7026937717022772034 ) ) ;
#85861 = LINE ( 'NONE', #92319, #2419 ) ;
#85862 = STYLED_ITEM ( 'NONE', ( #89770 ), #61133 ) ;
#85863 = CARTESIAN_POINT ( 'NONE',  ( -7.188101187500002709, -12.68750000204838635, 2.977408999572648707 ) ) ;
#85864 = AXIS2_PLACEMENT_3D ( 'NONE', #6699, #95724, #31546 ) ;
#85865 = DIRECTION ( 'NONE',  ( -0.5735764363510497121, 0.8191520442889892450, 1.003171929053521665E-16 ) ) ;
#85866 = AXIS2_PLACEMENT_3D ( 'NONE', #78783, #4374, #53969 ) ;
#85867 = CARTESIAN_POINT ( 'NONE',  ( 30.75723595955470557, 13.12755156482208108, -41.50738620754143682 ) ) ;
#85869 = EDGE_LOOP ( 'NONE', ( #82877, #25592, #97098, #10423 ) ) ;
#85868 = CARTESIAN_POINT ( 'NONE',  ( 8.866506694866188809, 1.474610560812782335E-15, 0.000000000000000000 ) ) ;
#85870 = CARTESIAN_POINT ( 'NONE',  ( 82.94047458007501916, -42.97468312252637190, 174.7032502363410629 ) ) ;
#85871 = EDGE_CURVE ( 'NONE', #12410, #32853, #54069, .T. ) ;
#85872 = CARTESIAN_POINT ( 'NONE',  ( 5.385673916453011856, 0.000000000000000000, 18.57417562100670949 ) ) ;
#85873 = CARTESIAN_POINT ( 'NONE',  ( 6.818286579240214529, -1.325012739682879692, -6.208253321455268647 ) ) ;
#85874 = ORIENTED_EDGE ( 'NONE', *, *, #13852, .F. ) ;
#85875 = CARTESIAN_POINT ( 'NONE',  ( -32.90753060623204362, 485.1134061475200951, 5.490696813865477921 ) ) ;
#85876 = FILL_AREA_STYLE ('',( #52948 ) ) ;
#85877 = CARTESIAN_POINT ( 'NONE',  ( 3.313708498984742512, -28.71874999999999289, -8.000000000000019540 ) ) ;
#85878 = CARTESIAN_POINT ( 'NONE',  ( 82.42421628608209971, 6.123233995736568081E-16, -5.000000000000011546 ) ) ;
#85879 =( LENGTH_UNIT ( ) NAMED_UNIT ( * ) SI_UNIT ( .MILLI., .METRE. ) );
#85880 = CARTESIAN_POINT ( 'NONE',  ( 17.86498552253326366, 43.17254421777826678, 5.722207910555678900 ) ) ;
#85881 = DIRECTION ( 'NONE',  ( 0.000000000000000000, -1.000000000000000000, 0.000000000000000000 ) ) ;
#85882 = VERTEX_POINT ( 'NONE', #29185 ) ;
#85883 =( GEOMETRIC_REPRESENTATION_CONTEXT ( 3 ) GLOBAL_UNCERTAINTY_ASSIGNED_CONTEXT ( ( #24712 ) ) GLOBAL_UNIT_ASSIGNED_CONTEXT ( ( #85782, #2701, #18387 ) ) REPRESENTATION_CONTEXT ( 'NONE', 'WORKASPACE' ) );
#85884 = CARTESIAN_POINT ( 'NONE',  ( -8.573043381437493338, 295.3718485560969498, 5.156920410645950525 ) ) ;
#85885 = DIRECTION ( 'NONE',  ( -0.000000000000000000, -1.000000000000000000, -0.000000000000000000 ) ) ;
#85886 = FACE_OUTER_BOUND ( 'NONE', #11122, .T. ) ;
#85888 = CYLINDRICAL_SURFACE ( 'NONE', #8474, 4.000000000000000000 ) ;
#85887 = DIRECTION ( 'NONE',  ( 1.000000000000000000, 0.000000000000000000, 0.000000000000000000 ) ) ;
#85889 = CARTESIAN_POINT ( 'NONE',  ( -2.977408999572654480, -27.12500000204838457, 7.188101187499999156 ) ) ;
#85890 = DIRECTION ( 'NONE',  ( 0.5735764363510442720, -0.8191520442889930198, 1.003171929053526349E-16 ) ) ;
#85891 = CARTESIAN_POINT ( 'NONE',  ( 9.743117168495814440, -5.000000000000000000, 2.583982984168559316 ) ) ;
#85892 = MECHANICAL_DESIGN_GEOMETRIC_PRESENTATION_REPRESENTATION (  '', ( #34241 ), #34311 ) ;
#85893 = CARTESIAN_POINT ( 'NONE',  ( 43.58349330513380693, 1.593028355512270567E-15, 0.000000000000000000 ) ) ;
#85894 = ITEM_DEFINED_TRANSFORMATION ( 'NONE', 'NONE', #71400,  #10728 ) ;
#85895 = VERTEX_POINT ( 'NONE', #4863 ) ;
#85896 = CARTESIAN_POINT ( 'NONE',  ( -17.49999999999999645, 2.500000000000000444, 25.00000000000000000 ) ) ;
#85897 = FILL_AREA_STYLE_COLOUR ( '', #73668 ) ;
#85898 = CARTESIAN_POINT ( 'NONE',  ( -4.334700171289733284, 10.76211272510062678, -5.000000000000000888 ) ) ;
#85899 = DIRECTION ( 'NONE',  ( -1.000000000000000000, -1.224606353822377258E-16, -0.000000000000000000 ) ) ;
#85900 = VERTEX_POINT ( 'NONE', #45851 ) ;
#85901 = VECTOR ( 'NONE', #48322, 1000.000000000000000 ) ;
#85902 = CARTESIAN_POINT ( 'NONE',  ( -8.559508646656389885, 51.55638410492942825, -4.031152949374503081 ) ) ;
#85903 = CARTESIAN_POINT ( 'NONE',  ( 7.999999999999998224, -21.78125000409677625, 3.313708498984766049 ) ) ;
#85904 = VERTEX_POINT ( 'NONE', #84712 ) ;
#85905 = EDGE_CURVE ( 'NONE', #25105, #38536, #97822, .T. ) ;
#85906 = CARTESIAN_POINT ( 'NONE',  ( -27.42256603292173267, 34.64699562455260207, 7.556984339685873131 ) ) ;
#85907 = CARTESIAN_POINT ( 'NONE',  ( 9.333892298909264085, 103.2172426837496602, -3.590295303293454587 ) ) ;
#85908 = CARTESIAN_POINT ( 'NONE',  ( -16.91704105317864659, 37.08060170114688248, 21.81528127871682798 ) ) ;
#85909 = UNCERTAINTY_MEASURE_WITH_UNIT (LENGTH_MEASURE( 1.000000000000000082E-05 ), #28104, 'distance_accuracy_value', 'NONE');
#85910 = CARTESIAN_POINT ( 'NONE',  ( -111.1105008086674388, -60.00000000000000000, 186.7259703680355472 ) ) ;
#85911 = DIRECTION ( 'NONE',  ( 0.000000000000000000, -1.000000000000000000, 0.000000000000000000 ) ) ;
#85913 = AXIS2_PLACEMENT_3D ( 'NONE', #90553, #16662, #66813 ) ;
#85912 = CARTESIAN_POINT ( 'NONE',  ( 6.310175713569941003, 53.41366202879699188, -8.023280885595736933 ) ) ;
#85914 = CARTESIAN_POINT ( 'NONE',  ( -45.33180403702434091, 464.4945808635454227, 2.178908857919817699 ) ) ;
#85915 = VECTOR ( 'NONE', #84006, 1000.000000000000000 ) ;
#85916 = CARTESIAN_POINT ( 'NONE',  ( -86.06160377997784394, -21.58091379659038722, 174.3369035936914884 ) ) ;
#85917 = CARTESIAN_POINT ( 'NONE',  ( 34.86657997040038737, 42.62263848107266995, -62.56637741842270373 ) ) ;
#85918 = EDGE_CURVE ( 'NONE', #53703, #54493, #104162, .T. ) ;
#85919 = ORIENTED_EDGE ( 'NONE', *, *, #39934, .F. ) ;
#85920 = CARTESIAN_POINT ( 'NONE',  ( -10.20373343965778545, 45.40217293244035091, -15.40779740156157374 ) ) ;
#85921 = EDGE_CURVE ( 'NONE', #3119, #18508, #19496, .T. ) ;
#85922 = CARTESIAN_POINT ( 'NONE',  ( 3.349796915312611478, -1.132149698119323311, 104.5044954676210125 ) ) ;
#85923 = CARTESIAN_POINT ( 'NONE',  ( -83.79706745093385223, -45.26740093649807761, 6.296018886061934161 ) ) ;
#85924 = DIRECTION ( 'NONE',  ( 0.000000000000000000, -1.000000000000000000, 0.000000000000000000 ) ) ;
#85925 = CARTESIAN_POINT ( 'NONE',  ( -4.678819457397884740, 143.9212778189118467, -5.000000000000000000 ) ) ;
#85926 = CARTESIAN_POINT ( 'NONE',  ( 8.020865862485518250, 104.2551619145343835, -5.000000000000000888 ) ) ;
#85928 = CARTESIAN_POINT ( 'NONE',  ( -4.678819457397884740, 143.9212778189118467, -5.000000000000000000 ) ) ;
#85927 = AXIS2_PLACEMENT_3D ( 'NONE', #16119, #90549, #16658 ) ;
#85929 = CARTESIAN_POINT ( 'NONE',  ( -36.40416150961017649, 41.99999999999999289, 47.37019975558912677 ) ) ;
#85930 = AXIS2_PLACEMENT_3D ( 'NONE', #83977, #75885, #889 ) ;
#85931 = CARTESIAN_POINT ( 'NONE',  ( 60.31460910868286618, -60.00000000000004263, 109.8329304423809702 ) ) ;
#85932 = CARTESIAN_POINT ( 'NONE',  ( -0.000000000000000000, 61.49999999999999289, -8.160374191332742555 ) ) ;
#85933 = CARTESIAN_POINT ( 'NONE',  ( -89.21220262753612928, -29.99999999999994316, 13.74661749290507906 ) ) ;
#85934 = CARTESIAN_POINT ( 'NONE',  ( -64.70029564103292330, -39.48557291963400928, 85.32163151726285832 ) ) ;
#85935 = ORIENTED_EDGE ( 'NONE', *, *, #5587, .T. ) ;
#85936 = CARTESIAN_POINT ( 'NONE',  ( 103.0033180414816343, -14.21045842199429643, 193.8537495780579150 ) ) ;
#85937 = CARTESIAN_POINT ( 'NONE',  ( 65.26569490341492497, 40.83736746500258619, 0.7620991476189149516 ) ) ;
#85938 = CARTESIAN_POINT ( 'NONE',  ( 30.70107235603070706, -60.00000000001240608, 46.11011145243585219 ) ) ;
#85939 = MECHANICAL_DESIGN_GEOMETRIC_PRESENTATION_REPRESENTATION (  '', ( #61852 ), #70459 ) ;
#85940 = ORIENTED_EDGE ( 'NONE', *, *, #15394, .T. ) ;
#85941 = LINE ( 'NONE', #45992, #40727 ) ;
#85942 = CARTESIAN_POINT ( 'NONE',  ( 4.401442555609581635E-16, -26.65625000204838813, -7.188101187500000044 ) ) ;
#85943 = CARTESIAN_POINT ( 'NONE',  ( 37.40949999999997289, 0.000000000000000000, 4.000000000000001776 ) ) ;
#85944 = ORIENTED_EDGE ( 'NONE', *, *, #64066, .T. ) ;
#85945 = FACE_OUTER_BOUND ( 'NONE', #18947, .T. ) ;
#85946 = ORIENTED_EDGE ( 'NONE', *, *, #96592, .T. ) ;
#85947 = LINE ( 'NONE', #77834, #40675 ) ;
#85948 = CARTESIAN_POINT ( 'NONE',  ( 47.14503195514078016, 18.54431490493022494, -14.71570748879639190 ) ) ;
#85949 = CARTESIAN_POINT ( 'NONE',  ( -5.653164214226177542, -59.99999999997061906, 41.97898663223412541 ) ) ;
#85950 = CARTESIAN_POINT ( 'NONE',  ( 69.92761780597730592, 6.856755485862130937E-15, 0.000000000000000000 ) ) ;
#85951 = CARTESIAN_POINT ( 'NONE',  ( 2.977408999572651815, -31.81250000204839168, 7.188101187500000933 ) ) ;
#85952 = CARTESIAN_POINT ( 'NONE',  ( -49.03498469565148099, 14.13689777146986870, 14.86104782056252205 ) ) ;
#85953 = FILL_AREA_STYLE_COLOUR ( '', #67083 ) ;
#85954 = CARTESIAN_POINT ( 'NONE',  ( 55.26095113931063452, 4.898587196589294500E-16, -4.000000000000007105 ) ) ;
#85955 = CARTESIAN_POINT ( 'NONE',  ( 11.68767211932355998, 50.00000000000000000, -88.14097461399491351 ) ) ;
#85956 = CARTESIAN_POINT ( 'NONE',  ( -7.800703710507054467, 108.5859569265794136, 1.791736796405269505 ) ) ;
#85957 = CARTESIAN_POINT ( 'NONE',  ( 0.000000000000000000, 0.000000000000000000, 0.000000000000000000 ) ) ;
#85958 = VERTEX_POINT ( 'NONE', #52333 ) ;
#85959 = SURFACE_STYLE_USAGE ( .BOTH. , #28809 ) ;
#85960 = MECHANICAL_DESIGN_GEOMETRIC_PRESENTATION_REPRESENTATION (  '', ( #78996 ), #34299 ) ;
#85962 = CARTESIAN_POINT ( 'NONE',  ( 33.47661863257818737, -18.69765052410563655, 30.56412019559146742 ) ) ;
#85961 = CARTESIAN_POINT ( 'NONE',  ( -80.00000000000000000, -52.00000000000000000, -23.09707704303352926 ) ) ;
#85963 = DIRECTION ( 'NONE',  ( 0.000000000000000000, -1.000000000000000000, 0.000000000000000000 ) ) ;
#85964 = ORIENTED_EDGE ( 'NONE', *, *, #78732, .T. ) ;
#85965 = CARTESIAN_POINT ( 'NONE',  ( -22.11381839868240107, 25.65490958513800734, -32.62441910024401892 ) ) ;
#85966 = TOROIDAL_SURFACE ( 'NONE', #42894, 64.50000000000000000, 0.5000000000000000000 ) ;
#85967 = EDGE_CURVE ( 'NONE', #36049, #32988, #28109, .T. ) ;
#85968 = AXIS2_PLACEMENT_3D ( 'NONE', #45559, #104294, #13688 ) ;
#85969 = B_SPLINE_CURVE_WITH_KNOTS ( 'NONE', 3,
 ( #3207, #50655, #83571, #9679, #30696, #95942, #29129, #78148, #62000, #38771, #62516, #63583, #4268, #22612, #95399, #37196, #46321, #6370, #54373, #86271 ),
 .UNSPECIFIED., .F., .F.,
 ( 4, 2, 2, 2, 2, 2, 2, 2, 2, 4 ),
 ( 0.007055264176649387285, 0.007558908847143414045, 0.008062553517637439937, 0.008566198188131465829, 0.008818020523378480510, 0.009069842858625493456, 0.009573487529119514144, 0.01007713219961353657, 0.01058077687010755726, 0.01108442154060157794 ),
 .UNSPECIFIED. ) ;
#85970 = CARTESIAN_POINT ( 'NONE',  ( -30.24427031855517711, 312.0196691915732004, -8.325478004009855937 ) ) ;
#85971 = DIRECTION ( 'NONE',  ( -1.000000000000000000, -1.224606353822377258E-16, -0.000000000000000000 ) ) ;
#85972 = DIRECTION ( 'NONE',  ( 0.000000000000000000, -1.000000000000000000, 0.000000000000000000 ) ) ;
#85973 = SURFACE_STYLE_FILL_AREA ( #42825 ) ;
#85974 = DIRECTION ( 'NONE',  ( 1.000000000000000000, -0.000000000000000000, -0.000000000000000000 ) ) ;
#85975 = PRESENTATION_STYLE_ASSIGNMENT (( #10974 ) ) ;
#85977 = VERTEX_POINT ( 'NONE', #11329 ) ;
#85976 = PRESENTATION_LAYER_ASSIGNMENT (  '', '', ( #5036 ) ) ;
#85978 = CARTESIAN_POINT ( 'NONE',  ( 91.92166457297645366, -60.00000000000000711, 16.22366861495048695 ) ) ;
#85979 = CARTESIAN_POINT ( 'NONE',  ( 0.000000000000000000, -100.0000000000000000, -13.00000000000003730 ) ) ;
#85980 = CARTESIAN_POINT ( 'NONE',  ( -35.76697723764162617, 397.1839565823023577, 5.954605915834287444 ) ) ;
#85981 = CARTESIAN_POINT ( 'NONE',  ( -6.812288195523935386, 40.56150966584056761, -71.12586875364199557 ) ) ;
#85982 = CARTESIAN_POINT ( 'NONE',  ( -12.82134596817017780, 18.88695635519247773, -8.090906795103039784 ) ) ;
#85983 = EDGE_CURVE ( 'NONE', #12726, #2575, #95174, .T. ) ;
#85984 = VERTEX_POINT ( 'NONE', #96530 ) ;
#85985 = CARTESIAN_POINT ( 'NONE',  ( -96.81373938066217022, -30.00000000000823164, 199.8413627685791312 ) ) ;
#85986 = EDGE_LOOP ( 'NONE', ( #70981, #72891, #97742, #91223 ) ) ;
#85987 = AXIS2_PLACEMENT_3D ( 'NONE', #43972, #52048, #27303 ) ;
#85988 = CARTESIAN_POINT ( 'NONE',  ( -9.378256585906134646, -55.78346096903717211, 23.52725134406122720 ) ) ;
#85989 = CARTESIAN_POINT ( 'NONE',  ( 0.000000000000000000, 23.58303312036771615, -45.10524579772351217 ) ) ;
#85990 = CARTESIAN_POINT ( 'NONE',  ( 15.79792377994583852, 22.78987439203660159, 0.2434392984428970785 ) ) ;
#85991 = CARTESIAN_POINT ( 'NONE',  ( 85.48529165631397575, -52.75865074998397830, -10.94020551895792970 ) ) ;
#85992 = CARTESIAN_POINT ( 'NONE',  ( -7.188101187500001821, -29.37500000204838457, -2.977408999572651371 ) ) ;
#85993 = CARTESIAN_POINT ( 'NONE',  ( -17.58856438785635490, 45.00000000000000711, 63.14100056368219782 ) ) ;
#85994 = CARTESIAN_POINT ( 'NONE',  ( -18.91950813577646784, 304.6927365361660804, 8.903189087522576983 ) ) ;
#85995 = EDGE_LOOP ( 'NONE', ( #6219, #24019, #36172, #93570 ) ) ;
#85996 =( BOUNDED_SURFACE ( )  B_SPLINE_SURFACE ( 3, 2, ( 
 ( #23679, #47384, #6387 ),
 ( #97005, #38275, #71135 ),
 ( #89456, #62530, #103507 ),
 ( #95416, #104026, #54392 ) ),
 .UNSPECIFIED., .F., .F., .F. ) 
 B_SPLINE_SURFACE_WITH_KNOTS ( ( 4, 4 ),
 ( 3, 3 ),
 ( 4.770489558936219510E-18, 0.001771883439662679666 ),
 ( 0.000000000000000000, 1.000000000000000000 ),
 .UNSPECIFIED. ) 
 GEOMETRIC_REPRESENTATION_ITEM ( )  RATIONAL_B_SPLINE_SURFACE ( (
 ( 1.000000000000000000, 0.7699558187665703768, 1.000000000000000000),
 ( 1.000000000000000000, 0.7661160612245745405, 1.000000000000000000),
 ( 1.000000000000000000, 0.7602452393655095841, 1.000000000000000000),
 ( 1.000000000000000000, 0.7533433155455017127, 1.000000000000000000) ) ) 
 REPRESENTATION_ITEM ( '' )  SURFACE ( )  );
#85997 = LINE ( 'NONE', #14179, #71938 ) ;
#85998 = VERTEX_POINT ( 'NONE', #6965 ) ;
#85999 = CARTESIAN_POINT ( 'NONE',  ( 49.27997219161959919, 7.868281554635434105, -15.62830927991629792 ) ) ;
#86000 = AXIS2_PLACEMENT_3D ( 'NONE', #27220, #99994, #26162 ) ;
#86002 = ORIENTED_EDGE ( 'NONE', *, *, #4796, .F. ) ;
#86001 = DIRECTION ( 'NONE',  ( 0.000000000000000000, 0.000000000000000000, 1.000000000000000000 ) ) ;
#86003 = CARTESIAN_POINT ( 'NONE',  ( 78.25203214054160128, -42.96388236615710809, 138.8363729379485960 ) ) ;
#86004 = EDGE_CURVE ( 'NONE', #105451, #89053, #5201, .T. ) ;
#86005 = AXIS2_PLACEMENT_3D ( 'NONE', #15683, #7578, #80412 ) ;
#86006 = ORIENTED_EDGE ( 'NONE', *, *, #21015, .F. ) ;
#86007 = CARTESIAN_POINT ( 'NONE',  ( 2.629190634011728367, -49.75653670290434150, 40.87823124498205374 ) ) ;
#86008 = CARTESIAN_POINT ( 'NONE',  ( -7.188101187500000933, -17.00000000204838813, -2.977408999572651371 ) ) ;
#86009 = CARTESIAN_POINT ( 'NONE',  ( -111.0360493097450529, -57.67057850706027722, 194.0974529949267549 ) ) ;
#86010 = EDGE_CURVE ( 'NONE', #54573, #92082, #64687, .T. ) ;
#86011 = B_SPLINE_CURVE_WITH_KNOTS ( 'NONE', 3,
 ( #37055, #51596, #68876, #10604 ),
 .UNSPECIFIED., .F., .F.,
 ( 4, 4 ),
 ( 0.000000000000000000, 0.0007940539003707024418 ),
 .UNSPECIFIED. ) ;
#86012 = ORIENTED_EDGE ( 'NONE', *, *, #9885, .T. ) ;
#86013 = PRESENTATION_STYLE_ASSIGNMENT (( #54650 ) ) ;
#86014 = CARTESIAN_POINT ( 'NONE',  ( 3.443305032968360102, 27.85938107923988483, 4.999999999999997335 ) ) ;
#86015 = CARTESIAN_POINT ( 'NONE',  ( -9.334514330295430540, 83.21377262318209489, -3.588704711590609442 ) ) ;
#86016 = CARTESIAN_POINT ( 'NONE',  ( 49.15269216906074234, 13.73471152902317272, -15.05374764292056078 ) ) ;
#86017 = CARTESIAN_POINT ( 'NONE',  ( -5.656854249492381470, -19.25000000409677270, 5.656854249492379694 ) ) ;
#86018 = CARTESIAN_POINT ( 'NONE',  ( -39.94456049126967656, -26.30212818477839321, 35.92538891840626292 ) ) ;
#86019 =( NAMED_UNIT ( * ) PLANE_ANGLE_UNIT ( ) SI_UNIT ( $, .RADIAN. ) );
#86020 = VECTOR ( 'NONE', #34776, 1000.000000000000000 ) ;
#86021 = CARTESIAN_POINT ( 'NONE',  ( 43.00000000000000000, 485.2629658518202405, -2.796394914059364911 ) ) ;
#86022 = CARTESIAN_POINT ( 'NONE',  ( -9.380894568449075877, 87.01130633110940948, -3.467341429141164610 ) ) ;
#86023 = DIRECTION ( 'NONE',  ( -1.000000000000000000, -1.224606353822377258E-16, -0.000000000000000000 ) ) ;
#86024 = EDGE_CURVE ( 'NONE', #105963, #30899, #64419, .T. ) ;
#86025 = DIRECTION ( 'NONE',  ( 0.000000000000000000, 0.000000000000000000, 1.000000000000000000 ) ) ;
#86026 = ORIENTED_EDGE ( 'NONE', *, *, #61711, .T. ) ;
#86027 = CARTESIAN_POINT ( 'NONE',  ( -3.711585775949200805, -49.05321961974463818, 40.67751789774135318 ) ) ;
#86028 = CARTESIAN_POINT ( 'NONE',  ( 11.60416385448452203, -4.915838321100066466, -12.56281314056613674 ) ) ;
#86029 = CARTESIAN_POINT ( 'NONE',  ( 0.1550192221702281492, 7.763576898078555111, 51.74244561565719636 ) ) ;
#86030 = CARTESIAN_POINT ( 'NONE',  ( 73.94814338752382810, -30.09466847450056903, -28.11389532863423568 ) ) ;
#86031 = CARTESIAN_POINT ( 'NONE',  ( -82.93722998966033799, -30.00000000000000000, 152.4467691388267951 ) ) ;
#86032 = CARTESIAN_POINT ( 'NONE',  ( -7.069742149889169269, 41.66287055432060527, -69.58314084294495672 ) ) ;
#86033 = AXIS2_PLACEMENT_3D ( 'NONE', #62042, #5881, #53907 ) ;
#86034 = ORIENTED_EDGE ( 'NONE', *, *, #29783, .T. ) ;
#86035 = CARTESIAN_POINT ( 'NONE',  ( 0.000000000000000000, 4.000000000000000000, 0.000000000000000000 ) ) ;
#86036 = CARTESIAN_POINT ( 'NONE',  ( 76.00644063775833104, -57.54596990661518419, 193.1823216553611076 ) ) ;
#86037 = CONICAL_SURFACE ( 'NONE', #1600, 4.000000000000001776, 0.9599310885968774798 ) ;
#86038 = CARTESIAN_POINT ( 'NONE',  ( 57.28004366725042473, -36.93788119843549822, -34.78852087230680468 ) ) ;
#86039 = CARTESIAN_POINT ( 'NONE',  ( 29.68315524077034695, -1.200000000000000030E-05, 42.10535821593451544 ) ) ;
#86040 = CARTESIAN_POINT ( 'NONE',  ( -65.75807407283386397, -60.00000000000000711, 121.3892982347636007 ) ) ;
#86041 = CARTESIAN_POINT ( 'NONE',  ( 87.04245038058458306, 6.123233995736582872E-16, -5.000000000000011546 ) ) ;
#86042 = CIRCLE ( 'NONE', #25793, 4.000000000000000888 ) ;
#86043 = CARTESIAN_POINT ( 'NONE',  ( 60.62677696746332145, 48.00000000000000000, 24.18439665019722540 ) ) ;
#86044 = CARTESIAN_POINT ( 'NONE',  ( -86.35312816053438212, -20.98790165847923461, 180.9809247037294142 ) ) ;
#86045 = ORIENTED_EDGE ( 'NONE', *, *, #26804, .T. ) ;
#86046 = CARTESIAN_POINT ( 'NONE',  ( 14.29190075645216851, 7.765108448534480345, -6.049455384114759582 ) ) ;
#86047 = CARTESIAN_POINT ( 'NONE',  ( -4.046613933372436023, -39.47588596367953784, 30.46164947777460696 ) ) ;
#86048 = CARTESIAN_POINT ( 'NONE',  ( -6.294744146068734558, 41.94828263137729607, -59.44631356406647882 ) ) ;
#86049 = CARTESIAN_POINT ( 'NONE',  ( 41.50669491856072568, 5.000000000000003553, 0.000000000000000000 ) ) ;
#86050 = CYLINDRICAL_SURFACE ( 'NONE', #62922, 4.000000000000000000 ) ;
#86051 = EDGE_CURVE ( 'NONE', #57919, #88345, #29673, .T. ) ;
#86052 = EDGE_LOOP ( 'NONE', ( #93880, #98671, #56320, #66841, #64532 ) ) ;
#86053 = DIRECTION ( 'NONE',  ( -1.000000000000000000, -1.224606353822377258E-16, -0.000000000000000000 ) ) ;
#86054 = FACE_OUTER_BOUND ( 'NONE', #94812, .T. ) ;
#86055 = CIRCLE ( 'NONE', #99798, 5.000000000000011546 ) ;
#86056 = CARTESIAN_POINT ( 'NONE',  ( 10.11650669486618881, -3.999999999999998224, 0.000000000000000000 ) ) ;
#86057 = DIRECTION ( 'NONE',  ( 0.000000000000000000, -1.000000000000000000, 0.000000000000000000 ) ) ;
#86058 = VERTEX_POINT ( 'NONE', #56030 ) ;
#86059 = CARTESIAN_POINT ( 'NONE',  ( 26.14799737485564890, 295.8871012151415130, -9.777418602662287128 ) ) ;
#86060 = EDGE_CURVE ( 'NONE', #46987, #49140, #56541, .T. ) ;
#86061 = CARTESIAN_POINT ( 'NONE',  ( 22.18906107735381283, 305.1406206946286943, -9.938500898755204815 ) ) ;
#86062 = EDGE_CURVE ( 'NONE', #49120, #6957, #76681, .T. ) ;
#86063 = CARTESIAN_POINT ( 'NONE',  ( -15.50035291838927876, -4.285714285714916194, 20.16952962162167395 ) ) ;
#86064 = SURFACE_STYLE_FILL_AREA ( #52592 ) ;
#86065 = VECTOR ( 'NONE', #92951, 1000.000000000000000 ) ;
#86066 = CARTESIAN_POINT ( 'NONE',  ( 102.4475954893556633, -30.00000000000004263, 111.1011446524310742 ) ) ;
#86067 = CARTESIAN_POINT ( 'NONE',  ( -79.16702777562869642, -56.85000040143994937, 161.1953825210129878 ) ) ;
#86068 = ORIENTED_EDGE ( 'NONE', *, *, #58413, .F. ) ;
#86069 = CARTESIAN_POINT ( 'NONE',  ( 0.000000000000000000, 15.00000000000000000, 0.000000000000000000 ) ) ;
#86070 = DIRECTION ( 'NONE',  ( -1.000000000000000000, 0.000000000000000000, 0.000000000000000000 ) ) ;
#86071 = CARTESIAN_POINT ( 'NONE',  ( 62.95715931499727702, 49.99999999999999289, 4.917584479073736858 ) ) ;
#86072 = CARTESIAN_POINT ( 'NONE',  ( 42.72237582395932520, 338.4720114372719308, 8.457513108131092139 ) ) ;
#86073 = AXIS2_PLACEMENT_3D ( 'NONE', #101805, #100738, #2570 ) ;
#86074 = CARTESIAN_POINT ( 'NONE',  ( 43.68737779332730753, 464.3703856682132027, 8.648249337468564946 ) ) ;
#86075 = ORIENTED_EDGE ( 'NONE', *, *, #77017, .T. ) ;
#86076 = DIRECTION ( 'NONE',  ( -1.000000000000000000, -0.000000000000000000, -0.000000000000000000 ) ) ;
#86077 = CARTESIAN_POINT ( 'NONE',  ( 31.61743702809175716, 439.0120537715812929, 23.38841530320140549 ) ) ;
#86078 = CARTESIAN_POINT ( 'NONE',  ( -5.082755093536325042, -24.59375000204838813, -5.082755093536325930 ) ) ;
#86079 = EDGE_LOOP ( 'NONE', ( #40020, #4523, #46692, #79067 ) ) ;
#86080 = CARTESIAN_POINT ( 'NONE',  ( -8.034710196240776243E-11, 303.8518027762758038, -9.000000000000005329 ) ) ;
#86081 = CARTESIAN_POINT ( 'NONE',  ( 5.129365358145452802, 41.91296950070222493, -69.99827769498368468 ) ) ;
#86082 = EDGE_CURVE ( 'NONE', #88814, #88610, #6425, .T. ) ;
#86083 = CARTESIAN_POINT ( 'NONE',  ( 6.249999999999998224, -6.928203230275504332, 4.000000000000011546 ) ) ;
#86084 = LINE ( 'NONE', #61811, #62845 ) ;
#86085 = B_SPLINE_CURVE_WITH_KNOTS ( 'NONE', 3,
 ( #56153, #9217, #89627, #65876, #64815, #97696, #89097, #49141, #40535, #98238 ),
 .UNSPECIFIED., .F., .F.,
 ( 4, 2, 2, 2, 4 ),
 ( 0.000000000000000000, 0.001247095126357080329, 0.002494190252714160658, 0.003741285379071240987, 0.004988380505428321315 ),
 .UNSPECIFIED. ) ;
#86086 = DIRECTION ( 'NONE',  ( 0.000000000000000000, -0.5000000000000013323, -0.8660254037844379305 ) ) ;
#86087 = EDGE_LOOP ( 'NONE', ( #99376, #101737, #67002, #12994, #49978, #52299 ) ) ;
#86088 = CARTESIAN_POINT ( 'NONE',  ( 68.54330978433023347, -60.00000000000000000, -33.08258948747816675 ) ) ;
#86090 = CARTESIAN_POINT ( 'NONE',  ( 25.48282336132001191, -56.86957850576434481, 34.80755836682993021 ) ) ;
#86089 = CARTESIAN_POINT ( 'NONE',  ( -68.63253095932553549, -60.00000000000002842, 147.4008728361381486 ) ) ;
#86091 = VECTOR ( 'NONE', #90361, 1000.000000000000000 ) ;
#86092 = CARTESIAN_POINT ( 'NONE',  ( -1.600194386257963230E-15, 60.33964880548970200, 13.06657876680918662 ) ) ;
#86093 = CARTESIAN_POINT ( 'NONE',  ( -36.01933158121845935, -22.19451844719506184, 32.43403767349134625 ) ) ;
#86094 = ADVANCED_FACE ( 'NONE', ( #72241 ), #86431, .T. ) ;
#86095 = UNCERTAINTY_MEASURE_WITH_UNIT (LENGTH_MEASURE( 1.000000000000000082E-05 ), #79374, 'distance_accuracy_value', 'NONE');
#86096 = ORIENTED_EDGE ( 'NONE', *, *, #14700, .T. ) ;
#86097 = CARTESIAN_POINT ( 'NONE',  ( -16.75187969033532553, -1.200000000000000030E-05, 23.05698433968612093 ) ) ;
#86098 = CARTESIAN_POINT ( 'NONE',  ( -13.53382989543471560, -56.00915974862302704, 30.58576288564093915 ) ) ;
#86099 = VECTOR ( 'NONE', #95002, 1000.000000000000000 ) ;
#86100 = DIRECTION ( 'NONE',  ( -1.000000000000000000, -0.000000000000000000, -0.000000000000000000 ) ) ;
#86101 = CARTESIAN_POINT ( 'NONE',  ( 6.445370176741822554, 4.584736124523701939, 5.738941594274445279 ) ) ;
#86102 = CARTESIAN_POINT ( 'NONE',  ( 81.84444444444444855, 1.023464760207051730E-14, 0.000000000000000000 ) ) ;
#86103 = ORIENTED_EDGE ( 'NONE', *, *, #86740, .F. ) ;
#86104 = CARTESIAN_POINT ( 'NONE',  ( -75.84932468004862471, -38.36924633978998145, 177.1874917199713195 ) ) ;
#86105 =( NAMED_UNIT ( * ) SI_UNIT ( $, .STERADIAN. ) SOLID_ANGLE_UNIT ( ) );
#86106 = CARTESIAN_POINT ( 'NONE',  ( 99.00547121574200560, -30.00000000000000000, 188.8237953836635654 ) ) ;
#86107 = CARTESIAN_POINT ( 'NONE',  ( 36.45193875802095107, 40.26000571314290255, -57.68880871784696751 ) ) ;
#86108 = CARTESIAN_POINT ( 'NONE',  ( 3.826931552919423218, 16.00000000000000000, 9.246279647933185686 ) ) ;
#86109 = CARTESIAN_POINT ( 'NONE',  ( 81.59236582409479865, -29.99999999999999289, -7.441647983982530690 ) ) ;
#86110 = LINE ( 'NONE', #69904, #93238 ) ;
#86111 = EDGE_CURVE ( 'NONE', #85724, #27470, #56045, .T. ) ;
#86112 = ORIENTED_EDGE ( 'NONE', *, *, #69048, .T. ) ;
#86113 = EDGE_CURVE ( 'NONE', #6669, #51522, #11225, .T. ) ;
#86114 = CONICAL_SURFACE ( 'NONE', #39596, 13.50000000000000178, 1.047197551196596077 ) ;
#86115 = ORIENTED_EDGE ( 'NONE', *, *, #355, .F. ) ;
#86116 = VERTEX_POINT ( 'NONE', #71710 ) ;
#86117 = DIRECTION ( 'NONE',  ( 1.000000000000000000, -0.000000000000000000, -0.000000000000000000 ) ) ;
#86118 = PLANE ( 'NONE',  #54478 ) ;
#86119 = CARTESIAN_POINT ( 'NONE',  ( 0.000000000000000000, 4.898587196589413815E-16, -4.000000000000000888 ) ) ;
#86120 = CARTESIAN_POINT ( 'NONE',  ( -37.63787431931454819, 432.3637935970024273, 5.163396886644006756 ) ) ;
#86121 = CARTESIAN_POINT ( 'NONE',  ( 5.912233003206735837, 54.01420674394145749, 6.185142564729861903 ) ) ;
#86122 = DIRECTION ( 'NONE',  ( -1.000000000000000000, -1.224606353822377258E-16, -0.000000000000000000 ) ) ;
#86124 = ORIENTED_EDGE ( 'NONE', *, *, #100665, .T. ) ;
#86123 = AXIS2_PLACEMENT_3D ( 'NONE', #54810, #15420, #62934 ) ;
#86125 = CARTESIAN_POINT ( 'NONE',  ( 29.87444201908948216, 8.057352084660386993, 42.09618695302963687 ) ) ;
#86126 = ORIENTED_EDGE ( 'NONE', *, *, #79320, .T. ) ;
#86127 = CARTESIAN_POINT ( 'NONE',  ( -5.981691436642410764, -61.02730900805882186, -0.5384679144502715342 ) ) ;
#86128 = CARTESIAN_POINT ( 'NONE',  ( 33.00000000000000000, 450.0000000000002274, 25.20242257375371864 ) ) ;
#86129 = DIRECTION ( 'NONE',  ( 0.000000000000000000, -1.000000000000000000, 0.000000000000000000 ) ) ;
#86130 = CARTESIAN_POINT ( 'NONE',  ( 26.68501260228623906, 296.2122705307798469, 2.231322931648561880 ) ) ;
#86131 = COLOUR_RGB ( '', 0.09019608, 0.27058824, 0.51372549) ;
#86132 = CARTESIAN_POINT ( 'NONE',  ( 6.326445470157513462, -5.253846677262528075, -4.563138989068575846 ) ) ;
#86133 = CARTESIAN_POINT ( 'NONE',  ( 64.43859380035580386, -22.10221476649115502, 75.67156401609979355 ) ) ;
#86134 = ORIENTED_EDGE ( 'NONE', *, *, #5809, .F. ) ;
#86135 = CARTESIAN_POINT ( 'NONE',  ( 28.79545026039418332, 10.21913446882435750, -41.74404769594831066 ) ) ;
#86136 = FACE_OUTER_BOUND ( 'NONE', #31999, .T. ) ;
#86137 = CARTESIAN_POINT ( 'NONE',  ( -42.33268550343508707, 436.4462712439766960, 6.764016893796111596 ) ) ;
#86138 =( BOUNDED_SURFACE ( )  B_SPLINE_SURFACE ( 3, 3, ( 
 ( #1902, #27841, #19225, #93058 ),
 ( #2441, #11054, #51523, #52585 ),
 ( #102208, #28356, #69850, #102745 ),
 ( #10534, #28906, #43451, #60712 ) ),
 .UNSPECIFIED., .F., .F., .F. ) 
 B_SPLINE_SURFACE_WITH_KNOTS ( ( 4, 4 ),
 ( 4, 4 ),
 ( 0.02698643027831503644, 0.9670246242088337274 ),
 ( 0.000000000000000000, 1.000000000000000000 ),
 .UNSPECIFIED. ) 
 GEOMETRIC_REPRESENTATION_ITEM ( )  RATIONAL_B_SPLINE_SURFACE ( (
 ( 1.000000000000000000, 0.3333333333333334259, 0.3333333333333334259, 1.000000000000000000),
 ( 1.000000000000000000, 0.3333333333333334259, 0.3333333333333334259, 1.000000000000000000),
 ( 1.000000000000000000, 0.3333333333333334259, 0.3333333333333334259, 1.000000000000000000),
 ( 1.000000000000000000, 0.3333333333333334259, 0.3333333333333334259, 1.000000000000000000) ) ) 
 REPRESENTATION_ITEM ( '' )  SURFACE ( )  );
#86139 = MECHANICAL_DESIGN_GEOMETRIC_PRESENTATION_REPRESENTATION (  '', ( #60271 ), #101583 ) ;
#86140 = CARTESIAN_POINT ( 'NONE',  ( 46.00000000000000000, 461.6622277975422435, 10.18145404766785589 ) ) ;
#86141 = EDGE_CURVE ( 'NONE', #14996, #44397, #96017, .T. ) ;
#86142 = VERTEX_POINT ( 'NONE', #87403 ) ;
#86143 = AXIS2_PLACEMENT_3D ( 'NONE', #69807, #52018, #102703 ) ;
#86144 = SURFACE_STYLE_USAGE ( .BOTH. , #30026 ) ;
#86145 = DIRECTION ( 'NONE',  ( 1.000000000000000000, -0.000000000000000000, -0.000000000000000000 ) ) ;
#86146 =( NAMED_UNIT ( * ) PLANE_ANGLE_UNIT ( ) SI_UNIT ( $, .RADIAN. ) );
#86147 = EDGE_CURVE ( 'NONE', #7244, #58869, #31921, .T. ) ;
#86148 = CARTESIAN_POINT ( 'NONE',  ( 0.000000000000000000, -19.99999999999998934, 0.000000000000000000 ) ) ;
#86149 = EDGE_CURVE ( 'NONE', #26262, #62903, #46401, .T. ) ;
#86150 = CARTESIAN_POINT ( 'NONE',  ( 86.32943948890100216, -46.49832263646349162, 190.0111496207520361 ) ) ;
#86151 = CARTESIAN_POINT ( 'NONE',  ( 7.500000000000001776, 0.000000000000000000, 8.400000000000000355 ) ) ;
#86152 = AXIS2_PLACEMENT_3D ( 'NONE', #42917, #83896, #27845 ) ;
#86153 = CARTESIAN_POINT ( 'NONE',  ( -2.989987493987218414, 50.23304204759762825, 5.000000000000000000 ) ) ;
#86154 = ORIENTED_EDGE ( 'NONE', *, *, #61367, .T. ) ;
#86155 = FILL_AREA_STYLE ('',( #3624 ) ) ;
#86156 = B_SPLINE_CURVE_WITH_KNOTS ( 'NONE', 3,
 ( #96361, #71522, #7843, #106004, #79618, #55844, #105492, #6791 ),
 .UNSPECIFIED., .F., .F.,
 ( 4, 2, 2, 4 ),
 ( 0.003797433802554458452, 0.004743183970586253503, 0.005688934138618048121, 0.007580434474681637357 ),
 .UNSPECIFIED. ) ;
#86157 = EDGE_CURVE ( 'NONE', #38000, #25389, #83689, .T. ) ;
#86158 = CARTESIAN_POINT ( 'NONE',  ( -9.073678795326815205, -16.06358835070689750, -34.89371268523018443 ) ) ;
#86159 = CARTESIAN_POINT ( 'NONE',  ( 89.64643850830432825, -5.000000000000000000, 6.123233995736778115E-16 ) ) ;
#86160 = CARTESIAN_POINT ( 'NONE',  ( 13.38090213880806978, -53.73807135754422859, 31.11721482942555639 ) ) ;
#86161 = CARTESIAN_POINT ( 'NONE',  ( 5.000000000000000000, -15.25461064142281487, 12.58690022914873374 ) ) ;
#86162 = CARTESIAN_POINT ( 'NONE',  ( -90.20584754825765117, -30.00000000000000711, 89.69724495916204887 ) ) ;
#86163 = CARTESIAN_POINT ( 'NONE',  ( -32.12958771267418712, 464.7275665249413805, 11.12424126545828784 ) ) ;
#86164 = CARTESIAN_POINT ( 'NONE',  ( 0.01856856229768925892, -57.67120202543696905, 41.61186673337733311 ) ) ;
#86165 = CIRCLE ( 'NONE', #46564, 3.309500000000007880 ) ;
#86167 = CARTESIAN_POINT ( 'NONE',  ( 12.19423397773156736, 304.5852035401753710, 9.880331998383338643 ) ) ;
#86166 = CARTESIAN_POINT ( 'NONE',  ( -9.253583916535191634, 248.7019609199495846, 3.792462592445559721 ) ) ;
#86168 =( NAMED_UNIT ( * ) SI_UNIT ( $, .STERADIAN. ) SOLID_ANGLE_UNIT ( ) );
#86169 = CARTESIAN_POINT ( 'NONE',  ( -49.19868921488087210, -37.82012451832441968, 48.88653370302302648 ) ) ;
#86170 = CARTESIAN_POINT ( 'NONE',  ( -32.22120753352784561, 464.6691781026584636, 10.60621122532581140 ) ) ;
#86171 = CARTESIAN_POINT ( 'NONE',  ( 18.91781669292794987, 48.00000000000000000, 62.18610382930901892 ) ) ;
#86172 = DIRECTION ( 'NONE',  ( -0.000000000000000000, -0.000000000000000000, -1.000000000000000000 ) ) ;
#86173 = CARTESIAN_POINT ( 'NONE',  ( -24.88460094139896839, -39.48002255589691600, 31.72060110609164241 ) ) ;
#86174 = VERTEX_POINT ( 'NONE', #80872 ) ;
#86175 = CARTESIAN_POINT ( 'NONE',  ( 40.62309488084314779, 485.6251729596485234, -4.313937499023156263 ) ) ;
#86176 = CARTESIAN_POINT ( 'NONE',  ( -9.482856158761272525, 107.4430711585472409, 3.177891129109647217 ) ) ;
#86177 = CARTESIAN_POINT ( 'NONE',  ( -21.13863729395087887, -32.51627878024107332, 29.94168239066533133 ) ) ;
#86179 = CARTESIAN_POINT ( 'NONE',  ( 1.249887406536827505, 36.80358475306034194, -28.33952629896104369 ) ) ;
#86178 = FILL_AREA_STYLE_COLOUR ( '', #32995 ) ;
#86180 = EDGE_CURVE ( 'NONE', #88567, #13709, #87034, .T. ) ;
#86181 = ORIENTED_EDGE ( 'NONE', *, *, #22223, .T. ) ;
#86182 = AXIS2_PLACEMENT_3D ( 'NONE', #4741, #102367, #95346 ) ;
#86183 = DIRECTION ( 'NONE',  ( 0.000000000000000000, -1.000000000000000000, 0.000000000000000000 ) ) ;
#86184 = ORIENTED_EDGE ( 'NONE', *, *, #11571, .F. ) ;
#86185 = CARTESIAN_POINT ( 'NONE',  ( 67.22793774957824553, 4.898587196589294500E-16, -4.000000000000007105 ) ) ;
#86186 = ADVANCED_FACE ( 'NONE', ( #47441 ), #85318, .T. ) ;
#86187 = AXIS2_PLACEMENT_3D ( 'NONE', #50568, #92645, #82963 ) ;
#86188 = CARTESIAN_POINT ( 'NONE',  ( 85.31310517497098544, 1.030564683017419500E-14, 0.000000000000000000 ) ) ;
#86189 = ORIENTED_EDGE ( 'NONE', *, *, #71855, .T. ) ;
#86190 = CARTESIAN_POINT ( 'NONE',  ( 33.00795325653295009, 439.3958174160654835, 23.82489859418973666 ) ) ;
#86191 = CARTESIAN_POINT ( 'NONE',  ( 9.609938133605346877, 50.00000000000000000, -77.63956163932782317 ) ) ;
#86192 = CARTESIAN_POINT ( 'NONE',  ( 102.8835412338887352, -52.71848775370781226, 190.2923971475949827 ) ) ;
#86194 = DIRECTION ( 'NONE',  ( 0.000000000000000000, -1.000000000000000000, 0.000000000000000000 ) ) ;
#86193 = CARTESIAN_POINT ( 'NONE',  ( 51.20698849084796223, -38.00000000000000711, 52.28247866703643609 ) ) ;
#86195 = VERTEX_POINT ( 'NONE', #39382 ) ;
#86196 = AXIS2_PLACEMENT_3D ( 'NONE', #1358, #60188, #100073 ) ;
#86197 = ORIENTED_EDGE ( 'NONE', *, *, #48450, .F. ) ;
#86198 = ORIENTED_EDGE ( 'NONE', *, *, #62048, .F. ) ;
#86199 = CARTESIAN_POINT ( 'NONE',  ( 22.46479421738874649, 305.4359882429142772, 10.06336503754929801 ) ) ;
#86200 = AXIS2_PLACEMENT_3D ( 'NONE', #41759, #56868, #24026 ) ;
#86201 = CARTESIAN_POINT ( 'NONE',  ( -40.78808449138670511, 461.0038402359688234, 2.292482253616661581 ) ) ;
#86202 = DIRECTION ( 'NONE',  ( -1.000000000000000000, -1.224606353822377258E-16, -0.000000000000000000 ) ) ;
#86203 = ORIENTED_EDGE ( 'NONE', *, *, #36770, .T. ) ;
#86204 = ADVANCED_FACE ( 'NONE', ( #65232 ), #72260, .T. ) ;
#86205 = DIRECTION ( 'NONE',  ( 0.000000000000000000, -1.000000000000000000, 0.000000000000000000 ) ) ;
#86206 = CARTESIAN_POINT ( 'NONE',  ( -7.984026910922526810, 6.036057507192810867, -4.337419204752972490 ) ) ;
#86207 = CARTESIAN_POINT ( 'NONE',  ( -91.37266855712616120, -59.99999999999998579, -21.09057864729411946 ) ) ;
#86208 = AXIS2_PLACEMENT_3D ( 'NONE', #64639, #15544, #65163 ) ;
#86209 = DIRECTION ( 'NONE',  ( -0.6621791990579699583, 0.000000000000000000, -0.7493455199939116351 ) ) ;
#86210 = CARTESIAN_POINT ( 'NONE',  ( 69.31621320414066645, -59.99999999998080114, -35.31426391149900468 ) ) ;
#86211 = DIRECTION ( 'NONE',  ( 1.000000000000000000, 0.000000000000000000, 0.000000000000000000 ) ) ;
#86212 = CARTESIAN_POINT ( 'NONE',  ( -6.426572956751082977, 41.32129836830301173, -58.37301679283319800 ) ) ;
#86214 = CARTESIAN_POINT ( 'NONE',  ( 5.972312261546847800, -18.58614341180641816, 26.97788726184341357 ) ) ;
#86213 = CARTESIAN_POINT ( 'NONE',  ( -108.0662369917864680, -29.99999999999997513, 149.4678941581608740 ) ) ;
#86215 = FACE_OUTER_BOUND ( 'NONE', #93454, .T. ) ;
#86216 = CARTESIAN_POINT ( 'NONE',  ( -48.69069850261567467, -39.52191310650646727, 48.66776383025324293 ) ) ;
#86217 = VECTOR ( 'NONE', #74853, 1000.000000000000000 ) ;
#86218 = VERTEX_POINT ( 'NONE', #98124 ) ;
#86219 = CARTESIAN_POINT ( 'NONE',  ( -3.972937144959854283, 18.38799044701208985, 5.763666621267263146 ) ) ;
#86220 = ORIENTED_EDGE ( 'NONE', *, *, #86276, .T. ) ;
#86221 = CARTESIAN_POINT ( 'NONE',  ( 0.07858671332656751163, 13.70447791526909143, -49.25000000000000711 ) ) ;
#86222 = CONICAL_SURFACE ( 'NONE', #29417, 4.250000000000000000, 0.9599310885968754814 ) ;
#86223 = CARTESIAN_POINT ( 'NONE',  ( 5.982126593009819082, -6.026657721070697526, 0.5333292889181923124 ) ) ;
#86224 = EDGE_LOOP ( 'NONE', ( #89154, #42232 ) ) ;
#86225 = FACE_OUTER_BOUND ( 'NONE', #3133, .T. ) ;
#86226 = ORIENTED_EDGE ( 'NONE', *, *, #99492, .F. ) ;
#86227 = CARTESIAN_POINT ( 'NONE',  ( 77.56003102942109706, -30.00000000000500577, -26.29825542485684053 ) ) ;
#86228 = PRESENTATION_STYLE_ASSIGNMENT (( #85686 ) ) ;
#86229 = CARTESIAN_POINT ( 'NONE',  ( 3.883877898720186739, -48.93467900693710959, 104.5781496044256471 ) ) ;
#86230 = CARTESIAN_POINT ( 'NONE',  ( 7.149999999999998579, 41.65000000000000568, -59.82695526683419729 ) ) ;
#86231 = CARTESIAN_POINT ( 'NONE',  ( -15.50526908267491066, 41.99999999999999289, 57.69562748408483088 ) ) ;
#86232 = CARTESIAN_POINT ( 'NONE',  ( 96.01405531091515400, -30.00000000000000711, 191.2846317128013993 ) ) ;
#86233 = CARTESIAN_POINT ( 'NONE',  ( 70.89460441624491693, 6.975173280561618775E-15, 0.000000000000000000 ) ) ;
#86234 = ORIENTED_EDGE ( 'NONE', *, *, #76359, .F. ) ;
#86235 = VERTEX_POINT ( 'NONE', #57121 ) ;
#86236 = ORIENTED_EDGE ( 'NONE', *, *, #74077, .F. ) ;
#86237 = CARTESIAN_POINT ( 'NONE',  ( 55.20647631999140970, -18.68557819068131565, 52.51210417480952941 ) ) ;
#86238 = CARTESIAN_POINT ( 'NONE',  ( -44.12456444187882454, 435.3734385797342270, 10.68335876406171181 ) ) ;
#86239 = VECTOR ( 'NONE', #39970, 1000.000000000000000 ) ;
#86240 = CARTESIAN_POINT ( 'NONE',  ( -43.75401118688380819, 486.3173572309548263, 5.908089951475163915 ) ) ;
#86241 = ORIENTED_EDGE ( 'NONE', *, *, #51664, .T. ) ;
#86242 = CARTESIAN_POINT ( 'NONE',  ( -88.03604560337967655, -38.37098769885366067, -19.52574164018452407 ) ) ;
#86243 = TOROIDAL_SURFACE ( 'NONE', #105151, 7.500000000000006217, 5.000000000000000000 ) ;
#86244 = EDGE_LOOP ( 'NONE', ( #6499, #75075, #15791 ) ) ;
#86245 = DIRECTION ( 'NONE',  ( -0.5000000000000014433, 0.8660254037844379305, 0.000000000000000000 ) ) ;
#86246 = CARTESIAN_POINT ( 'NONE',  ( 105.2091447253385468, -38.39005253448742394, 197.2722285801829116 ) ) ;
#86247 = CARTESIAN_POINT ( 'NONE',  ( 13.51895206827688511, 20.10414958935020024, 7.058517651309981211 ) ) ;
#86248 = B_SPLINE_CURVE_WITH_KNOTS ( 'NONE', 3,
 ( #19470, #44777, #36712, #52307, #86307, #35104, #18931, #44235 ),
 .UNSPECIFIED., .F., .F.,
 ( 4, 2, 2, 4 ),
 ( 0.01358597261296601820, 0.01555715282820523473, 0.01654274293582484387, 0.01752833304344444953 ),
 .UNSPECIFIED. ) ;
#86249 = CARTESIAN_POINT ( 'NONE',  ( 85.09130552977511286, -52.70812209273635318, 5.152046609888252249 ) ) ;
#86250 = CARTESIAN_POINT ( 'NONE',  ( 33.06122231440979675, 369.6080732779042819, 23.70317340430991493 ) ) ;
#86251 = CARTESIAN_POINT ( 'NONE',  ( 42.48296590554126340, 485.4097859441455398, -3.498432987059889587 ) ) ;
#86252 = CARTESIAN_POINT ( 'NONE',  ( -44.35776761200799001, 435.2162786697447814, 12.88191835534828478 ) ) ;
#86253 = DIRECTION ( 'NONE',  ( 0.000000000000000000, 0.000000000000000000, 1.000000000000000000 ) ) ;
#86254 = ORIENTED_EDGE ( 'NONE', *, *, #106466, .F. ) ;
#86255 = EDGE_CURVE ( 'NONE', #47728, #78767, #30200, .T. ) ;
#86256 = CARTESIAN_POINT ( 'NONE',  ( 7.176538911681105581, 40.00000000337644224, -70.93639500526144559 ) ) ;
#86257 = CIRCLE ( 'NONE', #103400, 66.50000000000000000 ) ;
#86258 = CARTESIAN_POINT ( 'NONE',  ( -32.42385571103915964, 438.8717992898766624, 23.74935544307452062 ) ) ;
#86259 = VERTEX_POINT ( 'NONE', #82479 ) ;
#86260 = ADVANCED_FACE ( 'NONE', ( #448 ), #6083, .T. ) ;
#86261 = CARTESIAN_POINT ( 'NONE',  ( -20.40408973000767290, 304.8517363292163509, -9.000014075294032523 ) ) ;
#86262 = CARTESIAN_POINT ( 'NONE',  ( -41.06716693784987626, 327.3805982724676369, 9.858883544215990113 ) ) ;
#86263 = CARTESIAN_POINT ( 'NONE',  ( 0.8333405213146051205, -30.00000000000001421, 28.88964995960238369 ) ) ;
#86264 = CARTESIAN_POINT ( 'NONE',  ( 3.313708498984762496, -21.78124999999999645, 7.999999999999998224 ) ) ;
#86265 = CARTESIAN_POINT ( 'NONE',  ( 22.16406547723535070, -20.70551619972588142, 36.17276813359887910 ) ) ;
#86266 = EDGE_CURVE ( 'NONE', #35660, #8756, #26759, .T. ) ;
#86267 = EDGE_CURVE ( 'NONE', #17393, #45061, #91644, .T. ) ;
#86268 = DIRECTION ( 'NONE',  ( 0.000000000000000000, -0.9523642049634558626, 0.3049629831706212046 ) ) ;
#86269 = ORIENTED_EDGE ( 'NONE', *, *, #34890, .F. ) ;
#86270 = CARTESIAN_POINT ( 'NONE',  ( 83.19851726930752989, -53.68871273878280448, 186.7541703894078466 ) ) ;
#86271 = CARTESIAN_POINT ( 'NONE',  ( -37.56673239365849781, 27.60449318992554169, 13.45617127781067168 ) ) ;
#86272 = CARTESIAN_POINT ( 'NONE',  ( 5.691929483231184861, 5.629165124598851655, -3.249999999999999556 ) ) ;
#86273 = ORIENTED_EDGE ( 'NONE', *, *, #19513, .T. ) ;
#86274 = CARTESIAN_POINT ( 'NONE',  ( -87.75695610596812912, -52.70950093229972566, 47.57269196313494319 ) ) ;
#86276 = EDGE_CURVE ( 'NONE', #2627, #19372, #40956, .T. ) ;
#86275 = CIRCLE ( 'NONE', #12178, 5.000000000000001776 ) ;
#86277 = CARTESIAN_POINT ( 'NONE',  ( 0.4964154566687934422, 8.859816792613651515, -0.6543471694412388295 ) ) ;
#86278 = CARTESIAN_POINT ( 'NONE',  ( -11.90609530896320045, -5.000000000000002665, -79.26133957281672338 ) ) ;
#86279 = CARTESIAN_POINT ( 'NONE',  ( 17.91929324317266037, -4.333298119783741242, -0.09842992273139013204 ) ) ;
#86280 = CARTESIAN_POINT ( 'NONE',  ( 0.000000000000000000, 115.0000000000000000, 0.000000000000000000 ) ) ;
#86281 = AXIS2_PLACEMENT_3D ( 'NONE', #62673, #56667, #80950 ) ;
#86282 = CARTESIAN_POINT ( 'NONE',  ( 14.11578347234595654, -59.99999999999998579, 39.75482815772654988 ) ) ;
#86283 = CARTESIAN_POINT ( 'NONE',  ( 11.71459821192806672, -20.98522750155807515, 35.53716617024250723 ) ) ;
#86284 = CIRCLE ( 'NONE', #22625, 1.000000000000000000 ) ;
#86285 = CARTESIAN_POINT ( 'NONE',  ( 1.468822083365074915, -0.02842019993896785848, 101.6459669435634936 ) ) ;
#86286 = CARTESIAN_POINT ( 'NONE',  ( 45.15274496246701119, -28.34823788395991429, 40.23751332069821984 ) ) ;
#86288 = CARTESIAN_POINT ( 'NONE',  ( -13.09871712087400297, 21.81423054753162560, 4.750713512999053201 ) ) ;
#86287 = CARTESIAN_POINT ( 'NONE',  ( -37.53089333674191153, -36.72970239472569887, 46.80208549195887713 ) ) ;
#86289 = CIRCLE ( 'NONE', #10495, 4.000000000000001776 ) ;
#86290 = CARTESIAN_POINT ( 'NONE',  ( 2.295593195821269195, 298.7070635966626355, -10.00347380708956635 ) ) ;
#86291 = DIRECTION ( 'NONE',  ( -1.000000000000000000, -1.224606353822377258E-16, -0.000000000000000000 ) ) ;
#86292 = PRESENTATION_STYLE_ASSIGNMENT (( #19457 ) ) ;
#86293 = LINE ( 'NONE', #30171, #83838 ) ;
#86294 = LINE ( 'NONE', #68502, #82741 ) ;
#86295 = VERTEX_POINT ( 'NONE', #74370 ) ;
#86296 = DIRECTION ( 'NONE',  ( 0.000000000000000000, 0.000000000000000000, 1.000000000000000000 ) ) ;
#86297 = PRODUCT_DEFINITION_SHAPE ( 'NONE', 'NONE',  #27211 ) ;
#86298 = ORIENTED_EDGE ( 'NONE', *, *, #57707, .T. ) ;
#86299 = CARTESIAN_POINT ( 'NONE',  ( -10.64183635766278435, -0.9494289261200415941, 20.26979409943867694 ) ) ;
#86300 = CARTESIAN_POINT ( 'NONE',  ( 0.000000000000000000, 4.898587196589413815E-16, -4.000000000000000888 ) ) ;
#86302 = CARTESIAN_POINT ( 'NONE',  ( 1.602313057358263348, -60.22811021425470557, -36.92768096916045550 ) ) ;
#86301 = DIRECTION ( 'NONE',  ( 0.000000000000000000, -1.000000000000000000, 0.000000000000000000 ) ) ;
#86303 = EDGE_CURVE ( 'NONE', #98095, #70327, #73206, .T. ) ;
#86304 = B_SPLINE_CURVE_WITH_KNOTS ( 'NONE', 3,
 ( #29287, #96106, #55089, #11447, #77800, #29809 ),
 .UNSPECIFIED., .F., .F.,
 ( 4, 2, 4 ),
 ( 0.000000000000000000, 0.001995463903526787514, 0.003990927807053575027 ),
 .UNSPECIFIED. ) ;
#86305 = EDGE_LOOP ( 'NONE', ( #26761, #20948, #19160, #100638 ) ) ;
#86306 = MECHANICAL_DESIGN_GEOMETRIC_PRESENTATION_REPRESENTATION (  '', ( #44961 ), #77665 ) ;
#86307 = CARTESIAN_POINT ( 'NONE',  ( 9.988791316060179781, 294.6431201125005828, 0.5781485321568775593 ) ) ;
#86308 = CARTESIAN_POINT ( 'NONE',  ( -41.47545032233811924, 461.4488778950835126, 2.700315249222962954 ) ) ;
#86309 = VERTEX_POINT ( 'NONE', #57649 ) ;
#86310 = CIRCLE ( 'NONE', #22577, 6.499999999999999112 ) ;
#86311 = EDGE_CURVE ( 'NONE', #102376, #63754, #799, .T. ) ;
#86312 = EDGE_CURVE ( 'NONE', #96386, #64846, #8580, .T. ) ;
#86313 = CARTESIAN_POINT ( 'NONE',  ( 11.89131030317610183, 5.000000000000003553, 0.000000000000000000 ) ) ;
#86314 = AXIS2_PLACEMENT_3D ( 'NONE', #70976, #89291, #105976 ) ;
#86315 = LINE ( 'NONE', #85779, #106207 ) ;
#86316 = CARTESIAN_POINT ( 'NONE',  ( -92.08870864087261054, -60.00000000000000711, 20.32441657550419123 ) ) ;
#86317 = VERTEX_POINT ( 'NONE', #100778 ) ;
#86318 = DIRECTION ( 'NONE',  ( -1.000000000000000000, -1.224606353822377258E-16, -0.000000000000000000 ) ) ;
#86319 = DIRECTION ( 'NONE',  ( 0.000000000000000000, -1.000000000000000000, 0.000000000000000000 ) ) ;
#86320 = FACE_OUTER_BOUND ( 'NONE', #12452, .T. ) ;
#86321 = CARTESIAN_POINT ( 'NONE',  ( -9.948181520647858989, 26.13107197239622081, 1.049088206181488792 ) ) ;
#86322 = CARTESIAN_POINT ( 'NONE',  ( -81.08330333408508750, -53.42614166648503726, 174.1528431049000005 ) ) ;
#86323 = ORIENTED_EDGE ( 'NONE', *, *, #80262, .T. ) ;
#86324 = CARTESIAN_POINT ( 'NONE',  ( -11.24494283604955491, -0.000000000000000000, 12.81923949847508837 ) ) ;
#86325 = ORIENTED_EDGE ( 'NONE', *, *, #23958, .T. ) ;
#86326 = ORIENTED_EDGE ( 'NONE', *, *, #21550, .F. ) ;
#86327 = CARTESIAN_POINT ( 'NONE',  ( -8.812315315237404079, -5.000000000000578204, -14.88097931263728313 ) ) ;
#86328 =( NAMED_UNIT ( * ) SI_UNIT ( $, .STERADIAN. ) SOLID_ANGLE_UNIT ( ) );
#86329 = ORIENTED_EDGE ( 'NONE', *, *, #16463, .F. ) ;
#86330 = EDGE_CURVE ( 'NONE', #49122, #72914, #99076, .T. ) ;
#86331 = CIRCLE ( 'NONE', #24280, 1.000000000000000888 ) ;
#86332 = CARTESIAN_POINT ( 'NONE',  ( -21.96335563855659601, 28.05277650238785725, 31.83030418064915779 ) ) ;
#86333 = CARTESIAN_POINT ( 'NONE',  ( 87.04245038058458306, -5.000000000000000000, 0.000000000000000000 ) ) ;
#86334 = CARTESIAN_POINT ( 'NONE',  ( -94.13300556333170732, -57.67265947060198528, 21.91134835779649137 ) ) ;
#86335 = CARTESIAN_POINT ( 'NONE',  ( -4.497431761510337189, -65.54098124251032687, -3.972160586670089089 ) ) ;
#86336 = CARTESIAN_POINT ( 'NONE',  ( 0.000000000000000000, 6.928203230275505220, 4.000000000000006217 ) ) ;
#86337 = CARTESIAN_POINT ( 'NONE',  ( -9.221216839714873714, 103.9524025183102083, 3.869414262756992517 ) ) ;
#86338 = DIRECTION ( 'NONE',  ( 0.000000000000000000, 0.000000000000000000, 1.000000000000000000 ) ) ;
#86339 =( NAMED_UNIT ( * ) SI_UNIT ( $, .STERADIAN. ) SOLID_ANGLE_UNIT ( ) );
#86340 = CARTESIAN_POINT ( 'NONE',  ( 85.44123078815633221, -14.21045842199435505, -16.45204874176463150 ) ) ;
#86341 = EDGE_CURVE ( 'NONE', #73607, #59854, #51388, .T. ) ;
#86342 = CARTESIAN_POINT ( 'NONE',  ( -66.35297339498846725, -60.00000000000000000, 134.7723483620486888 ) ) ;
#86343 = CARTESIAN_POINT ( 'NONE',  ( -55.41494957456509951, -25.62128524555114240, 55.61161846345970616 ) ) ;
#86344 = EDGE_LOOP ( 'NONE', ( #26006, #106173, #13530, #37445, #16854, #18966 ) ) ;
#86345 =( LENGTH_UNIT ( ) NAMED_UNIT ( * ) SI_UNIT ( .MILLI., .METRE. ) );
#86346 = ORIENTED_EDGE ( 'NONE', *, *, #76195, .T. ) ;
#86347 = CARTESIAN_POINT ( 'NONE',  ( -100.8637650043404221, -52.73819914637954298, 193.5090766411508980 ) ) ;
#86348 = CARTESIAN_POINT ( 'NONE',  ( 101.7408511833992009, -38.00000000000000000, 185.5768760481534514 ) ) ;
#86349 = EDGE_CURVE ( 'NONE', #19064, #77149, #7765, .T. ) ;
#86350 = CARTESIAN_POINT ( 'NONE',  ( -1.098815040102374185, 51.92265547973028816, 8.383320812314803305 ) ) ;
#86351 = ORIENTED_EDGE ( 'NONE', *, *, #54383, .T. ) ;
#86352 = CARTESIAN_POINT ( 'NONE',  ( 19.48449119670739549, 49.99674463650651290, 60.21304372869956012 ) ) ;
#86353 = CIRCLE ( 'NONE', #82854, 5.000000000000011546 ) ;
#86354 = FACE_BOUND ( 'NONE', #48517, .T. ) ;
#86355 = CARTESIAN_POINT ( 'NONE',  ( -7.188101187500001821, -15.87500000204838635, -2.977408999572651371 ) ) ;
#86356 = CARTESIAN_POINT ( 'NONE',  ( -1.788439362206281746, -69.58817794431396919, 12.85214533551791938 ) ) ;
#86357 = CARTESIAN_POINT ( 'NONE',  ( 27.10511071441176867, 36.60571256639526894, -10.05698433968634653 ) ) ;
#86358 = CARTESIAN_POINT ( 'NONE',  ( 7.999912353029506207, -81.00017529396907889, -0.2691822806795012846 ) ) ;
#86359 = CARTESIAN_POINT ( 'NONE',  ( 66.08383350088368502, -30.00000000000000000, 83.36352947276506598 ) ) ;
#86360 = AXIS2_PLACEMENT_3D ( 'NONE', #88097, #6096, #70321 ) ;
#86361 = CARTESIAN_POINT ( 'NONE',  ( 31.02212611900126760, 360.5725590293961318, 22.12937154125974715 ) ) ;
#86362 = CARTESIAN_POINT ( 'NONE',  ( -9.266991278717167546, 140.2840666555874805, -0.000000000000000000 ) ) ;
#86363 =( NAMED_UNIT ( * ) SI_UNIT ( $, .STERADIAN. ) SOLID_ANGLE_UNIT ( ) );
#86364 = CARTESIAN_POINT ( 'NONE',  ( -7.500000000000004441, 23.94542680926433320, -45.46585527945179450 ) ) ;
#86365 = CARTESIAN_POINT ( 'NONE',  ( -26.60308663855274602, -22.09595682646055081, 29.10650421446171165 ) ) ;
#86366 =( GEOMETRIC_REPRESENTATION_CONTEXT ( 3 ) GLOBAL_UNCERTAINTY_ASSIGNED_CONTEXT ( ( #27350 ) ) GLOBAL_UNIT_ASSIGNED_CONTEXT ( ( #52303, #20545, #85212 ) ) REPRESENTATION_CONTEXT ( 'NONE', 'WORKASPACE' ) );
#86367 = CARTESIAN_POINT ( 'NONE',  ( 48.43983201128956040, -32.59978484401640486, 46.13064193097132915 ) ) ;
#86368 = DIRECTION ( 'NONE',  ( 1.000000000000000000, 1.224606353822377258E-16, 0.000000000000000000 ) ) ;
#86369 = AXIS2_PLACEMENT_3D ( 'NONE', #22537, #39235, #72109 ) ;
#86370 = CARTESIAN_POINT ( 'NONE',  ( 12.39854599882998798, 8.430153398135439957, -0.8386200322165747734 ) ) ;
#86371 = VECTOR ( 'NONE', #51072, 1000.000000000000000 ) ;
#86372 = CARTESIAN_POINT ( 'NONE',  ( -87.14751124570071283, -38.58929230054740600, 199.6078792464353171 ) ) ;
#86373 = ORIENTED_EDGE ( 'NONE', *, *, #44750, .T. ) ;
#86374 = CARTESIAN_POINT ( 'NONE',  ( 90.70427241161488041, -38.34270740108069475, 7.520233764197877591 ) ) ;
#86375 = CARTESIAN_POINT ( 'NONE',  ( 12.79866983394184743, 6.544424113613374061, -7.674868532166754242 ) ) ;
#86376 = CARTESIAN_POINT ( 'NONE',  ( -18.93379861527105135, 49.15505328154679887, 62.08065835375955288 ) ) ;
#86377 =( NAMED_UNIT ( * ) PLANE_ANGLE_UNIT ( ) SI_UNIT ( $, .RADIAN. ) );
#86378 = CARTESIAN_POINT ( 'NONE',  ( 5.563666575369232703, 41.08730259753766489, -70.97074977071341095 ) ) ;
#86379 = CARTESIAN_POINT ( 'NONE',  ( -32.74248746529113419, 435.3839305082926785, 16.93970874907590840 ) ) ;
#86380 = CARTESIAN_POINT ( 'NONE',  ( 8.000000000000000000, -17.09375000409676915, -3.313708498984761164 ) ) ;
#86381 = CARTESIAN_POINT ( 'NONE',  ( 32.37370863962282641, 435.2098570401744837, 18.54444254976758799 ) ) ;
#86382 = CARTESIAN_POINT ( 'NONE',  ( 111.2603429936217339, -60.00000000000000711, 185.9078983323155398 ) ) ;
#86383 = CARTESIAN_POINT ( 'NONE',  ( -7.986452802927061612, -68.97309757691888876, 0.5332468218996320175 ) ) ;
#86384 = ORIENTED_EDGE ( 'NONE', *, *, #87798, .F. ) ;
#86385 = CARTESIAN_POINT ( 'NONE',  ( 7.003653396366580353, 31.05706205559676647, -3.866846144092864090 ) ) ;
#86386 = ADVANCED_FACE ( 'NONE', ( #34504 ), #28458, .T. ) ;
#86387 = CARTESIAN_POINT ( 'NONE',  ( 0.000000000000000000, 0.000000000000000000, 4.000000000000000888 ) ) ;
#86388 = ORIENTED_EDGE ( 'NONE', *, *, #83815, .T. ) ;
#86390 = DIRECTION ( 'NONE',  ( 0.000000000000000000, -1.000000000000000000, 0.000000000000000000 ) ) ;
#86389 = CARTESIAN_POINT ( 'NONE',  ( -47.71178637004413758, -38.32472025489722256, 63.29349205809943157 ) ) ;
#86391 = DIRECTION ( 'NONE',  ( 1.000000000000000000, 0.000000000000000000, -0.000000000000000000 ) ) ;
#86392 = CARTESIAN_POINT ( 'NONE',  ( -6.990291106834061630, -2.999999999999999556, -4.028951842967198438 ) ) ;
#86393 = CARTESIAN_POINT ( 'NONE',  ( 41.61957457421982554, 435.6113505990638828, 7.035653009325279150 ) ) ;
#86394 = CARTESIAN_POINT ( 'NONE',  ( 2.977408999572651815, -10.81250000204838457, 7.188101187500000933 ) ) ;
#86395 = AXIS2_PLACEMENT_3D ( 'NONE', #37941, #14135, #13607 ) ;
#86396 = CARTESIAN_POINT ( 'NONE',  ( -2.617478844990583031, -3.000000000000002665, -94.73972676610416954 ) ) ;
#86397 = EDGE_CURVE ( 'NONE', #92683, #79234, #84073, .T. ) ;
#86398 = ADVANCED_FACE ( 'NONE', ( #68974 ), #74892, .T. ) ;
#86399 = CARTESIAN_POINT ( 'NONE',  ( 30.29489621385904385, 12.93001532776398577, -41.94819669044333210 ) ) ;
#86401 = ORIENTED_EDGE ( 'NONE', *, *, #41989, .F. ) ;
#86400 = CYLINDRICAL_SURFACE ( 'NONE', #16750, 1.250000000000001110 ) ;
#86402 = CARTESIAN_POINT ( 'NONE',  ( 81.65977408556862827, -53.47473748660239323, 179.0429556740298835 ) ) ;
#86403 = ADVANCED_FACE ( 'NONE', ( #12301 ), #1637, .F. ) ;
#86404 = CARTESIAN_POINT ( 'NONE',  ( 9.209599246271393369, 12.38267295484908459, 0.000000000000000000 ) ) ;
#86406 = EDGE_CURVE ( 'NONE', #9002, #81288, #42937, .T. ) ;
#86405 = CARTESIAN_POINT ( 'NONE',  ( 9.177080501238306098, 85.53346942854270196, -3.972956046786645601 ) ) ;
#86407 = ORIENTED_EDGE ( 'NONE', *, *, #98895, .T. ) ;
#86408 = DIRECTION ( 'NONE',  ( 0.000000000000000000, -1.000000000000000000, 0.000000000000000000 ) ) ;
#86409 = EDGE_CURVE ( 'NONE', #87879, #214, #15493, .T. ) ;
#86410 = ADVANCED_FACE ( 'NONE', ( #64589 ), #50796, .T. ) ;
#86411 = DIRECTION ( 'NONE',  ( 0.000000000000000000, 0.000000000000000000, 1.000000000000000000 ) ) ;
#86412 = CARTESIAN_POINT ( 'NONE',  ( 0.000000000000000000, 0.000000000000000000, 0.000000000000000000 ) ) ;
#86413 = CARTESIAN_POINT ( 'NONE',  ( -29.07948315939603745, 13.68628896012808838, -39.75806671536133763 ) ) ;
#86414 = CARTESIAN_POINT ( 'NONE',  ( 1.115575871468929448, 14.48101611498047703, 51.08097729577264090 ) ) ;
#86415 = ORIENTED_EDGE ( 'NONE', *, *, #90788, .T. ) ;
#86416 = B_SPLINE_CURVE_WITH_KNOTS ( 'NONE', 3,
 ( #13970, #79780, #104584, #63626, #22648, #88420, #47405, #6410, #39348, #72227, #64154, #25855, #100741, #2042, #84038, #33925, #75944, #18815, #51120, #91612 ),
 .UNSPECIFIED., .F., .F.,
 ( 4, 2, 2, 2, 2, 2, 2, 2, 2, 4 ),
 ( 0.003145779775862817158, 0.003652023435422363865, 0.004158267094981910571, 0.004411388924761685225, 0.004664510754541460746, 0.005170754414101012657, 0.005676998073660564567, 0.006183241733220117345, 0.006689485392779668388, 0.007195729052339221166 ),
 .UNSPECIFIED. ) ;
#86417 =( LENGTH_UNIT ( ) NAMED_UNIT ( * ) SI_UNIT ( .MILLI., .METRE. ) );
#86418 = DIRECTION ( 'NONE',  ( -1.000000000000000000, -1.224606353822377258E-16, -0.000000000000000000 ) ) ;
#86419 = DIRECTION ( 'NONE',  ( 0.000000000000000000, -1.000000000000000000, 0.000000000000000000 ) ) ;
#86420 = DIRECTION ( 'NONE',  ( -1.000000000000000000, -1.224606353822377258E-16, -0.000000000000000000 ) ) ;
#86422 = DIRECTION ( 'NONE',  ( -1.000000000000000000, -0.000000000000000000, -0.000000000000000000 ) ) ;
#86421 = DIRECTION ( 'NONE',  ( 0.000000000000000000, 0.000000000000000000, -1.000000000000000000 ) ) ;
#86423 = CARTESIAN_POINT ( 'NONE',  ( -5.082755093536325042, -24.59375000204838813, -5.082755093536325930 ) ) ;
#86424 = DIRECTION ( 'NONE',  ( -1.000000000000000000, -1.224606353822377258E-16, -0.000000000000000000 ) ) ;
#86425 = CARTESIAN_POINT ( 'NONE',  ( 1.469576158976823947E-15, -78.00000000000000000, 15.00000000000000000 ) ) ;
#86426 = CARTESIAN_POINT ( 'NONE',  ( 1.517883041479706208E-15, -5.000000000000000888, -97.00000000000000000 ) ) ;
#86427 = ORIENTED_EDGE ( 'NONE', *, *, #5996, .T. ) ;
#86428 = AXIS2_PLACEMENT_3D ( 'NONE', #93318, #2699, #93848 ) ;
#86429 =( GEOMETRIC_REPRESENTATION_CONTEXT ( 3 ) GLOBAL_UNCERTAINTY_ASSIGNED_CONTEXT ( ( #76905 ) ) GLOBAL_UNIT_ASSIGNED_CONTEXT ( ( #98561, #66741, #74287 ) ) REPRESENTATION_CONTEXT ( 'NONE', 'WORKASPACE' ) );
#86430 = CARTESIAN_POINT ( 'NONE',  ( -5.290067270632269114, -1.200000000000000030E-05, -6.031152949374520844 ) ) ;
#86432 = DIRECTION ( 'NONE',  ( -3.700743415416444046E-15, 0.000000000000000000, 1.000000000000000000 ) ) ;
#86431 =( BOUNDED_SURFACE ( )  B_SPLINE_SURFACE ( 1, 2, ( 
 ( #64172, #431, #74875, #16661, #40401, #82991, #52604, #65748, #106722, #98628, #16123, #81908, #58175, #33400, #35952, #58729, #91628, #91102, #7485, #8024, #50598, #32871, #74353, #9086, #33943, #90018, #41995, #41463, #106178, #99158, #17738, #84991, #66271, #73283, #50085, #963, #3001, #43999, #57104, #11074, #32341, #24778, #27867, #40934, #76885, #98105, #24256, #68824, #99702, #49007, #57627, #73828, #93621, #101704, #66812, #60732, #49551, #19775, #90552, #82458, #65211, #8561, #25316, #25872, #17210, #38072, #70407, #45608, #22413, #28931, #21880, #37541, #46132, #69353, #87657, #53161, #95217, #104343, #12149, #36485, #78482, #71445, #70927, #45080, #85534, #20846, #86611, #62324, #12675, #102232, #28382, #54721, #13739, #103306, #61257, #30492, #46646, #29451, #63393, #87128, #20315, #77960, #86078, #62853, #103820, #94143, #3546, #11612, #4075, #44541, #29964, #37006, #61805, #69873, #102767, #94698, #95739, #5138, #13205, #53677, #4609, #96288, #79546, #79020, #21350, #77431, #5658, #54190, #38580, #73024, #41209, #49284, #24532, #81128, #16401, #66015, #98380, #32079, #7238, #96805, #74095, #47696, #71988, #47168, #80069, #80596, #7769, #6717, #33146, #97315, #105932, #6176, #82187, #64955, #57376, #90292, #8305, #39643, #64442, #40673, #181, #98894, #55257, #97848, #88182, #39109, #24006, #104899, #14267, #31038, #63918, #22936, #81642, #55774, #88709, #56850, #14802, #32620, #72513, #73560, #105419, #31559, #106462, #40146, #23467, #89772, #56304, #89243, #15341, #48225, #15872, #48748, #65493, #76226, #83782, #92407, #99972, #34752, #25604, #27194, #42803, #50347, #25055, #18013, #1796, #9894, #10945, #58462, #26143, #67089, #67625, #83258, #91886, #91371, #26660, #92948, #100503, #59539, #34217, #17485, #10427, #58998, #9351, #19110, #42262, #75154, #50878, #1247, #2866, #18556, #75697, #51419, #84332, #43343, #57909, #2332, #68700, #35274, #68145, #101039, #33674, #99425, #60084, #51948, #84863, #43866, #76758, #35819, #90834, #16949, #49827, #82732, #8834, #41738, #74625, #703, #66547, #28257, #37942, #61681, #62720, #77303, #21751, #94569, #3418, #45481, #5530, #53557, #69229 ),
 ( #70802, #69747, #46521, #46003, #86488, #62211, #102642, #4474, #102098, #103697, #12546, #20178, #101579, #20719, #78352, #37413, #87526, #61127, #28798, #36880, #70277, #53028, #103176, #94018, #29319, #95609, #95094, #21230, #3948, #85951, #87003, #54059, #12022, #54587, #44954, #77837, #13074, #78883, #79418, #5010, #29843, #13608, #38456, #27738, #60609, #93500, #19647, #52480, #85398, #11481, #36360, #44409, #15207, #97185, #98253, #15741, #48624, #90165, #47570, #72383, #31950, #56719, #23329, #105289, #80994, #73433, #47039, #104753, #7630, #31436, #32491, #79938, #24407, #64313, #6048, #48095, #82059, #56170, #38974, #89640, #64831, #7111, #40027, #63784, #23875, #22807, #49154, #6577, #72900, #96145, #65362, #105810, #40549, #106324, #57245, #96671, #80465, #81509, #16269, #8179, #71322, #97710, #104216, #63252, #30361, #22278, #55125, #88055, #71847, #14136, #30904, #55643, #88578, #89111, #14660, #39509, #35146, #67497, #25471, #84735, #59411, #26017, #50233, #58877, #68016, #43214, #84204, #17891, #100902, #33022, #83649, #65887, #18976, #41085, #49701, #24923, #100376, #51820, #8709, #91769, #48, #18429, #27070, #26539, #58327, #73968, #92275, #50743, #83135, #9761, #98770, #82605, #17359, #57777, #10300, #9232, #92819, #51283, #99845, #1669, #42137, #42675, #41617, #76098, #75574, #66415, #90705, #34094, #34626, #2199, #59953, #74501, #75023, #1121, #16814, #99298, #66967, #577, #33541, #91251, #94437, #20597, #20049, #77175, #103051, #44824, #69097, #78747, #101970, #28130, #77710, #61008, #95477, #12420, #85820, #3821, #78230, #52897, #43739, #86355, #54453, #93892, #3287, #11897, #19518, #85265, #61543, #36758, #37817, #62080, #94970, #29718, #69624, #102515, #4345, #29206, #28659, #53435, #45351, #12948, #93366, #44281, #53939, #37280, #4881, #52353, #70675, #70146, #11349, #21108, #21621, #86874, #36227, #45868, #103569, #62593, #10818, #76627, #2738, #35693, #68568, #101453, #27605, #60486, #81392, #31304, #23741, #56592, #48497, #79816, #96548, #72774, #64190, #73300, #88980, #22144, #14006, #54995, #64703, #39900, #30229, #5410, #13478, #63116, #24272, #105680, #5920, #30774, #104090 ) ),
 .UNSPECIFIED., .F., .F., .T. ) 
 B_SPLINE_SURFACE_WITH_KNOTS ( ( 2, 2 ),
 ( 3, 2, 2, 2, 2, 2, 2, 2, 2, 2, 2, 2, 2, 2, 2, 2, 2, 2, 2, 2, 2, 2, 2, 2, 2, 2, 2, 2, 2, 2, 2, 2, 2, 2, 2, 2, 2, 2, 2, 2, 2, 2, 2, 2, 2, 2, 2, 2, 2, 2, 2, 2, 2, 2, 2, 2, 2, 2, 2, 2, 2, 2, 2, 2, 2, 2, 2, 2, 2, 2, 2, 2, 2, 2, 2, 2, 2, 2, 2, 2, 2, 2, 2, 2, 2, 2, 2, 2, 2, 2, 2, 2, 2, 2, 2, 2, 2, 2, 2, 2, 2, 2, 2, 2, 2, 2, 2, 2, 2, 2, 2, 2, 2, 2, 2, 2, 2, 2, 2, 2, 2, 2, 2, 2, 2, 2, 2, 2, 2, 2, 2, 2, 2, 2, 3 ),
 ( 0.000000000000000000, 1.000000000000000000 ),
 ( 0.000000000000000000, 0.007352941176470588133, 0.01470588235294117627, 0.02205882352941176613, 0.02941176470588235253, 0.03676470588235294240, 0.04411764705882353227, 0.05147058823529411520, 0.05882352941176470507, 0.06617647058823529493, 0.07352941176470588480, 0.08088235294117647467, 0.08823529411764706454, 0.09558823529411764053, 0.1029411764705882304, 0.1102941176470588203, 0.1176470588235294101, 0.1250000000000000000, 0.1323529411764705899, 0.1397058823529411797, 0.1470588235294117696, 0.1544117647058823595, 0.1617647058823529493, 0.1691176470588235392, 0.1764705882352941291, 0.1838235294117647189, 0.1911764705882352811, 0.1985294117647058709, 0.2058823529411764608, 0.2132352941176470507, 0.2205882352941176405, 0.2279411764705882304, 0.2352941176470588203, 0.2426470588235294101, 0.2500000000000000000, 0.2573529411764705621, 0.2647058823529411797, 0.2720588235294117418, 0.2794117647058823595, 0.2867647058823529216, 0.2941176470588235392, 0.3014705882352941013, 0.3088235294117647189, 0.3161764705882352811, 0.3235294117647058987, 0.3308823529411764608, 0.3382352941176470784, 0.3455882352941176405, 0.3529411764705882582, 0.3602941176470588203, 0.3676470588235294379, 0.3750000000000000000, 0.3823529411764705621, 0.3897058823529411797, 0.3970588235294117418, 0.4044117647058823595, 0.4117647058823529216, 0.4191176470588235392, 0.4264705882352941013, 0.4338235294117647189, 0.4411764705882352811, 0.4485294117647058987, 0.4558823529411764608, 0.4632352941176470784, 0.4705882352941176405, 0.4779411764705882582, 0.4852941176470588203, 0.4926470588235294379, 0.5000000000000000000, 0.5073529411764705621, 0.5147058823529411242, 0.5220588235294117974, 0.5294117647058823595, 0.5367647058823529216, 0.5441176470588234837, 0.5514705882352941568, 0.5588235294117647189, 0.5661764705882352811, 0.5735294117647058432, 0.5808823529411765163, 0.5882352941176470784, 0.5955882352941176405, 0.6029411764705882026, 0.6102941176470588758, 0.6176470588235294379, 0.6250000000000000000, 0.6323529411764705621, 0.6397058823529411242, 0.6470588235294117974, 0.6544117647058823595, 0.6617647058823529216, 0.6691176470588234837, 0.6764705882352941568, 0.6838235294117647189, 0.6911764705882352811, 0.6985294117647058432, 0.7058823529411765163, 0.7132352941176470784, 0.7205882352941176405, 0.7279411764705882026, 0.7352941176470588758, 0.7426470588235294379, 0.7500000000000000000, 0.7573529411764705621, 0.7647058823529411242, 0.7720588235294117974, 0.7794117647058823595, 0.7867647058823529216, 0.7941176470588234837, 0.8014705882352941568, 0.8088235294117647189, 0.8161764705882352811, 0.8235294117647058432, 0.8308823529411765163, 0.8382352941176470784, 0.8455882352941176405, 0.8529411764705882026, 0.8602941176470588758, 0.8676470588235294379, 0.8750000000000000000, 0.8823529411764705621, 0.8897058823529411242, 0.8970588235294117974, 0.9044117647058823595, 0.9117647058823529216, 0.9191176470588234837, 0.9264705882352941568, 0.9338235294117647189, 0.9411764705882352811, 0.9485294117647058432, 0.9558823529411765163, 0.9632352941176470784, 0.9705882352941176405, 0.9779411764705882026, 0.9804062476879973342 ),
 .UNSPECIFIED. ) 
 GEOMETRIC_REPRESENTATION_ITEM ( )  RATIONAL_B_SPLINE_SURFACE ( (
 ( 1.000000000000000000, 0.9238795325112867385, 1.000000000000000000, 0.9238795325112867385, 1.000000000000000000, 0.9238795325112867385, 1.000000000000000000, 0.9238795325112867385, 1.000000000000000000, 0.9238795325112867385, 1.000000000000000000, 0.9238795325112867385, 1.000000000000000000, 0.9238795325112867385, 1.000000000000000000, 0.9238795325112867385, 1.000000000000000000, 0.9238795325112867385, 1.000000000000000000, 0.9238795325112867385, 1.000000000000000000, 0.9238795325112867385, 1.000000000000000000, 0.9238795325112867385, 1.000000000000000000, 0.9238795325112867385, 1.000000000000000000, 0.9238795325112867385, 1.000000000000000000, 0.9238795325112867385, 1.000000000000000000, 0.9238795325112867385, 1.000000000000000000, 0.9238795325112867385, 1.000000000000000000, 0.9238795325112867385, 1.000000000000000000, 0.9238795325112867385, 1.000000000000000000, 0.9238795325112867385, 1.000000000000000000, 0.9238795325112867385, 1.000000000000000000, 0.9238795325112867385, 1.000000000000000000, 0.9238795325112867385, 1.000000000000000000, 0.9238795325112867385, 1.000000000000000000, 0.9238795325112867385, 1.000000000000000000, 0.9238795325112867385, 1.000000000000000000, 0.9238795325112867385, 1.000000000000000000, 0.9238795325112867385, 1.000000000000000000, 0.9238795325112867385, 1.000000000000000000, 0.9238795325112867385, 1.000000000000000000, 0.9238795325112867385, 1.000000000000000000, 0.9238795325112867385, 1.000000000000000000, 0.9238795325112867385, 1.000000000000000000, 0.9238795325112867385, 1.000000000000000000, 0.9238795325112867385, 1.000000000000000000, 0.9238795325112867385, 1.000000000000000000, 0.9238795325112867385, 1.000000000000000000, 0.9238795325112867385, 1.000000000000000000, 0.9238795325112867385, 1.000000000000000000, 0.9238795325112867385, 1.000000000000000000, 0.9238795325112867385, 1.000000000000000000, 0.9238795325112867385, 1.000000000000000000, 0.9238795325112867385, 1.000000000000000000, 0.9238795325112867385, 1.000000000000000000, 0.9238795325112867385, 1.000000000000000000, 0.9238795325112867385, 1.000000000000000000, 0.9238795325112867385, 1.000000000000000000, 0.9238795325112867385, 1.000000000000000000, 0.9238795325112867385, 1.000000000000000000, 0.9238795325112867385, 1.000000000000000000, 0.9238795325112867385, 1.000000000000000000, 0.9238795325112867385, 1.000000000000000000, 0.9238795325112867385, 1.000000000000000000, 0.9238795325112867385, 1.000000000000000000, 0.9238795325112867385, 1.000000000000000000, 0.9238795325112867385, 1.000000000000000000, 0.9238795325112867385, 1.000000000000000000, 0.9238795325112867385, 1.000000000000000000, 0.9238795325112867385, 1.000000000000000000, 0.9238795325112867385, 1.000000000000000000, 0.9238795325112867385, 1.000000000000000000, 0.9238795325112867385, 1.000000000000000000, 0.9238795325112867385, 1.000000000000000000, 0.9238795325112867385, 1.000000000000000000, 0.9238795325112867385, 1.000000000000000000, 0.9238795325112867385, 1.000000000000000000, 0.9238795325112867385, 1.000000000000000000, 0.9238795325112867385, 1.000000000000000000, 0.9238795325112867385, 1.000000000000000000, 0.9238795325112867385, 1.000000000000000000, 0.9238795325112867385, 1.000000000000000000, 0.9238795325112867385, 1.000000000000000000, 0.9238795325112867385, 1.000000000000000000, 0.9238795325112867385, 1.000000000000000000, 0.9238795325112867385, 1.000000000000000000, 0.9238795325112867385, 1.000000000000000000, 0.9238795325112867385, 1.000000000000000000, 0.9238795325112867385, 1.000000000000000000, 0.9238795325112867385, 1.000000000000000000, 0.9238795325112867385, 1.000000000000000000, 0.9238795325112867385, 1.000000000000000000, 0.9238795325112867385, 1.000000000000000000, 0.9238795325112867385, 1.000000000000000000, 0.9238795325112867385, 1.000000000000000000, 0.9238795325112867385, 1.000000000000000000, 0.9238795325112867385, 1.000000000000000000, 0.9238795325112867385, 1.000000000000000000, 0.9238795325112867385, 1.000000000000000000, 0.9238795325112867385, 1.000000000000000000, 0.9238795325112867385, 1.000000000000000000, 0.9238795325112867385, 1.000000000000000000, 0.9238795325112867385, 1.000000000000000000, 0.9238795325112867385, 1.000000000000000000, 0.9238795325112867385, 1.000000000000000000, 0.9238795325112867385, 1.000000000000000000, 0.9238795325112867385, 1.000000000000000000, 0.9238795325112867385, 1.000000000000000000, 0.9238795325112867385, 1.000000000000000000, 0.9238795325112867385, 1.000000000000000000, 0.9238795325112867385, 1.000000000000000000, 0.9238795325112867385, 1.000000000000000000, 0.9238795325112867385, 1.000000000000000000, 0.9238795325112867385, 1.000000000000000000, 0.9238795325112867385, 1.000000000000000000, 0.9238795325112867385, 1.000000000000000000, 0.9238795325112867385, 1.000000000000000000, 0.9238795325112867385, 1.000000000000000000, 0.9238795325112867385, 1.000000000000000000, 0.9238795325112867385, 1.000000000000000000, 0.9238795325112867385, 1.000000000000000000, 0.9238795325112867385, 1.000000000000000000, 0.9238795325112867385, 1.000000000000000000, 0.9238795325112867385, 1.000000000000000000, 0.9238795325112867385, 1.000000000000000000, 0.9238795325112867385, 1.000000000000000000, 0.9238795325112867385, 1.000000000000000000, 0.9238795325112867385, 1.000000000000000000, 0.9238795325112867385, 1.000000000000000000, 0.9238795325112867385, 1.000000000000000000, 0.9238795325112867385, 1.000000000000000000, 0.9238795325112867385, 1.000000000000000000, 0.9238795325112867385, 1.000000000000000000, 0.9238795325112867385, 1.000000000000000000, 0.9238795325112867385, 1.000000000000000000, 0.9238795325112867385, 1.000000000000000000, 0.9238795325112867385, 1.000000000000000000, 0.9238795325112867385, 1.000000000000000000, 0.9238795325112867385, 1.000000000000000000, 0.9238795325112867385, 1.000000000000000000, 0.9238795325112867385, 1.000000000000000000, 0.9238795325112867385, 1.000000000000000000, 0.9238795325112867385, 1.000000000000000000, 0.9238795325112867385, 1.000000000000000000, 0.9744806372091472380, 0.9660719911213342392),
 ( 1.000000000000000000, 0.9238795325112867385, 1.000000000000000000, 0.9238795325112867385, 1.000000000000000000, 0.9238795325112867385, 1.000000000000000000, 0.9238795325112867385, 1.000000000000000000, 0.9238795325112867385, 1.000000000000000000, 0.9238795325112867385, 1.000000000000000000, 0.9238795325112867385, 1.000000000000000000, 0.9238795325112867385, 1.000000000000000000, 0.9238795325112867385, 1.000000000000000000, 0.9238795325112867385, 1.000000000000000000, 0.9238795325112867385, 1.000000000000000000, 0.9238795325112867385, 1.000000000000000000, 0.9238795325112867385, 1.000000000000000000, 0.9238795325112867385, 1.000000000000000000, 0.9238795325112867385, 1.000000000000000000, 0.9238795325112867385, 1.000000000000000000, 0.9238795325112867385, 1.000000000000000000, 0.9238795325112867385, 1.000000000000000000, 0.9238795325112867385, 1.000000000000000000, 0.9238795325112867385, 1.000000000000000000, 0.9238795325112867385, 1.000000000000000000, 0.9238795325112867385, 1.000000000000000000, 0.9238795325112867385, 1.000000000000000000, 0.9238795325112867385, 1.000000000000000000, 0.9238795325112867385, 1.000000000000000000, 0.9238795325112867385, 1.000000000000000000, 0.9238795325112867385, 1.000000000000000000, 0.9238795325112867385, 1.000000000000000000, 0.9238795325112867385, 1.000000000000000000, 0.9238795325112867385, 1.000000000000000000, 0.9238795325112867385, 1.000000000000000000, 0.9238795325112867385, 1.000000000000000000, 0.9238795325112867385, 1.000000000000000000, 0.9238795325112867385, 1.000000000000000000, 0.9238795325112867385, 1.000000000000000000, 0.9238795325112867385, 1.000000000000000000, 0.9238795325112867385, 1.000000000000000000, 0.9238795325112867385, 1.000000000000000000, 0.9238795325112867385, 1.000000000000000000, 0.9238795325112867385, 1.000000000000000000, 0.9238795325112867385, 1.000000000000000000, 0.9238795325112867385, 1.000000000000000000, 0.9238795325112867385, 1.000000000000000000, 0.9238795325112867385, 1.000000000000000000, 0.9238795325112867385, 1.000000000000000000, 0.9238795325112867385, 1.000000000000000000, 0.9238795325112867385, 1.000000000000000000, 0.9238795325112867385, 1.000000000000000000, 0.9238795325112867385, 1.000000000000000000, 0.9238795325112867385, 1.000000000000000000, 0.9238795325112867385, 1.000000000000000000, 0.9238795325112867385, 1.000000000000000000, 0.9238795325112867385, 1.000000000000000000, 0.9238795325112867385, 1.000000000000000000, 0.9238795325112867385, 1.000000000000000000, 0.9238795325112867385, 1.000000000000000000, 0.9238795325112867385, 1.000000000000000000, 0.9238795325112867385, 1.000000000000000000, 0.9238795325112867385, 1.000000000000000000, 0.9238795325112867385, 1.000000000000000000, 0.9238795325112867385, 1.000000000000000000, 0.9238795325112867385, 1.000000000000000000, 0.9238795325112867385, 1.000000000000000000, 0.9238795325112867385, 1.000000000000000000, 0.9238795325112867385, 1.000000000000000000, 0.9238795325112867385, 1.000000000000000000, 0.9238795325112867385, 1.000000000000000000, 0.9238795325112867385, 1.000000000000000000, 0.9238795325112867385, 1.000000000000000000, 0.9238795325112867385, 1.000000000000000000, 0.9238795325112867385, 1.000000000000000000, 0.9238795325112867385, 1.000000000000000000, 0.9238795325112867385, 1.000000000000000000, 0.9238795325112867385, 1.000000000000000000, 0.9238795325112867385, 1.000000000000000000, 0.9238795325112867385, 1.000000000000000000, 0.9238795325112867385, 1.000000000000000000, 0.9238795325112867385, 1.000000000000000000, 0.9238795325112867385, 1.000000000000000000, 0.9238795325112867385, 1.000000000000000000, 0.9238795325112867385, 1.000000000000000000, 0.9238795325112867385, 1.000000000000000000, 0.9238795325112867385, 1.000000000000000000, 0.9238795325112867385, 1.000000000000000000, 0.9238795325112867385, 1.000000000000000000, 0.9238795325112867385, 1.000000000000000000, 0.9238795325112867385, 1.000000000000000000, 0.9238795325112867385, 1.000000000000000000, 0.9238795325112867385, 1.000000000000000000, 0.9238795325112867385, 1.000000000000000000, 0.9238795325112867385, 1.000000000000000000, 0.9238795325112867385, 1.000000000000000000, 0.9238795325112867385, 1.000000000000000000, 0.9238795325112867385, 1.000000000000000000, 0.9238795325112867385, 1.000000000000000000, 0.9238795325112867385, 1.000000000000000000, 0.9238795325112867385, 1.000000000000000000, 0.9238795325112867385, 1.000000000000000000, 0.9238795325112867385, 1.000000000000000000, 0.9238795325112867385, 1.000000000000000000, 0.9238795325112867385, 1.000000000000000000, 0.9238795325112867385, 1.000000000000000000, 0.9238795325112867385, 1.000000000000000000, 0.9238795325112867385, 1.000000000000000000, 0.9238795325112867385, 1.000000000000000000, 0.9238795325112867385, 1.000000000000000000, 0.9238795325112867385, 1.000000000000000000, 0.9238795325112867385, 1.000000000000000000, 0.9238795325112867385, 1.000000000000000000, 0.9238795325112867385, 1.000000000000000000, 0.9238795325112867385, 1.000000000000000000, 0.9238795325112867385, 1.000000000000000000, 0.9238795325112867385, 1.000000000000000000, 0.9238795325112867385, 1.000000000000000000, 0.9238795325112867385, 1.000000000000000000, 0.9238795325112867385, 1.000000000000000000, 0.9238795325112867385, 1.000000000000000000, 0.9238795325112867385, 1.000000000000000000, 0.9238795325112867385, 1.000000000000000000, 0.9238795325112867385, 1.000000000000000000, 0.9238795325112867385, 1.000000000000000000, 0.9238795325112867385, 1.000000000000000000, 0.9238795325112867385, 1.000000000000000000, 0.9238795325112867385, 1.000000000000000000, 0.9238795325112867385, 1.000000000000000000, 0.9238795325112867385, 1.000000000000000000, 0.9238795325112867385, 1.000000000000000000, 0.9238795325112867385, 1.000000000000000000, 0.9238795325112867385, 1.000000000000000000, 0.9238795325112867385, 1.000000000000000000, 0.9238795325112867385, 1.000000000000000000, 0.9238795325112867385, 1.000000000000000000, 0.9238795325112867385, 1.000000000000000000, 0.9744806372091472380, 0.9660719911213342392) ) ) 
 REPRESENTATION_ITEM ( '' )  SURFACE ( )  );
#86433 = CONICAL_SURFACE ( 'NONE', #8931, 3.309499999999999886, 0.7853981633974369547 ) ;
#86434 = CARTESIAN_POINT ( 'NONE',  ( -2.883699206286927996, 61.97772922454487343, -4.999999999999999112 ) ) ;
#86435 = ORIENTED_EDGE ( 'NONE', *, *, #100591, .T. ) ;
#86436 = CARTESIAN_POINT ( 'NONE',  ( -33.00000000000000000, 500.0000000000002274, -12.00000000000000711 ) ) ;
#86437 = CARTESIAN_POINT ( 'NONE',  ( -12.13034742782428133, 49.99999999999999289, -93.82352941176471006 ) ) ;
#86439 = ORIENTED_EDGE ( 'NONE', *, *, #88929, .F. ) ;
#86438 = CONICAL_SURFACE ( 'NONE', #39914, 4.000000000000001776, 0.9599310885968808105 ) ;
#86440 = EDGE_CURVE ( 'NONE', #52615, #102808, #4314, .T. ) ;
#86442 = SURFACE_STYLE_USAGE ( .BOTH. , #88010 ) ;
#86441 = AXIS2_PLACEMENT_3D ( 'NONE', #42475, #9038, #41944 ) ;
#86443 = CARTESIAN_POINT ( 'NONE',  ( -3.215218824033863498, -1.016378598479024120, 104.3206516315225798 ) ) ;
#86444 = CARTESIAN_POINT ( 'NONE',  ( 9.221249107921748234, 103.9517862850151602, 3.869340886054262629 ) ) ;
#86445 =( NAMED_UNIT ( * ) SI_UNIT ( $, .STERADIAN. ) SOLID_ANGLE_UNIT ( ) );
#86446 = B_SPLINE_CURVE_WITH_KNOTS ( 'NONE', 3,
 ( #77226, #59465, #11407, #68625, #10352, #17940 ),
 .UNSPECIFIED., .F., .F.,
 ( 4, 2, 4 ),
 ( 0.000000000000000000, 0.005272480446829030769, 0.01054496089365805633 ),
 .UNSPECIFIED. ) ;
#86447 = CARTESIAN_POINT ( 'NONE',  ( -111.1425918653686864, -60.00000000000000000, 186.5575091249358763 ) ) ;
#86448 = CARTESIAN_POINT ( 'NONE',  ( 6.231493956936416723, 147.8264543773111654, 5.000000000000000000 ) ) ;
#86449 = CARTESIAN_POINT ( 'NONE',  ( 53.78349330513380266, 6.975173280561618775E-15, 0.000000000000000000 ) ) ;
#86450 = CARTESIAN_POINT ( 'NONE',  ( 6.509902245423385914, 53.49555288916370444, -7.566134441555309564 ) ) ;
#86451 = FACE_OUTER_BOUND ( 'NONE', #75314, .T. ) ;
#86452 = B_SPLINE_CURVE_WITH_KNOTS ( 'NONE', 3,
 ( #31605, #8354, #64489, #88232, #105977, #81175 ),
 .UNSPECIFIED., .F., .F.,
 ( 4, 2, 4 ),
 ( -4.604908129294629295E-06, 0.0003318387708540386852, 0.0006682824498373720733 ),
 .UNSPECIFIED. ) ;
#86453 = CARTESIAN_POINT ( 'NONE',  ( -83.33205040470181757, -50.10390547248005078, 184.7201514412779488 ) ) ;
#86454 = DIRECTION ( 'NONE',  ( 0.000000000000000000, 1.000000000000000000, 0.000000000000000000 ) ) ;
#86455 = ORIENTED_EDGE ( 'NONE', *, *, #64377, .T. ) ;
#86457 = EDGE_CURVE ( 'NONE', #27178, #9659, #62998, .T. ) ;
#86456 = CARTESIAN_POINT ( 'NONE',  ( -9.177191262247262671, 46.16966304056472126, -13.55798985375341204 ) ) ;
#86458 =( BOUNDED_SURFACE ( )  B_SPLINE_SURFACE ( 3, 2, ( 
 ( #13224, #61274, #54207 ),
 ( #46152, #94164, #87146 ),
 ( #20333, #11631, #53179 ),
 ( #44563, #12167, #45099 ),
 ( #61822, #20865, #64458 ),
 ( #40689, #48242, #56864 ),
 ( #22432, #24022, #74112 ),
 ( #97330, #48768, #55789 ),
 ( #57396, #24549, #40164 ),
 ( #97866, #15890, #23485 ) ),
 .UNSPECIFIED., .F., .F., .F. ) 
 B_SPLINE_SURFACE_WITH_KNOTS ( ( 4, 2, 2, 2, 4 ),
 ( 3, 3 ),
 ( 9.107298248878237246E-18, 0.002138704226848488731, 0.004277408453696967920, 0.006416112680545447977, 0.008554816907393927167 ),
 ( 0.000000000000000000, 1.000000000000000000 ),
 .UNSPECIFIED. ) 
 GEOMETRIC_REPRESENTATION_ITEM ( )  RATIONAL_B_SPLINE_SURFACE ( (
 ( 1.000000000000000000, 0.7301269460247288290, 1.000000000000000000),
 ( 1.000000000000000000, 0.7403364392953195594, 1.000000000000000000),
 ( 1.000000000000000000, 0.7528282336556595400, 1.000000000000000000),
 ( 1.000000000000000000, 0.7798877127538836884, 1.000000000000000000),
 ( 1.000000000000000000, 0.7945789861789882558, 1.000000000000000000),
 ( 1.000000000000000000, 0.8227729472765989982, 1.000000000000000000),
 ( 1.000000000000000000, 0.8364472417785102643, 1.000000000000000000),
 ( 1.000000000000000000, 0.8612666947766824954, 1.000000000000000000),
 ( 1.000000000000000000, 0.8720837947351824937, 1.000000000000000000),
 ( 1.000000000000000000, 0.8806660624989743891, 1.000000000000000000) ) ) 
 REPRESENTATION_ITEM ( '' )  SURFACE ( )  );
#86459 = CARTESIAN_POINT ( 'NONE',  ( -82.69027687505180779, -37.83053627336025215, 3.614385560145078724 ) ) ;
#86460 = VECTOR ( 'NONE', #24386, 1000.000000000000227 ) ;
#86461 = CARTESIAN_POINT ( 'NONE',  ( 27.33349330513380337, 1.593028355512270567E-15, 0.000000000000000000 ) ) ;
#86462 = CARTESIAN_POINT ( 'NONE',  ( 30.00000000000000000, 0.000000000000000000, -13.00000000000000000 ) ) ;
#86463 = CONICAL_SURFACE ( 'NONE', #57166, 3.309500000000001663, 0.9599310885968770357 ) ;
#86464 = CARTESIAN_POINT ( 'NONE',  ( 3.021271035810708661, 104.3218411490978070, -5.000000000000000000 ) ) ;
#86465 = SURFACE_SIDE_STYLE ('',( #104194 ) ) ;
#86466 = CARTESIAN_POINT ( 'NONE',  ( -37.36680950590233863, 18.64316884713579725, 10.04205104295027517 ) ) ;
#86467 = CARTESIAN_POINT ( 'NONE',  ( 78.81966326594580607, -14.21045842199438347, 187.8133603351751333 ) ) ;
#86468 = CARTESIAN_POINT ( 'NONE',  ( -1.145927044342081333E-15, 61.34242035161803841, 9.357204421225127078 ) ) ;
#86469 = EDGE_CURVE ( 'NONE', #48371, #58381, #55948, .T. ) ;
#86470 = CARTESIAN_POINT ( 'NONE',  ( -81.17775171884230190, -14.21045842199422005, -20.84891578014651259 ) ) ;
#86471 = MECHANICAL_DESIGN_GEOMETRIC_PRESENTATION_REPRESENTATION (  '', ( #46858 ), #17551 ) ;
#86472 = CARTESIAN_POINT ( 'NONE',  ( -64.25667017276946069, -46.43867898611913603, 87.64705215544989869 ) ) ;
#86473 = ORIENTED_EDGE ( 'NONE', *, *, #87004, .T. ) ;
#86474 = CARTESIAN_POINT ( 'NONE',  ( 85.76531507393636389, -14.21045842199426801, 195.9085670305863118 ) ) ;
#86475 = CARTESIAN_POINT ( 'NONE',  ( -56.10217589899048107, 39.42619182724450866, -33.37224010391948781 ) ) ;
#86476 = CARTESIAN_POINT ( 'NONE',  ( 72.15333944293220725, -60.00000000002454215, 177.4635911251213827 ) ) ;
#86477 = VERTEX_POINT ( 'NONE', #88860 ) ;
#86478 = LINE ( 'NONE', #54577, #63149 ) ;
#86479 = CARTESIAN_POINT ( 'NONE',  ( 2.977408999572650927, -25.25000000204839168, -7.188101187500000933 ) ) ;
#86480 = ADVANCED_FACE ( 'NONE', ( #23080 ), #87096, .T. ) ;
#86481 = DIRECTION ( 'NONE',  ( -0.000000000000000000, 0.000000000000000000, -1.000000000000000000 ) ) ;
#86482 = VERTEX_POINT ( 'NONE', #71593 ) ;
#86483 = CARTESIAN_POINT ( 'NONE',  ( -11.36508313652864821, 45.70357710343880342, 13.50657646266319567 ) ) ;
#86484 = ORIENTED_EDGE ( 'NONE', *, *, #81486, .F. ) ;
#86485 = DIRECTION ( 'NONE',  ( -2.742080092235280244E-17, -0.000000000000000000, 1.000000000000000000 ) ) ;
#86486 = CARTESIAN_POINT ( 'NONE',  ( 1.405425597968214055E-06, -60.00000000000002132, -42.63907915653317815 ) ) ;
#86487 = CARTESIAN_POINT ( 'NONE',  ( 9.171168021175072127, -55.04774845291035490, 30.98659277684255997 ) ) ;
#86488 = CARTESIAN_POINT ( 'NONE',  ( 4.401442555609581635E-16, -34.15625000204838813, -7.188101187500000044 ) ) ;
#86489 = CARTESIAN_POINT ( 'NONE',  ( 32.13501140704661196, 486.0946583834067383, 5.282944113654357565 ) ) ;
#86490 = PRESENTATION_STYLE_ASSIGNMENT (( #69749 ) ) ;
#86491 = CARTESIAN_POINT ( 'NONE',  ( 21.08349330513380337, 1.593028355512270567E-15, 0.000000000000000000 ) ) ;
#86492 = CARTESIAN_POINT ( 'NONE',  ( 11.68767211932491712, 50.00000000000000000, -81.85902538600508649 ) ) ;
#86493 = CARTESIAN_POINT ( 'NONE',  ( 3.857142857142850545, -1.200583151104938517, 103.1763305333244318 ) ) ;
#86494 = CARTESIAN_POINT ( 'NONE',  ( 41.60090381918656277, 436.7951626062907735, 6.075960697884984718 ) ) ;
#86495 = DIRECTION ( 'NONE',  ( 0.000000000000000000, -1.000000000000000000, 0.000000000000000000 ) ) ;
#86496 = ORIENTED_EDGE ( 'NONE', *, *, #10979, .T. ) ;
#86497 = CARTESIAN_POINT ( 'NONE',  ( 0.000000000000000000, 0.000000000000000000, 0.000000000000000000 ) ) ;
#86498 = CARTESIAN_POINT ( 'NONE',  ( 4.586789253316277737, -2.224716758486257717, 102.5764008378948091 ) ) ;
#86500 = CARTESIAN_POINT ( 'NONE',  ( 37.87242778715787495, -56.81031238840315467, 40.67136584880061179 ) ) ;
#86499 = CARTESIAN_POINT ( 'NONE',  ( -3.534854068998068310, -48.92952247113088049, 104.4405781011824530 ) ) ;
#86501 = ORIENTED_EDGE ( 'NONE', *, *, #74585, .T. ) ;
#86502 = CARTESIAN_POINT ( 'NONE',  ( -7.996668423981797780, 47.99999999999999289, -78.85453280025085121 ) ) ;
#86503 = EDGE_CURVE ( 'NONE', #55309, #90133, #66892, .T. ) ;
#86504 = PRODUCT_RELATED_PRODUCT_CATEGORY ( 'part', '', ( #3601 ) ) ;
#86506 = CARTESIAN_POINT ( 'NONE',  ( -21.23684446602550935, 304.9566545053270943, -9.977713076987674512 ) ) ;
#86505 = DIRECTION ( 'NONE',  ( -1.000000000000000000, -0.000000000000000000, -0.000000000000000000 ) ) ;
#86507 = CARTESIAN_POINT ( 'NONE',  ( -3.400000000000000355, 4.163799117101001052E-16, -8.000000000000000000 ) ) ;
#86508 = CARTESIAN_POINT ( 'NONE',  ( 8.000000000000000000, -23.18750000409677270, 0.000000000000000000 ) ) ;
#86509 =( NAMED_UNIT ( * ) SI_UNIT ( $, .STERADIAN. ) SOLID_ANGLE_UNIT ( ) );
#86510 = CARTESIAN_POINT ( 'NONE',  ( -40.02090011478443898, 436.4865077410172489, 5.635628130756175302 ) ) ;
#86511 = CARTESIAN_POINT ( 'NONE',  ( -49.26518742571406761, 13.24133944401902419, -15.39083778843300720 ) ) ;
#86512 = CARTESIAN_POINT ( 'NONE',  ( -7.500000000000000000, -4.330127018922201643, -7.422398894150036064 ) ) ;
#86513 = ORIENTED_EDGE ( 'NONE', *, *, #92544, .F. ) ;
#86514 = CARTESIAN_POINT ( 'NONE',  ( 92.72621184031598318, -60.00000000000000000, -5.596747031044355225 ) ) ;
#86515 = CARTESIAN_POINT ( 'NONE',  ( 0.000000000000000000, 0.000000000000000000, -10.00000000000000000 ) ) ;
#86516 = STYLED_ITEM ( 'NONE', ( #97012 ), #51736 ) ;
#86517 = CARTESIAN_POINT ( 'NONE',  ( -6.190137073498123144, 41.32597146626896034, -70.92513718978732129 ) ) ;
#86518 = CYLINDRICAL_SURFACE ( 'NONE', #58133, 10.00000000000001954 ) ;
#86519 = ORIENTED_EDGE ( 'NONE', *, *, #30370, .T. ) ;
#86520 = CARTESIAN_POINT ( 'NONE',  ( -85.82535587192259641, -29.99999999998809130, 197.6421767587684997 ) ) ;
#86521 = VERTEX_POINT ( 'NONE', #6864 ) ;
#86522 = EDGE_CURVE ( 'NONE', #87130, #44939, #88780, .T. ) ;
#86523 =( LENGTH_UNIT ( ) NAMED_UNIT ( * ) SI_UNIT ( .MILLI., .METRE. ) );
#86524 = CARTESIAN_POINT ( 'NONE',  ( 6.644028492724102897, 7.802520252160764613, 9.720400798523309454E-13 ) ) ;
#86525 = CARTESIAN_POINT ( 'NONE',  ( 15.72426027928839076, 22.05433369634782181, -3.882282778234776188 ) ) ;
#86526 = CARTESIAN_POINT ( 'NONE',  ( 82.96525807848877321, -45.27743543914848345, -14.54737611346266846 ) ) ;
#86527 = TOROIDAL_SURFACE ( 'NONE', #39983, 5.999999999999996447, 4.000000000000000000 ) ;
#86528 = CARTESIAN_POINT ( 'NONE',  ( -7.188101187500001821, -32.37500000204838813, -2.977408999572651371 ) ) ;
#86529 = CARTESIAN_POINT ( 'NONE',  ( -17.53252671428359477, 45.00000000000000000, 63.43329252951189545 ) ) ;
#86530 = CARTESIAN_POINT ( 'NONE',  ( -11.51741314084194734, 304.6035749955722167, 8.884240740051277285 ) ) ;
#86531 = DIRECTION ( 'NONE',  ( 0.000000000000000000, 0.000000000000000000, 1.000000000000000000 ) ) ;
#86532 = ADVANCED_FACE ( 'NONE', ( #56469 ), #100618, .T. ) ;
#86533 = AXIS2_PLACEMENT_3D ( 'NONE', #88788, #90373, #40228 ) ;
#86534 = ORIENTED_EDGE ( 'NONE', *, *, #78693, .T. ) ;
#86536 = ORIENTED_EDGE ( 'NONE', *, *, #103541, .T. ) ;
#86535 = FILL_AREA_STYLE ('',( #61727 ) ) ;
#86537 = CARTESIAN_POINT ( 'NONE',  ( 77.12720002150464893, -46.43306016149463034, 136.1069725533496921 ) ) ;
#86538 = CARTESIAN_POINT ( 'NONE',  ( 14.38793715987709554, 1.958934843042821505, 4.277839136693246225 ) ) ;
#86539 = ORIENTED_EDGE ( 'NONE', *, *, #105938, .F. ) ;
#86540 = CARTESIAN_POINT ( 'NONE',  ( 3.355259093261282022, -49.33750271349889971, 40.75586556368205748 ) ) ;
#86541 = ADVANCED_FACE ( 'NONE', ( #62466 ), #21674, .T. ) ;
#86542 = CARTESIAN_POINT ( 'NONE',  ( -1.320432766682874540E-15, -21.03125000204838457, 7.188101187500000044 ) ) ;
#86543 = EDGE_CURVE ( 'NONE', #6978, #59047, #64673, .T. ) ;
#86544 = CARTESIAN_POINT ( 'NONE',  ( -100.1205506810183152, -57.62746089781320791, 203.8952656938035091 ) ) ;
#86545 = ORIENTED_EDGE ( 'NONE', *, *, #97090, .T. ) ;
#86546 = AXIS2_PLACEMENT_3D ( 'NONE', #91106, #17214, #74356 ) ;
#86547 = EDGE_CURVE ( 'NONE', #96778, #23775, #21433, .T. ) ;
#86548 = CARTESIAN_POINT ( 'NONE',  ( -5.477432325710317684, -13.16479535570474368, 2.459915882346688676 ) ) ;
#86549 = CARTESIAN_POINT ( 'NONE',  ( 7.010778207173779641, 41.61257717850156013, -59.09056268933341727 ) ) ;
#86550 = AXIS2_PLACEMENT_3D ( 'NONE', #86449, #21712, #85911 ) ;
#86551 = CARTESIAN_POINT ( 'NONE',  ( 24.83349330513380337, -7.703719777548943412E-31, 4.000000000000001776 ) ) ;
#86552 = CARTESIAN_POINT ( 'NONE',  ( 7.999999999999998224, -18.78125000409677625, 3.313708498984766493 ) ) ;
#86553 = CARTESIAN_POINT ( 'NONE',  ( -37.78143777952784887, -25.35208823665809774, 34.67056976772743582 ) ) ;
#86554 = CARTESIAN_POINT ( 'NONE',  ( 9.571198553003723575, 15.30040232763830943, 2.918503601030441708 ) ) ;
#86555 = CARTESIAN_POINT ( 'NONE',  ( -1.000000000000000000, -69.59657292933731298, 12.76848391598547394 ) ) ;
#86556 = CARTESIAN_POINT ( 'NONE',  ( 0.000000000000000000, 0.000000000000000000, 0.000000000000000000 ) ) ;
#86557 = CARTESIAN_POINT ( 'NONE',  ( 4.659745271205086858, 51.51257451253292885, 8.372825955202660708 ) ) ;
#86558 = DIRECTION ( 'NONE',  ( -0.7742246717937522060, -3.125999150826534011E-16, -0.6329108606951350247 ) ) ;
#86559 = CARTESIAN_POINT ( 'NONE',  ( 6.947681302647271906, -29.99999999999999645, -2.194325991354435068 ) ) ;
#86560 = EDGE_LOOP ( 'NONE', ( #13089, #93836, #96943, #100518, #27359, #105044, #78503, #39528, #45117, #24722 ) ) ;
#86561 =( NAMED_UNIT ( * ) SI_UNIT ( $, .STERADIAN. ) SOLID_ANGLE_UNIT ( ) );
#86562 = CARTESIAN_POINT ( 'NONE',  ( 3.006829104376306210E-15, 0.000000000000000000, -24.55262289886175964 ) ) ;
#86563 = CARTESIAN_POINT ( 'NONE',  ( -39.42238789698101442, 436.7568662985884771, 5.264481638451546708 ) ) ;
#86564 = CARTESIAN_POINT ( 'NONE',  ( 7.677589009493908101, -18.26067908012137053, -37.91149814823734943 ) ) ;
#86565 = CARTESIAN_POINT ( 'NONE',  ( -77.43986148285553384, -30.00000000000000000, 121.9463532134702461 ) ) ;
#86566 = DIRECTION ( 'NONE',  ( -1.000000000000000000, -0.000000000000000000, -0.000000000000000000 ) ) ;
#86567 = ORIENTED_EDGE ( 'NONE', *, *, #32967, .F. ) ;
#86568 = CARTESIAN_POINT ( 'NONE',  ( -6.876313068558442154, -4.333298119783861146, 16.54772121373820326 ) ) ;
#86569 = CARTESIAN_POINT ( 'NONE',  ( 83.25052031436327127, -57.53743629746287525, 201.3212271054727580 ) ) ;
#86570 = CARTESIAN_POINT ( 'NONE',  ( 62.09620979924952167, -34.58946247023943954, -24.66282284637085453 ) ) ;
#86571 = EDGE_CURVE ( 'NONE', #89868, #45240, #33272, .T. ) ;
#86572 = DIRECTION ( 'NONE',  ( 0.000000000000000000, 0.000000000000000000, 1.000000000000000000 ) ) ;
#86573 = CARTESIAN_POINT ( 'NONE',  ( 11.08349330513380160, -7.703719777548943412E-31, 4.000000000000001776 ) ) ;
#86574 = CARTESIAN_POINT ( 'NONE',  ( -69.32805405156442191, -60.00000000000000000, 137.7891073056175060 ) ) ;
#86575 = CYLINDRICAL_SURFACE ( 'NONE', #62427, 14.00000000000000178 ) ;
#86576 = DIRECTION ( 'NONE',  ( 0.000000000000000000, 0.000000000000000000, 1.000000000000000000 ) ) ;
#86577 = CARTESIAN_POINT ( 'NONE',  ( 11.54772599577024295, 50.00000000000000000, 62.20121126512098186 ) ) ;
#86578 = CARTESIAN_POINT ( 'NONE',  ( -86.25609154892794095, -24.66340834717759023, 181.7636524898530865 ) ) ;
#86579 = AXIS2_PLACEMENT_3D ( 'NONE', #54928, #87853, #81321 ) ;
#86580 = VERTEX_POINT ( 'NONE', #330 ) ;
#86581 = CARTESIAN_POINT ( 'NONE',  ( 35.54351702707027272, 361.7442709301026298, 2.606710528293841644 ) ) ;
#86582 = CARTESIAN_POINT ( 'NONE',  ( 43.68078092307730032, 484.4268836469389612, 2.016138049968958512 ) ) ;
#86583 = CARTESIAN_POINT ( 'NONE',  ( -6.771436230215871710, 41.75941352900127157, -59.18670869008018087 ) ) ;
#86584 = VECTOR ( 'NONE', #106149, 1000.000000000000000 ) ;
#86585 = CARTESIAN_POINT ( 'NONE',  ( 6.162888688655344005, 3.752776749732565253, 6.499999999999997335 ) ) ;
#86587 = EDGE_CURVE ( 'NONE', #54991, #94321, #13940, .T. ) ;
#86586 = DIRECTION ( 'NONE',  ( 1.000000000000000000, 0.000000000000000000, -0.000000000000000000 ) ) ;
#86588 = PLANE ( 'NONE',  #794 ) ;
#86589 = DIRECTION ( 'NONE',  ( 0.000000000000000000, -1.000000000000000000, 0.000000000000000000 ) ) ;
#86590 = CARTESIAN_POINT ( 'NONE',  ( 0.000000000000000000, 0.000000000000000000, 0.000000000000000000 ) ) ;
#86591 = CARTESIAN_POINT ( 'NONE',  ( 105.5720000000000312, 6.123233995736768255E-16, -5.000000000000000888 ) ) ;
#86592 = ORIENTED_EDGE ( 'NONE', *, *, #65113, .F. ) ;
#86593 = AXIS2_PLACEMENT_3D ( 'NONE', #65917, #83682, #98796 ) ;
#86594 = CARTESIAN_POINT ( 'NONE',  ( 18.07381427182019706, 50.00000000000000000, 61.79284943879029157 ) ) ;
#86595 = DIRECTION ( 'NONE',  ( 0.000000000000000000, 0.000000000000000000, -1.000000000000000000 ) ) ;
#86596 = CARTESIAN_POINT ( 'NONE',  ( -17.78317311658302202, -3.469446951953614189E-15, -13.66642973270732142 ) ) ;
#86597 = CARTESIAN_POINT ( 'NONE',  ( 9.768254851146028983, 53.46555892738330584, -2.423069053207274504 ) ) ;
#86598 = CARTESIAN_POINT ( 'NONE',  ( 97.37780541404315215, -14.21045842199443143, 96.97658560636448044 ) ) ;
#86599 = CARTESIAN_POINT ( 'NONE',  ( -81.09943103650151386, -25.62393341775641531, 137.9297325403806553 ) ) ;
#86600 = ORIENTED_EDGE ( 'NONE', *, *, #92248, .T. ) ;
#86601 = SURFACE_SIDE_STYLE ('',( #102758 ) ) ;
#86602 = FILL_AREA_STYLE ('',( #88695 ) ) ;
#86603 = CARTESIAN_POINT ( 'NONE',  ( 2.851084197991860414, -57.67120200768756888, 41.61186728490002906 ) ) ;
#86604 = DIRECTION ( 'NONE',  ( -1.000000000000000000, -0.000000000000000000, -0.000000000000000000 ) ) ;
#86605 = CARTESIAN_POINT ( 'NONE',  ( 42.94916902413876159, 342.9903042650141742, 9.416962103331693257 ) ) ;
#86606 = EDGE_CURVE ( 'NONE', #9728, #14501, #45741, .T. ) ;
#86607 = CARTESIAN_POINT ( 'NONE',  ( 84.73333333333332007, 1.023464760207051730E-14, 0.000000000000000000 ) ) ;
#86608 = VERTEX_POINT ( 'NONE', #35438 ) ;
#86609 = DIRECTION ( 'NONE',  ( 0.000000000000000000, 0.000000000000000000, 1.000000000000000000 ) ) ;
#86610 = DIRECTION ( 'NONE',  ( -1.000000000000000000, -0.000000000000000000, -0.000000000000000000 ) ) ;
#86611 = CARTESIAN_POINT ( 'NONE',  ( -5.082755093536325042, -26.09375000204838813, -5.082755093536325930 ) ) ;
#86612 = ORIENTED_EDGE ( 'NONE', *, *, #105991, .T. ) ;
#86613 = CARTESIAN_POINT ( 'NONE',  ( 43.68566140667488895, 485.0560336449399870, 1.938913452013092842 ) ) ;
#86614 = AXIS2_PLACEMENT_3D ( 'NONE', #28575, #2658, #61462 ) ;
#86616 = EDGE_CURVE ( 'NONE', #84900, #1105, #59536, .T. ) ;
#86615 = CARTESIAN_POINT ( 'NONE',  ( 15.11650669486618881, 4.898587196589411843E-16, -4.000000000000000888 ) ) ;
#86617 = CARTESIAN_POINT ( 'NONE',  ( 5.504993149140188002, 41.95607710206238039, -69.87068889203474953 ) ) ;
#86618 = CARTESIAN_POINT ( 'NONE',  ( 0.7145311798163271888, -9.237604307034018802, 8.246630900752838649E-17 ) ) ;
#86619 = CARTESIAN_POINT ( 'NONE',  ( 19.34999999999999787, 1.533819458162526451E-15, 0.000000000000000000 ) ) ;
#86620 = DIRECTION ( 'NONE',  ( -0.000000000000000000, -0.000000000000000000, -1.000000000000000000 ) ) ;
#86621 = ORIENTED_EDGE ( 'NONE', *, *, #92736, .F. ) ;
#86622 = CARTESIAN_POINT ( 'NONE',  ( 90.46769687319441289, -60.00000000000001421, -18.02911679486343743 ) ) ;
#86623 = VECTOR ( 'NONE', #482, 1000.000000000000000 ) ;
#86625 = CARTESIAN_POINT ( 'NONE',  ( 25.70524614496113358, -29.04465569019870586, 30.12072865786996090 ) ) ;
#86624 = CARTESIAN_POINT ( 'NONE',  ( -55.31183857750818333, -60.00000000000000000, 93.46795725556545165 ) ) ;
#86626 = CARTESIAN_POINT ( 'NONE',  ( 23.61990465140407736, 60.76237703744687479, -11.80995232570203690 ) ) ;
#86628 = ORIENTED_EDGE ( 'NONE', *, *, #58254, .T. ) ;
#86627 =( BOUNDED_SURFACE ( )  B_SPLINE_SURFACE ( 3, 2, ( 
 ( #41406, #89962, #81318 ),
 ( #106124, #57570, #23662 ),
 ( #57044, #48949, #7966 ),
 ( #90494, #16603, #49494 ),
 ( #8503, #12222, #102306 ),
 ( #76963, #11685, #44078 ),
 ( #84540, #52681, #68357 ),
 ( #10625, #3079, #75901 ),
 ( #36025, #10103, #101255 ),
 ( #53233, #27409, #68899 ),
 ( #85067, #83997, #1999 ),
 ( #85611, #51621, #101773 ),
 ( #44620, #76424, #69424 ),
 ( #34947, #100174, #27939 ),
 ( #11149, #77509, #67818 ),
 ( #26343, #60802, #94225 ),
 ( #52152, #43014, #93694 ),
 ( #93157, #43544, #60286 ),
 ( #100700, #61335, #19324 ),
 ( #26867, #19846, #3622 ),
 ( #35482, #36555, #18773 ),
 ( #28456, #20390, #86153 ),
 ( #18222, #45152, #1462 ),
 ( #59737, #34424, #2539 ),
 ( #92614, #67296, #59204 ),
 ( #92081, #51076, #38143 ),
 ( #13276, #37081, #96356 ),
 ( #54797, #30565, #87200 ),
 ( #104418, #103888, #30034 ),
 ( #63994, #63463, #104967 ),
 ( #86681, #22486, #55327 ),
 ( #4152, #45675, #69946 ),
 ( #87730, #13809, #88254 ),
 ( #96870, #102844, #46721 ),
 ( #29011, #21947, #12752 ),
 ( #79612, #62924, #46204 ),
 ( #23004, #78555, #31108 ),
 ( #61877, #4685, #95818 ),
 ( #21417, #5213, #14333 ),
 ( #47240, #79090, #72059 ),
 ( #62394, #5727, #6242 ),
 ( #80141, #38651, #37618 ),
 ( #70481, #39179, #71517 ),
 ( #54257, #103376, #94771 ),
 ( #55840, #88779, #14869 ),
 ( #78033, #20919, #53753 ),
 ( #95288, #29523, #70997 ),
 ( #25125, #33747, #74168 ),
 ( #81713, #56378, #248 ),
 ( #89839, #33212, #82263 ),
 ( #105998, #105484, #40744 ),
 ( #58541, #65023, #90906 ),
 ( #106535, #31622, #73632 ),
 ( #8375, #23537, #32691 ),
 ( #41805, #6787, #16476 ),
 ( #90362, #17020, #24070 ),
 ( #7836, #24595, #56914 ),
 ( #15407, #65558, #49356 ),
 ( #98447, #15942, #99503 ),
 ( #41277, #48818, #57442 ) ),
 .UNSPECIFIED., .F., .F., .F. ) 
 B_SPLINE_SURFACE_WITH_KNOTS ( ( 4, 2, 2, 2, 2, 2, 2, 2, 2, 2, 2, 2, 2, 2, 2, 2, 2, 2, 2, 2, 2, 2, 2, 2, 2, 2, 2, 2, 2, 4 ),
 ( 3, 3 ),
 ( 0.06375477930561219975, 0.06599154682095068059, 0.06822831433628917530, 0.07270184936696613698, 0.07717538439764309866, 0.08164891942832006033, 0.09059598948967399756, 0.09954305955102793479, 0.1174371996737358093, 0.1353313397964436837, 0.1532254799191515582, 0.1711196200418594326, 0.1800666901032133560, 0.1890137601645672794, 0.1934872951952442410, 0.1979608302259212027, 0.2001975977412596974, 0.2013159814989289309, 0.2024343652565981921, 0.2035527490142674256, 0.2046711327719366591, 0.2057895165296059203, 0.2059293144993145641, 0.2059467892455281446, 0.2059555266186349209, 0.2059642639917417251, 0.2059992134841688860, 0.2060691124690232356, 0.2063487084084405510, 0.2069079002872751538 ),
 ( 0.000000000000000000, 1.000000000000000000 ),
 .UNSPECIFIED. ) 
 GEOMETRIC_REPRESENTATION_ITEM ( )  RATIONAL_B_SPLINE_SURFACE ( (
 ( 1.000000000000000000, 0.7071067811865474617, 1.000000000000000000),
 ( 1.000000000000000000, 0.7071067811865474617, 1.000000000000000000),
 ( 1.000000000000000000, 0.7071067811865474617, 1.000000000000000000),
 ( 1.000000000000000000, 0.7071067811865474617, 1.000000000000000000),
 ( 1.000000000000000000, 0.7071067811865476838, 1.000000000000000000),
 ( 1.000000000000000000, 0.7071067811865476838, 1.000000000000000000),
 ( 1.000000000000000000, 0.7071067811865476838, 1.000000000000000000),
 ( 1.000000000000000000, 0.7071067811865476838, 1.000000000000000000),
 ( 1.000000000000000000, 0.7071067811865474617, 1.000000000000000000),
 ( 1.000000000000000000, 0.7071067811865474617, 1.000000000000000000),
 ( 1.000000000000000000, 0.7071067811865475727, 1.000000000000000000),
 ( 1.000000000000000000, 0.7071067811865475727, 1.000000000000000000),
 ( 1.000000000000000000, 0.7071067811865474617, 1.000000000000000000),
 ( 1.000000000000000000, 0.7071067811865474617, 1.000000000000000000),
 ( 1.000000000000000000, 0.7071067811865475727, 1.000000000000000000),
 ( 1.000000000000000000, 0.7071067811865475727, 1.000000000000000000),
 ( 1.000000000000000000, 0.7071067811865475727, 1.000000000000000000),
 ( 1.000000000000000000, 0.7071067811865475727, 1.000000000000000000),
 ( 1.000000000000000000, 0.7071067811865474617, 1.000000000000000000),
 ( 1.000000000000000000, 0.7071067811865474617, 1.000000000000000000),
 ( 1.000000000000000000, 0.7071067811865475727, 1.000000000000000000),
 ( 1.000000000000000000, 0.7071067811865475727, 1.000000000000000000),
 ( 1.000000000000000000, 0.7071067811865475727, 1.000000000000000000),
 ( 1.000000000000000000, 0.7071067811865475727, 1.000000000000000000),
 ( 1.000000000000000000, 0.7071067811865475727, 1.000000000000000000),
 ( 1.000000000000000000, 0.7071067811865475727, 1.000000000000000000),
 ( 1.000000000000000000, 0.7071067811865475727, 1.000000000000000000),
 ( 1.000000000000000000, 0.7071067811865475727, 1.000000000000000000),
 ( 1.000000000000000000, 0.7071067811865475727, 1.000000000000000000),
 ( 1.000000000000000000, 0.7071067811865475727, 1.000000000000000000),
 ( 1.000000000000000000, 0.7071067811865475727, 1.000000000000000000),
 ( 1.000000000000000000, 0.7071067811865475727, 1.000000000000000000),
 ( 1.000000000000000000, 0.7071067811865475727, 1.000000000000000000),
 ( 1.000000000000000000, 0.7071067811865475727, 1.000000000000000000),
 ( 1.000000000000000000, 0.7071067811865475727, 1.000000000000000000),
 ( 1.000000000000000000, 0.7071067811865475727, 1.000000000000000000),
 ( 1.000000000000000000, 0.7071067811865475727, 1.000000000000000000),
 ( 1.000000000000000000, 0.7071067811865475727, 1.000000000000000000),
 ( 1.000000000000000000, 0.7071067811865475727, 1.000000000000000000),
 ( 1.000000000000000000, 0.7071067811865475727, 1.000000000000000000),
 ( 1.000000000000000000, 0.7071067811865475727, 1.000000000000000000),
 ( 1.000000000000000000, 0.7071067811865475727, 1.000000000000000000),
 ( 1.000000000000000000, 0.7071067811865475727, 1.000000000000000000),
 ( 1.000000000000000000, 0.7071067811865475727, 1.000000000000000000),
 ( 1.000000000000000000, 0.7071067811865475727, 1.000000000000000000),
 ( 1.000000000000000000, 0.7071067811865475727, 1.000000000000000000),
 ( 1.000000000000000000, 0.7071067811865475727, 1.000000000000000000),
 ( 1.000000000000000000, 0.7071067811865475727, 1.000000000000000000),
 ( 1.000000000000000000, 0.7071067811865475727, 1.000000000000000000),
 ( 1.000000000000000000, 0.7071067811865475727, 1.000000000000000000),
 ( 1.000000000000000000, 0.7071067811865475727, 1.000000000000000000),
 ( 1.000000000000000000, 0.7071067811865475727, 1.000000000000000000),
 ( 1.000000000000000000, 0.7071067811865475727, 1.000000000000000000),
 ( 1.000000000000000000, 0.7071067811865475727, 1.000000000000000000),
 ( 1.000000000000000000, 0.7071067811865475727, 1.000000000000000000),
 ( 1.000000000000000000, 0.7071067811865475727, 1.000000000000000000),
 ( 1.000000000000000000, 0.7071067811865475727, 1.000000000000000000),
 ( 1.000000000000000000, 0.7071067811865475727, 1.000000000000000000),
 ( 1.000000000000000000, 0.7071067811865475727, 1.000000000000000000),
 ( 1.000000000000000000, 0.7071067811865475727, 1.000000000000000000) ) ) 
 REPRESENTATION_ITEM ( '' )  SURFACE ( )  );
#86629 = VERTEX_POINT ( 'NONE', #11102 ) ;
#86630 = CARTESIAN_POINT ( 'NONE',  ( -25.22241582816893057, -4.285714285714296246, -1.650803255657555146 ) ) ;
#86631 = CARTESIAN_POINT ( 'NONE',  ( 1.370335905996620722E-14, 22.97884757028485225, -55.94820918777160301 ) ) ;
#86632 = CARTESIAN_POINT ( 'NONE',  ( -13.95408269174820148, -57.87006985093267986, 28.16184020435892421 ) ) ;
#86633 = VECTOR ( 'NONE', #6092, 1000.000000000000000 ) ;
#86634 = DIRECTION ( 'NONE',  ( -0.000000000000000000, 1.000000000000000000, -0.000000000000000000 ) ) ;
#86635 = CARTESIAN_POINT ( 'NONE',  ( 7.046289519167721060, -63.69408180055623347, -3.789821819998816288 ) ) ;
#86636 = EDGE_LOOP ( 'NONE', ( #59991, #24648, #105154, #42324 ) ) ;
#86637 = CARTESIAN_POINT ( 'NONE',  ( 17.50000000000002487, 44.85000000000000853, 62.61746187599675295 ) ) ;
#86638 = CARTESIAN_POINT ( 'NONE',  ( 85.39867414124013578, -29.99999999999999289, 60.46109300951300725 ) ) ;
#86639 = CARTESIAN_POINT ( 'NONE',  ( 33.09872316835808448, 40.69672373397799703, -62.13666886876760032 ) ) ;
#86640 = EDGE_CURVE ( 'NONE', #16503, #52389, #68140, .T. ) ;
#86641 = DIRECTION ( 'NONE',  ( -1.000000000000000000, -1.224606353822377258E-16, -0.000000000000000000 ) ) ;
#86642 = CARTESIAN_POINT ( 'NONE',  ( 80.95908799317884075, -30.00000000000000711, 4.750023924636396444 ) ) ;
#86643 = CARTESIAN_POINT ( 'NONE',  ( 43.58349330513380693, 1.593028355512270567E-15, 0.000000000000000000 ) ) ;
#86644 = ORIENTED_EDGE ( 'NONE', *, *, #93701, .T. ) ;
#86645 = EDGE_LOOP ( 'NONE', ( #29203, #94335, #95438, #103770 ) ) ;
#86646 = EDGE_LOOP ( 'NONE', ( #75472, #11453, #31831, #12126, #17529 ) ) ;
#86647 = CARTESIAN_POINT ( 'NONE',  ( -4.000000000000000000, 17.85270131633358304, -10.00000000000000178 ) ) ;
#86648 = CARTESIAN_POINT ( 'NONE',  ( 4.142849616820252293E-15, 27.68727484027578356, -33.82893434829263413 ) ) ;
#86649 = DIRECTION ( 'NONE',  ( 0.000000000000000000, 0.000000000000000000, -1.000000000000000000 ) ) ;
#86650 = CARTESIAN_POINT ( 'NONE',  ( 33.32951764101204617, 490.0033476588131975, 11.19754049617962721 ) ) ;
#86651 = CARTESIAN_POINT ( 'NONE',  ( -1.759014387761618226, -70.05783877895481737, 13.10925274558140252 ) ) ;
#86652 = DIRECTION ( 'NONE',  ( 0.000000000000000000, 0.000000000000000000, 1.000000000000000000 ) ) ;
#86653 = DIRECTION ( 'NONE',  ( -1.000000000000000000, -1.224606353822377258E-16, -0.000000000000000000 ) ) ;
#86654 = EDGE_LOOP ( 'NONE', ( #88066, #50204, #70112, #71675 ) ) ;
#86655 = CARTESIAN_POINT ( 'NONE',  ( 9.739726766104286781, 48.00000000000000000, -82.38252115500969808 ) ) ;
#86656 = ORIENTED_EDGE ( 'NONE', *, *, #65703, .T. ) ;
#86657 = CARTESIAN_POINT ( 'NONE',  ( -5.191472769733072035, -62.35908423281053103, -3.014900733016762313 ) ) ;
#86658 = CARTESIAN_POINT ( 'NONE',  ( 60.37928884598232315, -38.34250802169606942, 97.60144182010409963 ) ) ;
#86659 = CARTESIAN_POINT ( 'NONE',  ( 31.03678703375144821, 438.6650838204807314, 21.86890379897223013 ) ) ;
#86660 = CARTESIAN_POINT ( 'NONE',  ( 28.21269487252221708, 296.8969659935266918, 2.382781577419921248 ) ) ;
#86661 = TOROIDAL_SURFACE ( 'NONE', #46959, 14.78272384904389192, 0.5000000000000000000 ) ;
#86662 = CARTESIAN_POINT ( 'NONE',  ( 36.08349330513379982, 4.000000000000003553, 0.000000000000000000 ) ) ;
#86663 = CARTESIAN_POINT ( 'NONE',  ( 63.48522851496006325, -53.38631336116730353, 88.97494422768454569 ) ) ;
#86664 = VERTEX_POINT ( 'NONE', #61283 ) ;
#86665 = DIRECTION ( 'NONE',  ( 0.000000000000000000, 0.000000000000000000, 1.000000000000000000 ) ) ;
#86666 = EDGE_CURVE ( 'NONE', #71001, #75752, #74510, .T. ) ;
#86667 = CARTESIAN_POINT ( 'NONE',  ( -61.85959367383505736, -37.56337504497723501, -33.69606644638567161 ) ) ;
#86668 = CARTESIAN_POINT ( 'NONE',  ( -6.241401647512419437, 10.55153228299010593, -3.173604836376809679 ) ) ;
#86669 = EDGE_CURVE ( 'NONE', #22777, #70585, #53942, .T. ) ;
#86670 = CARTESIAN_POINT ( 'NONE',  ( -9.306844948305085907, 51.55227296925463776, 1.766188453538026559 ) ) ;
#86671 = ORIENTED_EDGE ( 'NONE', *, *, #72608, .T. ) ;
#86672 = CARTESIAN_POINT ( 'NONE',  ( -4.175533140205453186, -1.555218955346044929, 102.9090322054120747 ) ) ;
#86673 = CARTESIAN_POINT ( 'NONE',  ( 43.02661387979757279, 465.7449615347597955, 11.43319743843537850 ) ) ;
#86674 = CONICAL_SURFACE ( 'NONE', #45305, 3.400000000000000355, 0.9599310885968748153 ) ;
#86675 = EDGE_CURVE ( 'NONE', #55271, #19214, #66439, .T. ) ;
#86676 = DIRECTION ( 'NONE',  ( 1.000000000000000000, 0.000000000000000000, 0.000000000000000000 ) ) ;
#86677 = CARTESIAN_POINT ( 'NONE',  ( 3.313708498984762052, -33.40625000409677625, -8.000000000000000000 ) ) ;
#86678 = CARTESIAN_POINT ( 'NONE',  ( 74.07777777777778283, 3.309500000000014541, 4.052968581778174646E-16 ) ) ;
#86679 = CARTESIAN_POINT ( 'NONE',  ( 86.31913262548056309, -39.17055256143338937, 187.7253881214433875 ) ) ;
#86680 = DIRECTION ( 'NONE',  ( -1.000000000000000000, 0.000000000000000000, 0.000000000000000000 ) ) ;
#86681 = CARTESIAN_POINT ( 'NONE',  ( -9.079631412587994888, 13.97901777659653000, 0.000000000000000000 ) ) ;
#86682 = CARTESIAN_POINT ( 'NONE',  ( 8.000086790516057533, -5.999826418939942840, 0.2639471549312809584 ) ) ;
#86683 = DIRECTION ( 'NONE',  ( -1.000000000000000000, -1.224606353822377258E-16, -0.000000000000000000 ) ) ;
#86684 = SURFACE_SIDE_STYLE ('',( #53757 ) ) ;
#86685 = CARTESIAN_POINT ( 'NONE',  ( 5.000000000000000000, -13.90268927582264347, 9.980021952846888311 ) ) ;
#86686 = CONICAL_SURFACE ( 'NONE', #95292, 8.000000000000000000, 0.9599310885968911355 ) ;
#86687 = CARTESIAN_POINT ( 'NONE',  ( -97.63324830393105458, -30.00000000000000000, 134.9666292763866977 ) ) ;
#86688 = PRESENTATION_LAYER_ASSIGNMENT (  '', '', ( #66021 ) ) ;
#86689 = B_SPLINE_CURVE_WITH_KNOTS ( 'NONE', 3,
 ( #7917, #59150, #74771, #849, #41354, #33288, #40820, #16018, #9503, #91518 ),
 .UNSPECIFIED., .F., .F.,
 ( 4, 2, 2, 2, 4 ),
 ( 0.000000000000000000, 0.001993803085173303895, 0.003987606170346607790, 0.005981409255519911684, 0.007975212340693215579 ),
 .UNSPECIFIED. ) ;
#86690 = AXIS2_PLACEMENT_3D ( 'NONE', #104529, #70587, #23115 ) ;
#86691 = CARTESIAN_POINT ( 'NONE',  ( 19.24463328355616909, -57.67182880030375003, 42.11738475777909230 ) ) ;
#86693 = CARTESIAN_POINT ( 'NONE',  ( 7.093721425956736049, 304.7303285792975771, 9.911179277710184365 ) ) ;
#86692 = CARTESIAN_POINT ( 'NONE',  ( 9.954115923268258115, 44.05789748778097703, 12.94115310699293531 ) ) ;
#86694 = EDGE_CURVE ( 'NONE', #32439, #71545, #47377, .T. ) ;
#86695 = DIRECTION ( 'NONE',  ( -0.8660254037844381525, 0.5000000000000007772, 0.000000000000000000 ) ) ;
#86696 = CARTESIAN_POINT ( 'NONE',  ( -18.83251367839346457, 50.00000000000000000, 60.81264960944136533 ) ) ;
#86697 = FACE_OUTER_BOUND ( 'NONE', #73763, .T. ) ;
#86698 = B_SPLINE_CURVE_WITH_KNOTS ( 'NONE', 3,
 ( #2542, #26869, #59739, #92616, #104419, #39180, #23005, #88781, #30035, #96357 ),
 .UNSPECIFIED., .F., .F.,
 ( 4, 2, 2, 2, 4 ),
 ( 0.000000000000000000, 0.001989602278884367460, 0.003979204557768734919, 0.005968806836653102812, 0.007958409115537469838 ),
 .UNSPECIFIED. ) ;
#86699 = CARTESIAN_POINT ( 'NONE',  ( 11.73848531063677569, -16.54446083686769242, -34.66488886015380189 ) ) ;
#86700 = ADVANCED_FACE ( 'NONE', ( #93913 ), #12677, .F. ) ;
#86701 = DIRECTION ( 'NONE',  ( -1.000000000000000000, -1.224606353822377258E-16, -0.000000000000000000 ) ) ;
#86702 = ORIENTED_EDGE ( 'NONE', *, *, #26509, .T. ) ;
#86703 = CARTESIAN_POINT ( 'NONE',  ( 40.15309039158240267, 485.1828724906196157, -4.320808352507255812 ) ) ;
#86704 = FACE_OUTER_BOUND ( 'NONE', #14324, .T. ) ;
#86705 = CARTESIAN_POINT ( 'NONE',  ( -20.24774297161117431, -42.95817207100498081, 31.59261033110390926 ) ) ;
#86708 = ADVANCED_FACE ( 'NONE', ( #54894 ), #4394, .T. ) ;
#86707 = FACE_OUTER_BOUND ( 'NONE', #17345, .T. ) ;
#86706 = CARTESIAN_POINT ( 'NONE',  ( -86.12427509053026142, -60.00000000000003553, 8.940647230371650878 ) ) ;
#86709 = VERTEX_POINT ( 'NONE', #23632 ) ;
#86710 =( LENGTH_UNIT ( ) NAMED_UNIT ( * ) SI_UNIT ( .MILLI., .METRE. ) );
#86711 = ORIENTED_EDGE ( 'NONE', *, *, #40482, .F. ) ;
#86712 = CARTESIAN_POINT ( 'NONE',  ( 42.87890743752956979, 485.5827513099150110, 6.686224016671874715 ) ) ;
#86713 = DIRECTION ( 'NONE',  ( -1.000000000000000000, -0.000000000000000000, -0.000000000000000000 ) ) ;
#86714 = DIRECTION ( 'NONE',  ( -1.000000000000000000, -0.000000000000000000, -0.000000000000000000 ) ) ;
#86715 = ORIENTED_EDGE ( 'NONE', *, *, #14040, .F. ) ;
#86716 = FILL_AREA_STYLE ('',( #12264 ) ) ;
#86717 = CARTESIAN_POINT ( 'NONE',  ( 100.7952419678079821, -37.84774286652142905, 188.8884646472686200 ) ) ;
#86718 = AXIS2_PLACEMENT_3D ( 'NONE', #82876, #8973, #92558 ) ;
#86720 = DIRECTION ( 'NONE',  ( 0.5735764363510490460, 0.8191520442889896891, 0.000000000000000000 ) ) ;
#86719 = CARTESIAN_POINT ( 'NONE',  ( -13.50000000000000000, 7.794228634059933825, -1.205771365940051520 ) ) ;
#86721 = EDGE_LOOP ( 'NONE', ( #76020, #105514, #74796, #87733, #106455 ) ) ;
#86722 = ORIENTED_EDGE ( 'NONE', *, *, #66599, .T. ) ;
#86723 = CIRCLE ( 'NONE', #19616, 15.00000000000001243 ) ;
#86724 = ORIENTED_EDGE ( 'NONE', *, *, #53947, .T. ) ;
#86725 = CARTESIAN_POINT ( 'NONE',  ( 26.26255647543327143, 307.7041406114180973, 10.82825725285463925 ) ) ;
#86726 = ADVANCED_FACE ( 'NONE', ( #55938 ), #63556, .T. ) ;
#86727 = FACE_OUTER_BOUND ( 'NONE', #95764, .T. ) ;
#86728 = FACE_OUTER_BOUND ( 'NONE', #15480, .T. ) ;
#86729 = ORIENTED_EDGE ( 'NONE', *, *, #60456, .F. ) ;
#86730 = LINE ( 'NONE', #12804, #87612 ) ;
#86731 = CARTESIAN_POINT ( 'NONE',  ( -5.956988534971662475, 4.556784786910193397, -5.000000000000000000 ) ) ;
#86732 = CARTESIAN_POINT ( 'NONE',  ( -85.18694157166503089, -59.99999999999020162, -27.35932843724341978 ) ) ;
#86733 = CARTESIAN_POINT ( 'NONE',  ( 6.683837171061802529, 3.955946848495958346, -6.851900933636989599 ) ) ;
#86734 = CARTESIAN_POINT ( 'NONE',  ( 35.33767613680186059, -60.00000000000000000, 46.68008179612595399 ) ) ;
#86735 = CARTESIAN_POINT ( 'NONE',  ( 15.35331269684644617, -5.000000000000000000, -5.840831470021132787 ) ) ;
#86736 = CARTESIAN_POINT ( 'NONE',  ( -6.526057575926256682, 41.69808020043258523, -58.86835240465277508 ) ) ;
#86737 = AXIS2_PLACEMENT_3D ( 'NONE', #73201, #23635, #88882 ) ;
#86739 = CARTESIAN_POINT ( 'NONE',  ( 13.52092337146004475, -42.95373788567773943, 31.13298423633953504 ) ) ;
#86738 = CARTESIAN_POINT ( 'NONE',  ( -98.75680450758818552, -14.21045842199431064, 105.0421542466116023 ) ) ;
#86740 = EDGE_CURVE ( 'NONE', #23780, #45532, #105768, .T. ) ;
#86741 = CARTESIAN_POINT ( 'NONE',  ( -8.400598463031300867, 51.89207564805971629, 1.531152949374564365 ) ) ;
#86742 = CARTESIAN_POINT ( 'NONE',  ( -47.71978414336781782, -36.06698018952960183, 46.18487447919529387 ) ) ;
#86743 = ADVANCED_FACE ( 'NONE', ( #31206 ), #64090, .T. ) ;
#86744 = DIRECTION ( 'NONE',  ( 1.000000000000000000, 0.000000000000000000, 0.000000000000000000 ) ) ;
#86745 = ORIENTED_EDGE ( 'NONE', *, *, #24505, .T. ) ;
#86746 = EDGE_CURVE ( 'NONE', #68169, #69676, #350, .T. ) ;
#86747 = CARTESIAN_POINT ( 'NONE',  ( 36.19807994336332513, 437.5493722796938982, 4.275365344036610615 ) ) ;
#86748 = FACE_OUTER_BOUND ( 'NONE', #49169, .T. ) ;
#86749 = CARTESIAN_POINT ( 'NONE',  ( 6.585531397294614564, 4.023063057964794353, 6.499999999999997335 ) ) ;
#86750 = ORIENTED_EDGE ( 'NONE', *, *, #42092, .F. ) ;
#86751 = CARTESIAN_POINT ( 'NONE',  ( -12.30664161282574831, -4.730394409147478996, 20.32424246445631510 ) ) ;
#86752 = EDGE_LOOP ( 'NONE', ( #73515, #89276 ) ) ;
#86753 = CARTESIAN_POINT ( 'NONE',  ( 47.64963052949291011, -38.32453750017476324, 63.16317949360573891 ) ) ;
#86754 = CARTESIAN_POINT ( 'NONE',  ( 4.003587701500182838, -48.94962346669694142, 104.5574048719321780 ) ) ;
#86756 = ADVANCED_FACE ( 'NONE', ( #41913 ), #45768, .F. ) ;
#86755 = VECTOR ( 'NONE', #99630, 1000.000000000000000 ) ;
#86757 = CARTESIAN_POINT ( 'NONE',  ( 6.780292695530274472, 41.80198870715022252, -59.33023448964987523 ) ) ;
#86758 = CARTESIAN_POINT ( 'NONE',  ( -59.23741894013591036, 42.00000000000000711, -7.754160006507100356 ) ) ;
#86759 = CARTESIAN_POINT ( 'NONE',  ( 100.4511241798009564, -30.00000000000000000, 183.1650932517458159 ) ) ;
#86760 =( BOUNDED_CURVE ( )  B_SPLINE_CURVE ( 2, ( #78192, #79251, #38808, #22105, #54960, #96514, #22647, #55482, #70103 ),
 .UNSPECIFIED., .F., .F. ) 
 B_SPLINE_CURVE_WITH_KNOTS ( ( 3, 2, 2, 2, 3 ),
 ( 0.2205882352941176683, 0.2279411764705882582, 0.2352941176470588758, 0.2426470588235294656, 0.2500000000000000555 ),
 .UNSPECIFIED. ) 
 CURVE ( )  GEOMETRIC_REPRESENTATION_ITEM ( )  RATIONAL_B_SPLINE_CURVE ( ( 0.9999999999999996669, 0.9238795325112870716, 1.000000000000000000, 0.9238795325112867385, 1.000000000000000000, 0.9238795325112867385, 1.000000000000000000, 0.9238795325112861834, 1.000000000000000666 ) ) 
 REPRESENTATION_ITEM ( '' )  );
#86761 = AXIS2_PLACEMENT_3D ( 'NONE', #12061, #20216, #29357 ) ;
#86762 = LINE ( 'NONE', #21500, #89704 ) ;
#86763 = ORIENTED_EDGE ( 'NONE', *, *, #78405, .T. ) ;
#86764 = B_SPLINE_CURVE_WITH_KNOTS ( 'NONE', 3,
 ( #44625, #77513, #3626, #45679, #69951, #12226, #94776, #45156 ),
 .UNSPECIFIED., .F., .F.,
 ( 4, 2, 2, 4 ),
 ( 0.000000000000000000, 0.5000000000000000000, 0.7500000000000000000, 1.000000000000000000 ),
 .UNSPECIFIED. ) ;
#86765 = EDGE_LOOP ( 'NONE', ( #91220, #30785, #5184, #93863, #44378 ) ) ;
#86766 = EDGE_LOOP ( 'NONE', ( #70971, #53103, #30173, #36538, #66301, #42821 ) ) ;
#86767 = CARTESIAN_POINT ( 'NONE',  ( 55.71012702596955535, -18.68161350975861978, 53.46581880971264411 ) ) ;
#86768 = AXIS2_PLACEMENT_3D ( 'NONE', #16872, #59463, #65940 ) ;
#86769 = CARTESIAN_POINT ( 'NONE',  ( 43.89370568762518587, 435.4157859806081206, 16.19551141317264253 ) ) ;
#86770 = CARTESIAN_POINT ( 'NONE',  ( 0.000000000000000000, 0.000000000000000000, -13.00000000000000000 ) ) ;
#86771 = ORIENTED_EDGE ( 'NONE', *, *, #16509, .T. ) ;
#86772 = DIRECTION ( 'NONE',  ( -0.5735764363510461594, 0.8191520442889916875, 1.003171929053524870E-16 ) ) ;
#86773 = VERTEX_POINT ( 'NONE', #59715 ) ;
#86774 = CARTESIAN_POINT ( 'NONE',  ( 0.2565376335216161818, -2.516992571280038504, -6.500000000000001776 ) ) ;
#86775 = CARTESIAN_POINT ( 'NONE',  ( 94.08446777513815107, -38.49224043567311071, 201.1962447641767540 ) ) ;
#86776 = CARTESIAN_POINT ( 'NONE',  ( 10.18950581449328396, 16.02640291263062622, 10.16991645412965362 ) ) ;
#86777 = CARTESIAN_POINT ( 'NONE',  ( 83.68965721369660571, -45.28337549153452102, 9.534655265776285304 ) ) ;
#86778 = DIRECTION ( 'NONE',  ( 1.000000000000000000, 0.000000000000000000, 0.000000000000000000 ) ) ;
#86779 = CARTESIAN_POINT ( 'NONE',  ( 40.95762649053725113, 390.9034865917477646, 27.40818397757877634 ) ) ;
#86780 = CARTESIAN_POINT ( 'NONE',  ( -42.77633007792896791, 465.0956601421924006, 12.68100826425808414 ) ) ;
#86781 = CARTESIAN_POINT ( 'NONE',  ( -42.08762648273019380, 487.0030674539066808, 9.106351919860241395 ) ) ;
#86782 = FACE_OUTER_BOUND ( 'NONE', #12538, .T. ) ;
#86783 = ORIENTED_EDGE ( 'NONE', *, *, #45856, .T. ) ;
#86784 = EDGE_CURVE ( 'NONE', #61668, #76086, #67274, .T. ) ;
#86785 = CARTESIAN_POINT ( 'NONE',  ( 5.947762761376478302, 6.880090707843046438, 1.083333333333333481 ) ) ;
#86786 = CARTESIAN_POINT ( 'NONE',  ( 7.321078409834592904, 40.29402549786116339, -70.66288766115398801 ) ) ;
#86787 = CARTESIAN_POINT ( 'NONE',  ( -3.625510372800185177, 129.4077472144158492, 5.000000000000000000 ) ) ;
#86788 = EDGE_LOOP ( 'NONE', ( #81805, #13919 ) ) ;
#86789 = CARTESIAN_POINT ( 'NONE',  ( -29.40856938088932182, 310.8503673664380358, -7.608145749800559798 ) ) ;
#86790 = CARTESIAN_POINT ( 'NONE',  ( -38.31345439580793055, 310.9608064124970497, 5.782998304085245067 ) ) ;
#86791 = CARTESIAN_POINT ( 'NONE',  ( -10.67808697576670873, -5.000000000000000888, -77.27709671284311810 ) ) ;
#86792 = CARTESIAN_POINT ( 'NONE',  ( 7.999999999999998224, -21.59374999999999289, 3.313708498984766493 ) ) ;
#86793 = CARTESIAN_POINT ( 'NONE',  ( -33.88587854726462467, -34.92297979730529534, 43.18992221583581426 ) ) ;
#86794 = EDGE_CURVE ( 'NONE', #21594, #85984, #41096, .T. ) ;
#86795 = LINE ( 'NONE', #28570, #1940 ) ;
#86796 = AXIS2_PLACEMENT_3D ( 'NONE', #88666, #5099, #4034 ) ;
#86797 = VERTEX_POINT ( 'NONE', #66190 ) ;
#86798 = CARTESIAN_POINT ( 'NONE',  ( 85.85839205898065529, -25.04722136935922450, 177.1349197526708679 ) ) ;
#86799 = DIRECTION ( 'NONE',  ( 0.000000000000000000, 0.000000000000000000, -1.000000000000000000 ) ) ;
#86800 = ORIENTED_EDGE ( 'NONE', *, *, #3652, .T. ) ;
#86801 =( GEOMETRIC_REPRESENTATION_CONTEXT ( 3 ) GLOBAL_UNCERTAINTY_ASSIGNED_CONTEXT ( ( #2340 ) ) GLOBAL_UNIT_ASSIGNED_CONTEXT ( ( #36595, #60322, #76464 ) ) REPRESENTATION_CONTEXT ( 'NONE', 'WORKASPACE' ) );
#86802 = CARTESIAN_POINT ( 'NONE',  ( -93.98801953623500083, -37.82080309286048703, 101.9196238546772548 ) ) ;
#86803 = SURFACE_STYLE_USAGE ( .BOTH. , #93286 ) ;
#86804 = CARTESIAN_POINT ( 'NONE',  ( -12.76706325321399049, -5.000000000000002665, -81.58101990454278507 ) ) ;
#86805 = CARTESIAN_POINT ( 'NONE',  ( 15.83991689176772866, -4.333298119783770552, 8.379008989516183448 ) ) ;
#86806 = LINE ( 'NONE', #60931, #56142 ) ;
#86807 = EDGE_CURVE ( 'NONE', #5468, #30156, #25791, .T. ) ;
#86808 =( LENGTH_UNIT ( ) NAMED_UNIT ( * ) SI_UNIT ( .MILLI., .METRE. ) );
#86809 = CARTESIAN_POINT ( 'NONE',  ( 1.343583726616268681, -18.03024427876663793, 35.00504070719485838 ) ) ;
#86810 = FILL_AREA_STYLE_COLOUR ( '', #53098 ) ;
#86811 = CARTESIAN_POINT ( 'NONE',  ( 49.75182367352914525, -29.64110475095384700, 46.21721366459617286 ) ) ;
#86813 = CARTESIAN_POINT ( 'NONE',  ( -11.45111553290054474, 14.76784682119976289, 9.859086153280458120 ) ) ;
#86812 = CARTESIAN_POINT ( 'NONE',  ( 0.5974722283283642188, -8.315303285985693904, -0.7026937717022943009 ) ) ;
#86814 = EDGE_CURVE ( 'NONE', #103201, #26677, #86866, .T. ) ;
#86815 = CARTESIAN_POINT ( 'NONE',  ( 1.798224084799555200, 298.0247695551061042, -10.00218504963162758 ) ) ;
#86816 = CARTESIAN_POINT ( 'NONE',  ( 40.07586470527510158, 337.7832441655235129, 20.21182470898328631 ) ) ;
#86817 =( NAMED_UNIT ( * ) PLANE_ANGLE_UNIT ( ) SI_UNIT ( $, .RADIAN. ) );
#86818 = DIRECTION ( 'NONE',  ( 0.000000000000000000, 0.000000000000000000, 1.000000000000000000 ) ) ;
#86819 = CARTESIAN_POINT ( 'NONE',  ( -86.44795749754025849, -38.00000000000003553, 55.89569772577183215 ) ) ;
#86820 = ADVANCED_FACE ( 'NONE', ( #82910 ), #7590, .T. ) ;
#86821 = COLOUR_RGB ( '', 0.66274510, 0.83137255, 0.94901961) ;
#86822 = ORIENTED_EDGE ( 'NONE', *, *, #86060, .T. ) ;
#86823 = CARTESIAN_POINT ( 'NONE',  ( -14.83485053268217158, 0.1083361287566932396, 15.00090388149735254 ) ) ;
#86824 = CARTESIAN_POINT ( 'NONE',  ( 46.00000000000000000, 487.9624651068497201, 0.8047872055790837864 ) ) ;
#86825 = CARTESIAN_POINT ( 'NONE',  ( -42.23079339798738374, 460.7352525929354101, 2.726051457480726636 ) ) ;
#86828 = EDGE_CURVE ( 'NONE', #72809, #90326, #66683, .T. ) ;
#86827 = CARTESIAN_POINT ( 'NONE',  ( -9.567179087380816682, -47.40889396972781356, -34.57814075494444950 ) ) ;
#86826 = CARTESIAN_POINT ( 'NONE',  ( 18.00000000000001421, -20.00000000000001776, -9.000000000000008882 ) ) ;
#86829 = VERTEX_POINT ( 'NONE', #42445 ) ;
#86830 = STYLED_ITEM ( 'NONE', ( #63703 ), #16277 ) ;
#86831 = CARTESIAN_POINT ( 'NONE',  ( -43.71037717921252863, 462.3391554988666599, 4.824299547746595529 ) ) ;
#86832 =( NAMED_UNIT ( * ) PLANE_ANGLE_UNIT ( ) SI_UNIT ( $, .RADIAN. ) );
#86833 = ORIENTED_EDGE ( 'NONE', *, *, #16415, .F. ) ;
#86834 = CARTESIAN_POINT ( 'NONE',  ( 66.00571552735603120, 4.000000000000013323, 0.000000000000000000 ) ) ;
#86835 = DIRECTION ( 'NONE',  ( -1.000000000000000000, -0.000000000000000000, -0.000000000000000000 ) ) ;
#86836 = CARTESIAN_POINT ( 'NONE',  ( -93.40600019352365280, -60.00000000000000000, 36.18128804451619374 ) ) ;
#86837 = B_SPLINE_CURVE_WITH_KNOTS ( 'NONE', 3,
 ( #96123, #28776, #45456, #86981, #22786, #13585, #62187, #63761, #4447, #21206 ),
 .UNSPECIFIED., .F., .F.,
 ( 4, 2, 2, 2, 4 ),
 ( 1.909096309310500434E-19, 0.001989602278884367460, 0.003979204557768734919, 0.005968806836653102812, 0.007958409115537469838 ),
 .UNSPECIFIED. ) ;
#86838 = EDGE_LOOP ( 'NONE', ( #34854, #77977, #50572, #52555 ) ) ;
#86839 = DIRECTION ( 'NONE',  ( -0.000000000000000000, -0.000000000000000000, -1.000000000000000000 ) ) ;
#86840 = CARTESIAN_POINT ( 'NONE',  ( 44.46823338009918558, -5.000000000000000000, 6.123233995736768255E-16 ) ) ;
#86841 = CARTESIAN_POINT ( 'NONE',  ( -3.454253436624922458, -49.15858197120396511, 103.7259032015043090 ) ) ;
#86842 = FACE_OUTER_BOUND ( 'NONE', #36544, .T. ) ;
#86843 = CARTESIAN_POINT ( 'NONE',  ( -85.74753642962151901, -18.52699961319207134, 162.5183481292275758 ) ) ;
#86844 = ORIENTED_EDGE ( 'NONE', *, *, #2619, .T. ) ;
#86845 = CARTESIAN_POINT ( 'NONE',  ( -2.220638482700625804, -0.000000000000000000, -16.90642566760435983 ) ) ;
#86846 = EDGE_LOOP ( 'NONE', ( #83801, #106297, #81934, #95788, #99145, #10531, #104100 ) ) ;
#86847 = EDGE_LOOP ( 'NONE', ( #38562, #73554, #101640, #22445, #58828, #23713 ) ) ;
#86848 = EDGE_CURVE ( 'NONE', #95837, #75560, #69840, .T. ) ;
#86849 = CARTESIAN_POINT ( 'NONE',  ( -6.611670918688361098, -11.93296314122861190, 9.735702799542698571 ) ) ;
#86850 = FILL_AREA_STYLE_COLOUR ( '', #38111 ) ;
#86851 = EDGE_LOOP ( 'NONE', ( #39418, #21385, #44442, #80527, #84685 ) ) ;
#86852 = CARTESIAN_POINT ( 'NONE',  ( 16.64348903516512834, 45.60392139269950462, -6.657797401561770911 ) ) ;
#86853 = DIRECTION ( 'NONE',  ( -1.000000000000000000, -1.224606353822377258E-16, -0.000000000000000000 ) ) ;
#86854 = CARTESIAN_POINT ( 'NONE',  ( -100.9355741078537676, -57.67123050614609525, 74.71304529006944506 ) ) ;
#86855 = CARTESIAN_POINT ( 'NONE',  ( 7.934203308536662114, -13.86700340017798183, 1.057099537198543882 ) ) ;
#86856 = CARTESIAN_POINT ( 'NONE',  ( 43.53200981659315971, 464.6079291498570001, 9.489543392920072762 ) ) ;
#86857 = CARTESIAN_POINT ( 'NONE',  ( -9.999952458099485852, 101.0001188547613395, 0.2653554233229110104 ) ) ;
#86858 = CARTESIAN_POINT ( 'NONE',  ( -13.69909788704105935, -51.35317944603409046, 24.10694589033532154 ) ) ;
#86859 = CARTESIAN_POINT ( 'NONE',  ( 3.082707893549470057, 15.00000000000000178, -9.999999999999998224 ) ) ;
#86860 = CARTESIAN_POINT ( 'NONE',  ( 82.54285424309888697, -59.99999999999997868, -29.20801037391389698 ) ) ;
#86861 = ADVANCED_FACE ( 'NONE', ( #98546 ), #1437, .T. ) ;
#86862 = CARTESIAN_POINT ( 'NONE',  ( -69.85357985695409866, -59.99999999999993605, 155.8687211249902873 ) ) ;
#86863 = CARTESIAN_POINT ( 'NONE',  ( -54.66613860792094926, -42.97099802834101467, 60.96799278605171679 ) ) ;
#86864 = ORIENTED_EDGE ( 'NONE', *, *, #73248, .F. ) ;
#86865 = CARTESIAN_POINT ( 'NONE',  ( 5.835411572216777643, 14.05761036835583333, -3.866789010015639239 ) ) ;
#86866 = CIRCLE ( 'NONE', #102564, 4.000000000000007105 ) ;
#86867 = VERTEX_POINT ( 'NONE', #42990 ) ;
#86868 = CARTESIAN_POINT ( 'NONE',  ( -102.3879661117660334, -52.71380871076068786, 191.3657242593055798 ) ) ;
#86869 = CARTESIAN_POINT ( 'NONE',  ( -30.71756172600976953, 13.08262462249239633, -41.56006324341318958 ) ) ;
#86870 = ORIENTED_EDGE ( 'NONE', *, *, #102114, .F. ) ;
#86871 = CARTESIAN_POINT ( 'NONE',  ( 19.45280783995336193, 49.97908042910276549, 60.60017717165798246 ) ) ;
#86872 =( GEOMETRIC_REPRESENTATION_CONTEXT ( 3 ) GLOBAL_UNCERTAINTY_ASSIGNED_CONTEXT ( ( #43350 ) ) GLOBAL_UNIT_ASSIGNED_CONTEXT ( ( #81759, #90414, #17064 ) ) REPRESENTATION_CONTEXT ( 'NONE', 'WORKASPACE' ) );
#86873 = FACE_OUTER_BOUND ( 'NONE', #75744, .T. ) ;
#86874 = CARTESIAN_POINT ( 'NONE',  ( -7.188101187500001821, -12.87500000204838813, -2.977408999572651371 ) ) ;
#86875 = EDGE_CURVE ( 'NONE', #20727, #12676, #39762, .T. ) ;
#86876 = CARTESIAN_POINT ( 'NONE',  ( -4.220606381948455166, -66.96246410476639710, 13.14687599345784896 ) ) ;
#86877 = CARTESIAN_POINT ( 'NONE',  ( 29.66054107240687543, 1.482358050883964840E-15, 0.000000000000000000 ) ) ;
#86878 = FACE_OUTER_BOUND ( 'NONE', #47202, .T. ) ;
#86879 = CARTESIAN_POINT ( 'NONE',  ( -34.95237279327285762, 304.8277712208536627, 12.26231981495593537 ) ) ;
#86880 = CARTESIAN_POINT ( 'NONE',  ( -7.948255254545235182, 97.89041063984025470, 1.301042606982605321E-15 ) ) ;
#86881 = DIRECTION ( 'NONE',  ( -0.000000000000000000, -0.000000000000000000, -1.000000000000000000 ) ) ;
#86882 = CARTESIAN_POINT ( 'NONE',  ( -33.70841932975971389, 485.0774894644218307, 1.934193826885679313 ) ) ;
#86883 = UNCERTAINTY_MEASURE_WITH_UNIT (LENGTH_MEASURE( 1.000000000000000082E-05 ), #92032, 'distance_accuracy_value', 'NONE');
#86884 = CARTESIAN_POINT ( 'NONE',  ( -28.17640869695596706, -60.34565798028340566, 36.16065794429692204 ) ) ;
#86885 = VERTEX_POINT ( 'NONE', #84515 ) ;
#86886 = ORIENTED_EDGE ( 'NONE', *, *, #73375, .T. ) ;
#86887 = CARTESIAN_POINT ( 'NONE',  ( 48.45783950018828534, -56.82067350140248152, 53.79819978640338718 ) ) ;
#86888 = VERTEX_POINT ( 'NONE', #12729 ) ;
#86889 = DIRECTION ( 'NONE',  ( 0.000000000000000000, 0.000000000000000000, 1.000000000000000000 ) ) ;
#86890 = CARTESIAN_POINT ( 'NONE',  ( -6.560102024233680496, 16.17028887884159971, -2.452861370513718331 ) ) ;
#86891 = CARTESIAN_POINT ( 'NONE',  ( -110.8707848989685516, -38.35619458718431929, 167.2301363532564267 ) ) ;
#86892 = VERTEX_POINT ( 'NONE', #93131 ) ;
#86893 = CARTESIAN_POINT ( 'NONE',  ( 91.22471603993383837, -38.35915892665957472, -1.047709165501598427 ) ) ;
#86894 = CARTESIAN_POINT ( 'NONE',  ( 13.66298729346737773, 5.052113668166707150, -6.101274280624832791 ) ) ;
#86895 = LINE ( 'NONE', #53456, #75046 ) ;
#86896 = CARTESIAN_POINT ( 'NONE',  ( 11.04004868613161072, 43.74858494517264518, 13.15750084466564118 ) ) ;
#86897 = CARTESIAN_POINT ( 'NONE',  ( 6.208655437490365969, 40.93126392761964638, -71.11611063721394999 ) ) ;
#86898 = CARTESIAN_POINT ( 'NONE',  ( -32.65708775173074230, 434.9895743886469859, 13.53061570434023153 ) ) ;
#86899 = CARTESIAN_POINT ( 'NONE',  ( -31.17290040000586515, 438.0040945452082042, 21.19833760118956789 ) ) ;
#86900 = CARTESIAN_POINT ( 'NONE',  ( 12.50000000000000533, -3.000000000000000000, -55.73109925765190553 ) ) ;
#86901 = CARTESIAN_POINT ( 'NONE',  ( 109.7065984538688923, -60.00000000000000711, 191.9969423268659057 ) ) ;
#86902 = VECTOR ( 'NONE', #15537, 1000.000000000000000 ) ;
#86903 = TOROIDAL_SURFACE ( 'NONE', #52446, 62.00000000000000000, 0.5000000000000000000 ) ;
#86904 = DIRECTION ( 'NONE',  ( -1.000000000000000000, -1.224606353822377258E-16, -0.000000000000000000 ) ) ;
#86905 = ORIENTED_EDGE ( 'NONE', *, *, #34766, .T. ) ;
#86906 = EDGE_CURVE ( 'NONE', #74088, #77482, #47412, .T. ) ;
#86907 = CARTESIAN_POINT ( 'NONE',  ( 3.677391134430175512, -48.98477995422159381, 104.0097548473154916 ) ) ;
#86908 = AXIS2_PLACEMENT_3D ( 'NONE', #85476, #68773, #75775 ) ;
#86909 =( GEOMETRIC_REPRESENTATION_CONTEXT ( 3 ) GLOBAL_UNCERTAINTY_ASSIGNED_CONTEXT ( ( #76107 ) ) GLOBAL_UNIT_ASSIGNED_CONTEXT ( ( #79735, #79205, #77621 ) ) REPRESENTATION_CONTEXT ( 'NONE', 'WORKASPACE' ) );
#86910 = CARTESIAN_POINT ( 'NONE',  ( -7.045755811259133417, 28.69658396986446647, 3.790843699961854441 ) ) ;
#86911 = ORIENTED_EDGE ( 'NONE', *, *, #84117, .T. ) ;
#86913 = CARTESIAN_POINT ( 'NONE',  ( 5.293242423775784466, 18.43190769382419703, -37.80783146079790669 ) ) ;
#86912 = CARTESIAN_POINT ( 'NONE',  ( -91.33478035347820878, -38.36421997627891045, -2.728810306399620078 ) ) ;
#86914 = CARTESIAN_POINT ( 'NONE',  ( 46.00000000000000000, 437.9217094256704854, 13.73710413246956641 ) ) ;
#86915 = DIRECTION ( 'NONE',  ( -0.000000000000000000, 1.000000000000000000, -0.000000000000000000 ) ) ;
#86916 =( NAMED_UNIT ( * ) PLANE_ANGLE_UNIT ( ) SI_UNIT ( $, .RADIAN. ) );
#86917 = CARTESIAN_POINT ( 'NONE',  ( -7.188101187500001821, -14.37500000204838635, -2.977408999572651371 ) ) ;
#86918 = CARTESIAN_POINT ( 'NONE',  ( -9.739726766101606259, -5.000000000000002665, -82.38252115500968387 ) ) ;
#86919 = ADVANCED_FACE ( 'NONE', ( #19303 ), #74969, .T. ) ;
#86920 = CARTESIAN_POINT ( 'NONE',  ( 32.33349330513380693, -4.000000000000000888, 4.898587196589416773E-16 ) ) ;
#86921 = EDGE_CURVE ( 'NONE', #44907, #71961, #37153, .T. ) ;
#86923 = ORIENTED_EDGE ( 'NONE', *, *, #86828, .F. ) ;
#86922 = CARTESIAN_POINT ( 'NONE',  ( 19.34999999999999787, 1.533819458162526451E-15, 0.000000000000000000 ) ) ;
#86924 = CARTESIAN_POINT ( 'NONE',  ( 85.91903949933247020, -18.46740127454976843, 164.5912266175255070 ) ) ;
#86925 = CARTESIAN_POINT ( 'NONE',  ( -46.00000000000000000, 461.2902899409307338, 8.859728897578733608 ) ) ;
#86926 = DIRECTION ( 'NONE',  ( 0.000000000000000000, -1.000000000000000000, 0.000000000000000000 ) ) ;
#86927 = VERTEX_POINT ( 'NONE', #4660 ) ;
#86928 = CARTESIAN_POINT ( 'NONE',  ( -29.12616872298675474, 306.7985789502500893, -9.112683410444441634 ) ) ;
#86929 = LINE ( 'NONE', #37869, #61614 ) ;
#86930 = CARTESIAN_POINT ( 'NONE',  ( 39.83349330513380693, 4.000000000000003553, 0.000000000000000000 ) ) ;
#86931 = CARTESIAN_POINT ( 'NONE',  ( -4.567209634097059379, 250.9359978608551387, -3.891254717191793056 ) ) ;
#86932 = CARTESIAN_POINT ( 'NONE',  ( -42.58433969240390127, 479.4768267386957632, 9.887265036231987381 ) ) ;
#86933 = B_SPLINE_SURFACE_WITH_KNOTS ( 'NONE', 3, 1, ( 
 ( #92226, #10772 ),
 ( #68515, #76050 ),
 ( #100860, #36713 ),
 ( #69578, #101924 ) ),
 .UNSPECIFIED., .F., .F., .F.,
 ( 4, 4 ),
 ( 2, 2 ),
 ( 0.000000000000000000, 0.9982556956955090932 ),
 ( 0.000000000000000000, 1.000000000000000000 ),
 .UNSPECIFIED. ) ;
#86934 = CONICAL_SURFACE ( 'NONE', #90614, 7.000000000000000000, 0.9599310885968753704 ) ;
#86935 = EDGE_CURVE ( 'NONE', #29277, #12516, #56777, .T. ) ;
#86936 = ORIENTED_EDGE ( 'NONE', *, *, #18926, .F. ) ;
#86937 = AXIS2_PLACEMENT_3D ( 'NONE', #94318, #20480, #70028 ) ;
#86938 = CARTESIAN_POINT ( 'NONE',  ( -9.492026425949987356, 294.7525273391970586, 3.163606944373883234 ) ) ;
#86939 = CARTESIAN_POINT ( 'NONE',  ( 37.72560624927822914, 25.42169923041442559, 13.45617127781006950 ) ) ;
#86941 = EDGE_CURVE ( 'NONE', #75237, #2439, #86011, .T. ) ;
#86940 = DIRECTION ( 'NONE',  ( 1.000000000000000000, -0.000000000000000000, -0.000000000000000000 ) ) ;
#86943 = FACE_OUTER_BOUND ( 'NONE', #54722, .T. ) ;
#86942 = DIRECTION ( 'NONE',  ( 0.000000000000000000, -0.000000000000000000, 1.000000000000000000 ) ) ;
#86944 = PRESENTATION_LAYER_ASSIGNMENT (  '', '', ( #18028 ) ) ;
#86945 = CARTESIAN_POINT ( 'NONE',  ( -7.188101187500001821, -17.00000000204838457, -2.977408999572651371 ) ) ;
#86946 = CARTESIAN_POINT ( 'NONE',  ( 46.00000000000000000, 438.0652200859153140, 14.81161132415559578 ) ) ;
#86947 = PRESENTATION_LAYER_ASSIGNMENT (  '', '', ( #31811 ) ) ;
#86948 = CARTESIAN_POINT ( 'NONE',  ( 8.716351559230176349, -4.999999999999999112, 5.062179317057519334 ) ) ;
#86949 = PRESENTATION_LAYER_ASSIGNMENT (  '', '', ( #28454 ) ) ;
#86950 = VECTOR ( 'NONE', #3296, 1000.000000000000000 ) ;
#86951 = ITEM_DEFINED_TRANSFORMATION ( 'NONE', 'NONE', #78263,  #10728 ) ;
#86952 = ORIENTED_EDGE ( 'NONE', *, *, #31867, .T. ) ;
#86953 = CARTESIAN_POINT ( 'NONE',  ( 41.71039089155822666, 485.6269440496952825, -4.295528331870388072 ) ) ;
#86954 = CARTESIAN_POINT ( 'NONE',  ( -5.363597346089342466, 41.33266196706077267, -58.39526881795508473 ) ) ;
#86955 = CARTESIAN_POINT ( 'NONE',  ( -8.985503747028566579, 15.44863866163618304, -5.000000000000635048 ) ) ;
#86956 = DIRECTION ( 'NONE',  ( 0.000000000000000000, 0.000000000000000000, 1.000000000000000000 ) ) ;
#86957 = CARTESIAN_POINT ( 'NONE',  ( -14.89734172080860297, 1.349300515452548588, 1.760806480411474695 ) ) ;
#86958 = ORIENTED_EDGE ( 'NONE', *, *, #9971, .F. ) ;
#86959 = FACE_OUTER_BOUND ( 'NONE', #27575, .T. ) ;
#86960 = CARTESIAN_POINT ( 'NONE',  ( 9.312033689592260188, 50.00000000000000000, -94.29807022305527653 ) ) ;
#86961 = EDGE_LOOP ( 'NONE', ( #33434, #26781 ) ) ;
#86962 = EDGE_CURVE ( 'NONE', #27782, #63587, #97379, .T. ) ;
#86963 = CARTESIAN_POINT ( 'NONE',  ( -27.72495481923087368, 34.28547018021359349, 9.895597501992106970 ) ) ;
#86964 = CARTESIAN_POINT ( 'NONE',  ( -3.499286860947127931, -0.8580408876376250937, 104.2445795335848544 ) ) ;
#86965 = DIRECTION ( 'NONE',  ( 0.000000000000000000, 1.000000000000000000, 0.000000000000000000 ) ) ;
#86966 = UNCERTAINTY_MEASURE_WITH_UNIT (LENGTH_MEASURE( 1.000000000000000082E-05 ), #30600, 'distance_accuracy_value', 'NONE');
#86967 = CARTESIAN_POINT ( 'NONE',  ( -104.3903561930018355, -60.00000000000000000, 199.7463460733462171 ) ) ;
#86968 = CARTESIAN_POINT ( 'NONE',  ( 0.000000000000000000, 45.00000000000000711, 0.000000000000000000 ) ) ;
#86969 = CARTESIAN_POINT ( 'NONE',  ( 38.47428897412579119, 485.7788508071993760, -4.770630528148342542 ) ) ;
#86970 = CARTESIAN_POINT ( 'NONE',  ( 16.14595037822613932, 20.23371447307438586, 4.922994507617745263 ) ) ;
#86971 = CARTESIAN_POINT ( 'NONE',  ( -83.96270013590550718, -39.45081235419423393, 178.0757026163669821 ) ) ;
#86972 = DIRECTION ( 'NONE',  ( -1.000000000000000000, -1.224606353822377258E-16, -0.000000000000000000 ) ) ;
#86973 = VERTEX_POINT ( 'NONE', #68331 ) ;
#86974 = ADVANCED_FACE ( 'NONE', ( #45652 ), #92217, .T. ) ;
#86975 = CARTESIAN_POINT ( 'NONE',  ( 5.382954851612914204, -67.99987491489444835, -2.657971597726724866 ) ) ;
#86976 = MECHANICAL_DESIGN_GEOMETRIC_PRESENTATION_REPRESENTATION (  '', ( #39691 ), #58625 ) ;
#86977 = CARTESIAN_POINT ( 'NONE',  ( -84.64863869684523934, -45.26546037518905052, 31.07901721422380703 ) ) ;
#86978 = CARTESIAN_POINT ( 'NONE',  ( 10.28624191511840280, 46.12099395432375104, 12.90779740156148847 ) ) ;
#86979 = CARTESIAN_POINT ( 'NONE',  ( -4.315100334823573469, 141.0329282757117824, -5.000000000000000000 ) ) ;
#86980 = CARTESIAN_POINT ( 'NONE',  ( 9.517802784862999133, 142.5467050672999676, 0.000000000000000000 ) ) ;
#86981 = CARTESIAN_POINT ( 'NONE',  ( -2.262848203703083261, -6.566616684922180092, -6.208169345099799230 ) ) ;
#86982 = CARTESIAN_POINT ( 'NONE',  ( -10.04205104296119622, 18.64316884715858080, 37.36680950591986772 ) ) ;
#86983 = CARTESIAN_POINT ( 'NONE',  ( 100.3457197225335733, -14.21045842199427511, 196.5350150060856720 ) ) ;
#86984 = CARTESIAN_POINT ( 'NONE',  ( -119.0671996398097008, 7.666536031838888654, -59.53359981990485750 ) ) ;
#86985 = EDGE_CURVE ( 'NONE', #99690, #24250, #103354, .T. ) ;
#86986 = CARTESIAN_POINT ( 'NONE',  ( -101.2960459709432826, -29.99999999999998579, 104.2733491104911963 ) ) ;
#86987 = B_SPLINE_CURVE_WITH_KNOTS ( 'NONE', 3,
 ( #33864, #33324, #15516, #66195, #48407, #31730, #99079, #64617, #91030, #17133, #50010, #82914, #9012, #96975, #23109, #55951, #88885, #14976, #11131, #10087, #2518, #44061, #34932, #27925, #100159, #18754, #3062, #100684, #52135, #67281, #58653, #60792, #25800, #51603, #76949, #77493, #93139, #27390, #91554, #36010, #17663, #84524, #75884, #92598, #11670, #26326, #19832, #10610 ),
 .UNSPECIFIED., .F., .F.,
 ( 4, 2, 2, 2, 2, 2, 2, 2, 2, 2, 2, 2, 2, 2, 2, 2, 2, 2, 2, 2, 2, 2, 2, 4 ),
 ( 0.0009115642548457684189, 0.01973540046764989814, 0.03855923668045402319, 0.05738307289325814825, 0.06679499099966014486, 0.07620690910606212065, 0.08561882721246411032, 0.09503074531886608611, 0.1044426634252680758, 0.1138545815316700377, 0.1185605405848710187, 0.1232664996380720135, 0.1256194791646725040, 0.1279724586912729944, 0.1326784177444739754, 0.1350313972710744659, 0.1373843767976749564, 0.1397373563242754191, 0.1409138460875756782, 0.1420903358508759096, 0.1444433153774764000, 0.1456198051407766314, 0.1467962949040768905, 0.1515022539572777605 ),
 .UNSPECIFIED. ) ;
#86988 = CARTESIAN_POINT ( 'NONE',  ( -64.78455580451337426, -22.10248187533688125, 76.63264628624035879 ) ) ;
#86989 = ORIENTED_EDGE ( 'NONE', *, *, #41133, .T. ) ;
#86990 = CARTESIAN_POINT ( 'NONE',  ( -5.921793164125095821, 39.42528690638199862, 64.79870964707900782 ) ) ;
#86991 = CARTESIAN_POINT ( 'NONE',  ( 68.99430565880821575, -59.99999999999998579, 149.4797282245464203 ) ) ;
#86992 = VERTEX_POINT ( 'NONE', #69399 ) ;
#86993 = CARTESIAN_POINT ( 'NONE',  ( -33.77559172535806908, 464.7834715296606873, 7.192701217093215860 ) ) ;
#86994 = CARTESIAN_POINT ( 'NONE',  ( 4.401442555609581635E-16, -19.15625000204838457, -7.188101187500000044 ) ) ;
#86995 = DIRECTION ( 'NONE',  ( 0.000000000000000000, 0.000000000000000000, -1.000000000000000000 ) ) ;
#86996 = ORIENTED_EDGE ( 'NONE', *, *, #39965, .F. ) ;
#86997 = DIRECTION ( 'NONE',  ( -1.000000000000000000, -1.224606353822377258E-16, -0.000000000000000000 ) ) ;
#86998 = ORIENTED_EDGE ( 'NONE', *, *, #34197, .F. ) ;
#86999 = CARTESIAN_POINT ( 'NONE',  ( 10.28624191512063746, 46.12099395432516502, -12.90779740155508826 ) ) ;
#87000 = CARTESIAN_POINT ( 'NONE',  ( 47.77442396816185521, 17.34920168383012040, -14.37330342454831289 ) ) ;
#87001 = CARTESIAN_POINT ( 'NONE',  ( -2.833865952193512783, -59.99999999997060485, 41.99999969629084973 ) ) ;
#87002 = CARTESIAN_POINT ( 'NONE',  ( 3.898086217683919497, -13.33789614101576149, -0.2204769333331217940 ) ) ;
#87003 = CARTESIAN_POINT ( 'NONE',  ( 5.082755093536324154, -31.71875000204838457, 5.082755093536326818 ) ) ;
#87004 = EDGE_CURVE ( 'NONE', #99083, #95250, #26849, .T. ) ;
#87005 = CARTESIAN_POINT ( 'NONE',  ( -32.10528697966012857, 486.1671898930081852, 5.449875171704860577 ) ) ;
#87006 = CARTESIAN_POINT ( 'NONE',  ( 0.000000000000000000, 4.898587196589412829E-16, -4.000000000000000000 ) ) ;
#87007 = CARTESIAN_POINT ( 'NONE',  ( 5.000000000000000888, -48.52751354257630823, 2.643394033337469473 ) ) ;
#87008 = CARTESIAN_POINT ( 'NONE',  ( 1.308996937483428491, 49.99999999999999289, -95.00000000000001421 ) ) ;
#87009 = CARTESIAN_POINT ( 'NONE',  ( 32.92227116393141984, 439.7404285724723536, 24.14402898922816476 ) ) ;
#87010 = SURFACE_STYLE_FILL_AREA ( #43872 ) ;
#87011 = CONICAL_SURFACE ( 'NONE', #62910, 4.000000000000001776, 0.9599310885968774798 ) ;
#87012 = CARTESIAN_POINT ( 'NONE',  ( 34.46660312962831796, 319.4207929304380968, -5.979192388231528987 ) ) ;
#87013 = ORIENTED_EDGE ( 'NONE', *, *, #74203, .T. ) ;
#87014 = CARTESIAN_POINT ( 'NONE',  ( -9.812456964692255923, 53.40207289977589511, -2.924987046467517171 ) ) ;
#87015 = CARTESIAN_POINT ( 'NONE',  ( 33.67987230928347486, -22.16572803534493019, 31.32075179795772257 ) ) ;
#87016 = AXIS2_PLACEMENT_3D ( 'NONE', #54885, #71605, #44298 ) ;
#87017 = CARTESIAN_POINT ( 'NONE',  ( 11.19959342722337681, 2.897043466792154898E-12, -19.43146043914873289 ) ) ;
#87018 = ORIENTED_EDGE ( 'NONE', *, *, #92768, .T. ) ;
#87019 = CARTESIAN_POINT ( 'NONE',  ( 0.000000000000000000, 81.00000000000000000, 0.000000000000000000 ) ) ;
#87020 = VECTOR ( 'NONE', #17979, 1000.000000000000000 ) ;
#87022 = CARTESIAN_POINT ( 'NONE',  ( -24.80105969489321893, 306.0237540681346218, -9.745911707960095427 ) ) ;
#87021 = CARTESIAN_POINT ( 'NONE',  ( 9.499926694067500677, -5.000000000000000888, -20.04229455990067166 ) ) ;
#87023 = CYLINDRICAL_SURFACE ( 'NONE', #87177, 5.000000000000000888 ) ;
#87024 = CARTESIAN_POINT ( 'NONE',  ( -23.21751746555244722, -1.200000000000000030E-05, 30.70617127781060418 ) ) ;
#87025 = VECTOR ( 'NONE', #64581, 1000.000000000000000 ) ;
#87026 =( GEOMETRIC_REPRESENTATION_CONTEXT ( 3 ) GLOBAL_UNCERTAINTY_ASSIGNED_CONTEXT ( ( #102060 ) ) GLOBAL_UNIT_ASSIGNED_CONTEXT ( ( #23306, #23848, #89616 ) ) REPRESENTATION_CONTEXT ( 'NONE', 'WORKASPACE' ) );
#87027 = SURFACE_SIDE_STYLE ('',( #85973 ) ) ;
#87028 = AXIS2_PLACEMENT_3D ( 'NONE', #48201, #39082, #13712 ) ;
#87029 = CARTESIAN_POINT ( 'NONE',  ( 0.5805565836007602343, 3.752776749732561257, -6.499999999999999112 ) ) ;
#87030 = FACE_OUTER_BOUND ( 'NONE', #61688, .T. ) ;
#87031 = ORIENTED_EDGE ( 'NONE', *, *, #103584, .F. ) ;
#87032 = CARTESIAN_POINT ( 'NONE',  ( 92.20688357260412715, -60.00000000000002132, 2.776348851982239463 ) ) ;
#87033 = DIRECTION ( 'NONE',  ( -1.000000000000000000, -1.224606353822377258E-16, -0.000000000000000000 ) ) ;
#87034 = CIRCLE ( 'NONE', #105928, 5.000000000000001776 ) ;
#87035 = CYLINDRICAL_SURFACE ( 'NONE', #58309, 4.000000000000000000 ) ;
#87036 = CONICAL_SURFACE ( 'NONE', #57722, 7.000000000000000000, 0.9599310885968753704 ) ;
#87037 = CARTESIAN_POINT ( 'NONE',  ( -5.225680118539934860, 40.98154234353523151, -70.87362174390516145 ) ) ;
#87038 = CARTESIAN_POINT ( 'NONE',  ( -12.15584546671134802, 10.26194364132355297, -9.624033779842585901 ) ) ;
#87039 = VERTEX_POINT ( 'NONE', #94199 ) ;
#87040 = EDGE_CURVE ( 'NONE', #26937, #51023, #85157, .T. ) ;
#87041 = B_SPLINE_CURVE_WITH_KNOTS ( 'NONE', 3,
 ( #22118, #103546, #38822, #54430, #104595, #78205, #37255, #78719, #46889, #87376, #12925, #46375, #70118, #103025, #30749, #4321, #77687, #79264, #29693, #21599, #52867, #94946 ),
 .UNSPECIFIED., .F., .F.,
 ( 4, 2, 2, 2, 2, 2, 2, 2, 2, 2, 4 ),
 ( 0.000000000000000000, 0.001580156024417029908, 0.003160312048834081067, 0.004740468073251132008, 0.006320624097668182950, 0.007900780122085233892, 0.009480936146502284834, 0.01027101415871079643, 0.01106109217091930629, 0.01185117018312781788, 0.01264124819533632947 ),
 .UNSPECIFIED. ) ;
#87042 = CARTESIAN_POINT ( 'NONE',  ( -86.00551523489100703, -29.99999999999667821, -19.89116246976540481 ) ) ;
#87043 = ORIENTED_EDGE ( 'NONE', *, *, #75083, .F. ) ;
#87044 = CARTESIAN_POINT ( 'NONE',  ( 28.58349330513380337, 4.000000000000003553, 0.000000000000000000 ) ) ;
#87045 = CARTESIAN_POINT ( 'NONE',  ( 14.29190075645433922, 21.26710225494878514, -5.626279437267652561 ) ) ;
#87046 = CARTESIAN_POINT ( 'NONE',  ( 81.59424421858821574, -37.83104312327714780, -14.43779184493780399 ) ) ;
#87047 = CARTESIAN_POINT ( 'NONE',  ( 7.188101187500001821, -32.93750000204839523, -2.977408999572650483 ) ) ;
#87048 = CARTESIAN_POINT ( 'NONE',  ( 20.24579557674108088, 304.8297271373347144, -10.00469232190996927 ) ) ;
#87049 = CARTESIAN_POINT ( 'NONE',  ( 10.12154985177016364, 46.15835141668620878, -12.90779740156137123 ) ) ;
#87050 = EDGE_CURVE ( 'NONE', #1155, #84498, #14522, .T. ) ;
#87051 = ADVANCED_FACE ( 'NONE', ( #11663 ), #56962, .F. ) ;
#87052 = VERTEX_POINT ( 'NONE', #63441 ) ;
#87053 = ORIENTED_EDGE ( 'NONE', *, *, #81590, .F. ) ;
#87054 = CARTESIAN_POINT ( 'NONE',  ( 77.75032079266158291, -60.30862840971112604, 154.2286336114433141 ) ) ;
#87055 = CARTESIAN_POINT ( 'NONE',  ( 14.97625732068849835, 1.268789641109442812, 0.8714310519259138577 ) ) ;
#87056 = VERTEX_POINT ( 'NONE', #38122 ) ;
#87057 = DIRECTION ( 'NONE',  ( -1.000000000000000000, -0.000000000000000000, -0.000000000000000000 ) ) ;
#87058 = CARTESIAN_POINT ( 'NONE',  ( 7.188101187500000044, -19.15625000204838457, 0.000000000000000000 ) ) ;
#87059 = AXIS2_PLACEMENT_3D ( 'NONE', #13014, #69688, #22219 ) ;
#87060 = CARTESIAN_POINT ( 'NONE',  ( -105.5530292394789882, -57.64680470462099038, 201.3003284212183246 ) ) ;
#87061 = EDGE_CURVE ( 'NONE', #92662, #21224, #105978, .T. ) ;
#87062 = VERTEX_POINT ( 'NONE', #88755 ) ;
#87063 = CARTESIAN_POINT ( 'NONE',  ( 3.225573779814635333, 36.35262730105617379, 4.999999999999998224 ) ) ;
#87064 = CARTESIAN_POINT ( 'NONE',  ( 7.081808280621250340, 41.46696771993406827, -58.88886753944292707 ) ) ;
#87065 = EDGE_CURVE ( 'NONE', #23216, #71690, #21925, .T. ) ;
#87066 = CARTESIAN_POINT ( 'NONE',  ( 49.09761780907516027, 12.98984206366268701, -16.25597134832139901 ) ) ;
#87067 = CARTESIAN_POINT ( 'NONE',  ( -8.000000000000001776, -14.84375000409677092, 3.313708498984758943 ) ) ;
#87068 = CARTESIAN_POINT ( 'NONE',  ( -40.94175040987683190, -26.72553514667153962, 36.58944239903460982 ) ) ;
#87069 = CARTESIAN_POINT ( 'NONE',  ( -36.34489372084551206, 26.08142535203068135, 11.89321794026316681 ) ) ;
#87070 = CARTESIAN_POINT ( 'NONE',  ( -1.000000000000000000, -63.14890303517896086, 9.346194641685219295 ) ) ;
#87071 = EDGE_CURVE ( 'NONE', #74465, #55990, #69686, .T. ) ;
#87072 = CARTESIAN_POINT ( 'NONE',  ( -9.483056940782029542, 87.44387790106578962, -3.177305548492604270 ) ) ;
#87073 = AXIS2_PLACEMENT_3D ( 'NONE', #28737, #76170, #28209 ) ;
#87074 = DIRECTION ( 'NONE',  ( 4.233437538138742344E-17, 0.1845977156002912289, 0.9828141652393672656 ) ) ;
#87075 = CARTESIAN_POINT ( 'NONE',  ( -9.176855344542989457, 30.52960426977409725, -3.973472207155926750 ) ) ;
#87076 = VERTEX_POINT ( 'NONE', #87705 ) ;
#87077 = CARTESIAN_POINT ( 'NONE',  ( -3.338674867580755379, -49.24767650228190519, 44.08270169569225061 ) ) ;
#87078 = CARTESIAN_POINT ( 'NONE',  ( 11.74288065822411831, -4.879695075740994703, -12.55922237203875191 ) ) ;
#87079 = CARTESIAN_POINT ( 'NONE',  ( -42.20041562234357002, 435.2369744135583574, 7.788607701745487333 ) ) ;
#87080 = CARTESIAN_POINT ( 'NONE',  ( 75.51533756583158663, -29.99999999999997868, -27.33238513093786537 ) ) ;
#87081 = CARTESIAN_POINT ( 'NONE',  ( -68.54014073437507193, -30.00000000000000000, 90.70798278420799932 ) ) ;
#87082 = CARTESIAN_POINT ( 'NONE',  ( 0.000000000000000000, 0.000000000000000000, -6.606815774914157835 ) ) ;
#87083 = STYLED_ITEM ( 'NONE', ( #55431 ), #63566 ) ;
#87084 = EDGE_LOOP ( 'NONE', ( #100490, #95241, #91285, #64379 ) ) ;
#87085 = DIRECTION ( 'NONE',  ( -1.000000000000000000, -0.000000000000000000, -0.000000000000000000 ) ) ;
#87086 = CARTESIAN_POINT ( 'NONE',  ( 82.51619662115577114, -57.52811307887816383, 200.8615502966897566 ) ) ;
#87087 = CARTESIAN_POINT ( 'NONE',  ( 72.96298303301223598, -34.58959179241216475, -20.39840084324062985 ) ) ;
#87088 = CARTESIAN_POINT ( 'NONE',  ( 33.21599328327231149, 465.5375697722676591, 9.463303254740063508 ) ) ;
#87089 = CARTESIAN_POINT ( 'NONE',  ( -15.68557340203132533, 21.69024387811347054, 4.767881275868345980 ) ) ;
#87090 = DIRECTION ( 'NONE',  ( 1.000000000000000000, 0.000000000000000000, 0.000000000000000000 ) ) ;
#87091 = CARTESIAN_POINT ( 'NONE',  ( -50.30040434326485155, -60.00000000000000711, 72.55815636389731083 ) ) ;
#87092 = TOROIDAL_SURFACE ( 'NONE', #61221, 12.00000000000000711, 3.000000000000000000 ) ;
#87093 = AXIS2_PLACEMENT_3D ( 'NONE', #77014, #34998, #25866 ) ;
#87094 = DIRECTION ( 'NONE',  ( -1.000000000000000000, 0.000000000000000000, 0.000000000000000000 ) ) ;
#87095 = CARTESIAN_POINT ( 'NONE',  ( -28.00203968317432057, 50.00000000000000000, 56.72941417029706201 ) ) ;
#87096 = TOROIDAL_SURFACE ( 'NONE', #54328, 61.00000000000000000, 0.5000000000000000000 ) ;
#87097 = CARTESIAN_POINT ( 'NONE',  ( -85.94079226153354512, -35.60111559732363418, 185.2110495663119991 ) ) ;
#87098 = EDGE_LOOP ( 'NONE', ( #58482, #29624, #42904, #24825, #56689, #2620, #39081, #72037, #18170, #55491 ) ) ;
#87099 = CARTESIAN_POINT ( 'NONE',  ( 32.17347608656518787, 319.0370483936366668, -5.555387326066758114 ) ) ;
#87100 = CARTESIAN_POINT ( 'NONE',  ( 0.000000000000000000, 6.123233995736767268E-16, -5.000000000000000888 ) ) ;
#87101 = CONICAL_SURFACE ( 'NONE', #49189, 4.000000000000007105, 0.9599310885968835860 ) ;
#87102 = CARTESIAN_POINT ( 'NONE',  ( -6.846707577100250575, 41.84866040025745093, -59.70429183036502252 ) ) ;
#87103 = CARTESIAN_POINT ( 'NONE',  ( 35.97836163550933009, 491.7764920885226161, 12.54497382757449131 ) ) ;
#87104 = CARTESIAN_POINT ( 'NONE',  ( 10.50000000000000711, -5.000000000000000000, -77.33514508527181874 ) ) ;
#87105 = EDGE_CURVE ( 'NONE', #49899, #6924, #24879, .T. ) ;
#87106 = PRESENTATION_STYLE_ASSIGNMENT (( #45583 ) ) ;
#87107 = CARTESIAN_POINT ( 'NONE',  ( -84.30038697636420864, -52.73262689129283842, -14.69966796222219862 ) ) ;
#87108 = DIRECTION ( 'NONE',  ( 0.000000000000000000, -1.000000000000000000, 0.000000000000000000 ) ) ;
#87109 = DIRECTION ( 'NONE',  ( -0.7142857142857134134, 0.6998542122237662033, 0.000000000000000000 ) ) ;
#87110 = VERTEX_POINT ( 'NONE', #13786 ) ;
#87111 = CARTESIAN_POINT ( 'NONE',  ( 32.93513049338658760, 465.6726574193327792, 10.66039033145146142 ) ) ;
#87112 = ADVANCED_FACE ( 'NONE', ( #46698 ), #94171, .F. ) ;
#87113 = DIRECTION ( 'NONE',  ( 0.000000000000000000, 0.000000000000000000, 1.000000000000000000 ) ) ;
#87114 = EDGE_CURVE ( 'NONE', #1378, #46291, #59059, .T. ) ;
#87115 = CARTESIAN_POINT ( 'NONE',  ( 85.55833380596646975, -30.00000000000001776, -20.40969086358413520 ) ) ;
#87116 = CARTESIAN_POINT ( 'NONE',  ( -81.01834315243938534, -18.68267671355141601, 131.0834654034409823 ) ) ;
#87117 = ORIENTED_EDGE ( 'NONE', *, *, #52326, .T. ) ;
#87118 = LINE ( 'NONE', #61248, #1593 ) ;
#87119 = CARTESIAN_POINT ( 'NONE',  ( -5.500000000000007994, 42.00000000000000000, -68.91429205818155879 ) ) ;
#87120 = CARTESIAN_POINT ( 'NONE',  ( 62.69693952681404170, -57.67812735391505896, 116.6625076095181726 ) ) ;
#87121 = CARTESIAN_POINT ( 'NONE',  ( 45.43595897156877328, 50.00000000000001421, 43.65914459177244566 ) ) ;
#87122 = CARTESIAN_POINT ( 'NONE',  ( 42.59298759914230459, 320.2223789555831104, -3.850798572401481934 ) ) ;
#87123 = CYLINDRICAL_SURFACE ( 'NONE', #73526, 65.00000000000000000 ) ;
#87124 = VERTEX_POINT ( 'NONE', #41788 ) ;
#87125 = CARTESIAN_POINT ( 'NONE',  ( 4.522409606147229866, 53.69437142520751394, -8.280415083304497159 ) ) ;
#87126 = CARTESIAN_POINT ( 'NONE',  ( 31.81284829423740135, 439.0025894409650959, 23.54372111369165310 ) ) ;
#87127 = CARTESIAN_POINT ( 'NONE',  ( -15.97269242673987932, 37.21081289561242755, 22.07591361862206014 ) ) ;
#87128 = CARTESIAN_POINT ( 'NONE',  ( 2.977408999572650927, -24.87500000204838457, -7.188101187500001821 ) ) ;
#87129 = EDGE_CURVE ( 'NONE', #98079, #36198, #74670, .T. ) ;
#87130 = VERTEX_POINT ( 'NONE', #75748 ) ;
#87131 = CARTESIAN_POINT ( 'NONE',  ( 3.313708498984761608, -19.90625000409677270, -8.000000000000000000 ) ) ;
#87132 = AXIS2_PLACEMENT_3D ( 'NONE', #82544, #43677, #1603 ) ;
#87133 = DIRECTION ( 'NONE',  ( -1.000000000000000000, -1.224606353822377258E-16, -0.000000000000000000 ) ) ;
#87134 = CARTESIAN_POINT ( 'NONE',  ( -44.35014475220779673, 435.2396861789843001, 12.17836948353843596 ) ) ;
#87135 = CARTESIAN_POINT ( 'NONE',  ( 26.94607068127204386, 36.65998315651609829, 10.05698433968586691 ) ) ;
#87136 = CARTESIAN_POINT ( 'NONE',  ( 12.50000000000000178, -3.000000000000001332, -35.13068384735336736 ) ) ;
#87137 = CARTESIAN_POINT ( 'NONE',  ( 6.962331184707186918E-15, 44.84115912518001323, -56.85174851683467523 ) ) ;
#87138 = ORIENTED_EDGE ( 'NONE', *, *, #72474, .F. ) ;
#87139 = CARTESIAN_POINT ( 'NONE',  ( 92.68765510100411120, -60.00000000000002132, -9.247194546651380520 ) ) ;
#87141 = CARTESIAN_POINT ( 'NONE',  ( 26.45493447348655991, -18.61830836965839353, 28.46775629927182294 ) ) ;
#87140 = CARTESIAN_POINT ( 'NONE',  ( -69.85357985695409866, -59.99999999999993605, 155.8687211249902873 ) ) ;
#87142 = CARTESIAN_POINT ( 'NONE',  ( 33.83237027343565018, 58.72416816948007323, -16.91618513671781798 ) ) ;
#87143 = ORIENTED_EDGE ( 'NONE', *, *, #70530, .T. ) ;
#87144 = UNCERTAINTY_MEASURE_WITH_UNIT (LENGTH_MEASURE( 1.000000000000000082E-05 ), #36460, 'distance_accuracy_value', 'NONE');
#87145 = ORIENTED_EDGE ( 'NONE', *, *, #18934, .F. ) ;
#87146 = CARTESIAN_POINT ( 'NONE',  ( 34.14532928921329358, 464.2269668280595738, 6.057797726091872725 ) ) ;
#87147 = CARTESIAN_POINT ( 'NONE',  ( -5.802268690544502228, -46.54360925828362383, 103.8899761878886636 ) ) ;
#87148 = DIRECTION ( 'NONE',  ( 0.000000000000000000, 0.000000000000000000, -1.000000000000000000 ) ) ;
#87149 = DIRECTION ( 'NONE',  ( 0.000000000000000000, -0.8568390274594179790, -0.5155840193628955515 ) ) ;
#87150 = CARTESIAN_POINT ( 'NONE',  ( 0.000000000000000000, 4.000000000000000000, 0.000000000000000000 ) ) ;
#87151 = ORIENTED_EDGE ( 'NONE', *, *, #61779, .F. ) ;
#87152 = CARTESIAN_POINT ( 'NONE',  ( 17.50000000000002132, 44.85000000000000853, 64.09953197957062798 ) ) ;
#87153 = VECTOR ( 'NONE', #56956, 1000.000000000000000 ) ;
#87154 = DIRECTION ( 'NONE',  ( -1.000000000000000000, -1.224606353822377258E-16, -0.000000000000000000 ) ) ;
#87155 = CARTESIAN_POINT ( 'NONE',  ( -10.72008664263877620, 18.40195438196344568, -9.341170610878782199 ) ) ;
#87156 = CARTESIAN_POINT ( 'NONE',  ( 0.000000000000000000, 14.17434517210798184, -56.74723269274520021 ) ) ;
#87157 = CARTESIAN_POINT ( 'NONE',  ( 81.21951335026766117, -29.99999999999999645, -11.15224753138006264 ) ) ;
#87158 = DIRECTION ( 'NONE',  ( 0.000000000000000000, 0.000000000000000000, -1.000000000000000000 ) ) ;
#87159 = ORIENTED_EDGE ( 'NONE', *, *, #76070, .T. ) ;
#87160 = EDGE_LOOP ( 'NONE', ( #22133, #27037, #11526, #80565, #21013 ) ) ;
#87161 = VERTEX_POINT ( 'NONE', #99478 ) ;
#87162 = CARTESIAN_POINT ( 'NONE',  ( -2.352990130084491319E-16, 8.660254037844390851, -7.422398894150036064 ) ) ;
#87163 = DIRECTION ( 'NONE',  ( 1.000000000000000000, 0.000000000000000000, 0.000000000000000000 ) ) ;
#87164 = DIRECTION ( 'NONE',  ( 1.000000000000000000, 0.000000000000000000, -0.000000000000000000 ) ) ;
#87165 = CARTESIAN_POINT ( 'NONE',  ( -37.61995194924682551, 438.1737809428368564, 4.432418093030975115 ) ) ;
#87166 = DIRECTION ( 'NONE',  ( -0.000000000000000000, 1.000000000000000000, -0.000000000000000000 ) ) ;
#87167 = CARTESIAN_POINT ( 'NONE',  ( -6.928203230275508773, -85.26930929695541295, -4.000000000000001776 ) ) ;
#87168 = CARTESIAN_POINT ( 'NONE',  ( 6.326592304916277776, -5.253140224433049177, 4.564380808752273921 ) ) ;
#87169 = ORIENTED_EDGE ( 'NONE', *, *, #7530, .T. ) ;
#87171 = EDGE_CURVE ( 'NONE', #84621, #95530, #40409, .T. ) ;
#87170 = CARTESIAN_POINT ( 'NONE',  ( 42.72731753109084707, 485.8496451746399316, 7.279150061871429322 ) ) ;
#87172 = ORIENTED_EDGE ( 'NONE', *, *, #10896, .T. ) ;
#87173 = CARTESIAN_POINT ( 'NONE',  ( -4.696906829037967412, -63.56001852512106609, -3.734050370377311356 ) ) ;
#87174 = FACE_OUTER_BOUND ( 'NONE', #9647, .T. ) ;
#87175 = CARTESIAN_POINT ( 'NONE',  ( -39.80120353649695630, 485.6913716985619658, -4.529092486723600430 ) ) ;
#87176 = PRESENTATION_LAYER_ASSIGNMENT (  '', '', ( #19985 ) ) ;
#87177 = AXIS2_PLACEMENT_3D ( 'NONE', #93518, #95632, #21770 ) ;
#87178 = CIRCLE ( 'NONE', #63062, 5.000000000000000888 ) ;
#87179 = CARTESIAN_POINT ( 'NONE',  ( 5.644640995548282802, 301.6279895259619366, -10.01771135672319879 ) ) ;
#87180 = CARTESIAN_POINT ( 'NONE',  ( 63.94774550461288243, -18.62871603261821818, 72.61133700325008533 ) ) ;
#87181 = EDGE_LOOP ( 'NONE', ( #56054, #57924 ) ) ;
#87182 = CARTESIAN_POINT ( 'NONE',  ( 41.14212900119734684, 464.2935350810450359, 17.75680570235805078 ) ) ;
#87183 = AXIS2_PLACEMENT_3D ( 'NONE', #43162, #35639, #83084 ) ;
#87184 = CARTESIAN_POINT ( 'NONE',  ( -46.34826540902298575, -34.70201877029627724, -36.70216098910028535 ) ) ;
#87185 = CARTESIAN_POINT ( 'NONE',  ( -6.561040333616081632, 9.827807988210597756, -2.450206053579249144 ) ) ;
#87186 = EDGE_CURVE ( 'NONE', #99203, #68693, #59369, .T. ) ;
#87187 = CARTESIAN_POINT ( 'NONE',  ( -8.876313894634513701, 51.71968240765218638, 1.561724931196740274 ) ) ;
#87188 = ORIENTED_EDGE ( 'NONE', *, *, #100533, .F. ) ;
#87189 = CARTESIAN_POINT ( 'NONE',  ( 0.000000000000000000, 1.502314598737161398E-15, 6.499999999999999112 ) ) ;
#87190 = CARTESIAN_POINT ( 'NONE',  ( 92.53532739719321398, -2.002967142162725287E-29, 5.000000000000011546 ) ) ;
#87191 = AXIS2_PLACEMENT_3D ( 'NONE', #64105, #46831, #13920 ) ;
#87192 = FACE_OUTER_BOUND ( 'NONE', #97548, .T. ) ;
#87193 = CARTESIAN_POINT ( 'NONE',  ( 3.400000000000000355, 0.000000000000000000, -8.000000000000000000 ) ) ;
#87194 = FACE_OUTER_BOUND ( 'NONE', #106569, .T. ) ;
#87195 = CARTESIAN_POINT ( 'NONE',  ( 86.96496777674417444, -31.71578965763157498, 187.3089302373552982 ) ) ;
#87196 = EDGE_CURVE ( 'NONE', #76623, #26294, #32123, .T. ) ;
#87197 = CARTESIAN_POINT ( 'NONE',  ( -5.105409892807596606, -2.846581877981202879, -18.47267145302658164 ) ) ;
#87198 = ADVANCED_FACE ( 'NONE', ( #1300 ), #15922, .T. ) ;
#87199 = B_SPLINE_CURVE_WITH_KNOTS ( 'NONE', 3,
 ( #20851, #47172, #94704, #45086, #70934, #88187, #37011, #86618 ),
 .UNSPECIFIED., .F., .F.,
 ( 4, 2, 2, 4 ),
 ( 0.004673709593152156581, 0.005837709341827645136, 0.007001709090503132824, 0.009329708587854111668 ),
 .UNSPECIFIED. ) ;
#87200 = CARTESIAN_POINT ( 'NONE',  ( -3.763170808999132255, 19.48428572230863409, 5.000000000000000888 ) ) ;
#87201 = PLANE ( 'NONE',  #30991 ) ;
#87202 = CARTESIAN_POINT ( 'NONE',  ( 53.23435742203598409, -28.20034973435990011, -27.12572715517088184 ) ) ;
#87203 = CARTESIAN_POINT ( 'NONE',  ( -43.00000000000000711, 485.2629658518202973, -2.796394914059372905 ) ) ;
#87204 = CARTESIAN_POINT ( 'NONE',  ( 5.947762761376476526, 2.501851166488377576, 6.500000000000000000 ) ) ;
#87205 = CARTESIAN_POINT ( 'NONE',  ( 33.52756498066074187, 435.4194806154983439, 9.514010192928232357 ) ) ;
#87206 = CIRCLE ( 'NONE', #20105, 3.309500000000007880 ) ;
#87207 = CARTESIAN_POINT ( 'NONE',  ( -100.7566295605840594, -29.99999999999999645, 180.7218492552073599 ) ) ;
#87208 = CARTESIAN_POINT ( 'NONE',  ( 0.5805565836007643421, -3.752776749732575468, -6.499999999999999112 ) ) ;
#87209 = CARTESIAN_POINT ( 'NONE',  ( 19.28957066462841752, -57.67183861258752131, 42.12264632805888454 ) ) ;
#87210 = CARTESIAN_POINT ( 'NONE',  ( 1.380949872273418549E-15, 50.89575828009192549, 11.27631144943088692 ) ) ;
#87211 = CARTESIAN_POINT ( 'NONE',  ( -52.56483885390523625, 40.83906611473335602, -38.23529411764705088 ) ) ;
#87212 = CARTESIAN_POINT ( 'NONE',  ( -17.96390936993321930, 50.00000000000000000, 61.93590888982013354 ) ) ;
#87213 = CARTESIAN_POINT ( 'NONE',  ( -0.1687174074039889671, 44.08548369317415450, 16.24999999999993250 ) ) ;
#87214 = CARTESIAN_POINT ( 'NONE',  ( 3.505862197715610140, -0.8815186120392470848, 103.6125913840232329 ) ) ;
#87215 = CYLINDRICAL_SURFACE ( 'NONE', #8822, 8.000000000000000000 ) ;
#87216 = PLANE ( 'NONE',  #63084 ) ;
#87217 = AXIS2_PLACEMENT_3D ( 'NONE', #90410, #84306, #17060 ) ;
#87218 = FACE_OUTER_BOUND ( 'NONE', #87289, .T. ) ;
#87219 = ORIENTED_EDGE ( 'NONE', *, *, #33675, .F. ) ;
#87220 = CARTESIAN_POINT ( 'NONE',  ( 41.97131279570576368, 485.5606288621858653, -4.070573943143920737 ) ) ;
#87221 = CARTESIAN_POINT ( 'NONE',  ( 40.31754836868392289, 437.2079761516864664, 22.20092987877936608 ) ) ;
#87222 = CARTESIAN_POINT ( 'NONE',  ( -13.37379485725665162, -32.51307406780899356, 29.38708954896887704 ) ) ;
#87224 = CARTESIAN_POINT ( 'NONE',  ( -40.92146453211002921, 438.1322861037302800, 22.38370651923338173 ) ) ;
#87223 = CARTESIAN_POINT ( 'NONE',  ( -90.88575953229592130, -59.99999999999998579, 60.76790198270563792 ) ) ;
#87225 = ORIENTED_EDGE ( 'NONE', *, *, #38007, .T. ) ;
#87226 = CARTESIAN_POINT ( 'NONE',  ( -43.69780420584740455, 464.4352583045362621, 7.050850226778779373 ) ) ;
#87227 = CARTESIAN_POINT ( 'NONE',  ( 15.79261075262967573, 4.810720122702399237, -5.431533035175681867 ) ) ;
#87228 = CARTESIAN_POINT ( 'NONE',  ( 43.03987588564152844, 486.0760633267547632, 5.817066388976027902 ) ) ;
#87229 = CONICAL_SURFACE ( 'NONE', #56395, 6.499999999999999112, 1.047197551196600296 ) ;
#87230 = FACE_OUTER_BOUND ( 'NONE', #8238, .T. ) ;
#87231 = CIRCLE ( 'NONE', #32124, 5.000000000000001776 ) ;
#87232 = CARTESIAN_POINT ( 'NONE',  ( -0.1682904726799566431, 53.39766064372320642, -10.24999999999999822 ) ) ;
#87233 = ORIENTED_EDGE ( 'NONE', *, *, #26824, .T. ) ;
#87234 = CARTESIAN_POINT ( 'NONE',  ( -5.290067270632269114, -1.200000000000000030E-05, -7.281152949374520844 ) ) ;
#87235 = DIRECTION ( 'NONE',  ( -0.000000000000000000, -1.000000000000000000, -0.000000000000000000 ) ) ;
#87236 = CONICAL_SURFACE ( 'NONE', #20137, 5.000000000000001776, 0.9599310885968803664 ) ;
#87237 = MECHANICAL_DESIGN_GEOMETRIC_PRESENTATION_REPRESENTATION (  '', ( #78591 ), #54482 ) ;
#87239 = CARTESIAN_POINT ( 'NONE',  ( 0.000000000000000000, 0.000000000000000000, 0.000000000000000000 ) ) ;
#87238 = CARTESIAN_POINT ( 'NONE',  ( 36.20918625285742110, -33.55288256454751661, 34.82669593431387511 ) ) ;
#87240 = CARTESIAN_POINT ( 'NONE',  ( -10.50000000000000178, -5.000000000000000000, -34.12705335493774328 ) ) ;
#87241 = VERTEX_POINT ( 'NONE', #101631 ) ;
#87242 = AXIS2_PLACEMENT_3D ( 'NONE', #1787, #36869, #103167 ) ;
#87243 = ORIENTED_EDGE ( 'NONE', *, *, #14201, .T. ) ;
#87245 = CIRCLE ( 'NONE', #61469, 3.309500000000001663 ) ;
#87244 = CARTESIAN_POINT ( 'NONE',  ( -28.07965516020418306, 315.5842071114037708, 11.56093435300535965 ) ) ;
#87246 = EDGE_CURVE ( 'NONE', #51147, #55118, #104080, .T. ) ;
#87247 = EDGE_LOOP ( 'NONE', ( #41491, #106295, #38618, #29603, #49327, #105463 ) ) ;
#87248 = CARTESIAN_POINT ( 'NONE',  ( 21.43726646001635672, 305.0999692234804002, 8.990123627463036726 ) ) ;
#87249 = ADVANCED_FACE ( 'NONE', ( #76276 ), #4241, .T. ) ;
#87250 = CARTESIAN_POINT ( 'NONE',  ( 61.11682663846713837, 6.975173280561618775E-15, 0.000000000000000000 ) ) ;
#87251 = FILL_AREA_STYLE ('',( #53281 ) ) ;
#87252 = EDGE_LOOP ( 'NONE', ( #12918, #89187, #80076, #101502 ) ) ;
#87253 = DIRECTION ( 'NONE',  ( 0.000000000000000000, -1.000000000000000000, 0.000000000000000000 ) ) ;
#87254 = CARTESIAN_POINT ( 'NONE',  ( -6.075687308901098760, 41.99394926078448265, -68.91429205814512216 ) ) ;
#87255 = CARTESIAN_POINT ( 'NONE',  ( -112.8557562759809798, -60.00000000003905853, 147.0001122092953381 ) ) ;
#87256 = DIRECTION ( 'NONE',  ( 0.5735764363510468256, 0.8191520442889913545, 0.000000000000000000 ) ) ;
#87257 = CONICAL_SURFACE ( 'NONE', #32140, 3.309500000000001663, 0.9599310885968770357 ) ;
#87258 = CARTESIAN_POINT ( 'NONE',  ( 26.81477069726286544, -60.00000000000001421, 41.67871456507009498 ) ) ;
#87259 = DIRECTION ( 'NONE',  ( 0.000000000000000000, 0.000000000000000000, -1.000000000000000000 ) ) ;
#87260 = CARTESIAN_POINT ( 'NONE',  ( -5.897540648542782371, 41.82858959817294675, -58.91931066433214426 ) ) ;
#87262 = CARTESIAN_POINT ( 'NONE',  ( 11.48827963599770285, -53.39680579818115547, 32.81982166506503518 ) ) ;
#87261 = CARTESIAN_POINT ( 'NONE',  ( -95.66383100604464573, -60.00000000000002132, 35.18327952992021324 ) ) ;
#87263 = CARTESIAN_POINT ( 'NONE',  ( -48.90657022356846539, -46.44393484032057984, 51.21248264059143196 ) ) ;
#87264 = DIRECTION ( 'NONE',  ( 0.000000000000000000, -1.000000000000000000, 0.000000000000000000 ) ) ;
#87265 = ORIENTED_EDGE ( 'NONE', *, *, #51061, .F. ) ;
#87266 = CARTESIAN_POINT ( 'NONE',  ( 1.235451739553820927, 10.14988630190398311, -50.72637377003573533 ) ) ;
#87267 = DIRECTION ( 'NONE',  ( 1.000000000000000000, 0.000000000000000000, 0.000000000000000000 ) ) ;
#87268 = FILL_AREA_STYLE ('',( #15487 ) ) ;
#87270 = VERTEX_POINT ( 'NONE', #2384 ) ;
#87269 = AXIS2_PLACEMENT_3D ( 'NONE', #82851, #66134, #33794 ) ;
#87271 = CARTESIAN_POINT ( 'NONE',  ( -11.87389578517861288, -10.58298652339508372, 10.63284064146614405 ) ) ;
#87272 = ORIENTED_EDGE ( 'NONE', *, *, #83070, .T. ) ;
#87273 = CARTESIAN_POINT ( 'NONE',  ( 89.30885607944193794, -29.99999999992603250, 7.018915378132053462 ) ) ;
#87274 = DIRECTION ( 'NONE',  ( 1.000000000000000000, 1.224606353822377258E-16, 0.000000000000000000 ) ) ;
#87275 = DIRECTION ( 'NONE',  ( 0.000000000000000000, 0.000000000000000000, -1.000000000000000000 ) ) ;
#87276 = AXIS2_PLACEMENT_3D ( 'NONE', #66411, #32487, #98249 ) ;
#87277 = CARTESIAN_POINT ( 'NONE',  ( 29.83308852626540641, 42.00000000008230927, -51.76085035116526711 ) ) ;
#87278 = CARTESIAN_POINT ( 'NONE',  ( 96.30119089153456002, -30.00000000000000000, 191.2506517886558299 ) ) ;
#87279 = DIRECTION ( 'NONE',  ( 0.000000000000000000, 0.000000000000000000, 1.000000000000000000 ) ) ;
#87280 = ORIENTED_EDGE ( 'NONE', *, *, #84813, .T. ) ;
#87281 = VERTEX_POINT ( 'NONE', #34801 ) ;
#87282 = VERTEX_POINT ( 'NONE', #19162 ) ;
#87283 = CARTESIAN_POINT ( 'NONE',  ( 9.797174393178825657E-16, -0.5000000000000000000, -8.000000000000000000 ) ) ;
#87284 = CARTESIAN_POINT ( 'NONE',  ( 43.51517875624352172, 462.0595338174632047, 4.327785711310748518 ) ) ;
#87285 = DIRECTION ( 'NONE',  ( 0.000000000000000000, 1.000000000000000000, 0.000000000000000000 ) ) ;
#87286 = EDGE_LOOP ( 'NONE', ( #2872, #100545, #15618, #54448, #6734 ) ) ;
#87288 = EDGE_CURVE ( 'NONE', #50075, #88346, #94064, .T. ) ;
#87287 = CARTESIAN_POINT ( 'NONE',  ( 64.29999999999999716, -3.309500000000000774, 0.000000000000000000 ) ) ;
#87289 = EDGE_LOOP ( 'NONE', ( #11544, #27497, #71983, #36903 ) ) ;
#87290 = CARTESIAN_POINT ( 'NONE',  ( 101.5729318683832361, -38.45079819966511536, 199.8890759196411011 ) ) ;
#87291 = CARTESIAN_POINT ( 'NONE',  ( 11.42362078197221997, 14.22850026525571110, 9.928456956968465974 ) ) ;
#87292 = CARTESIAN_POINT ( 'NONE',  ( 84.90889233706131733, -52.71069020251738380, 13.63360479297925032 ) ) ;
#87293 = CARTESIAN_POINT ( 'NONE',  ( 93.97977184163765685, 1.030564683017419500E-14, 0.000000000000000000 ) ) ;
#87294 = LINE ( 'NONE', #69518, #13699 ) ;
#87295 = CARTESIAN_POINT ( 'NONE',  ( -43.03894652950386757, 464.9992092536282939, 11.55502599540882791 ) ) ;
#87296 =( REPRESENTATION_RELATIONSHIP ('NONE','NONE', #69581, #77771 ) REPRESENTATION_RELATIONSHIP_WITH_TRANSFORMATION ( #52971 )SHAPE_REPRESENTATION_RELATIONSHIP( ) );
#87297 = CARTESIAN_POINT ( 'NONE',  ( 32.62207953394533178, 1.482358050883964840E-15, 0.000000000000000000 ) ) ;
#87298 = AXIS2_PLACEMENT_3D ( 'NONE', #44459, #25655, #34803 ) ;
#87299 = DIRECTION ( 'NONE',  ( -1.000000000000000000, -1.224606353822377258E-16, -0.000000000000000000 ) ) ;
#87300 = EDGE_LOOP ( 'NONE', ( #84347, #74786, #78690, #55692, #76928 ) ) ;
#87301 = EDGE_CURVE ( 'NONE', #35905, #37591, #7677, .T. ) ;
#87302 = CARTESIAN_POINT ( 'NONE',  ( 4.898587196589412829E-16, -19.81250000409677270, -8.000000000000000000 ) ) ;
#87303 = DIRECTION ( 'NONE',  ( -1.000000000000000000, -1.224606353822377258E-16, -0.000000000000000000 ) ) ;
#87304 = CARTESIAN_POINT ( 'NONE',  ( -26.48391857604995892, 37.08887766516708950, 7.710198647837219532 ) ) ;
#87305 = ORIENTED_EDGE ( 'NONE', *, *, #103537, .T. ) ;
#87306 = CARTESIAN_POINT ( 'NONE',  ( -6.891666673413887896E-15, -70.53271932724189242, 13.00000000000000000 ) ) ;
#87307 = CARTESIAN_POINT ( 'NONE',  ( -25.77050100732808602, 305.3127693512194583, 10.48956834842311459 ) ) ;
#87308 = CARTESIAN_POINT ( 'NONE',  ( -12.23812927463290023, -4.553267922722016081, -76.78892216552449668 ) ) ;
#87309 = FACE_OUTER_BOUND ( 'NONE', #35447, .T. ) ;
#87310 = CARTESIAN_POINT ( 'NONE',  ( -1.469576158976823947E-15, -21.87499999999999289, 8.000000000000000000 ) ) ;
#87311 = VECTOR ( 'NONE', #97665, 1000.000000000000000 ) ;
#87313 = CARTESIAN_POINT ( 'NONE',  ( -22.77004263405657625, -20.97328029508773639, 36.31169601591036411 ) ) ;
#87312 = AXIS2_PLACEMENT_3D ( 'NONE', #2975, #35932, #1362 ) ;
#87314 =( GEOMETRIC_REPRESENTATION_CONTEXT ( 3 ) GLOBAL_UNCERTAINTY_ASSIGNED_CONTEXT ( ( #51563 ) ) GLOBAL_UNIT_ASSIGNED_CONTEXT ( ( #92316, #42715, #100416 ) ) REPRESENTATION_CONTEXT ( 'NONE', 'WORKASPACE' ) );
#87315 = COLOUR_RGB ( '', 0.09019608, 0.27058824, 0.51372549) ;
#87316 = CARTESIAN_POINT ( 'NONE',  ( 16.64348903516512834, -1.200000000000000030E-05, -4.157797401561768247 ) ) ;
#87317 = ORIENTED_EDGE ( 'NONE', *, *, #9871, .F. ) ;
#87318 = CARTESIAN_POINT ( 'NONE',  ( 83.21382037009784938, -57.31687954804421281, 189.0388902036028185 ) ) ;
#87319 = CARTESIAN_POINT ( 'NONE',  ( -48.49490330227218493, 10.48921555948077611, 14.43974515805995829 ) ) ;
#87320 = ADVANCED_FACE ( 'NONE', ( #2911 ), #67977, .T. ) ;
#87321 = CARTESIAN_POINT ( 'NONE',  ( 7.929588024479113465E-15, 50.00000000000000000, -64.50000000000000000 ) ) ;
#87322 = VERTEX_POINT ( 'NONE', #36409 ) ;
#87323 = CARTESIAN_POINT ( 'NONE',  ( 94.40785360964090955, -57.67103502906764589, -0.2615027077762412944 ) ) ;
#87324 = AXIS2_PLACEMENT_3D ( 'NONE', #25175, #56961, #64552 ) ;
#87325 = DIRECTION ( 'NONE',  ( 0.000000000000000000, -1.000000000000000000, 0.000000000000000000 ) ) ;
#87326 = CARTESIAN_POINT ( 'NONE',  ( -9.937561876414743978, -5.000000000000002665, -76.56466736914423166 ) ) ;
#87327 = CARTESIAN_POINT ( 'NONE',  ( -30.23165830866663129, 7.786015354292214141, 41.98067155130487293 ) ) ;
#87328 = AXIS2_PLACEMENT_3D ( 'NONE', #34180, #17978, #11448 ) ;
#87329 = DIRECTION ( 'NONE',  ( 0.000000000000000000, 0.000000000000000000, 1.000000000000000000 ) ) ;
#87330 = ADVANCED_FACE ( 'NONE', ( #19694 ), #1844, .F. ) ;
#87331 = VERTEX_POINT ( 'NONE', #43191 ) ;
#87332 = DIRECTION ( 'NONE',  ( 0.9987673911192530563, 4.332722927543991053E-22, -0.04963565690953686271 ) ) ;
#87333 = CARTESIAN_POINT ( 'NONE',  ( 9.408375277128495640, -19.97193506209725200, 35.33198514726674944 ) ) ;
#87334 = CARTESIAN_POINT ( 'NONE',  ( 2.122576366386045521, -0.2161414388924163821, 102.5552564100479032 ) ) ;
#87335 = CARTESIAN_POINT ( 'NONE',  ( 51.47742418153980282, -29.90942068293205480, 49.13780789315548247 ) ) ;
#87337 = CARTESIAN_POINT ( 'NONE',  ( -11.46727569567480387, 9.426839320540786105, 9.363982917197334999 ) ) ;
#87336 = DIRECTION ( 'NONE',  ( 0.000000000000000000, 0.000000000000000000, 1.000000000000000000 ) ) ;
#87338 = CARTESIAN_POINT ( 'NONE',  ( 33.09999999999999432, 3.309500000000003439, 0.000000000000000000 ) ) ;
#87339 = CARTESIAN_POINT ( 'NONE',  ( -15.39222209860203883, 44.06956899279646933, -5.345204092738742752 ) ) ;
#87340 = ADVANCED_FACE ( 'NONE', ( #99823 ), #19761, .T. ) ;
#87341 = CARTESIAN_POINT ( 'NONE',  ( 34.24477232042282537, 301.4776311158785802, -0.5002871126718249073 ) ) ;
#87342 = FACE_OUTER_BOUND ( 'NONE', #29999, .T. ) ;
#87343 = CARTESIAN_POINT ( 'NONE',  ( -82.55502573126497623, -38.00000000000004263, -12.59846151849247420 ) ) ;
#87344 = AXIS2_PLACEMENT_3D ( 'NONE', #65488, #75691, #7763 ) ;
#87345 = EDGE_CURVE ( 'NONE', #65192, #75037, #65865, .T. ) ;
#87346 = ADVANCED_FACE ( 'NONE', ( #98227 ), #58304, .F. ) ;
#87347 = ORIENTED_EDGE ( 'NONE', *, *, #39623, .T. ) ;
#87348 = CARTESIAN_POINT ( 'NONE',  ( -9.275681565049682220, -2.829365477041055676, 14.74133895328401245 ) ) ;
#87349 = CARTESIAN_POINT ( 'NONE',  ( 0.000000000000000000, -1.200000000000000030E-05, 10.24999999999999822 ) ) ;
#87350 = CIRCLE ( 'NONE', #70174, 5.000000000000010658 ) ;
#87352 = CARTESIAN_POINT ( 'NONE',  ( -7.863041645572806715, -34.58964495997116728, -32.51031543117136380 ) ) ;
#87351 = CARTESIAN_POINT ( 'NONE',  ( 0.000000000000000000, -19.99999999999998934, 0.000000000000000000 ) ) ;
#87353 = ORIENTED_EDGE ( 'NONE', *, *, #70808, .F. ) ;
#87354 = CARTESIAN_POINT ( 'NONE',  ( -0.3483149870578508001, 8.861353789385022495, -7.493854785173812871 ) ) ;
#87355 = CARTESIAN_POINT ( 'NONE',  ( 0.05533025579362559065, -4.993776679985863609, -4.350525068611871049 ) ) ;
#87356 = ORIENTED_EDGE ( 'NONE', *, *, #23428, .F. ) ;
#87357 = CARTESIAN_POINT ( 'NONE',  ( 6.585468679846621320, 3.617797563910810865, 6.733790807807553236 ) ) ;
#87358 = CARTESIAN_POINT ( 'NONE',  ( 73.59428447264397732, 4.898587196589294500E-16, -4.000000000000007105 ) ) ;
#87359 = CARTESIAN_POINT ( 'NONE',  ( -92.61039005374894373, -59.99999999999997868, -10.20672413289644531 ) ) ;
#87360 = ORIENTED_EDGE ( 'NONE', *, *, #35335, .F. ) ;
#87361 = CARTESIAN_POINT ( 'NONE',  ( 8.369914041613107258, 42.00000000000000000, -59.54702718917638293 ) ) ;
#87362 = CARTESIAN_POINT ( 'NONE',  ( -1.469576158976823947E-15, -21.87499999999999289, 8.000000000000000000 ) ) ;
#87363 = CARTESIAN_POINT ( 'NONE',  ( -9.381394091586571449, 27.98650394418389098, 3.465950112474260880 ) ) ;
#87364 = AXIS2_PLACEMENT_3D ( 'NONE', #83724, #69171, #76701 ) ;
#87366 = DIRECTION ( 'NONE',  ( -1.000000000000000000, -0.000000000000000000, -0.000000000000000000 ) ) ;
#87365 = DIRECTION ( 'NONE',  ( -0.3900125511318229821, 0.5465874153434815419, 0.7410346870071464753 ) ) ;
#87367 = CARTESIAN_POINT ( 'NONE',  ( -84.14012639669060434, -29.03968219319695976, 163.8444925067498730 ) ) ;
#87368 = CIRCLE ( 'NONE', #21946, 4.000000000000001776 ) ;
#87369 = ORIENTED_EDGE ( 'NONE', *, *, #95409, .T. ) ;
#87370 = CARTESIAN_POINT ( 'NONE',  ( 6.663127973346358424, 3.846958729056439985, -6.460793508093575888 ) ) ;
#87371 = ORIENTED_EDGE ( 'NONE', *, *, #40103, .T. ) ;
#87372 = ORIENTED_EDGE ( 'NONE', *, *, #66363, .F. ) ;
#87374 =( BOUNDED_SURFACE ( )  B_SPLINE_SURFACE ( 2, 3, ( 
 ( #87152, #19796, #62352, #103845 ),
 ( #86637, #28958, #54750, #37569 ),
 ( #67374, #85564, #77460, #45630 ) ),
 .UNSPECIFIED., .F., .F., .T. ) 
 B_SPLINE_SURFACE_WITH_KNOTS ( ( 3, 3 ),
 ( 4, 4 ),
 ( 0.000000000000000000, 1.000000000000000000 ),
 ( 0.04485000000000000792, 0.04800000000000000100 ),
 .UNSPECIFIED. ) 
 GEOMETRIC_REPRESENTATION_ITEM ( )  RATIONAL_B_SPLINE_SURFACE ( (
 ( 1.000000000000000000, 1.000000000000000000, 1.000000000000000000, 1.000000000000000000),
 ( 1.857142857142858317, 1.857142857142858317, 1.857142857142858317, 1.857142857142858317),
 ( 1.000000000000000000, 1.000000000000000000, 1.000000000000000000, 1.000000000000000000) ) ) 
 REPRESENTATION_ITEM ( '' )  SURFACE ( )  );
#87373 = CARTESIAN_POINT ( 'NONE',  ( 31.35993874404257298, 436.8062917347268694, 22.71845294991138786 ) ) ;
#87375 = EDGE_CURVE ( 'NONE', #9488, #10770, #82144, .T. ) ;
#87376 = CARTESIAN_POINT ( 'NONE',  ( -5.139041025450133304, -67.43305464250801151, 13.97603388998033580 ) ) ;
#87377 = CARTESIAN_POINT ( 'NONE',  ( 0.000000000000000000, -78.00000000000000000, 27.00000000000000000 ) ) ;
#87378 = VERTEX_POINT ( 'NONE', #99272 ) ;
#87379 = DIRECTION ( 'NONE',  ( 0.000000000000000000, 0.000000000000000000, 1.000000000000000000 ) ) ;
#87380 = CARTESIAN_POINT ( 'NONE',  ( -42.19179521602437433, 484.5286692029248456, -4.078961064713001683 ) ) ;
#87381 = CARTESIAN_POINT ( 'NONE',  ( -104.1916751217198822, -57.64030415157957066, 202.2041723927455905 ) ) ;
#87382 = CARTESIAN_POINT ( 'NONE',  ( -5.999511540169428336, -68.99926730885432846, -0.2833228702578380331 ) ) ;
#87383 = CARTESIAN_POINT ( 'NONE',  ( 47.33349330513379982, 4.898587196589405926E-16, -4.000000000000001776 ) ) ;
#87384 = AXIS2_PLACEMENT_3D ( 'NONE', #78704, #37773, #70635 ) ;
#87385 = CARTESIAN_POINT ( 'NONE',  ( -9.989690267985800176, 101.0255558340509197, -0.5238310916885776658 ) ) ;
#87386 = SURFACE_SIDE_STYLE ('',( #3804 ) ) ;
#87387 = AXIS2_PLACEMENT_3D ( 'NONE', #94542, #62184, #12520 ) ;
#87388 = DIRECTION ( 'NONE',  ( 9.251858538543049530E-15, 0.9349068334195396179, -0.3548932414479730180 ) ) ;
#87389 = EDGE_CURVE ( 'NONE', #90523, #36223, #83451, .T. ) ;
#87390 = CARTESIAN_POINT ( 'NONE',  ( 76.02438791174152755, -14.21045842199433729, -24.18563911012876844 ) ) ;
#87391 = CARTESIAN_POINT ( 'NONE',  ( -68.99627713242672655, -30.00000000000000355, 123.4899896973233808 ) ) ;
#87392 = CARTESIAN_POINT ( 'NONE',  ( -54.78113597286795056, -29.09368185507433324, 55.71807950450840252 ) ) ;
#87393 = ORIENTED_EDGE ( 'NONE', *, *, #16250, .T. ) ;
#87394 = DIRECTION ( 'NONE',  ( -0.000000000000000000, 1.000000000000000000, 0.000000000000000000 ) ) ;
#87395 = AXIS2_PLACEMENT_3D ( 'NONE', #31862, #56080, #31349 ) ;
#87397 = ORIENTED_EDGE ( 'NONE', *, *, #1716, .F. ) ;
#87396 = AXIS2_PLACEMENT_3D ( 'NONE', #88795, #56394, #105504 ) ;
#87398 = AXIS2_PLACEMENT_3D ( 'NONE', #72867, #53653, #70904 ) ;
#87399 = CARTESIAN_POINT ( 'NONE',  ( -100.5507501323638735, -45.26067218560441319, 191.9851517464235542 ) ) ;
#87400 = CARTESIAN_POINT ( 'NONE',  ( -0.6457514547323006671, 51.32291280783120158, 10.08327392035491599 ) ) ;
#87401 = ORIENTED_EDGE ( 'NONE', *, *, #6401, .T. ) ;
#87402 = CARTESIAN_POINT ( 'NONE',  ( 18.91781669292794987, 48.00000000000000000, 62.18610382930901892 ) ) ;
#87403 = CARTESIAN_POINT ( 'NONE',  ( 17.23461538461538467, 4.172000000000003261, 0.000000000000000000 ) ) ;
#87404 = CARTESIAN_POINT ( 'NONE',  ( -4.667584529657848869, -65.20519645549873644, 13.09134375087143809 ) ) ;
#87405 = COLOUR_RGB ( '', 0.72549020, 0.75294118, 0.79215686) ;
#87407 = CARTESIAN_POINT ( 'NONE',  ( 32.85155332502863956, 463.8111683108725174, 7.359358840565810134 ) ) ;
#87406 = UNCERTAINTY_MEASURE_WITH_UNIT (LENGTH_MEASURE( 1.000000000000000082E-05 ), #16586, 'distance_accuracy_value', 'NONE');
#87408 = AXIS2_PLACEMENT_3D ( 'NONE', #5796, #95887, #53301 ) ;
#87409 = CARTESIAN_POINT ( 'NONE',  ( -8.421452989284619051, 123.3367927118327714, -8.987673073807111741E-31 ) ) ;
#87410 = CARTESIAN_POINT ( 'NONE',  ( -0.6420036228809623546, 34.23282312928377991, 29.57568823882862219 ) ) ;
#87411 = EDGE_CURVE ( 'NONE', #36600, #47158, #68056, .T. ) ;
#87412 = FACE_OUTER_BOUND ( 'NONE', #25921, .T. ) ;
#87413 = CARTESIAN_POINT ( 'NONE',  ( -28.68834382076860479, -29.06026199098176832, 30.85835075655344895 ) ) ;
#87414 = EDGE_LOOP ( 'NONE', ( #49143, #46830, #69264, #59384, #24974, #7416 ) ) ;
#87415 = VERTEX_POINT ( 'NONE', #83632 ) ;
#87416 = CARTESIAN_POINT ( 'NONE',  ( 48.25720115522312881, -49.89967198185726716, 51.25044237583277607 ) ) ;
#87417 = CARTESIAN_POINT ( 'NONE',  ( 105.5353273971932140, 1.030564683017419500E-14, 0.000000000000000000 ) ) ;
#87418 = FACE_OUTER_BOUND ( 'NONE', #56284, .T. ) ;
#87420 = EDGE_CURVE ( 'NONE', #85648, #15028, #11143, .T. ) ;
#87419 = CARTESIAN_POINT ( 'NONE',  ( -108.8776466121674247, -38.35654235866562090, 190.5204387342744496 ) ) ;
#87421 = CIRCLE ( 'NONE', #54655, 4.000000000000007105 ) ;
#87422 = VERTEX_POINT ( 'NONE', #25451 ) ;
#87423 = CARTESIAN_POINT ( 'NONE',  ( 84.59625264859418792, -38.35850040426321783, -23.20098218201213314 ) ) ;
#87424 = CARTESIAN_POINT ( 'NONE',  ( 13.52444138084156400, 7.616853773666340643, -8.431612038840972545 ) ) ;
#87425 = CARTESIAN_POINT ( 'NONE',  ( -19.47898085236668919, 49.99431953961255459, 60.29633468442251854 ) ) ;
#87426 =( LENGTH_UNIT ( ) NAMED_UNIT ( * ) SI_UNIT ( .MILLI., .METRE. ) );
#87427 = CARTESIAN_POINT ( 'NONE',  ( 5.211029210576866078, 40.56334907184437810, -70.92280024200073285 ) ) ;
#87428 = CARTESIAN_POINT ( 'NONE',  ( -31.73514475001178781, 436.7265089541918996, 21.10053246029738006 ) ) ;
#87429 = CARTESIAN_POINT ( 'NONE',  ( -32.28930913497472943, 488.2717154064631586, 9.213726894912662502 ) ) ;
#87430 = CARTESIAN_POINT ( 'NONE',  ( 12.50000000000000000, -3.000000000000000000, -11.21398294031086706 ) ) ;
#87431 = STYLED_ITEM ( 'NONE', ( #58321 ), #29400 ) ;
#87432 = CARTESIAN_POINT ( 'NONE',  ( 103.4822615650508482, -59.99999999999999289, 200.3271293562201834 ) ) ;
#87433 = ORIENTED_EDGE ( 'NONE', *, *, #48254, .T. ) ;
#87434 = CARTESIAN_POINT ( 'NONE',  ( -29.80964876741045444, 297.6586656248026657, -1.384360942660989746 ) ) ;
#87435 = ADVANCED_FACE ( 'NONE', ( #41592 ), #57637, .T. ) ;
#87436 = CARTESIAN_POINT ( 'NONE',  ( 7.801642220026313801, 33.58796826149033166, 1.787233835843581087 ) ) ;
#87437 = CARTESIAN_POINT ( 'NONE',  ( -6.928203230275510549, 29.99999999999999645, -4.000000000000000000 ) ) ;
#87438 = ORIENTED_EDGE ( 'NONE', *, *, #41488, .T. ) ;
#87440 = CARTESIAN_POINT ( 'NONE',  ( 5.221666942817044799, 7.014479873995792758, -27.48209584563044316 ) ) ;
#87439 = CARTESIAN_POINT ( 'NONE',  ( -91.45565477381764197, -38.38900636631056074, -7.819068096363136711 ) ) ;
#87441 = CARTESIAN_POINT ( 'NONE',  ( 4.205882352941182845, -5.000000000000000000, -72.69916451482998809 ) ) ;
#87442 = CARTESIAN_POINT ( 'NONE',  ( 7.500000000000000000, 4.330127018922203419, -0.9999999999999974465 ) ) ;
#87443 = CYLINDRICAL_SURFACE ( 'NONE', #105743, 1.249999999999999334 ) ;
#87444 = CARTESIAN_POINT ( 'NONE',  ( 5.082755093536325930, -16.34375000204838813, -5.082755093536325042 ) ) ;
#87445 = CARTESIAN_POINT ( 'NONE',  ( 7.996668422910687468, -3.000000000000002665, -91.14546720082027775 ) ) ;
#87446 = VECTOR ( 'NONE', #45616, 1000.000000000000000 ) ;
#87447 = SURFACE_STYLE_FILL_AREA ( #30823 ) ;
#87449 = EDGE_LOOP ( 'NONE', ( #37383, #5257, #92602, #1762, #657, #41492 ) ) ;
#87448 = DIRECTION ( 'NONE',  ( 0.000000000000000000, 0.000000000000000000, 1.000000000000000000 ) ) ;
#87450 = CARTESIAN_POINT ( 'NONE',  ( 80.98187379999048119, -56.93991788919779395, 178.5819717544341358 ) ) ;
#87451 = CARTESIAN_POINT ( 'NONE',  ( 33.86650669486618881, 1.474610560812782335E-15, 0.000000000000000000 ) ) ;
#87452 = CONICAL_SURFACE ( 'NONE', #94378, 5.000000000000001776, 0.9599310885968803664 ) ;
#87453 = CARTESIAN_POINT ( 'NONE',  ( -41.75331920095275251, 461.8277566036530288, 2.915730576367146831 ) ) ;
#87454 = ORIENTED_EDGE ( 'NONE', *, *, #88242, .F. ) ;
#87455 = CARTESIAN_POINT ( 'NONE',  ( -37.70494463962872089, 407.6443545989597510, 6.531502666333342866 ) ) ;
#87456 = CARTESIAN_POINT ( 'NONE',  ( 17.08031957351993668, 34.19942078064286761, 24.26593081561334486 ) ) ;
#87457 = CARTESIAN_POINT ( 'NONE',  ( -15.99999999999008793, 2.437231117890474863, 5.694551215252954712 ) ) ;
#87458 = DIRECTION ( 'NONE',  ( 0.5735764363510462704, 0.8191520442889915765, 0.000000000000000000 ) ) ;
#87459 = CARTESIAN_POINT ( 'NONE',  ( -25.52709155447669076, 43.61749475787997454, -75.40605120386278770 ) ) ;
#87460 = EDGE_CURVE ( 'NONE', #95530, #3257, #50210, .T. ) ;
#87461 = ORIENTED_EDGE ( 'NONE', *, *, #100790, .F. ) ;
#87462 =( LENGTH_UNIT ( ) NAMED_UNIT ( * ) SI_UNIT ( .MILLI., .METRE. ) );
#87463 = AXIS2_PLACEMENT_3D ( 'NONE', #53922, #86853, #70654 ) ;
#87464 = CARTESIAN_POINT ( 'NONE',  ( -8.728354254914082233, 295.2541512756494058, 4.889958989508364162 ) ) ;
#87465 = CARTESIAN_POINT ( 'NONE',  ( -5.000000000000000000, -3.274064727865673152, -10.50970520401928177 ) ) ;
#87466 = DIRECTION ( 'NONE',  ( 0.8191520442889974607, 1.003171929053531649E-16, -0.5735764363510379438 ) ) ;
#87467 = ADVANCED_FACE ( 'NONE', ( #83110 ), #34070, .T. ) ;
#87468 = LINE ( 'NONE', #46465, #37953 ) ;
#87469 = CARTESIAN_POINT ( 'NONE',  ( -2.977408999572650039, -21.68750000204838813, -7.188101187500001821 ) ) ;
#87470 = CARTESIAN_POINT ( 'NONE',  ( 11.51004862373886262, 294.5990991804076202, -2.053735195510829836 ) ) ;
#87471 = MECHANICAL_DESIGN_GEOMETRIC_PRESENTATION_REPRESENTATION (  '', ( #94398 ), #16867 ) ;
#87472 = CARTESIAN_POINT ( 'NONE',  ( 0.000000000000000000, 0.000000000000000000, -7.974599999999995248 ) ) ;
#87473 = ORIENTED_EDGE ( 'NONE', *, *, #3608, .F. ) ;
#87474 = EDGE_CURVE ( 'NONE', #29093, #61957, #71429, .T. ) ;
#87475 = LINE ( 'NONE', #79360, #40619 ) ;
#87476 = DIRECTION ( 'NONE',  ( -1.000000000000000000, 0.000000000000000000, 0.000000000000000000 ) ) ;
#87477 = CARTESIAN_POINT ( 'NONE',  ( -5.043779463085778403, 6.427503865159613916, -5.000000000000000000 ) ) ;
#87478 =( GEOMETRIC_REPRESENTATION_CONTEXT ( 3 ) GLOBAL_UNCERTAINTY_ASSIGNED_CONTEXT ( ( #43747 ) ) GLOBAL_UNIT_ASSIGNED_CONTEXT ( ( #67761, #35427, #10049 ) ) REPRESENTATION_CONTEXT ( 'NONE', 'WORKASPACE' ) );
#87479 = DIRECTION ( 'NONE',  ( 0.000000000000000000, 0.000000000000000000, 1.000000000000000000 ) ) ;
#87480 = CARTESIAN_POINT ( 'NONE',  ( -14.27029591641004380, 3.391655494187081565, 4.551126452522245458 ) ) ;
#87481 = ORIENTED_EDGE ( 'NONE', *, *, #96370, .F. ) ;
#87482 = VECTOR ( 'NONE', #52974, 1000.000000000000000 ) ;
#87483 = CARTESIAN_POINT ( 'NONE',  ( 44.36529472639534788, 435.1964152669797841, 13.54961189024334267 ) ) ;
#87484 = DIRECTION ( 'NONE',  ( 0.000000000000000000, 0.000000000000000000, 1.000000000000000000 ) ) ;
#87485 = ORIENTED_EDGE ( 'NONE', *, *, #101340, .F. ) ;
#87486 = CARTESIAN_POINT ( 'NONE',  ( 13.58349330513380160, -4.000000000000000000, 4.898587196589415787E-16 ) ) ;
#87487 = AXIS2_PLACEMENT_3D ( 'NONE', #97716, #70810, #55649 ) ;
#87488 = CARTESIAN_POINT ( 'NONE',  ( 7.054522925320324767, 41.71556257522360767, -59.55896313260247865 ) ) ;
#87489 = CARTESIAN_POINT ( 'NONE',  ( 0.000000000000000000, 0.000000000000000000, -2.575493252495433261 ) ) ;
#87490 = CARTESIAN_POINT ( 'NONE',  ( -110.4357402000322992, -60.00000000000000711, 147.0196122877912330 ) ) ;
#87491 = FACE_OUTER_BOUND ( 'NONE', #76094, .T. ) ;
#87492 = CARTESIAN_POINT ( 'NONE',  ( 16.85921514102166796, 304.5746142243267514, -9.058973955187422433 ) ) ;
#87493 = DIRECTION ( 'NONE',  ( -1.000000000000000000, 0.000000000000000000, -0.000000000000000000 ) ) ;
#87494 = STYLED_ITEM ( 'NONE', ( #96425 ), #29969 ) ;
#87495 = CARTESIAN_POINT ( 'NONE',  ( -82.96961521666786155, -53.66285722192446173, 186.0285578845195857 ) ) ;
#87496 = CARTESIAN_POINT ( 'NONE',  ( 4.699999999999999289, 0.000000000000000000, 0.000000000000000000 ) ) ;
#87497 = ORIENTED_EDGE ( 'NONE', *, *, #32524, .T. ) ;
#87498 = SURFACE_SIDE_STYLE ('',( #47012 ) ) ;
#87499 = EDGE_CURVE ( 'NONE', #29512, #20310, #45666, .T. ) ;
#87500 = CARTESIAN_POINT ( 'NONE',  ( 5.191472769733077364, -67.64091576718948318, -3.014900733016756540 ) ) ;
#87501 = CARTESIAN_POINT ( 'NONE',  ( -86.21150843268111430, -60.13471841444653876, 7.287450485273263112 ) ) ;
#87502 = CARTESIAN_POINT ( 'NONE',  ( -32.04841611708074112, 486.3115588597283363, 5.780120484955278748 ) ) ;
#87503 = AXIS2_PLACEMENT_3D ( 'NONE', #33626, #42219, #35230 ) ;
#87504 = CARTESIAN_POINT ( 'NONE',  ( 8.167402502818406518, 112.7203465494857966, -5.000000000000000888 ) ) ;
#87505 = DIRECTION ( 'NONE',  ( -0.2529971249647445797, 0.000000000000000000, 0.9674670303217436373 ) ) ;
#87506 = CARTESIAN_POINT ( 'NONE',  ( -38.36535705883633085, 18.64316884711714195, -5.022013495247519721 ) ) ;
#87507 = EDGE_CURVE ( 'NONE', #101359, #20792, #9735, .T. ) ;
#87508 = VECTOR ( 'NONE', #85822, 999.9999999999998863 ) ;
#87509 = CARTESIAN_POINT ( 'NONE',  ( 78.68869634200761709, -14.21045842199439591, 170.0117969751115652 ) ) ;
#87510 = CARTESIAN_POINT ( 'NONE',  ( -111.4777060157506128, -60.00000000000003553, 136.6114436209108760 ) ) ;
#87511 = CARTESIAN_POINT ( 'NONE',  ( -65.69038446180861968, -18.62633488832963380, 77.38884398866117920 ) ) ;
#87512 = ORIENTED_EDGE ( 'NONE', *, *, #86255, .F. ) ;
#87513 = CARTESIAN_POINT ( 'NONE',  ( -63.23885718349010432, 38.95363886516651775, -7.929982538254300550 ) ) ;
#87514 = CARTESIAN_POINT ( 'NONE',  ( 101.5656943390243043, -59.99999999999504752, 203.9136707109788063 ) ) ;
#87515 = ORIENTED_EDGE ( 'NONE', *, *, #29726, .T. ) ;
#87516 = CARTESIAN_POINT ( 'NONE',  ( 13.44292909870241459, -55.29335566891484888, 30.91132584605806244 ) ) ;
#87517 = CARTESIAN_POINT ( 'NONE',  ( -5.082755093536325042, -18.96875000204838457, -5.082755093536325930 ) ) ;
#87518 = CARTESIAN_POINT ( 'NONE',  ( -32.88333705524179607, 439.7317646416724415, 24.13381181826117583 ) ) ;
#87519 = ORIENTED_EDGE ( 'NONE', *, *, #71667, .F. ) ;
#87520 = CARTESIAN_POINT ( 'NONE',  ( -11.50618969897588428, 45.40753567543399782, 14.44225189481708682 ) ) ;
#87521 = ORIENTED_EDGE ( 'NONE', *, *, #64988, .F. ) ;
#87522 = FACE_OUTER_BOUND ( 'NONE', #85641, .T. ) ;
#87523 = CARTESIAN_POINT ( 'NONE',  ( -41.96546066671912456, 485.5623541565421988, -4.077117913357734658 ) ) ;
#87524 = CARTESIAN_POINT ( 'NONE',  ( -89.61226365779903347, -59.99999999999998579, -19.45967901788216281 ) ) ;
#87525 = DIRECTION ( 'NONE',  ( -1.000000000000000000, -1.224606353822377258E-16, -0.000000000000000000 ) ) ;
#87526 = CARTESIAN_POINT ( 'NONE',  ( 7.188101187500000044, -33.03125000204838813, 0.000000000000000000 ) ) ;
#87527 = CARTESIAN_POINT ( 'NONE',  ( 23.73746414932995208, 1.482358050883964840E-15, 0.000000000000000000 ) ) ;
#87528 =( NAMED_UNIT ( * ) PLANE_ANGLE_UNIT ( ) SI_UNIT ( $, .RADIAN. ) );
#87529 = CARTESIAN_POINT ( 'NONE',  ( -1.308996937483426715, 48.00000000000000000, -95.00000000000000000 ) ) ;
#87530 = CARTESIAN_POINT ( 'NONE',  ( -46.00000000000001421, 437.8931063572202333, 13.37370747421774730 ) ) ;
#87531 = CARTESIAN_POINT ( 'NONE',  ( 8.866506694866188809, -3.999999999999998224, 0.000000000000000000 ) ) ;
#87532 = EDGE_CURVE ( 'NONE', #96201, #35207, #42652, .T. ) ;
#87533 = CARTESIAN_POINT ( 'NONE',  ( 102.1218162488970052, -59.99999999999997868, 194.0110499945668892 ) ) ;
#87534 = ORIENTED_EDGE ( 'NONE', *, *, #54077, .F. ) ;
#87535 = CARTESIAN_POINT ( 'NONE',  ( 3.294249609603385309, 39.99999999999999289, -70.27378291343094929 ) ) ;
#87536 = CARTESIAN_POINT ( 'NONE',  ( 5.000000000000000000, 6.123233995736766282E-16, -9.974599999999998801 ) ) ;
#87537 = AXIS2_PLACEMENT_3D ( 'NONE', #83509, #8557, #33395 ) ;
#87538 = AXIS2_PLACEMENT_3D ( 'NONE', #60336, #19375, #71985 ) ;
#87539 = CARTESIAN_POINT ( 'NONE',  ( 35.84311413758839393, -39.50387582939524833, 35.79840239775683841 ) ) ;
#87541 = CONICAL_SURFACE ( 'NONE', #39341, 18.72828050308589454, 0.7292773806962717931 ) ;
#87540 = CARTESIAN_POINT ( 'NONE',  ( 8.569529079651905690, -1.734723475976807094E-15, -14.86825985027703290 ) ) ;
#87542 = ORIENTED_EDGE ( 'NONE', *, *, #45808, .T. ) ;
#87543 = CARTESIAN_POINT ( 'NONE',  ( 0.000000000000000000, 0.000000000000000000, 0.000000000000000000 ) ) ;
#87544 = VERTEX_POINT ( 'NONE', #74476 ) ;
#87546 = CARTESIAN_POINT ( 'NONE',  ( -35.74363442581862671, 380.1068966271811860, 4.951945592532029927 ) ) ;
#87545 = CARTESIAN_POINT ( 'NONE',  ( 8.678535172863940161, -4.999999999999999112, -16.67878089796255381 ) ) ;
#87547 = FACE_OUTER_BOUND ( 'NONE', #82288, .T. ) ;
#87548 = CARTESIAN_POINT ( 'NONE',  ( 6.683837171061805194, -3.955946848495972556, -6.851900933636989599 ) ) ;
#87549 = AXIS2_PLACEMENT_3D ( 'NONE', #106252, #74949, #81443 ) ;
#87550 = CARTESIAN_POINT ( 'NONE',  ( -42.20041562234358423, 435.2369744135583574, 7.788607701745487333 ) ) ;
#87551 = DIRECTION ( 'NONE',  ( 0.000000000000000000, 0.000000000000000000, -1.000000000000000000 ) ) ;
#87552 = CARTESIAN_POINT ( 'NONE',  ( -2.345389088905535324, -49.77582587123195879, 44.62432230782176390 ) ) ;
#87553 = ORIENTED_EDGE ( 'NONE', *, *, #75496, .T. ) ;
#87554 = CARTESIAN_POINT ( 'NONE',  ( 93.32736978825312235, -59.99999999999999289, 35.45440158309499168 ) ) ;
#87555 = CARTESIAN_POINT ( 'NONE',  ( 28.32728760970740112, 34.16880792299276948, -9.119155454780885961 ) ) ;
#87556 = FACE_OUTER_BOUND ( 'NONE', #102221, .T. ) ;
#87557 = DIRECTION ( 'NONE',  ( -1.000000000000000000, -0.000000000000000000, -0.000000000000000000 ) ) ;
#87558 = CARTESIAN_POINT ( 'NONE',  ( -13.59109867861701382, 7.493105839183076711, -8.373922924896398001 ) ) ;
#87559 = ORIENTED_EDGE ( 'NONE', *, *, #60700, .T. ) ;
#87560 = COLOUR_RGB ( '', 0.09019608, 0.27058824, 0.51372549) ;
#87561 = CARTESIAN_POINT ( 'NONE',  ( -85.43970026633695625, -30.00000000001166711, -20.50169416853363913 ) ) ;
#87562 = ORIENTED_EDGE ( 'NONE', *, *, #69975, .T. ) ;
#87563 = CARTESIAN_POINT ( 'NONE',  ( 5.007715329123895321E-16, -7.505553499465175804, -8.000000000000000000 ) ) ;
#87564 = DIRECTION ( 'NONE',  ( 0.5735764363510462704, 0.8191520442889915765, 0.000000000000000000 ) ) ;
#87565 = CARTESIAN_POINT ( 'NONE',  ( 16.10099483391905295, 21.87267635329353510, 0.2108314046451076063 ) ) ;
#87566 = CARTESIAN_POINT ( 'NONE',  ( 84.79608313886490123, -60.18564194205600160, -16.37796101195803899 ) ) ;
#87567 = CARTESIAN_POINT ( 'NONE',  ( -7.188101187500000044, -29.28125000204838813, -8.802885111219163269E-16 ) ) ;
#87568 = CARTESIAN_POINT ( 'NONE',  ( 83.28888888888889142, -4.171999999999998820, 0.000000000000000000 ) ) ;
#87569 = PRESENTATION_STYLE_ASSIGNMENT (( #71361 ) ) ;
#87570 = ORIENTED_EDGE ( 'NONE', *, *, #92045, .F. ) ;
#87571 = CIRCLE ( 'NONE', #94507, 8.000000000000007105 ) ;
#87572 = AXIS2_PLACEMENT_3D ( 'NONE', #38223, #53838, #55415 ) ;
#87574 = VERTEX_POINT ( 'NONE', #552 ) ;
#87573 = DIRECTION ( 'NONE',  ( -1.000000000000000000, -1.224606353822377258E-16, -0.000000000000000000 ) ) ;
#87575 = CARTESIAN_POINT ( 'NONE',  ( 81.45652690482418734, -25.62336553616171386, 139.9540395895450615 ) ) ;
#87576 = CARTESIAN_POINT ( 'NONE',  ( -37.88732364326676816, 27.49841400577992445, -13.42516778733551241 ) ) ;
#87577 = ORIENTED_EDGE ( 'NONE', *, *, #54899, .F. ) ;
#87578 = CARTESIAN_POINT ( 'NONE',  ( 28.50099738913158376, 1.340359594676612611E-15, 0.000000000000000000 ) ) ;
#87579 = DIRECTION ( 'NONE',  ( -0.2237693372482013887, 0.01887181578571871243, 0.9744594082240937150 ) ) ;
#87580 = CARTESIAN_POINT ( 'NONE',  ( -5.082755093536326818, -18.21875000204838457, 5.082755093536325042 ) ) ;
#87581 = CARTESIAN_POINT ( 'NONE',  ( -67.94141844175470624, -57.68152395592925785, 141.0744097219443347 ) ) ;
#87582 = CYLINDRICAL_SURFACE ( 'NONE', #60708, 4.000000000000000000 ) ;
#87583 = EDGE_CURVE ( 'NONE', #876, #826, #42181, .T. ) ;
#87584 = EDGE_LOOP ( 'NONE', ( #46683, #64068, #80626, #32478, #80509 ) ) ;
#87585 = EDGE_CURVE ( 'NONE', #31429, #48619, #95628, .T. ) ;
#87586 = VECTOR ( 'NONE', #89062, 1000.000000000000000 ) ;
#87587 = CARTESIAN_POINT ( 'NONE',  ( 3.021265037602210324, 47.67867182518293134, 5.000000000000001776 ) ) ;
#87588 = MANIFOLD_SOLID_BREP ( '<13. Handle Knob>-<Fillet1>', #92802 ) ;
#87589 = AXIS2_PLACEMENT_3D ( 'NONE', #77989, #28410, #85569 ) ;
#87590 = CARTESIAN_POINT ( 'NONE',  ( 6.943035990376878352, 41.50417910381163011, -58.81491866537869129 ) ) ;
#87591 = ADVANCED_FACE ( 'NONE', ( #9996 ), #65174, .T. ) ;
#87592 = CARTESIAN_POINT ( 'NONE',  ( 3.313708498984762496, -14.46875000409676915, 7.999999999999998224 ) ) ;
#87593 = CARTESIAN_POINT ( 'NONE',  ( -19.40485415781282441, -16.85763090055889180, 31.48763308485285606 ) ) ;
#87594 =( LENGTH_UNIT ( ) NAMED_UNIT ( * ) SI_UNIT ( .MILLI., .METRE. ) );
#87595 = AXIS2_PLACEMENT_3D ( 'NONE', #15465, #72114, #14928 ) ;
#87596 = DIRECTION ( 'NONE',  ( 1.000000000000000000, 0.000000000000000000, 0.000000000000000000 ) ) ;
#87597 = VECTOR ( 'NONE', #50305, 1000.000000000000000 ) ;
#87598 = DIRECTION ( 'NONE',  ( 0.000000000000000000, 0.000000000000000000, 1.000000000000000000 ) ) ;
#87599 = B_SPLINE_CURVE_WITH_KNOTS ( 'NONE', 3,
 ( #15374, #57412, #72547, #39673 ),
 .UNSPECIFIED., .F., .F.,
 ( 4, 4 ),
 ( 3.469446951953614189E-18, 0.002256496660487678635 ),
 .UNSPECIFIED. ) ;
#87600 = CARTESIAN_POINT ( 'NONE',  ( -31.87080426956102031, 439.0384429942135398, 24.63328115755084013 ) ) ;
#87601 = DIRECTION ( 'NONE',  ( 0.7999999999999989342, 0.000000000000000000, -0.6000000000000014211 ) ) ;
#87602 = CARTESIAN_POINT ( 'NONE',  ( 38.32908635939623565, 27.37244634754295092, 13.21054841214205311 ) ) ;
#87603 = ORIENTED_EDGE ( 'NONE', *, *, #28229, .T. ) ;
#87604 = CARTESIAN_POINT ( 'NONE',  ( -2.802997532626366972, -53.56901273344412573, 40.71799139369159803 ) ) ;
#87605 = ADVANCED_FACE ( 'NONE', ( #98858 ), #28350, .F. ) ;
#87606 = CARTESIAN_POINT ( 'NONE',  ( 31.36650669486618881, 1.474610560812782335E-15, 0.000000000000000000 ) ) ;
#87607 = CARTESIAN_POINT ( 'NONE',  ( -40.03012460245057724, 436.4820657380744251, 5.641945619390483557 ) ) ;
#87608 = CARTESIAN_POINT ( 'NONE',  ( -67.72357546289919128, -30.20750568365551914, -30.58700924850430525 ) ) ;
#87609 = CARTESIAN_POINT ( 'NONE',  ( -82.85790275495963897, -30.00000000000000355, 151.8675718132654708 ) ) ;
#87610 = CARTESIAN_POINT ( 'NONE',  ( 7.500000000000007105, 40.00000000000000000, -62.89165061482969321 ) ) ;
#87611 = ORIENTED_EDGE ( 'NONE', *, *, #72484, .T. ) ;
#87612 = VECTOR ( 'NONE', #45719, 1000.000000000000000 ) ;
#87613 = CARTESIAN_POINT ( 'NONE',  ( 4.488554439770307297E-15, -1.341159125180006795, -15.80007993603364724 ) ) ;
#87614 = CARTESIAN_POINT ( 'NONE',  ( 90.68632663689517415, -57.61165737844666523, 204.1158738846914105 ) ) ;
#87615 = CARTESIAN_POINT ( 'NONE',  ( 60.68635431291335891, -60.22842679285083278, -29.53366749605343244 ) ) ;
#87616 = CARTESIAN_POINT ( 'NONE',  ( -2.075968632160923644, -6.306992450857648258, -6.056431503346049183 ) ) ;
#87617 = CARTESIAN_POINT ( 'NONE',  ( -14.81450998444591249, 22.88381389411949485, -2.101451306596820334 ) ) ;
#87618 = DIRECTION ( 'NONE',  ( 0.000000000000000000, 0.5000000000000008882, -0.8660254037844381525 ) ) ;
#87619 = CARTESIAN_POINT ( 'NONE',  ( -54.67094165204726153, -59.99999999999999289, 84.31617412822056679 ) ) ;
#87620 =( GEOMETRIC_REPRESENTATION_CONTEXT ( 3 ) GLOBAL_UNCERTAINTY_ASSIGNED_CONTEXT ( ( #25807 ) ) GLOBAL_UNIT_ASSIGNED_CONTEXT ( ( #106682, #65168, #33898 ) ) REPRESENTATION_CONTEXT ( 'NONE', 'WORKASPACE' ) );
#87621 = SURFACE_STYLE_FILL_AREA ( #103265 ) ;
#87622 = CARTESIAN_POINT ( 'NONE',  ( -32.20054824794776493, 485.9557913861499969, 4.953638954091799995 ) ) ;
#87623 = CARTESIAN_POINT ( 'NONE',  ( -5.957442974701830707, 49.99999999999999289, 65.00000000000000000 ) ) ;
#87624 = CARTESIAN_POINT ( 'NONE',  ( -85.88675850019390623, -35.61340147578555104, 185.0195460185883007 ) ) ;
#87625 = VERTEX_POINT ( 'NONE', #76719 ) ;
#87626 = CARTESIAN_POINT ( 'NONE',  ( 35.50900462289761350, 382.2641358326593490, 6.015446932962731807 ) ) ;
#87627 = CARTESIAN_POINT ( 'NONE',  ( 12.13955930136260442, -4.660274349647991698, -76.81824564200809391 ) ) ;
#87628 = EDGE_CURVE ( 'NONE', #35844, #76618, #38744, .T. ) ;
#87629 = CARTESIAN_POINT ( 'NONE',  ( -83.04293233812605024, -45.25987585949575731, -14.40421945740175502 ) ) ;
#87630 = VECTOR ( 'NONE', #101417, 1000.000000000000000 ) ;
#87631 = CARTESIAN_POINT ( 'NONE',  ( 8.099999999999999645, -3.752776749732574135, -6.500000000000001776 ) ) ;
#87632 = CARTESIAN_POINT ( 'NONE',  ( 99.75754961941544252, 1.030564683017419500E-14, 0.000000000000000000 ) ) ;
#87633 = CONICAL_SURFACE ( 'NONE', #73830, 4.172000000000001485, 0.9599310885968750373 ) ;
#87634 = VERTEX_POINT ( 'NONE', #36324 ) ;
#87635 = CARTESIAN_POINT ( 'NONE',  ( 19.14172393082469981, 50.00000000000001421, 60.39347634864844849 ) ) ;
#87636 = CARTESIAN_POINT ( 'NONE',  ( 13.54336320516353176, 24.68363219323660473, 1.315439817157240343 ) ) ;
#87637 = EDGE_CURVE ( 'NONE', #25507, #25785, #60574, .T. ) ;
#87638 = ADVANCED_FACE ( 'NONE', ( #1760 ), #59455, .T. ) ;
#87639 = CARTESIAN_POINT ( 'NONE',  ( -19.43146043914380172, -4.830718742626120971E-12, 11.19959342723174522 ) ) ;
#87640 = CIRCLE ( 'NONE', #101412, 3.309500000000001663 ) ;
#87641 = DIRECTION ( 'NONE',  ( -0.5735764363510497121, 0.8191520442889892450, 1.003171929053521665E-16 ) ) ;
#87642 = AXIS2_PLACEMENT_3D ( 'NONE', #54138, #33100, #48176 ) ;
#87643 = CARTESIAN_POINT ( 'NONE',  ( 72.33341283407553135, -14.21045842199439235, -25.95464913363236548 ) ) ;
#87644 = CARTESIAN_POINT ( 'NONE',  ( -80.37542441551636330, -32.56178760357695268, 140.7699095010514441 ) ) ;
#87645 = ORIENTED_EDGE ( 'NONE', *, *, #42854, .F. ) ;
#87646 = CARTESIAN_POINT ( 'NONE',  ( 42.99999999999999289, 485.2629658518202973, -2.796394914059370240 ) ) ;
#87647 = SURFACE_STYLE_FILL_AREA ( #86602 ) ;
#87648 = CARTESIAN_POINT ( 'NONE',  ( 95.57460276385096165, -57.62113478352900842, 204.5314498424847329 ) ) ;
#87649 = CARTESIAN_POINT ( 'NONE',  ( 56.29065232361070059, 49.99999999999999289, -28.72822482865823801 ) ) ;
#87650 = CARTESIAN_POINT ( 'NONE',  ( 38.38704938250420184, 306.2898962380254488, -7.348315413633529580 ) ) ;
#87651 = FACE_OUTER_BOUND ( 'NONE', #7574, .T. ) ;
#87652 = VERTEX_POINT ( 'NONE', #1213 ) ;
#87653 = CARTESIAN_POINT ( 'NONE',  ( 7.500000000000000888, 2.932633423934448924, -0.4709827563909285697 ) ) ;
#87654 = SURFACE_SIDE_STYLE ('',( #63390 ) ) ;
#87656 = CARTESIAN_POINT ( 'NONE',  ( -102.6106292806730949, -37.82052530689579584, 165.6551701195334658 ) ) ;
#87655 = PLANE ( 'NONE',  #103524 ) ;
#87657 = CARTESIAN_POINT ( 'NONE',  ( -5.082755093536326818, -27.21875000204838813, 5.082755093536325042 ) ) ;
#87658 = DIRECTION ( 'NONE',  ( 0.000000000000000000, 0.7863624351922580136, -0.6177654251562657572 ) ) ;
#87659 = EDGE_CURVE ( 'NONE', #23322, #70575, #9438, .T. ) ;
#87660 = DIRECTION ( 'NONE',  ( 1.734723475976807094E-16, 0.000000000000000000, 1.000000000000000000 ) ) ;
#87661 = FACE_OUTER_BOUND ( 'NONE', #106638, .T. ) ;
#87662 = CARTESIAN_POINT ( 'NONE',  ( 25.92903732128599970, 37.10984168163323460, 9.238478874643890393 ) ) ;
#87663 = DIRECTION ( 'NONE',  ( -1.000000000000000000, -0.000000000000000000, -0.000000000000000000 ) ) ;
#87664 = EDGE_CURVE ( 'NONE', #26284, #83206, #69763, .T. ) ;
#87666 = CARTESIAN_POINT ( 'NONE',  ( -35.07179216366830588, 463.5162043426217338, 19.70794395571720159 ) ) ;
#87665 = CIRCLE ( 'NONE', #103128, 4.000000000000000888 ) ;
#87667 = ORIENTED_EDGE ( 'NONE', *, *, #36078, .T. ) ;
#87668 = CARTESIAN_POINT ( 'NONE',  ( 43.32251133975108814, 485.6545735287631942, 4.688172406453896990 ) ) ;
#87670 = CARTESIAN_POINT ( 'NONE',  ( 27.39423346129563441, -56.86438257397906426, 35.32388413555721485 ) ) ;
#87669 = CARTESIAN_POINT ( 'NONE',  ( -48.02140427201592132, -30.00000000000008527, 60.50294052774201958 ) ) ;
#87671 = CARTESIAN_POINT ( 'NONE',  ( 23.21751746555144180, 27.38103382803512176, -33.20617127781698485 ) ) ;
#87672 = ORIENTED_EDGE ( 'NONE', *, *, #92013, .T. ) ;
#87673 = EDGE_CURVE ( 'NONE', #58987, #21224, #27698, .T. ) ;
#87674 = EDGE_LOOP ( 'NONE', ( #20007, #69916, #9529, #33008 ) ) ;
#87675 = CARTESIAN_POINT ( 'NONE',  ( -6.539732759932824102, -4.285714285714295357, -24.41571844174603712 ) ) ;
#87676 = CARTESIAN_POINT ( 'NONE',  ( 119.9999999999999432, 0.000000000000000000, 60.00000000000001421 ) ) ;
#87677 = FACE_OUTER_BOUND ( 'NONE', #63247, .T. ) ;
#87678 = CARTESIAN_POINT ( 'NONE',  ( 5.947762761376476526, -4.378239541354671971, -5.416666666666665186 ) ) ;
#87679 = EDGE_CURVE ( 'NONE', #97678, #105636, #37073, .T. ) ;
#87680 = CARTESIAN_POINT ( 'NONE',  ( -30.00000000000000355, 489.0503989117699462, 4.976653691326955453 ) ) ;
#87681 = FACE_OUTER_BOUND ( 'NONE', #100423, .T. ) ;
#87682 = VERTEX_POINT ( 'NONE', #84296 ) ;
#87683 = CARTESIAN_POINT ( 'NONE',  ( 78.10340256886549071, -29.99999999999998224, 123.8744046566280161 ) ) ;
#87684 = CARTESIAN_POINT ( 'NONE',  ( -10.37205271324882894, 10.88037002444788115, -10.43000608149194974 ) ) ;
#87685 = CARTESIAN_POINT ( 'NONE',  ( -4.250000000000000000, 5.204748896376250699E-16, -1.971869939371574620 ) ) ;
#87686 = CARTESIAN_POINT ( 'NONE',  ( 81.59416543435395397, -30.00000000000000000, -6.868947773689183300 ) ) ;
#87687 =( BOUNDED_SURFACE ( )  B_SPLINE_SURFACE ( 3, 2, ( 
 ( #68165, #19666, #68719 ),
 ( #3967, #20196, #76779 ),
 ( #61698, #12042, #101602 ),
 ( #60107, #10448, #53052 ),
 ( #42824, #69767, #35839 ),
 ( #59556, #27757, #94592 ),
 ( #34771, #94035, #83805 ),
 ( #36382, #50897, #2355 ),
 ( #100523, #18579, #51441 ),
 ( #69246, #102661, #51967 ) ),
 .UNSPECIFIED., .F., .F., .F. ) 
 B_SPLINE_SURFACE_WITH_KNOTS ( ( 4, 2, 2, 2, 4 ),
 ( 3, 3 ),
 ( 1.647987302177966740E-17, 0.002793818337085216940, 0.003492272921356517380, 0.004190727505627817387, 0.005587636674170417400 ),
 ( 0.000000000000000000, 1.000000000000000000 ),
 .UNSPECIFIED. ) 
 GEOMETRIC_REPRESENTATION_ITEM ( )  RATIONAL_B_SPLINE_SURFACE ( (
 ( 1.000000000000000000, 0.8239349643288649272, 1.000000000000000000),
 ( 1.000000000000000000, 0.8395566633290327818, 1.000000000000000000),
 ( 1.000000000000000000, 0.8448327636212329406, 1.000000000000000000),
 ( 1.000000000000000000, 0.8449253469007168560, 1.000000000000000000),
 ( 1.000000000000000000, 0.8445754865294070601, 1.000000000000000000),
 ( 1.000000000000000000, 0.8431693930219159583, 1.000000000000000000),
 ( 1.000000000000000000, 0.8421154100742880289, 1.000000000000000000),
 ( 1.000000000000000000, 0.8378581409644991762, 1.000000000000000000),
 ( 1.000000000000000000, 0.8335888548715134627, 1.000000000000000000),
 ( 1.000000000000000000, 0.8273155905869840065, 1.000000000000000000) ) ) 
 REPRESENTATION_ITEM ( '' )  SURFACE ( )  );
#87688 = ORIENTED_EDGE ( 'NONE', *, *, #3704, .F. ) ;
#87689 = B_SPLINE_CURVE_WITH_KNOTS ( 'NONE', 3,
 ( #91389, #17505, #1270, #99992 ),
 .UNSPECIFIED., .F., .F.,
 ( 4, 4 ),
 ( 0.04383972994809587354, 1.043839729948095485 ),
 .UNSPECIFIED. ) ;
#87690 = ORIENTED_EDGE ( 'NONE', *, *, #33227, .F. ) ;
#87691 = ORIENTED_EDGE ( 'NONE', *, *, #1396, .F. ) ;
#87692 = DIRECTION ( 'NONE',  ( -0.000000000000000000, -0.000000000000000000, 1.000000000000000000 ) ) ;
#87693 = CARTESIAN_POINT ( 'NONE',  ( 38.86638200451619696, -5.000000000000000000, 0.000000000000000000 ) ) ;
#87694 = LINE ( 'NONE', #12190, #15556 ) ;
#87695 = CARTESIAN_POINT ( 'NONE',  ( 4.898587196589412829E-16, -16.81250000409677270, -8.000000000000000000 ) ) ;
#87696 = DIRECTION ( 'NONE',  ( 0.9737456255364647095, 0.000000000000000000, -0.2276388735444786204 ) ) ;
#87698 =( NAMED_UNIT ( * ) PLANE_ANGLE_UNIT ( ) SI_UNIT ( $, .RADIAN. ) );
#87697 = VECTOR ( 'NONE', #95804, 1000.000000000000000 ) ;
#87699 = DIRECTION ( 'NONE',  ( -1.000000000000000000, -1.224606353822377258E-16, -0.000000000000000000 ) ) ;
#87700 = EDGE_LOOP ( 'NONE', ( #6911, #46605 ) ) ;
#87701 = CARTESIAN_POINT ( 'NONE',  ( 30.23149608710470915, 7.786108077162794849, 41.98074016422795296 ) ) ;
#87702 = VERTEX_POINT ( 'NONE', #91854 ) ;
#87703 = DIRECTION ( 'NONE',  ( -0.000000000000000000, -1.000000000000000000, -0.000000000000000000 ) ) ;
#87704 = CARTESIAN_POINT ( 'NONE',  ( 49.92867099129379227, -38.33222471381543528, 68.31434411807451568 ) ) ;
#87705 = CARTESIAN_POINT ( 'NONE',  ( 14.29190075645646907, 21.26710225494832329, -5.626279437268317807 ) ) ;
#87706 = AXIS2_PLACEMENT_3D ( 'NONE', #68514, #12376, #85216 ) ;
#87707 = CARTESIAN_POINT ( 'NONE',  ( -82.88816647256838621, -60.00000000000002132, 189.8675524425106005 ) ) ;
#87708 = CARTESIAN_POINT ( 'NONE',  ( 62.93388706622030071, -56.86266190362758977, 89.13451098117751314 ) ) ;
#87709 = EDGE_LOOP ( 'NONE', ( #56821, #89082, #43708, #88100 ) ) ;
#87710 = CARTESIAN_POINT ( 'NONE',  ( 40.62545454912861942, 465.1696752979974576, 17.15421908636345449 ) ) ;
#87711 = CARTESIAN_POINT ( 'NONE',  ( -67.61735429566955702, -38.09521185367891860, -32.01360535522618989 ) ) ;
#87712 = CARTESIAN_POINT ( 'NONE',  ( 18.58349330513380337, 1.593028355512270567E-15, 0.000000000000000000 ) ) ;
#87713 = DIRECTION ( 'NONE',  ( 0.000000000000000000, 1.000000000000000000, 0.000000000000000000 ) ) ;
#87714 = ADVANCED_FACE ( 'NONE', ( #51914 ), #100469, .T. ) ;
#87715 = ORIENTED_EDGE ( 'NONE', *, *, #38965, .F. ) ;
#87716 = AXIS2_PLACEMENT_3D ( 'NONE', #43054, #50066, #44117 ) ;
#87717 = DIRECTION ( 'NONE',  ( -0.9915366780650374245, 0.1269898409407624329, 0.02699252395739039703 ) ) ;
#87718 = CARTESIAN_POINT ( 'NONE',  ( -22.49475958402852172, -60.00000000000000711, -35.87305261535499312 ) ) ;
#87719 = ADVANCED_FACE ( 'NONE', ( #75660 ), #85359, .F. ) ;
#87720 = CIRCLE ( 'NONE', #10239, 8.000000000000000000 ) ;
#87721 = CARTESIAN_POINT ( 'NONE',  ( 0.000000000000000000, -100.0000000000000000, -8.000000000000007105 ) ) ;
#87722 = EDGE_CURVE ( 'NONE', #96540, #45187, #31887, .T. ) ;
#87723 = CARTESIAN_POINT ( 'NONE',  ( -5.656854249492379694, -27.12500000409677270, -5.656854249492380582 ) ) ;
#87724 = CARTESIAN_POINT ( 'NONE',  ( 4.175893272575848414, -4.999999999999998224, 7.137815226408912750 ) ) ;
#87725 = CARTESIAN_POINT ( 'NONE',  ( 86.71645349442924555, -24.38046412487985393, 185.1854681036936370 ) ) ;
#87726 = EDGE_CURVE ( 'NONE', #37342, #18064, #62836, .T. ) ;
#87727 = AXIS2_PLACEMENT_3D ( 'NONE', #86080, #12152, #103309 ) ;
#87728 = EDGE_CURVE ( 'NONE', #89753, #21060, #71510, .T. ) ;
#87729 = CARTESIAN_POINT ( 'NONE',  ( -5.182201362424698310, 2.673072912720999561, -23.53106308636114008 ) ) ;
#87730 = CARTESIAN_POINT ( 'NONE',  ( -9.316042626968680906, 11.20129626819939617, -3.173958893453993444E-13 ) ) ;
#87731 = DIRECTION ( 'NONE',  ( 1.160749806054361473E-16, 0.000000000000000000, -1.000000000000000000 ) ) ;
#87732 = CARTESIAN_POINT ( 'NONE',  ( 15.26317471455340602, -17.21745123649166231, -34.34608131406640297 ) ) ;
#87733 = ORIENTED_EDGE ( 'NONE', *, *, #9395, .F. ) ;
#87734 = CARTESIAN_POINT ( 'NONE',  ( 13.97203307284001994, -50.12825479938464923, 26.07838388608699631 ) ) ;
#87735 = EDGE_CURVE ( 'NONE', #51428, #1378, #7435, .T. ) ;
#87736 = CARTESIAN_POINT ( 'NONE',  ( -5.656854249492381470, -10.06249999999999112, 5.656854249492379694 ) ) ;
#87737 = CARTESIAN_POINT ( 'NONE',  ( -100.8735123380655949, -29.99999999999999645, 179.4413083801154301 ) ) ;
#87738 = AXIS2_PLACEMENT_3D ( 'NONE', #19965, #52270, #10221 ) ;
#87739 = CARTESIAN_POINT ( 'NONE',  ( -37.85084083633361729, 438.0234350436313093, 4.171260309356228824 ) ) ;
#87740 = CARTESIAN_POINT ( 'NONE',  ( 52.23423719002784793, -57.67654141413034807, 83.35420455408277007 ) ) ;
#87742 = FILL_AREA_STYLE ('',( #103903 ) ) ;
#87741 = CARTESIAN_POINT ( 'NONE',  ( -0.3345420830801542067, 25.18327404291766669, -40.70732875437715137 ) ) ;
#87744 = CARTESIAN_POINT ( 'NONE',  ( -28.55298245902970677, 43.39596509286685944, -71.24613896942491920 ) ) ;
#87743 = VECTOR ( 'NONE', #66016, 1000.000000000000000 ) ;
#87745 = CARTESIAN_POINT ( 'NONE',  ( -18.20729755737727373, 50.00000000000000000, 61.62669174679179918 ) ) ;
#87746 = CARTESIAN_POINT ( 'NONE',  ( -46.00000000000000000, 461.7880546943549689, 10.79349299898142789 ) ) ;
#87747 =( NAMED_UNIT ( * ) PLANE_ANGLE_UNIT ( ) SI_UNIT ( $, .RADIAN. ) );
#87748 = DIRECTION ( 'NONE',  ( 0.000000000000000000, 1.000000000000000000, 0.000000000000000000 ) ) ;
#87749 = MECHANICAL_DESIGN_GEOMETRIC_PRESENTATION_REPRESENTATION (  '', ( #18945 ), #49850 ) ;
#87750 =( NAMED_UNIT ( * ) SI_UNIT ( $, .STERADIAN. ) SOLID_ANGLE_UNIT ( ) );
#87751 = CARTESIAN_POINT ( 'NONE',  ( -86.68846525915618884, -17.00810435402869913, 185.5403106198691887 ) ) ;
#87752 = ORIENTED_EDGE ( 'NONE', *, *, #15917, .F. ) ;
#87753 = PRESENTATION_STYLE_ASSIGNMENT (( #54823 ) ) ;
#87754 = CARTESIAN_POINT ( 'NONE',  ( 33.00496812083888898, 465.6658704666191966, 15.15901827093884258 ) ) ;
#87755 = CARTESIAN_POINT ( 'NONE',  ( -11.28694547044951868, -35.99452350529739419, 29.91534077212351761 ) ) ;
#87757 = FILL_AREA_STYLE ('',( #31135 ) ) ;
#87756 = CARTESIAN_POINT ( 'NONE',  ( 32.61650669486618881, 1.474610560812782335E-15, 0.000000000000000000 ) ) ;
#87758 = VERTEX_POINT ( 'NONE', #94533 ) ;
#87759 = CARTESIAN_POINT ( 'NONE',  ( 16.13590653351247184, 6.313628335805621106, -5.716602451449240618 ) ) ;
#87760 = DIRECTION ( 'NONE',  ( 0.000000000000000000, -1.000000000000000000, 0.000000000000000000 ) ) ;
#87761 = EDGE_CURVE ( 'NONE', #17374, #38799, #21630, .T. ) ;
#87762 = CARTESIAN_POINT ( 'NONE',  ( 15.90328822607585479, 3.524689239570375499, -2.889827284395872553 ) ) ;
#87763 = CARTESIAN_POINT ( 'NONE',  ( 65.89100576562174183, -60.00000000000002842, 121.9363084267107809 ) ) ;
#87764 = CARTESIAN_POINT ( 'NONE',  ( -1.217303283917842371, 53.94016066554750211, -8.674587859239702325 ) ) ;
#87765 = B_SPLINE_CURVE_WITH_KNOTS ( 'NONE', 3,
 ( #97632, #57175, #32943, #15134, #16192, #81977 ),
 .UNSPECIFIED., .F., .F.,
 ( 4, 2, 4 ),
 ( 0.003990927807053575027, 0.005983070073873390966, 0.007975212340693206906 ),
 .UNSPECIFIED. ) ;
#87766 = ORIENTED_EDGE ( 'NONE', *, *, #87929, .F. ) ;
#87767 = CARTESIAN_POINT ( 'NONE',  ( 18.58349330513380337, 4.000000000000002665, 0.000000000000000000 ) ) ;
#87768 = CARTESIAN_POINT ( 'NONE',  ( -34.99928578097298981, 435.2191065300279433, 7.261429118812875672 ) ) ;
#87769 = AXIS2_PLACEMENT_3D ( 'NONE', #23762, #64721, #54613 ) ;
#87770 = CARTESIAN_POINT ( 'NONE',  ( 7.069742150690448312, 41.66287055390499461, -69.58314084581829206 ) ) ;
#87771 = CARTESIAN_POINT ( 'NONE',  ( 4.474408960159398596, 142.5175018677392416, -5.000000000000000000 ) ) ;
#87772 = CARTESIAN_POINT ( 'NONE',  ( -4.750186375023972118, -1.378107633083692329, 104.3180500829675026 ) ) ;
#87773 = ORIENTED_EDGE ( 'NONE', *, *, #33990, .T. ) ;
#87774 = VERTEX_POINT ( 'NONE', #71815 ) ;
#87775 = CARTESIAN_POINT ( 'NONE',  ( -24.24905399839806464, 305.2659941753802286, 10.24863818738177024 ) ) ;
#87776 = VERTEX_POINT ( 'NONE', #95579 ) ;
#87777 = CARTESIAN_POINT ( 'NONE',  ( 22.01171728258022853, 305.2737328247270625, 10.02785900982430256 ) ) ;
#87778 = CARTESIAN_POINT ( 'NONE',  ( 5.656854249492380582, -14.00000000409677092, -5.656854249492379694 ) ) ;
#87779 = ORIENTED_EDGE ( 'NONE', *, *, #70250, .T. ) ;
#87780 = CARTESIAN_POINT ( 'NONE',  ( -5.625019081819781164, 41.66287055468434630, -70.61600276915974916 ) ) ;
#87781 = AXIS2_PLACEMENT_3D ( 'NONE', #82845, #820, #66666 ) ;
#87782 = CARTESIAN_POINT ( 'NONE',  ( -86.26287741613369064, -59.99999999999507594, 203.3882217285910201 ) ) ;
#87783 = CARTESIAN_POINT ( 'NONE',  ( 45.99999999999428013, 486.0809427139465697, 1.692663251875475394 ) ) ;
#87784 = AXIS2_PLACEMENT_3D ( 'NONE', #95289, #47241, #63995 ) ;
#87785 = CARTESIAN_POINT ( 'NONE',  ( 74.21466443961692505, -60.00000000000000000, 174.3944259474788510 ) ) ;
#87786 = CARTESIAN_POINT ( 'NONE',  ( -10.00000000000000355, 30.00000000000000000, 0.000000000000000000 ) ) ;
#87787 = DIRECTION ( 'NONE',  ( 0.000000000000000000, -1.000000000000000000, 0.000000000000000000 ) ) ;
#87789 = CARTESIAN_POINT ( 'NONE',  ( 8.111369670363336226, -32.51052359539890801, 29.30105919468876152 ) ) ;
#87788 = CARTESIAN_POINT ( 'NONE',  ( -110.8742113967375928, -60.00000000000001421, 132.3764718065442594 ) ) ;
#87790 = DIRECTION ( 'NONE',  ( 1.000000000000000000, 0.000000000000000000, 0.000000000000000000 ) ) ;
#87791 = ADVANCED_FACE ( 'NONE', ( #86451 ), #4976, .F. ) ;
#87792 = CARTESIAN_POINT ( 'NONE',  ( -45.59210809638418027, -46.44287893288203151, 46.30682524688919699 ) ) ;
#87793 = CARTESIAN_POINT ( 'NONE',  ( -0.000000000000000000, 0.000000000000000000, -5.000000000000000000 ) ) ;
#87794 = ORIENTED_EDGE ( 'NONE', *, *, #102067, .T. ) ;
#87795 = CARTESIAN_POINT ( 'NONE',  ( 41.31850805822517714, 460.1795573263356118, 2.184907985913608908 ) ) ;
#87796 = CARTESIAN_POINT ( 'NONE',  ( 17.51117938516244976, 36.87948859581990035, 22.05134542098255324 ) ) ;
#87797 = CONICAL_SURFACE ( 'NONE', #80839, 4.000000000000001776, 0.9599310885968808105 ) ;
#87798 = EDGE_CURVE ( 'NONE', #52756, #38536, #104716, .T. ) ;
#87799 = CARTESIAN_POINT ( 'NONE',  ( 26.08349330513380693, 4.898587196589411843E-16, -4.000000000000001776 ) ) ;
#87800 = ORIENTED_EDGE ( 'NONE', *, *, #42074, .T. ) ;
#87801 = CARTESIAN_POINT ( 'NONE',  ( -12.00539508356256491, -6.854840103463671674, 19.79463260135151614 ) ) ;
#87802 = B_SPLINE_CURVE_WITH_KNOTS ( 'NONE', 3,
 ( #89112, #72901, #15208, #90706, #105290, #8711, #82060, #64314, #48096, #16815, #31951, #97711, #89642, #7631 ),
 .UNSPECIFIED., .F., .F.,
 ( 4, 2, 2, 2, 2, 2, 4 ),
 ( 7.410741937918042371E-18, 0.002039551581737956108, 0.003059327372606909443, 0.004079103163475863644, 0.006118654745213768578, 0.007138430536082721913, 0.008158206326951673512 ),
 .UNSPECIFIED. ) ;
#87803 = ORIENTED_EDGE ( 'NONE', *, *, #29467, .T. ) ;
#87804 = CARTESIAN_POINT ( 'NONE',  ( 80.99227329964719502, -29.99999999995507238, 192.5733771533335812 ) ) ;
#87805 = CARTESIAN_POINT ( 'NONE',  ( 13.09999999999999787, 1.533819458162526451E-15, 0.000000000000000000 ) ) ;
#87806 = DIRECTION ( 'NONE',  ( 0.000000000000000000, -1.000000000000000000, 0.000000000000000000 ) ) ;
#87807 =( NAMED_UNIT ( * ) PLANE_ANGLE_UNIT ( ) SI_UNIT ( $, .RADIAN. ) );
#87808 = CARTESIAN_POINT ( 'NONE',  ( 99.00617620828374754, -29.99999999999999645, 188.8169106426751966 ) ) ;
#87809 = AXIS2_PLACEMENT_3D ( 'NONE', #29081, #36624, #11757 ) ;
#87810 = CARTESIAN_POINT ( 'NONE',  ( -9.938519914450460599E-16, 0.3912769056150340874, 7.999999999999998224 ) ) ;
#87811 = ORIENTED_EDGE ( 'NONE', *, *, #17543, .T. ) ;
#87813 = B_SPLINE_CURVE_WITH_KNOTS ( 'NONE', 3,
 ( #29865, #13632, #79441, #88081, #104243, #63276, #96176, #55151, #65389, #32517, #33049, #48649, #57271, #97733, #98795, #58356, #41643, #74527, #9257, #42167, #75050, #65916, #1146, #81533, #7658, #40577, #34121, #89668, #89134, #90729, #82085, #79, #97210, #23360, #73996, #8203 ),
 .UNSPECIFIED., .F., .F.,
 ( 4, 2, 2, 2, 2, 2, 2, 2, 2, 2, 2, 2, 2, 2, 2, 2, 2, 4 ),
 ( 0.01291936762762758983, 0.01372441420841339667, 0.01452946078919920350, 0.01533450736998501034, 0.01613955395077081717, 0.01694460053155662227, 0.01774964711234243084, 0.01855469369312823594, 0.01935974027391404451, 0.02016478685469984961, 0.02096983343548565470, 0.02177488001627146327, 0.02257992659705727184, 0.02338497317784307694, 0.02419001975862888204, 0.02459254304902178806, 0.02499506633941468714, 0.02580011292020053387 ),
 .UNSPECIFIED. ) ;
#87812 = AXIS2_PLACEMENT_3D ( 'NONE', #13138, #46067, #96218 ) ;
#87814 = ORIENTED_EDGE ( 'NONE', *, *, #10407, .F. ) ;
#87815 = ORIENTED_EDGE ( 'NONE', *, *, #52061, .F. ) ;
#87816 = CARTESIAN_POINT ( 'NONE',  ( -27.26366621554978309, 36.83106128561345827, 7.556984339686017904 ) ) ;
#87817 = DIRECTION ( 'NONE',  ( -0.5735764363510512664, 0.8191520442889881348, 1.003171929053520309E-16 ) ) ;
#87818 = CARTESIAN_POINT ( 'NONE',  ( 11.82165952410163356, 294.5900423753296309, -10.05563889079273210 ) ) ;
#87819 = EDGE_LOOP ( 'NONE', ( #41499, #97017, #53162, #13642 ) ) ;
#87820 = LINE ( 'NONE', #105060, #68406 ) ;
#87821 = CONICAL_SURFACE ( 'NONE', #10342, 8.000000000000000000, 1.047197551196600296 ) ;
#87822 = ORIENTED_EDGE ( 'NONE', *, *, #21536, .T. ) ;
#87823 = LINE ( 'NONE', #81289, #70739 ) ;
#87824 = CARTESIAN_POINT ( 'NONE',  ( 105.8687044990643500, -38.37890680998027904, 196.5118811510903640 ) ) ;
#87825 = CARTESIAN_POINT ( 'NONE',  ( 12.11348346901124273, 7.908161531528928201, 8.621634460951579371 ) ) ;
#87826 = CARTESIAN_POINT ( 'NONE',  ( 87.01625201393999021, -60.20567772451860122, -8.192381583340527129 ) ) ;
#87827 = CARTESIAN_POINT ( 'NONE',  ( -1.112596765064915338, -50.00000000000000711, 101.1535177161686647 ) ) ;
#87828 = CARTESIAN_POINT ( 'NONE',  ( 36.34158003242083623, 308.9628109182459639, 13.30132686757931459 ) ) ;
#87829 = CARTESIAN_POINT ( 'NONE',  ( -1.469576158976823947E-15, -25.06250000409677270, 8.000000000000000000 ) ) ;
#87830 = CIRCLE ( 'NONE', #49916, 1.000000000000000888 ) ;
#87831 = DIRECTION ( 'NONE',  ( -0.000000000000000000, -0.000000000000000000, -1.000000000000000000 ) ) ;
#87832 = CARTESIAN_POINT ( 'NONE',  ( -39.82070819426019170, 460.7076632888579866, 2.105638695486015344 ) ) ;
#87833 = VERTEX_POINT ( 'NONE', #86970 ) ;
#87834 = DIRECTION ( 'NONE',  ( 0.000000000000000000, 0.000000000000000000, 1.000000000000000000 ) ) ;
#87835 = CARTESIAN_POINT ( 'NONE',  ( -37.85256771641471829, 460.2291302834033218, 2.227843630145174725 ) ) ;
#87836 = CARTESIAN_POINT ( 'NONE',  ( -2.880896649345847216, 62.46336717673360539, 4.999999999999999112 ) ) ;
#87837 = EDGE_LOOP ( 'NONE', ( #44967, #92049, #62476, #86567 ) ) ;
#87838 = DIRECTION ( 'NONE',  ( -0.000000000000000000, -0.000000000000000000, -1.000000000000000000 ) ) ;
#87839 = CARTESIAN_POINT ( 'NONE',  ( -32.36878476726423060, 299.8745122917198387, 3.062535334108964946 ) ) ;
#87840 = DIRECTION ( 'NONE',  ( 1.000000000000000000, 0.000000000000000000, 0.000000000000000000 ) ) ;
#87841 = CARTESIAN_POINT ( 'NONE',  ( -12.13034742782428133, 42.00000299511174973, -93.82352941176471006 ) ) ;
#87842 = CARTESIAN_POINT ( 'NONE',  ( -5.656854249492379694, -14.93749999999999289, -5.656854249492380582 ) ) ;
#87843 = CARTESIAN_POINT ( 'NONE',  ( 43.54313159148357926, -29.68436378173572265, 52.44550087950238293 ) ) ;
#87844 = CONICAL_SURFACE ( 'NONE', #49932, 8.605212085995399107, 1.221730476396037490 ) ;
#87845 = ADVANCED_FACE ( 'NONE', ( #78846 ), #39048, .T. ) ;
#87846 = LINE ( 'NONE', #102428, #89735 ) ;
#87847 = ORIENTED_EDGE ( 'NONE', *, *, #18572, .F. ) ;
#87848 = CARTESIAN_POINT ( 'NONE',  ( 83.13947484406011768, -60.93864057100361009, 190.8861806389487867 ) ) ;
#87849 = CARTESIAN_POINT ( 'NONE',  ( -48.48335035450828201, 8.813057796081508855, 16.77177117249955174 ) ) ;
#87850 = CARTESIAN_POINT ( 'NONE',  ( 3.454253436624936668, -0.8414180287960456583, 103.7259032015043232 ) ) ;
#87851 = ORIENTED_EDGE ( 'NONE', *, *, #105370, .T. ) ;
#87852 = CARTESIAN_POINT ( 'NONE',  ( 95.57416616939285348, -57.67170004321813082, 37.82161414657011989 ) ) ;
#87853 = DIRECTION ( 'NONE',  ( -0.000000000000000000, -0.000000000000000000, -1.000000000000000000 ) ) ;
#87854 = CARTESIAN_POINT ( 'NONE',  ( 6.231493956936422940, 4.173545622688802581, 5.000000000000000000 ) ) ;
#87855 = ADVANCED_FACE ( 'NONE', ( #1080 ), #101092, .F. ) ;
#87856 = CARTESIAN_POINT ( 'NONE',  ( -9.288740593950837621, -22.45067348962094300, -38.54328090126934114 ) ) ;
#87857 = ADVANCED_FACE ( 'NONE', ( #59376 ), #84171, .T. ) ;
#87858 = CIRCLE ( 'NONE', #20776, 57.50357696970299770 ) ;
#87859 = CYLINDRICAL_SURFACE ( 'NONE', #14023, 5.000000000000002665 ) ;
#87860 = CARTESIAN_POINT ( 'NONE',  ( 8.922269033012840467, -5.000000000000000000, 5.219866590718108768 ) ) ;
#87861 = CARTESIAN_POINT ( 'NONE',  ( 51.04048647703990582, -29.85962867422984246, 48.35404991630245775 ) ) ;
#87864 = CARTESIAN_POINT ( 'NONE',  ( -12.92250098416157478, 4.492494496599526599, 7.510829452561845976 ) ) ;
#87863 = AXIS2_PLACEMENT_3D ( 'NONE', #76976, #71010, #96369 ) ;
#87862 = DIRECTION ( 'NONE',  ( 1.000000000000000000, -0.000000000000000000, -0.000000000000000000 ) ) ;
#87865 =( NAMED_UNIT ( * ) SI_UNIT ( $, .STERADIAN. ) SOLID_ANGLE_UNIT ( ) );
#87866 = FILL_AREA_STYLE_COLOUR ( '', #92839 ) ;
#87867 = DIRECTION ( 'NONE',  ( -0.000000000000000000, 1.000000000000000000, -0.000000000000000000 ) ) ;
#87868 = CARTESIAN_POINT ( 'NONE',  ( -4.463429423125057305, 13.01149508916975428, -12.86120860535742239 ) ) ;
#87869 = CARTESIAN_POINT ( 'NONE',  ( -102.8125839197916775, -37.99999999999999289, 170.8447077551169002 ) ) ;
#87870 = AXIS2_PLACEMENT_3D ( 'NONE', #15099, #80893, #84505 ) ;
#87871 = VERTEX_POINT ( 'NONE', #38299 ) ;
#87872 = CARTESIAN_POINT ( 'NONE',  ( -8.503038991956803017, 2.981673336380457950, 14.70105501402611381 ) ) ;
#87873 =( LENGTH_UNIT ( ) NAMED_UNIT ( * ) SI_UNIT ( .MILLI., .METRE. ) );
#87874 = DIRECTION ( 'NONE',  ( 0.000000000000000000, 0.000000000000000000, 1.000000000000000000 ) ) ;
#87875 = CIRCLE ( 'NONE', #58630, 1.999999999999998890 ) ;
#87877 = CARTESIAN_POINT ( 'NONE',  ( -47.71675376065731200, -47.40886959700829806, -30.35352467222949358 ) ) ;
#87876 =( LENGTH_UNIT ( ) NAMED_UNIT ( * ) SI_UNIT ( .MILLI., .METRE. ) );
#87878 = B_SPLINE_CURVE_WITH_KNOTS ( 'NONE', 3,
 ( #83787, #57382, #49830, #90295, #9899, #42807, #42267, #75160 ),
 .UNSPECIFIED., .F., .F.,
 ( 4, 2, 2, 4 ),
 ( 0.007886720825438833446, 0.009850969036564032402, 0.01181521724768922962, 0.01574371366993962754 ),
 .UNSPECIFIED. ) ;
#87879 = VERTEX_POINT ( 'NONE', #5380 ) ;
#87880 = CIRCLE ( 'NONE', #51675, 4.172000000000001485 ) ;
#87881 = CARTESIAN_POINT ( 'NONE',  ( 3.080866544135465013, 6.881514909250465273, -7.026396753507434312 ) ) ;
#87882 = VERTEX_POINT ( 'NONE', #95983 ) ;
#87883 = ADVANCED_FACE ( 'NONE', ( #3788 ), #38805, .T. ) ;
#87884 = DIRECTION ( 'NONE',  ( -0.8191520442889884679, 1.003171929053520679E-16, 0.5735764363510509334 ) ) ;
#87885 = AXIS2_PLACEMENT_3D ( 'NONE', #101497, #100421, #17403 ) ;
#87886 = DIRECTION ( 'NONE',  ( -1.000000000000000000, -1.224606353822377258E-16, -0.000000000000000000 ) ) ;
#87887 = CARTESIAN_POINT ( 'NONE',  ( -92.53668747331201416, -60.00000000000000711, -1.795014215929801260 ) ) ;
#87888 = ORIENTED_EDGE ( 'NONE', *, *, #15775, .F. ) ;
#87889 = CARTESIAN_POINT ( 'NONE',  ( 0.000000000000000000, 0.000000000000000000, -4.289342857142857568 ) ) ;
#87890 = CARTESIAN_POINT ( 'NONE',  ( 45.36923076923077502, 4.172000000000003261, 0.000000000000000000 ) ) ;
#87891 = CARTESIAN_POINT ( 'NONE',  ( 21.19348424345033521, 294.8901562694577478, 1.945151701991110205 ) ) ;
#87893 = FACE_OUTER_BOUND ( 'NONE', #38303, .T. ) ;
#87892 = DIRECTION ( 'NONE',  ( -0.000000000000000000, 1.000000000000000000, -0.000000000000000000 ) ) ;
#87894 = CARTESIAN_POINT ( 'NONE',  ( -79.61189064004022953, -56.85762575183416345, 165.3701725720323736 ) ) ;
#87895 = ORIENTED_EDGE ( 'NONE', *, *, #64455, .T. ) ;
#87896 = CARTESIAN_POINT ( 'NONE',  ( -39.95753117817366729, 490.6049172992401850, 11.69497456421621528 ) ) ;
#87897 = ORIENTED_EDGE ( 'NONE', *, *, #60293, .F. ) ;
#87898 = ORIENTED_EDGE ( 'NONE', *, *, #46622, .T. ) ;
#87899 = CARTESIAN_POINT ( 'NONE',  ( 14.22021666642421955, -5.000000000000000000, 8.714242330525232560 ) ) ;
#87900 = EDGE_CURVE ( 'NONE', #3711, #70143, #30870, .T. ) ;
#87901 = SURFACE_STYLE_FILL_AREA ( #71170 ) ;
#87902 = DIRECTION ( 'NONE',  ( 0.000000000000000000, 1.000000000000000000, 0.000000000000000000 ) ) ;
#87903 = ORIENTED_EDGE ( 'NONE', *, *, #50182, .F. ) ;
#87904 = CARTESIAN_POINT ( 'NONE',  ( 15.39709502357282922, 46.16515237750017775, -5.602001606816853219 ) ) ;
#87905 =( NAMED_UNIT ( * ) PLANE_ANGLE_UNIT ( ) SI_UNIT ( $, .RADIAN. ) );
#87906 = CARTESIAN_POINT ( 'NONE',  ( -80.15954706948889452, -57.50857130571672826, 199.0044224626226139 ) ) ;
#87907 = CARTESIAN_POINT ( 'NONE',  ( 0.3157512944460784676, -3.097794232780207491, 8.000000000000000000 ) ) ;
#87908 = DIRECTION ( 'NONE',  ( -0.000000000000000000, 1.000000000000000000, -0.000000000000000000 ) ) ;
#87909 = FACE_OUTER_BOUND ( 'NONE', #27703, .T. ) ;
#87910 = CARTESIAN_POINT ( 'NONE',  ( -17.08493112194819830, 36.32471929476455585, -24.27338705487295201 ) ) ;
#87911 = CARTESIAN_POINT ( 'NONE',  ( 86.58362542449755495, -60.00000000000002132, -26.27920600484676683 ) ) ;
#87912 = CARTESIAN_POINT ( 'NONE',  ( -48.81109529425772564, -14.21045842199442788, 55.84243332122913017 ) ) ;
#87913 = CARTESIAN_POINT ( 'NONE',  ( -54.79799674529369469, -49.91194600308500640, 64.09558544181255968 ) ) ;
#87914 = COLOUR_RGB ( '', 0.08235294, 0.09019608, 0.10196078) ;
#87915 = ORIENTED_EDGE ( 'NONE', *, *, #16250, .F. ) ;
#87916 = CARTESIAN_POINT ( 'NONE',  ( 6.770546484616568605, 16.58436325196198879, -1.794795801736670748 ) ) ;
#87917 = ORIENTED_EDGE ( 'NONE', *, *, #78742, .F. ) ;
#87918 = CARTESIAN_POINT ( 'NONE',  ( -102.3353922011937556, -60.19607622334896035, 193.7979307818540349 ) ) ;
#87919 = APPLICATION_CONTEXT ( 'automotive_design' ) ;
#87920 = CARTESIAN_POINT ( 'NONE',  ( 30.11650669486618881, 1.474610560812782335E-15, 0.000000000000000000 ) ) ;
#87921 = EDGE_CURVE ( 'NONE', #34061, #32906, #71678, .T. ) ;
#87922 = ORIENTED_EDGE ( 'NONE', *, *, #86906, .F. ) ;
#87923 = CARTESIAN_POINT ( 'NONE',  ( 19.45330446674461911, 49.97940989288292002, 60.59551982431160866 ) ) ;
#87924 = CARTESIAN_POINT ( 'NONE',  ( 88.11249734486904117, -38.37137927187098541, -19.43261626278027521 ) ) ;
#87925 = PRESENTATION_STYLE_ASSIGNMENT (( #104089 ) ) ;
#87926 = CARTESIAN_POINT ( 'NONE',  ( -10.00000000000000355, 30.00000000000000000, -4.000000000000000000 ) ) ;
#87927 = CARTESIAN_POINT ( 'NONE',  ( -5.290067270632216712, 52.08006895350504095, 6.031152949374556371 ) ) ;
#87928 = CARTESIAN_POINT ( 'NONE',  ( -40.61216075948964033, 351.1469683695276558, 22.89433108575548914 ) ) ;
#87929 = EDGE_CURVE ( 'NONE', #100942, #100925, #24103, .T. ) ;
#87930 = CARTESIAN_POINT ( 'NONE',  ( 0.000000000000000000, 1.502314598737160412E-15, 6.500000000000000888 ) ) ;
#87931 = CARTESIAN_POINT ( 'NONE',  ( 37.06438722625302518, 1.482358050883964840E-15, 0.000000000000000000 ) ) ;
#87932 = DIRECTION ( 'NONE',  ( 0.000000000000000000, 0.000000000000000000, 1.000000000000000000 ) ) ;
#87933 = UNCERTAINTY_MEASURE_WITH_UNIT (LENGTH_MEASURE( 1.000000000000000082E-05 ), #29028, 'distance_accuracy_value', 'NONE');
#87934 = CARTESIAN_POINT ( 'NONE',  ( -27.64215802503290575, -32.53081356062803309, 31.18544280887772757 ) ) ;
#87935 = TOROIDAL_SURFACE ( 'NONE', #12157, 12.00000000000000711, 3.000000000000000000 ) ;
#87936 = ORIENTED_EDGE ( 'NONE', *, *, #84117, .F. ) ;
#87937 = ORIENTED_EDGE ( 'NONE', *, *, #37238, .T. ) ;
#87938 = CARTESIAN_POINT ( 'NONE',  ( 48.77471784688194134, -32.59704705468854513, 46.61485220210019520 ) ) ;
#87939 = CARTESIAN_POINT ( 'NONE',  ( -0.8340752422583500580, 12.93528688290565043, 49.56574184153335239 ) ) ;
#87940 = MANIFOLD_SOLID_BREP ( 'Fillet1', #103219 ) ;
#87941 = CARTESIAN_POINT ( 'NONE',  ( -6.969759372139044729, 16.94689987907234041, -0.6630323575263610270 ) ) ;
#87942 = CARTESIAN_POINT ( 'NONE',  ( -104.5350828174626798, -38.40247479459341662, 197.9350992758817540 ) ) ;
#87943 = ORIENTED_EDGE ( 'NONE', *, *, #94030, .F. ) ;
#87944 = CARTESIAN_POINT ( 'NONE',  ( 91.38818257286023083, -38.39638879886640410, -9.329338805212154639 ) ) ;
#87945 = CARTESIAN_POINT ( 'NONE',  ( 11.01150283225517157, 16.91336324511702571, -9.209782235539176298 ) ) ;
#87946 = CARTESIAN_POINT ( 'NONE',  ( -19.44925841602305283, 49.97667730683129861, 60.63295307910983922 ) ) ;
#87947 = DIRECTION ( 'NONE',  ( 0.000000000000000000, 1.000000000000000000, 0.000000000000000000 ) ) ;
#87948 = CARTESIAN_POINT ( 'NONE',  ( 38.86638200451619696, 6.123233995736770227E-16, -5.000000000000002665 ) ) ;
#87949 = DIRECTION ( 'NONE',  ( -1.000000000000000000, 0.000000000000000000, 0.000000000000000000 ) ) ;
#87950 = CARTESIAN_POINT ( 'NONE',  ( 22.80797863425486938, 28.18718824344973584, 30.77216081686022875 ) ) ;
#87951 = CARTESIAN_POINT ( 'NONE',  ( -35.67189472734460054, 438.4023653113565047, 3.943223222944094886 ) ) ;
#87952 = CARTESIAN_POINT ( 'NONE',  ( 0.000000000000000000, -5.629165124598843661, 3.250000000000012879 ) ) ;
#87953 = CARTESIAN_POINT ( 'NONE',  ( 12.49955057316562090, -4.332870170068738425, -12.71907580248059233 ) ) ;
#87954 = CARTESIAN_POINT ( 'NONE',  ( 93.39948790556088909, -59.99999999999999289, 202.5047245700688450 ) ) ;
#87955 = EDGE_CURVE ( 'NONE', #8366, #76134, #52570, .T. ) ;
#87956 = CIRCLE ( 'NONE', #56897, 5.000000000000010658 ) ;
#87957 = DIRECTION ( 'NONE',  ( -1.000000000000000000, -0.000000000000000000, -0.000000000000000000 ) ) ;
#87958 = CIRCLE ( 'NONE', #75930, 4.000000000000001776 ) ;
#87959 = ORIENTED_EDGE ( 'NONE', *, *, #63182, .F. ) ;
#87960 = CARTESIAN_POINT ( 'NONE',  ( 58.40048366602277952, -36.01844938180519762, 66.61435485081292995 ) ) ;
#87961 = CARTESIAN_POINT ( 'NONE',  ( -27.28250412859145868, 305.2104144000636552, -9.479816361705919903 ) ) ;
#87962 = CARTESIAN_POINT ( 'NONE',  ( 7.619135598915494967, 33.17305367784678083, 2.449260492474801154 ) ) ;
#87963 = CARTESIAN_POINT ( 'NONE',  ( -7.002990960197232440, 28.94733181616541984, 3.868040364119522678 ) ) ;
#87964 = VERTEX_POINT ( 'NONE', #45315 ) ;
#87965 = CONICAL_SURFACE ( 'NONE', #79325, 15.00000000000000000, 0.7509290623979402168 ) ;
#87967 = CARTESIAN_POINT ( 'NONE',  ( -9.423772032809306864, -51.98692372519796834, 23.65101655106710510 ) ) ;
#87966 = CARTESIAN_POINT ( 'NONE',  ( -105.0601071971127993, -38.35601112544424751, 118.3067828870811553 ) ) ;
#87968 = CYLINDRICAL_SURFACE ( 'NONE', #8134, 15.00000000000000711 ) ;
#87969 = CARTESIAN_POINT ( 'NONE',  ( 30.50103796836107861, 337.4180749914852981, 16.76525021871696097 ) ) ;
#87970 = LINE ( 'NONE', #38887, #54070 ) ;
#87971 = CARTESIAN_POINT ( 'NONE',  ( 5.656854249492380582, -30.31249999999999645, -5.656854249492379694 ) ) ;
#87972 = CARTESIAN_POINT ( 'NONE',  ( -1.308996937480702005, -3.000000000000002665, -95.00000000000000000 ) ) ;
#87973 = AXIS2_PLACEMENT_3D ( 'NONE', #25382, #83056, #76015 ) ;
#87974 = CARTESIAN_POINT ( 'NONE',  ( 19.83349330513379982, 1.593028355512270567E-15, 0.000000000000000000 ) ) ;
#87975 = ORIENTED_EDGE ( 'NONE', *, *, #105179, .T. ) ;
#87976 = CARTESIAN_POINT ( 'NONE',  ( 82.07540746790368758, -53.52673662087732964, 181.8248042487631437 ) ) ;
#87977 = CARTESIAN_POINT ( 'NONE',  ( 8.427920798850724537, 123.5502821094338941, 0.000000000000000000 ) ) ;
#87978 = B_SPLINE_CURVE_WITH_KNOTS ( 'NONE', 3,
 ( #5009, #54058, #46002, #39508, #87002, #104215, #72382, #79417 ),
 .UNSPECIFIED., .F., .F.,
 ( 4, 2, 2, 4 ),
 ( 0.007886720825438776200, 0.009850969036563999442, 0.01181521724768922268, 0.01574371366993966917 ),
 .UNSPECIFIED. ) ;
#87979 = CARTESIAN_POINT ( 'NONE',  ( -33.65893543312866143, 439.0634705965974263, 24.00849711452648805 ) ) ;
#87980 = ORIENTED_EDGE ( 'NONE', *, *, #53413, .F. ) ;
#87981 = CARTESIAN_POINT ( 'NONE',  ( -37.66149909514062699, 377.9508026867375179, 5.097312388780781411 ) ) ;
#87982 = CARTESIAN_POINT ( 'NONE',  ( 5.692357205178650403, -4.313020517866006820, -16.93296622886375147 ) ) ;
#87983 = CARTESIAN_POINT ( 'NONE',  ( 3.250000000000015099, 5.629165124598843661, 1.734723475976807094E-15 ) ) ;
#87984 = CARTESIAN_POINT ( 'NONE',  ( -26.92780252270988939, 43.51495311933407351, -73.48039199225773643 ) ) ;
#87985 = DIRECTION ( 'NONE',  ( 0.06744659395731267271, 0.6445107564549666934, 0.7616146281272467844 ) ) ;
#87986 = EDGE_CURVE ( 'NONE', #6442, #85478, #63082, .T. ) ;
#87987 = ORIENTED_EDGE ( 'NONE', *, *, #88113, .F. ) ;
#87988 = CARTESIAN_POINT ( 'NONE',  ( -81.02915809513567069, -30.00000000000000355, 21.48644426250730533 ) ) ;
#87989 = CIRCLE ( 'NONE', #46712, 8.000000000000000000 ) ;
#87990 = EDGE_CURVE ( 'NONE', #82451, #68326, #73258, .T. ) ;
#87991 = CARTESIAN_POINT ( 'NONE',  ( -1.000000000000000000, -15.67301612170368053, -10.31008658363377251 ) ) ;
#87992 = CARTESIAN_POINT ( 'NONE',  ( 14.38372150811336425, 21.54773996110925083, -5.213918010984154527 ) ) ;
#87994 = CARTESIAN_POINT ( 'NONE',  ( -11.80829252637672511, 6.727529389947712879, -9.058755809531316316 ) ) ;
#87993 = CARTESIAN_POINT ( 'NONE',  ( -3.554850123176898080, -18.30354541650124389, 35.04484280488642156 ) ) ;
#87995 = AXIS2_PLACEMENT_3D ( 'NONE', #80642, #96332, #105464 ) ;
#87996 = CARTESIAN_POINT ( 'NONE',  ( 5.082755093536324154, -22.34375000204838457, 5.082755093536326818 ) ) ;
#87997 = CARTESIAN_POINT ( 'NONE',  ( -64.91565662652770641, 40.83906611473043569, 6.815324757234163755 ) ) ;
#87998 = LINE ( 'NONE', #38917, #3527 ) ;
#87999 = VERTEX_POINT ( 'NONE', #13973 ) ;
#88000 = DIRECTION ( 'NONE',  ( -0.000000000000000000, -0.000000000000000000, -1.000000000000000000 ) ) ;
#88001 = CARTESIAN_POINT ( 'NONE',  ( -8.066622878784276196, 44.48464632161616805, -5.000000000000000888 ) ) ;
#88002 =( BOUNDED_SURFACE ( )  B_SPLINE_SURFACE ( 3, 2, ( 
 ( #22185, #67926, #99757 ),
 ( #67409, #41521, #33454 ),
 ( #58785, #66329, #25928 ),
 ( #83564, #34535, #58233 ),
 ( #16719, #1021, #43123 ),
 ( #18336, #34001, #50646 ),
 ( #51191, #84111, #90610 ),
 ( #91680, #91162, #17796 ),
 ( #10210, #100811, #49067 ),
 ( #16181, #26972, #100285 ),
 ( #50140, #76008, #99212 ),
 ( #25376, #57687, #92186 ),
 ( #2108, #90074, #66871 ),
 ( #24833, #35058, #42579 ),
 ( #81962, #9666, #17267 ),
 ( #26447, #49608, #8088 ),
 ( #59314, #75479, #1572 ),
 ( #40994, #73882, #106777 ),
 ( #32928, #74408, #82515 ),
 ( #8618, #65802, #74935 ),
 ( #98679, #485, #83048 ),
 ( #9140, #42051, #60392 ),
 ( #86262, #20505, #45261 ),
 ( #19959, #93802, #101883 ),
 ( #44191, #85175, #92727 ),
 ( #12335, #77079, #27515 ),
 ( #102423, #37731, #85727 ),
 ( #21021, #69008, #11260 ),
 ( #3736, #36666, #53861 ),
 ( #94343, #11799, #78139 ),
 ( #4260, #84648, #44731 ),
 ( #53342, #37189, #28043 ),
 ( #93269, #77619, #12861 ),
 ( #94881, #69531, #70051 ),
 ( #86790, #45779, #19431 ),
 ( #28564, #60915, #102957 ),
 ( #78653, #70590, #18886 ),
 ( #51731, #103481, #29121 ),
 ( #52801, #4791, #61448 ),
 ( #61989, #59856, #10732 ),
 ( #43647, #76536, #2647 ),
 ( #101362, #35594, #68471 ),
 ( #52261, #3196, #36139 ),
 ( #22055, #5326, #31737 ),
 ( #15521, #105593, #64623 ),
 ( #13921, #14447, #23119 ),
 ( #38248, #47360, #30687 ),
 ( #5837, #48413, #39296 ),
 ( #64106, #63574, #46832 ),
 ( #30147, #79203, #55438 ),
 ( #54364, #7418, #72175 ),
 ( #88372, #88892, #87307 ),
 ( #105082, #38762, #31222 ),
 ( #55960, #80786, #104532 ),
 ( #63031, #80248, #89431 ),
 ( #97489, #6354, #96984 ),
 ( #23646, #56501, #95928 ),
 ( #71111, #103999, #81305 ),
 ( #87839, #14984, #47879 ),
 ( #71629, #40333, #96466 ),
 ( #22601, #73215, #6899 ),
 ( #29630, #39820, #54913 ),
 ( #46312, #62505, #79732 ),
 ( #13391, #72697, #95392 ),
 ( #21532, #91560, #106111 ),
 ( #98560, #81830, #1449 ),
 ( #92070, #75347, #34412 ),
 ( #90483, #91035, #99628 ),
 ( #7956, #17139, #363 ),
 ( #89948, #106652, #18213 ),
 ( #98038, #42456, #16590 ),
 ( #33332, #41396, #9547 ),
 ( #25805, #74809, #67284 ),
 ( #32803, #58658, #66200 ),
 ( #24710, #82385, #100164 ),
 ( #32262, #17667, #66740 ),
 ( #99085, #25248, #58102 ),
 ( #26332, #49479, #57557 ),
 ( #8492, #50533, #74286 ),
 ( #65675, #48937, #50015 ),
 ( #24188, #83981, #9017 ),
 ( #82919, #83445, #57034 ) ),
 .UNSPECIFIED., .F., .F., .T. ) 
 B_SPLINE_SURFACE_WITH_KNOTS ( ( 4, 2, 2, 2, 2, 2, 2, 2, 2, 2, 2, 2, 2, 2, 2, 2, 2, 2, 2, 2, 2, 2, 2, 2, 2, 2, 2, 2, 2, 2, 2, 2, 2, 2, 2, 2, 2, 2, 2, 2, 4 ),
 ( 3, 3 ),
 ( 0.05188019136508568302, 0.06984908127900800456, 0.07883352623596917574, 0.08781797119293033305, 0.1057868611068526477, 0.1147713060638138050, 0.1237557510207749761, 0.1417246409346973046, 0.1507090858916584619, 0.1596935308486196192, 0.1619396420878599363, 0.1641857533271002256, 0.1686779758055808043, 0.1731701982840613829, 0.1754163095233016723, 0.1776624207625419616, 0.1787854763821621062, 0.1793470041919721925, 0.1799085320017822509, 0.1821546432410225402, 0.1844007544802628296, 0.1849622822900728880, 0.1852430461949779450, 0.1855238100998829742, 0.1866468657195031189, 0.1877699213391232635, 0.1879103032915757643, 0.1879804942678020285, 0.1880506852440282928, 0.1883314491489333498, 0.1888929769587434082, 0.1900160325783635529, 0.1902967964832685821, 0.1905775603881736391, 0.1911390881979836975, 0.1922621438176038422, 0.1928236716274139284, 0.1929640535798664569, 0.1931044355323189576, 0.1933851994372239869, 0.1956313106764642762 ),
 ( 0.000000000000000000, 1.000000000000000000 ),
 .UNSPECIFIED. ) 
 GEOMETRIC_REPRESENTATION_ITEM ( )  RATIONAL_B_SPLINE_SURFACE ( (
 ( 1.000000000000000000, 0.7071066915981665257, 1.000000000000000000),
 ( 1.000000000000000000, 0.7071066382886482815, 1.000000000000000000),
 ( 1.000000000000000000, 0.7071067819013748812, 1.000000000000000000),
 ( 1.000000000000000000, 0.7071067819013748812, 1.000000000000000000),
 ( 1.000000000000000000, 0.7071067881452209880, 1.000000000000000000),
 ( 1.000000000000000000, 0.7071067881452209880, 1.000000000000000000),
 ( 1.000000000000000000, 0.7071067820841906437, 1.000000000000000000),
 ( 1.000000000000000000, 0.7071067820841906437, 1.000000000000000000),
 ( 1.000000000000000000, 0.7071082744393792918, 1.000000000000000000),
 ( 1.000000000000000000, 0.7071090812208852272, 1.000000000000000000),
 ( 1.000000000000000000, 0.7071085750256929092, 1.000000000000000000),
 ( 1.000000000000000000, 0.7071071111271418630, 1.000000000000000000),
 ( 1.000000000000000000, 0.7071064681235214033, 1.000000000000000000),
 ( 1.000000000000000000, 0.7071084972331730389, 1.000000000000000000),
 ( 1.000000000000000000, 0.7071099221851442351, 1.000000000000000000),
 ( 1.000000000000000000, 0.7071070408053770073, 1.000000000000000000),
 ( 1.000000000000000000, 0.7071068064871738335, 1.000000000000000000),
 ( 1.000000000000000000, 0.7071095048012291384, 1.000000000000000000),
 ( 1.000000000000000000, 0.7071073154889575552, 1.000000000000000000),
 ( 1.000000000000000000, 0.7071067115369314982, 1.000000000000000000),
 ( 1.000000000000000000, 0.7071075951519679714, 1.000000000000000000),
 ( 1.000000000000000000, 0.7071139925282480254, 1.000000000000000000),
 ( 1.000000000000000000, 0.7071183661598045012, 1.000000000000000000),
 ( 1.000000000000000000, 0.7071289949713209788, 1.000000000000000000),
 ( 1.000000000000000000, 0.7071314560732923082, 1.000000000000000000),
 ( 1.000000000000000000, 0.7071209471556917370, 1.000000000000000000),
 ( 1.000000000000000000, 0.7071073686105321388, 1.000000000000000000),
 ( 1.000000000000000000, 0.7071065108360928830, 1.000000000000000000),
 ( 1.000000000000000000, 0.7071095461198974030, 1.000000000000000000),
 ( 1.000000000000000000, 0.7071118034369724414, 1.000000000000000000),
 ( 1.000000000000000000, 0.7071112127294267857, 1.000000000000000000),
 ( 1.000000000000000000, 0.7071089568612387577, 1.000000000000000000),
 ( 1.000000000000000000, 0.7071080543739914903, 1.000000000000000000),
 ( 1.000000000000000000, 0.7071071383726338366, 1.000000000000000000),
 ( 1.000000000000000000, 0.7071069085306952440, 1.000000000000000000),
 ( 1.000000000000000000, 0.7071067322179039882, 1.000000000000000000),
 ( 1.000000000000000000, 0.7071073362163841081, 1.000000000000000000),
 ( 1.000000000000000000, 0.7071285152900517179, 1.000000000000000000),
 ( 1.000000000000000000, 0.7071790023132530356, 1.000000000000000000),
 ( 1.000000000000000000, 0.7072040895942260930, 1.000000000000000000),
 ( 1.000000000000000000, 0.7071723949973123258, 1.000000000000000000),
 ( 1.000000000000000000, 0.7071267374085528079, 1.000000000000000000),
 ( 1.000000000000000000, 0.7071181237617968351, 1.000000000000000000),
 ( 1.000000000000000000, 0.7071098451417374697, 1.000000000000000000),
 ( 1.000000000000000000, 0.7071078748714980655, 1.000000000000000000),
 ( 1.000000000000000000, 0.7071063635215881771, 1.000000000000000000),
 ( 1.000000000000000000, 0.7071068237248464561, 1.000000000000000000),
 ( 1.000000000000000000, 0.7071083882213404781, 1.000000000000000000),
 ( 1.000000000000000000, 0.7071118710946099339, 1.000000000000000000),
 ( 1.000000000000000000, 0.7071122098397134570, 1.000000000000000000),
 ( 1.000000000000000000, 0.7071084160890762638, 1.000000000000000000),
 ( 1.000000000000000000, 0.7071068976071489542, 1.000000000000000000),
 ( 1.000000000000000000, 0.7071067909637599458, 1.000000000000000000),
 ( 1.000000000000000000, 0.7071067772271979468, 1.000000000000000000),
 ( 1.000000000000000000, 0.7071067571163546228, 1.000000000000000000),
 ( 1.000000000000000000, 0.7071066487236993270, 1.000000000000000000),
 ( 1.000000000000000000, 0.7071065680923671604, 1.000000000000000000),
 ( 1.000000000000000000, 0.7071060580930246253, 1.000000000000000000),
 ( 1.000000000000000000, 0.7071053146948335089, 1.000000000000000000),
 ( 1.000000000000000000, 0.7071028930956892999, 1.000000000000000000),
 ( 1.000000000000000000, 0.7071011043164672216, 1.000000000000000000),
 ( 1.000000000000000000, 0.7070987825526636739, 1.000000000000000000),
 ( 1.000000000000000000, 0.7071026651449159317, 1.000000000000000000),
 ( 1.000000000000000000, 0.7071061651848329355, 1.000000000000000000),
 ( 1.000000000000000000, 0.7071066975805828658, 1.000000000000000000),
 ( 1.000000000000000000, 0.7071068470435215580, 1.000000000000000000),
 ( 1.000000000000000000, 0.7071077911912049263, 1.000000000000000000),
 ( 1.000000000000000000, 0.7071127756005890497, 1.000000000000000000),
 ( 1.000000000000000000, 0.7071176452039118487, 1.000000000000000000),
 ( 1.000000000000000000, 0.7071257956655977450, 1.000000000000000000),
 ( 1.000000000000000000, 0.7071209011550627643, 1.000000000000000000),
 ( 1.000000000000000000, 0.7071103648264748243, 1.000000000000000000),
 ( 1.000000000000000000, 0.7071068888656230067, 1.000000000000000000),
 ( 1.000000000000000000, 0.7071067572802584023, 1.000000000000000000),
 ( 1.000000000000000000, 0.7071071039850833628, 1.000000000000000000),
 ( 1.000000000000000000, 0.7071084011956232374, 1.000000000000000000),
 ( 1.000000000000000000, 0.7071093283064042723, 1.000000000000000000),
 ( 1.000000000000000000, 0.7071125871578549660, 1.000000000000000000),
 ( 1.000000000000000000, 0.7071153771953387901, 1.000000000000000000),
 ( 1.000000000000000000, 0.7071397769056843030, 1.000000000000000000),
 ( 1.000000000000000000, 0.7071225043649866926, 1.000000000000000000),
 ( 1.000000000000000000, 0.7071067811865480168, 1.000000000000000000) ) ) 
 REPRESENTATION_ITEM ( '' )  SURFACE ( )  );
#88003 = DIRECTION ( 'NONE',  ( -1.000000000000000000, -1.224606353822377258E-16, -0.000000000000000000 ) ) ;
#88004 = DIRECTION ( 'NONE',  ( -0.9396926207859143121, 0.000000000000000000, -0.3420201433256525592 ) ) ;
#88005 = VERTEX_POINT ( 'NONE', #46879 ) ;
#88006 = DIRECTION ( 'NONE',  ( 0.000000000000000000, 1.000000000000000000, 0.000000000000000000 ) ) ;
#88007 = STYLED_ITEM ( 'NONE', ( #75721 ), #12305 ) ;
#88008 = CARTESIAN_POINT ( 'NONE',  ( 35.00384615384614762, 1.411358822780289120E-15, 0.000000000000000000 ) ) ;
#88009 = VERTEX_POINT ( 'NONE', #79782 ) ;
#88010 = SURFACE_SIDE_STYLE ('',( #71800 ) ) ;
#88011 = EDGE_CURVE ( 'NONE', #96068, #27489, #16385, .T. ) ;
#88012 = CARTESIAN_POINT ( 'NONE',  ( -1.257803174883066255, -3.680419541196005571E-09, 101.3280723980861495 ) ) ;
#88013 = SURFACE_STYLE_USAGE ( .BOTH. , #29804 ) ;
#88014 = CARTESIAN_POINT ( 'NONE',  ( 5.980073869853586466, 2.767359234578507188, -6.499999999999999112 ) ) ;
#88015 = UNCERTAINTY_MEASURE_WITH_UNIT (LENGTH_MEASURE( 1.000000000000000082E-05 ), #61140, 'distance_accuracy_value', 'NONE');
#88016 = CARTESIAN_POINT ( 'NONE',  ( -110.1493983374076464, -60.00000000000000000, 144.6509950877594690 ) ) ;
#88017 = CARTESIAN_POINT ( 'NONE',  ( 1.040949779275250140E-15, -14.49999999999999822, 8.500000000000000000 ) ) ;
#88018 = FACE_OUTER_BOUND ( 'NONE', #34914, .T. ) ;
#88019 = DIRECTION ( 'NONE',  ( 0.000000000000000000, 0.000000000000000000, 1.000000000000000000 ) ) ;
#88020 = EDGE_CURVE ( 'NONE', #103578, #47564, #2674, .T. ) ;
#88021 = CARTESIAN_POINT ( 'NONE',  ( -82.38425619239932018, -57.17888456031388955, 186.5847884272003228 ) ) ;
#88022 = EDGE_LOOP ( 'NONE', ( #24171, #26554, #39803, #48038, #45830 ) ) ;
#88023 = CARTESIAN_POINT ( 'NONE',  ( 34.55566962155668875, 42.66456075483809229, -62.99380848079916007 ) ) ;
#88024 = AXIS2_PLACEMENT_3D ( 'NONE', #64865, #97224, #40589 ) ;
#88025 = VERTEX_POINT ( 'NONE', #105645 ) ;
#88026 = DIRECTION ( 'NONE',  ( 0.8308658609248535942, -0.5564727496918441263, 0.000000000000000000 ) ) ;
#88027 = EDGE_CURVE ( 'NONE', #94772, #84900, #49535, .T. ) ;
#88028 = CARTESIAN_POINT ( 'NONE',  ( 5.981691436642412540, -68.97269099194116393, -0.5384679144502658721 ) ) ;
#88029 = CARTESIAN_POINT ( 'NONE',  ( -83.66837389949749593, -45.26505878923314441, 10.83132005844547940 ) ) ;
#88030 = VECTOR ( 'NONE', #59359, 1000.000000000000000 ) ;
#88031 = FACE_OUTER_BOUND ( 'NONE', #11433, .T. ) ;
#88032 = CARTESIAN_POINT ( 'NONE',  ( -14.95236164053784478, 4.204970931314857552, -5.179833178255818460 ) ) ;
#88033 = CARTESIAN_POINT ( 'NONE',  ( 2.869473476660086675, 64.67010818586889798, -5.000000000000000000 ) ) ;
#88034 = CARTESIAN_POINT ( 'NONE',  ( 67.48317336153286305, 6.856755485862130937E-15, 0.000000000000000000 ) ) ;
#88035 = CARTESIAN_POINT ( 'NONE',  ( 38.36535705883633085, 18.64316884711714550, -5.022013495247578341 ) ) ;
#88036 =( GEOMETRIC_REPRESENTATION_CONTEXT ( 3 ) GLOBAL_UNCERTAINTY_ASSIGNED_CONTEXT ( ( #26820 ) ) GLOBAL_UNIT_ASSIGNED_CONTEXT ( ( #90012, #88432, #39360 ) ) REPRESENTATION_CONTEXT ( 'NONE', 'WORKASPACE' ) );
#88037 = CARTESIAN_POINT ( 'NONE',  ( 104.7858654919042465, -14.21045842199433018, 190.1692295410596785 ) ) ;
#88038 = COLOUR_RGB ( '', 0.08235294, 0.09019608, 0.10196078) ;
#88039 = CARTESIAN_POINT ( 'NONE',  ( -90.15663891815873399, -29.99999999999996447, 30.33658191415442573 ) ) ;
#88040 = CARTESIAN_POINT ( 'NONE',  ( -65.35149797169954411, -49.91477803733943830, 92.77736392452831637 ) ) ;
#88041 = ORIENTED_EDGE ( 'NONE', *, *, #90079, .F. ) ;
#88042 = CARTESIAN_POINT ( 'NONE',  ( 63.17898818519600468, 39.42583325260841320, 15.56321689764842908 ) ) ;
#88043 = CARTESIAN_POINT ( 'NONE',  ( 64.99933408347442310, -60.00000000015575097, 127.5571855012964733 ) ) ;
#88044 = ORIENTED_EDGE ( 'NONE', *, *, #97164, .T. ) ;
#88045 = CARTESIAN_POINT ( 'NONE',  ( 2.020670042218083218, -42.95360395253835861, 31.04613490824499067 ) ) ;
#88046 = CARTESIAN_POINT ( 'NONE',  ( -7.188101187500000044, -21.78125000204838457, -8.802885111219163269E-16 ) ) ;
#88047 = CARTESIAN_POINT ( 'NONE',  ( -4.660674839411965920, -8.682175146955943390, -3.778981567323763002 ) ) ;
#88048 = ORIENTED_EDGE ( 'NONE', *, *, #87628, .T. ) ;
#88049 = CARTESIAN_POINT ( 'NONE',  ( -10.92969676275529700, 45.30189166192088379, 15.24269870591663079 ) ) ;
#88050 = ORIENTED_EDGE ( 'NONE', *, *, #44309, .F. ) ;
#88051 = DIRECTION ( 'NONE',  ( 0.000000000000000000, 0.000000000000000000, -1.000000000000000000 ) ) ;
#88052 = CARTESIAN_POINT ( 'NONE',  ( 0.000000000000000000, 3.000000000000002665, 0.000000000000000000 ) ) ;
#88053 = CARTESIAN_POINT ( 'NONE',  ( -91.22230685359441793, -60.00000000000002132, 202.2302250722651706 ) ) ;
#88054 = DIRECTION ( 'NONE',  ( 0.000000000000000000, 1.000000000000000000, 0.000000000000000000 ) ) ;
#88055 = CARTESIAN_POINT ( 'NONE',  ( -2.977408999572654480, -24.50000000204839168, 7.188101187499999156 ) ) ;
#88056 = DIRECTION ( 'NONE',  ( 1.000000000000000000, 1.224606353822377258E-16, 0.000000000000000000 ) ) ;
#88057 = DIRECTION ( 'NONE',  ( 0.000000000000000000, 0.000000000000000000, -1.000000000000000000 ) ) ;
#88058 = CARTESIAN_POINT ( 'NONE',  ( 5.000000000000000888, -67.35888985736187351, 11.51944599242068890 ) ) ;
#88059 = CARTESIAN_POINT ( 'NONE',  ( -8.737863884121431113, 48.00000000000000000, -79.96381019768850251 ) ) ;
#88060 = ADVANCED_FACE ( 'NONE', ( #31785 ), #48992, .T. ) ;
#88061 = CARTESIAN_POINT ( 'NONE',  ( 32.96117425224227304, 439.7497740807306172, 24.15381775812835130 ) ) ;
#88062 = DIRECTION ( 'NONE',  ( 1.000000000000000000, 0.000000000000000000, -0.000000000000000000 ) ) ;
#88063 = CARTESIAN_POINT ( 'NONE',  ( 104.7431539673617493, -60.00000000000000000, 188.6673425520828573 ) ) ;
#88064 = CARTESIAN_POINT ( 'NONE',  ( -36.59778291639800329, -32.58603346802485135, 34.88119437908692078 ) ) ;
#88065 = VECTOR ( 'NONE', #67206, 1000.000000000000000 ) ;
#88066 = ORIENTED_EDGE ( 'NONE', *, *, #62055, .T. ) ;
#88067 = CARTESIAN_POINT ( 'NONE',  ( -35.05484418697486149, 463.2659305983892750, 4.633372620823961618 ) ) ;
#88068 = CARTESIAN_POINT ( 'NONE',  ( 36.59759212853143850, -53.35504654647210998, 39.00208765491442620 ) ) ;
#88069 = CARTESIAN_POINT ( 'NONE',  ( -14.86825985028395181, -1.734723475976807094E-15, -8.569529079644194525 ) ) ;
#88070 = ORIENTED_EDGE ( 'NONE', *, *, #87114, .F. ) ;
#88071 = ADVANCED_FACE ( 'NONE', ( #88945 ), #23349, .T. ) ;
#88072 = CARTESIAN_POINT ( 'NONE',  ( 5.975663821520919683, -4.257391242883398874, 5.625982059627139265 ) ) ;
#88073 = CARTESIAN_POINT ( 'NONE',  ( -67.36060469812591123, -38.33500041653474710, 122.7867264952750475 ) ) ;
#88074 = VERTEX_POINT ( 'NONE', #72741 ) ;
#88076 = CARTESIAN_POINT ( 'NONE',  ( -27.57151080649627417, 314.0751515626058676, 12.18133379269485239 ) ) ;
#88075 = CARTESIAN_POINT ( 'NONE',  ( 9.339269934323091604, -5.000000000000000000, -18.52512058521576677 ) ) ;
#88077 = CARTESIAN_POINT ( 'NONE',  ( 16.34245632501163925, 37.19060558336133226, 21.87293403489666588 ) ) ;
#88078 = CARTESIAN_POINT ( 'NONE',  ( 8.000000000000000000, -23.09375000409677270, -3.313708498984761164 ) ) ;
#88079 = CARTESIAN_POINT ( 'NONE',  ( 5.581309233574441675E-23, 43.17555810750860701, -18.75000000000000355 ) ) ;
#88080 = CARTESIAN_POINT ( 'NONE',  ( -17.49999999999997513, 45.00000000000000711, 64.09953197936602010 ) ) ;
#88081 = CARTESIAN_POINT ( 'NONE',  ( 4.589925132946516939, -86.06526016292519898, 3.864926970398267603 ) ) ;
#88082 = CARTESIAN_POINT ( 'NONE',  ( 42.57704743493908950, 486.1612337113410263, 7.852296464539637810 ) ) ;
#88083 = CARTESIAN_POINT ( 'NONE',  ( 94.50007956662228992, -60.00000000000000711, 45.30279473861475026 ) ) ;
#88084 = DIRECTION ( 'NONE',  ( 0.000000000000000000, 0.000000000000000000, -1.000000000000000000 ) ) ;
#88085 = CARTESIAN_POINT ( 'NONE',  ( 0.000000000000000000, 0.000000000000000000, 0.000000000000000000 ) ) ;
#88086 = CARTESIAN_POINT ( 'NONE',  ( -34.12349128637494289, 490.8027302422244134, 11.84948222508913318 ) ) ;
#88087 = ORIENTED_EDGE ( 'NONE', *, *, #62163, .T. ) ;
#88088 = VECTOR ( 'NONE', #45113, 1000.000000000000114 ) ;
#88089 = CARTESIAN_POINT ( 'NONE',  ( -84.45496583931854673, -29.99999999999999645, 165.1288136768957031 ) ) ;
#88090 = EDGE_LOOP ( 'NONE', ( #101300, #70314, #17520, #33254 ) ) ;
#88091 = CARTESIAN_POINT ( 'NONE',  ( 1.517883041479706208E-15, -5.000000000000000888, -97.00000000000000000 ) ) ;
#88092 =( NAMED_UNIT ( * ) SI_UNIT ( $, .STERADIAN. ) SOLID_ANGLE_UNIT ( ) );
#88093 = CARTESIAN_POINT ( 'NONE',  ( 8.167402502809283149, 39.27965345049499746, -1.228220045931598409E-12 ) ) ;
#88094 = CARTESIAN_POINT ( 'NONE',  ( 0.000000000000000000, -30.00000000000000000, 0.000000000000000000 ) ) ;
#88095 = CARTESIAN_POINT ( 'NONE',  ( 0.000000000000000000, 0.000000000000000000, 0.000000000000000000 ) ) ;
#88096 = CARTESIAN_POINT ( 'NONE',  ( 2.977408999572650927, -31.25000000204838813, -7.188101187500001821 ) ) ;
#88097 = CARTESIAN_POINT ( 'NONE',  ( 0.000000000000000000, 0.000000000000000000, 0.000000000000000000 ) ) ;
#88098 = LINE ( 'NONE', #55689, #54253 ) ;
#88099 = CARTESIAN_POINT ( 'NONE',  ( 31.84025839850067996, 489.2002011298899333, 8.970818581732807218 ) ) ;
#88100 = ORIENTED_EDGE ( 'NONE', *, *, #91739, .T. ) ;
#88102 = ORIENTED_EDGE ( 'NONE', *, *, #13287, .T. ) ;
#88101 = CARTESIAN_POINT ( 'NONE',  ( 0.000000000000000000, 299.9999999999999432, 0.000000000000000000 ) ) ;
#88103 = CARTESIAN_POINT ( 'NONE',  ( 80.30221349524663310, -39.49731160925162499, 147.7246413452121487 ) ) ;
#88104 = CIRCLE ( 'NONE', #86428, 5.000000000000002665 ) ;
#88105 = SURFACE_STYLE_FILL_AREA ( #21802 ) ;
#88106 = EDGE_LOOP ( 'NONE', ( #18090, #12724, #67141, #21320, #44592 ) ) ;
#88107 = CARTESIAN_POINT ( 'NONE',  ( -12.50000000000000000, 25.10944952739952996, -42.56876883562922842 ) ) ;
#88108 = CARTESIAN_POINT ( 'NONE',  ( 43.58492305596168137, 465.9553058690736407, 13.43507729846636245 ) ) ;
#88109 = CARTESIAN_POINT ( 'NONE',  ( 7.188101187500000933, -14.56250000204838457, -2.977408999572650483 ) ) ;
#88110 = AXIS2_PLACEMENT_3D ( 'NONE', #54629, #14709, #47610 ) ;
#88111 = CARTESIAN_POINT ( 'NONE',  ( 10.45113867624397841, 45.35217484112028075, 15.40779740156150091 ) ) ;
#88112 = CARTESIAN_POINT ( 'NONE',  ( 15.65208535197129613, 294.5588103013598129, 9.874721941290198757 ) ) ;
#88113 = EDGE_CURVE ( 'NONE', #16386, #77688, #35458, .T. ) ;
#88114 = VERTEX_POINT ( 'NONE', #7468 ) ;
#88115 = CIRCLE ( 'NONE', #13790, 5.000000000000002665 ) ;
#88116 = LINE ( 'NONE', #63319, #25257 ) ;
#88117 = CARTESIAN_POINT ( 'NONE',  ( -4.472135954999580498, -10.00000000000000888, 4.000000000000000000 ) ) ;
#88118 = EDGE_CURVE ( 'NONE', #92331, #68935, #15577, .T. ) ;
#88119 = MANIFOLD_SOLID_BREP ( 'Cut-Extrude3', #106576 ) ;
#88120 = CARTESIAN_POINT ( 'NONE',  ( 7.237253906321553742, 41.05631881893103952, -58.62831218766484653 ) ) ;
#88121 = AXIS2_PLACEMENT_3D ( 'NONE', #1864, #57980, #25673 ) ;
#88122 = ORIENTED_EDGE ( 'NONE', *, *, #29529, .T. ) ;
#88123 = CARTESIAN_POINT ( 'NONE',  ( -3.313708498984760720, -9.218750004096769146, -8.000000000000000000 ) ) ;
#88124 = CARTESIAN_POINT ( 'NONE',  ( -29.69263446058518596, -21.53086560699351892, 32.09607384880168723 ) ) ;
#88125 = CARTESIAN_POINT ( 'NONE',  ( 9.999999999999957367, 15.00000000000001066, 3.836411046841756711 ) ) ;
#88126 = DIRECTION ( 'NONE',  ( 0.000000000000000000, 0.000000000000000000, 1.000000000000000000 ) ) ;
#88127 = B_SPLINE_CURVE_WITH_KNOTS ( 'NONE', 3,
 ( #64064, #9909, #74107, #67102, #55911, #99987, #31179, #66562, #90845, #42819, #88852, #39254, #91384, #75714, #16963, #91902, #72129, #49839, #26157, #82746, #33160, #1808, #34767, #41221, #8847, #50362, #41752, #42279, #25618, #67640 ),
 .UNSPECIFIED., .F., .F.,
 ( 4, 2, 2, 2, 2, 2, 2, 2, 2, 2, 2, 2, 2, 2, 4 ),
 ( 0.008220542767890477720, 0.008453091251724709904, 0.008685639735558942087, 0.009150736703227401250, 0.009615833670895858679, 0.01008093063856431784, 0.01101112457390123443, 0.01194131850923815102, 0.01287151244457507282, 0.01380170637991199462, 0.01426680334758045204, 0.01473190031524891121, 0.01519699728291737037, 0.01542954576675160082, 0.01566209425058583127 ),
 .UNSPECIFIED. ) ;
#88128 = CARTESIAN_POINT ( 'NONE',  ( 7.500000000016720847, 43.33959969848655192, -60.00534814812574780 ) ) ;
#88129 = PRESENTATION_STYLE_ASSIGNMENT (( #63859 ) ) ;
#88130 = CARTESIAN_POINT ( 'NONE',  ( -9.537909130738274399, 32.64614830963394354, -3.010726932293863012 ) ) ;
#88131 = VERTEX_POINT ( 'NONE', #47931 ) ;
#88132 = CARTESIAN_POINT ( 'NONE',  ( -4.861345245134582882, -47.05236803399135681, 42.74555668121053742 ) ) ;
#88133 = CARTESIAN_POINT ( 'NONE',  ( 90.51111111111110574, 4.172000000000019249, 0.000000000000000000 ) ) ;
#88134 = CARTESIAN_POINT ( 'NONE',  ( -41.61957457421983975, 435.6113505990639396, 7.035653009325270268 ) ) ;
#88135 = CARTESIAN_POINT ( 'NONE',  ( -46.00000000000000000, 461.6622277975412203, 10.18145404766301709 ) ) ;
#88136 = CARTESIAN_POINT ( 'NONE',  ( -72.03391849934671143, -30.00000000000000000, 102.0186397125481506 ) ) ;
#88137 = CARTESIAN_POINT ( 'NONE',  ( 7.500000000000007105, 40.00000000000000000, -59.28631038546474485 ) ) ;
#88138 = EDGE_CURVE ( 'NONE', #12068, #5362, #96517, .T. ) ;
#88139 = AXIS2_PLACEMENT_3D ( 'NONE', #63762, #40007, #73409 ) ;
#88140 = VERTEX_POINT ( 'NONE', #105130 ) ;
#88141 = B_SPLINE_CURVE_WITH_KNOTS ( 'NONE', 3,
 ( #50141, #91163, #91681, #486, #76009, #1573, #33455, #49068, #26448, #34002, #58234, #66872, #81963, #57688, #25377, #73883 ),
 .UNSPECIFIED., .F., .F.,
 ( 4, 2, 2, 2, 2, 2, 2, 4 ),
 ( 0.007045997238651392942, 0.007550033810006847451, 0.008054070381362302827, 0.008558106952717758203, 0.009062143524073211845, 0.009566180095428667221, 0.01007021666678412086, 0.01107828980949503161 ),
 .UNSPECIFIED. ) ;
#88142 = LINE ( 'NONE', #47126, #70249 ) ;
#88143 = CARTESIAN_POINT ( 'NONE',  ( 88.84533078683669771, -57.60264346193348928, 203.6993548357257851 ) ) ;
#88144 = CARTESIAN_POINT ( 'NONE',  ( 73.91531349502166393, -47.40886024016416656, -22.31105010388982279 ) ) ;
#88145 = DIRECTION ( 'NONE',  ( 0.000000000000000000, 0.000000000000000000, 1.000000000000000000 ) ) ;
#88146 = CARTESIAN_POINT ( 'NONE',  ( -14.60001457338410269, 22.21450448813268252, 3.985393712994455218 ) ) ;
#88147 = CARTESIAN_POINT ( 'NONE',  ( -5.934039023508266730, 53.39575557745317980, 8.365659210409152280 ) ) ;
#88148 = CARTESIAN_POINT ( 'NONE',  ( -75.41707018382817296, -60.00000000000002132, 184.0048572794236179 ) ) ;
#88149 = FACE_OUTER_BOUND ( 'NONE', #91904, .T. ) ;
#88150 = CARTESIAN_POINT ( 'NONE',  ( 103.5111111111111057, 1.023464760207051730E-14, 0.000000000000000000 ) ) ;
#88151 = CARTESIAN_POINT ( 'NONE',  ( -56.06936961859863544, 49.99999999999999289, -33.41736086620520751 ) ) ;
#88152 = CARTESIAN_POINT ( 'NONE',  ( -85.41682882701736901, -42.92406899005316490, 186.8839715543561510 ) ) ;
#88153 = VERTEX_POINT ( 'NONE', #98090 ) ;
#88154 = CARTESIAN_POINT ( 'NONE',  ( 35.46172211909674843, 432.6321351846624452, 5.657271128263613669 ) ) ;
#88155 = CARTESIAN_POINT ( 'NONE',  ( 12.23630716935516816, -4.549675231767582595, -76.78946638291472482 ) ) ;
#88156 = ADVANCED_FACE ( 'NONE', ( #106706 ), #76672, .F. ) ;
#88157 = CARTESIAN_POINT ( 'NONE',  ( 8.572527594031464315E-16, 60.00000000000000000, -6.999999999999992895 ) ) ;
#88158 = CARTESIAN_POINT ( 'NONE',  ( 40.81102101573196705, 489.2883016990687111, 10.51949396897182787 ) ) ;
#88159 = CARTESIAN_POINT ( 'NONE',  ( 67.48317336153286305, 4.000000000000015099, 4.898587196589422689E-16 ) ) ;
#88160 = CYLINDRICAL_SURFACE ( 'NONE', #63733, 4.000000000000000000 ) ;
#88161 = EDGE_LOOP ( 'NONE', ( #93882, #66007, #36509, #49078, #14498, #47084 ) ) ;
#88162 = CARTESIAN_POINT ( 'NONE',  ( 18.12922454741385891, 50.00000000000001421, 61.72358472360003390 ) ) ;
#88163 = CARTESIAN_POINT ( 'NONE',  ( 10.05835083440616273, 14.72912344306572408, 10.42335925054806545 ) ) ;
#88164 = SHAPE_REPRESENTATION ( 'hex flange bolt_din_DIN 6921 - M8 x 40 x 40-S', ( #10728 ), #33394 ) ;
#88165 = CARTESIAN_POINT ( 'NONE',  ( 2.723397405354400211E-15, -8.673617379884035472E-16, 22.23822744035697241 ) ) ;
#88166 = CARTESIAN_POINT ( 'NONE',  ( -34.88900972249400212, 464.6206820655984870, 18.69027339340994232 ) ) ;
#88167 = CARTESIAN_POINT ( 'NONE',  ( 89.90448154148772630, -29.99999999999993605, -11.15250327688899645 ) ) ;
#88168 = CARTESIAN_POINT ( 'NONE',  ( -80.36800950332954585, -29.09175213282752992, 137.3191375394279419 ) ) ;
#88169 = ORIENTED_EDGE ( 'NONE', *, *, #72475, .T. ) ;
#88170 = CARTESIAN_POINT ( 'NONE',  ( 28.47648766833107103, -14.21045842199436926, 36.49840447651481412 ) ) ;
#88171 = CARTESIAN_POINT ( 'NONE',  ( 0.000000000000000000, 29.08768991669519721, 0.000000000000000000 ) ) ;
#88172 = CARTESIAN_POINT ( 'NONE',  ( 103.6548915283567993, -57.63783869900026247, 202.5245876488449426 ) ) ;
#88173 =( LENGTH_UNIT ( ) NAMED_UNIT ( * ) SI_UNIT ( .MILLI., .METRE. ) );
#88174 = CARTESIAN_POINT ( 'NONE',  ( 35.85994258077860053, 303.7596300888440624, 0.04768371627283522762 ) ) ;
#88175 = DIRECTION ( 'NONE',  ( 0.2472079847635547389, 0.000000000000000000, -0.9689624411034424289 ) ) ;
#88176 = ORIENTED_EDGE ( 'NONE', *, *, #17416, .F. ) ;
#88177 = CARTESIAN_POINT ( 'NONE',  ( -23.05214773880026513, 26.02499767950420306, 30.70617127781060418 ) ) ;
#88178 = CONICAL_SURFACE ( 'NONE', #15869, 6.500000000000000000, 1.047197551196600296 ) ;
#88179 = PRESENTATION_STYLE_ASSIGNMENT (( #6173 ) ) ;
#88181 = CARTESIAN_POINT ( 'NONE',  ( -106.5035232221163426, -60.15522548674435654, 170.5901316164547836 ) ) ;
#88180 = CARTESIAN_POINT ( 'NONE',  ( 33.58349330513379982, 4.000000000000003553, 0.000000000000000000 ) ) ;
#88182 = CARTESIAN_POINT ( 'NONE',  ( 4.401442555609581635E-16, -18.78125000204838457, -7.188101187500000044 ) ) ;
#88183 = DIRECTION ( 'NONE',  ( 0.000000000000000000, 1.000000000000000000, 0.000000000000000000 ) ) ;
#88184 =( GEOMETRIC_REPRESENTATION_CONTEXT ( 3 ) GLOBAL_UNCERTAINTY_ASSIGNED_CONTEXT ( ( #54915 ) ) GLOBAL_UNIT_ASSIGNED_CONTEXT ( ( #57288, #74544, #620 ) ) REPRESENTATION_CONTEXT ( 'NONE', 'WORKASPACE' ) );
#88185 = DIRECTION ( 'NONE',  ( 0.000000000000000000, -1.000000000000000000, 0.000000000000000000 ) ) ;
#88186 = ADVANCED_FACE ( 'NONE', ( #63628 ), #6412, .F. ) ;
#88187 = CARTESIAN_POINT ( 'NONE',  ( 0.3173508448886566691, -8.480771745766407577, -1.310872448937994150 ) ) ;
#88188 = FILL_AREA_STYLE_COLOUR ( '', #92079 ) ;
#88189 = CARTESIAN_POINT ( 'NONE',  ( -3.400000000000000355, 4.163799117101001052E-16, -6.123524522925831270 ) ) ;
#88190 = ORIENTED_EDGE ( 'NONE', *, *, #88739, .F. ) ;
#88191 = DIRECTION ( 'NONE',  ( -1.000000000000000000, -1.224606353822377258E-16, -0.000000000000000000 ) ) ;
#88192 = AXIS2_PLACEMENT_3D ( 'NONE', #29968, #30495, #62859 ) ;
#88194 = CARTESIAN_POINT ( 'NONE',  ( 27.18233788174618937, -36.00292342176191340, 31.66508634081275630 ) ) ;
#88193 = CARTESIAN_POINT ( 'NONE',  ( -25.54656159126955117, -59.99999999999990763, 43.65498583421084788 ) ) ;
#88195 = DIRECTION ( 'NONE',  ( 0.000000000000000000, 0.000000000000000000, 1.000000000000000000 ) ) ;
#88196 = ORIENTED_EDGE ( 'NONE', *, *, #38797, .T. ) ;
#88197 = EDGE_CURVE ( 'NONE', #67545, #23216, #47485, .T. ) ;
#88198 = UNCERTAINTY_MEASURE_WITH_UNIT (LENGTH_MEASURE( 1.000000000000000082E-05 ), #21090, 'distance_accuracy_value', 'NONE');
#88199 = VERTEX_POINT ( 'NONE', #10143 ) ;
#88200 = PRODUCT_DEFINITION_SHAPE ( 'NONE', 'NONE',  #106818 ) ;
#88202 = CARTESIAN_POINT ( 'NONE',  ( -113.4247593822225042, -60.00000000000000000, 152.6440057603899447 ) ) ;
#88201 = LINE ( 'NONE', #39127, #43408 ) ;
#88203 = CARTESIAN_POINT ( 'NONE',  ( 7.251496294514814700, 41.03131494657971956, -58.65726288480846051 ) ) ;
#88204 = DIRECTION ( 'NONE',  ( 1.000000000000000000, -0.000000000000000000, 1.224646799147353207E-16 ) ) ;
#88205 = DIRECTION ( 'NONE',  ( -1.000000000000000000, 8.881784197001252323E-16, 0.000000000000000000 ) ) ;
#88206 = CARTESIAN_POINT ( 'NONE',  ( 0.6191880370026833225, 18.48281550088974257, -49.41023453029059453 ) ) ;
#88207 = ORIENTED_EDGE ( 'NONE', *, *, #96914, .F. ) ;
#88208 = DIRECTION ( 'NONE',  ( 0.000000000000000000, 0.000000000000000000, 1.000000000000000000 ) ) ;
#88209 = CARTESIAN_POINT ( 'NONE',  ( 63.72657953987652490, -30.00000000000000000, 76.60532204191858341 ) ) ;
#88210 = CARTESIAN_POINT ( 'NONE',  ( -10.02621571918099264, 14.06829240002694092, 10.51410051269792234 ) ) ;
#88212 = EDGE_CURVE ( 'NONE', #62199, #106204, #13056, .T. ) ;
#88211 = CARTESIAN_POINT ( 'NONE',  ( 0.000000000000000000, 6.123233995736767268E-16, -5.000000000000000888 ) ) ;
#88213 = CARTESIAN_POINT ( 'NONE',  ( 11.84999999999999787, 1.533819458162526451E-15, 0.000000000000000000 ) ) ;
#88214 = CARTESIAN_POINT ( 'NONE',  ( 0.000000000000000000, 0.000000000000000000, -8.000000000000000000 ) ) ;
#88215 = EDGE_LOOP ( 'NONE', ( #98093, #69529, #8231 ) ) ;
#88216 = PRESENTATION_LAYER_ASSIGNMENT (  '', '', ( #84814 ) ) ;
#88217 = VERTEX_POINT ( 'NONE', #59246 ) ;
#88218 = ORIENTED_EDGE ( 'NONE', *, *, #9154, .F. ) ;
#88219 = DIRECTION ( 'NONE',  ( -1.000000000000000000, -0.000000000000000000, -0.000000000000000000 ) ) ;
#88220 = DIRECTION ( 'NONE',  ( -0.000000000000000000, 1.000000000000000000, -0.000000000000000000 ) ) ;
#88221 = CARTESIAN_POINT ( 'NONE',  ( 7.000000000000000000, 0.000000000000000000, -13.00000000000000000 ) ) ;
#88222 = TOROIDAL_SURFACE ( 'NONE', #98508, 7.500000000000006217, 5.000000000000000000 ) ;
#88223 = CARTESIAN_POINT ( 'NONE',  ( 4.472135954999581386, -10.00000000000000888, -4.000000000000000000 ) ) ;
#88224 = PRESENTATION_STYLE_ASSIGNMENT (( #22453 ) ) ;
#88225 =( NAMED_UNIT ( * ) SI_UNIT ( $, .STERADIAN. ) SOLID_ANGLE_UNIT ( ) );
#88226 = DIRECTION ( 'NONE',  ( 0.000000000000000000, 0.000000000000000000, 1.000000000000000000 ) ) ;
#88227 = VERTEX_POINT ( 'NONE', #34990 ) ;
#88228 = CARTESIAN_POINT ( 'NONE',  ( -9.739726766104285005, 48.00000000000000000, -82.38252115500968387 ) ) ;
#88229 = CONICAL_SURFACE ( 'NONE', #96767, 4.172000000000009479, 0.9599310885968813656 ) ;
#88230 = ORIENTED_EDGE ( 'NONE', *, *, #97905, .T. ) ;
#88231 = CARTESIAN_POINT ( 'NONE',  ( -43.71037717921252863, 462.3391554988666599, 4.824299547746595529 ) ) ;
#88232 = CARTESIAN_POINT ( 'NONE',  ( -6.539196172010136365, -3.775406670193843794, -6.286444963328675861 ) ) ;
#88233 = CARTESIAN_POINT ( 'NONE',  ( -41.14690903223496576, 485.7356601713278224, -4.640470638255251856 ) ) ;
#88234 = B_SPLINE_CURVE_WITH_KNOTS ( 'NONE', 3,
 ( #80181, #21986, #87770, #88300, #46764, #96397, #71040, #5769 ),
 .UNSPECIFIED., .F., .F.,
 ( 4, 2, 2, 4 ),
 ( 0.000000000000000000, 0.5000000000000000000, 0.7500000000000000000, 1.000000000000000000 ),
 .UNSPECIFIED. ) ;
#88235 = CARTESIAN_POINT ( 'NONE',  ( 0.000000000000000000, 55.00000000000000000, 0.000000000000000000 ) ) ;
#88236 = CARTESIAN_POINT ( 'NONE',  ( 63.81288939447262010, -42.95796419212698680, 84.51729907025924149 ) ) ;
#88237 = EDGE_LOOP ( 'NONE', ( #64260, #102132, #49949, #1242, #31261, #63407 ) ) ;
#88238 = CARTESIAN_POINT ( 'NONE',  ( -7.493949047870493096, 40.57569111244914950, -68.91429205788598722 ) ) ;
#88239 = CARTESIAN_POINT ( 'NONE',  ( 9.833493305133805151, 1.593028355512270962E-15, 0.000000000000000000 ) ) ;
#88240 = DIRECTION ( 'NONE',  ( 0.000000000000000000, 1.000000000000000000, 0.000000000000000000 ) ) ;
#88241 = CARTESIAN_POINT ( 'NONE',  ( -14.05937931246655026, -57.67120694556813731, -44.20476115079929258 ) ) ;
#88242 = EDGE_CURVE ( 'NONE', #96664, #44923, #102593, .T. ) ;
#88243 = EDGE_LOOP ( 'NONE', ( #10078, #93316, #9836, #29280 ) ) ;
#88244 = CARTESIAN_POINT ( 'NONE',  ( 47.55484174479031623, 16.07433637411964611, 16.76829442854542052 ) ) ;
#88245 = CARTESIAN_POINT ( 'NONE',  ( -1.780747208277499993, -60.00000000000000000, -36.88202602987092860 ) ) ;
#88246 = EDGE_CURVE ( 'NONE', #40596, #84887, #42510, .T. ) ;
#88247 = EDGE_CURVE ( 'NONE', #25439, #24651, #940, .T. ) ;
#88248 = LINE ( 'NONE', #30029, #18631 ) ;
#88249 = CARTESIAN_POINT ( 'NONE',  ( -1.469576158976823947E-15, -32.56250000409677625, 8.000000000000000000 ) ) ;
#88250 = CARTESIAN_POINT ( 'NONE',  ( 5.219866590718106991, -5.000000000000000000, 8.922269033012842243 ) ) ;
#88251 = CARTESIAN_POINT ( 'NONE',  ( 86.84945405509184013, -28.04156739919917385, 186.3543369133316503 ) ) ;
#88252 = EDGE_CURVE ( 'NONE', #81173, #50100, #93197, .T. ) ;
#88253 = SURFACE_STYLE_FILL_AREA ( #55325 ) ;
#88254 = CARTESIAN_POINT ( 'NONE',  ( -4.339355498967208291, 10.71439286440603489, 4.999999999999999112 ) ) ;
#88255 = CARTESIAN_POINT ( 'NONE',  ( 7.414346147791998298, -7.354108423377371473, -3.010818766110529232 ) ) ;
#88256 = AXIS2_PLACEMENT_3D ( 'NONE', #36152, #78673, #79217 ) ;
#88257 = CARTESIAN_POINT ( 'NONE',  ( -4.582575694955839829, 15.00000000000000000, -9.999999999999998224 ) ) ;
#88258 = ORIENTED_EDGE ( 'NONE', *, *, #5467, .T. ) ;
#88259 = DIRECTION ( 'NONE',  ( 0.000000000000000000, 1.000000000000000000, 0.000000000000000000 ) ) ;
#88260 = COLOUR_RGB ( '', 0.31764706, 0.68627451, 0.89019608) ;
#88261 = CARTESIAN_POINT ( 'NONE',  ( 39.15529195327606971, -60.00000000000000000, 50.94776041160520208 ) ) ;
#88262 = CARTESIAN_POINT ( 'NONE',  ( -99.14678559174451777, -29.99999999999999645, 146.1870180612345109 ) ) ;
#88263 = B_SPLINE_CURVE_WITH_KNOTS ( 'NONE', 3,
 ( #11657, #87167, #30007, #77477, #3589, #69391, #102274, #28423, #37047, #12193, #61299, #103345, #28976, #69914, #45124, #85035, #21391, #13248, #61842, #78002, #95260, #4118, #102814, #45644, #103857, #46172, #94739, #78520, #70450, #29493, #62369, #54228, #79062, #5181 ),
 .UNSPECIFIED., .F., .F.,
 ( 4, 2, 2, 2, 2, 2, 2, 2, 2, 2, 2, 2, 2, 2, 2, 2, 4 ),
 ( 0.000000000000000000, 0.0007951492273476391814, 0.001590298454695278363, 0.002385447682042917544, 0.003180596909390556726, 0.003975746136738195907, 0.004770895364085835089, 0.005566044591433473403, 0.006361193818781111717, 0.007156343046128750031, 0.007951492273476388345, 0.008746641500824025792, 0.009541790728171663238, 0.01033693995551930069, 0.01113208918286693987, 0.01192723841021457558, 0.01272238763756221476 ),
 .UNSPECIFIED. ) ;
#88264 = EDGE_CURVE ( 'NONE', #87422, #53391, #70511, .T. ) ;
#88265 = CARTESIAN_POINT ( 'NONE',  ( 48.02835407290504577, 16.78162100668611956, -14.35535821593549954 ) ) ;
#88266 = CONICAL_SURFACE ( 'NONE', #21092, 6.500000000000000888, 0.8987552595851637793 ) ;
#88267 = CARTESIAN_POINT ( 'NONE',  ( 35.66404283213154258, -57.69580505578924345, 49.84151983041640932 ) ) ;
#88269 = CARTESIAN_POINT ( 'NONE',  ( 0.000000000000000000, 0.000000000000000000, 0.000000000000000000 ) ) ;
#88268 = CARTESIAN_POINT ( 'NONE',  ( 9.147872746976656089, 44.02395455486185227, 13.63474389503118012 ) ) ;
#88270 = ADVANCED_FACE ( 'NONE', ( #78071 ), #69984, .T. ) ;
#88271 = CARTESIAN_POINT ( 'NONE',  ( -40.47244160127206669, 40.24842158074789467, -54.85959184083456819 ) ) ;
#88272 = CARTESIAN_POINT ( 'NONE',  ( -18.14538688196167726, 50.00000000000000711, 61.70354622640617492 ) ) ;
#88273 = DIRECTION ( 'NONE',  ( 1.000000000000000000, 0.000000000000000000, 0.000000000000000000 ) ) ;
#88274 = CARTESIAN_POINT ( 'NONE',  ( -16.78325067526352044, -60.00000000000000711, 39.90621369170523991 ) ) ;
#88275 = ADVANCED_FACE ( 'NONE', ( #4721 ), #97444, .T. ) ;
#88276 = CARTESIAN_POINT ( 'NONE',  ( -86.87673661167058015, -20.64820290907504940, 186.0011859003656980 ) ) ;
#88277 = ORIENTED_EDGE ( 'NONE', *, *, #31356, .F. ) ;
#88278 = CARTESIAN_POINT ( 'NONE',  ( 17.50000000000004974, 49.99999999999836575, 59.86364615470527184 ) ) ;
#88279 = CARTESIAN_POINT ( 'NONE',  ( 33.50220463782144265, 465.4655183566888468, 16.55182854115482272 ) ) ;
#88280 = CARTESIAN_POINT ( 'NONE',  ( -14.55865618082035873, -39.47623590528959880, 30.59058187625803527 ) ) ;
#88281 = MECHANICAL_DESIGN_GEOMETRIC_PRESENTATION_REPRESENTATION (  '', ( #31492 ), #52160 ) ;
#88283 = CARTESIAN_POINT ( 'NONE',  ( 40.45545246860639566, 460.8457769820566909, 2.191470225627300206 ) ) ;
#88282 = CARTESIAN_POINT ( 'NONE',  ( -105.0711731827093018, -60.00000000000000711, 187.5141690426402192 ) ) ;
#88284 = ORIENTED_EDGE ( 'NONE', *, *, #64647, .F. ) ;
#88285 = CARTESIAN_POINT ( 'NONE',  ( -43.72400580963713423, 464.7562747155352554, 7.841095524562895491 ) ) ;
#88286 = PRESENTATION_LAYER_ASSIGNMENT (  '', '', ( #90042 ) ) ;
#88287 = SURFACE_STYLE_FILL_AREA ( #61907 ) ;
#88288 = CARTESIAN_POINT ( 'NONE',  ( 0.05458999538772899701, -1.264741368073337036, -6.500000000000000888 ) ) ;
#88289 = VECTOR ( 'NONE', #25491, 1000.000000000000000 ) ;
#88291 = MANIFOLD_SOLID_BREP ( 'Fillet7', #44631 ) ;
#88290 = FACE_OUTER_BOUND ( 'NONE', #60733, .T. ) ;
#88292 = CARTESIAN_POINT ( 'NONE',  ( 15.91668924485835390, 3.370617522763084128, -2.350968163827917845 ) ) ;
#88293 = CARTESIAN_POINT ( 'NONE',  ( 68.86877790052056980, -60.00000000000000711, 135.3615938647542407 ) ) ;
#88294 = FACE_OUTER_BOUND ( 'NONE', #38967, .T. ) ;
#88295 = ORIENTED_EDGE ( 'NONE', *, *, #60558, .T. ) ;
#88296 = CARTESIAN_POINT ( 'NONE',  ( -7.853841075665486393, -30.00000000000001066, -1.477988678308346016 ) ) ;
#88297 = CARTESIAN_POINT ( 'NONE',  ( -17.49999999999999645, 2.500000000000000444, 25.00000000000000000 ) ) ;
#88298 = VECTOR ( 'NONE', #28838, 1000.000000000000000 ) ;
#88300 = CARTESIAN_POINT ( 'NONE',  ( 6.965116047733301841, 41.61856606189723351, -70.00485699918135651 ) ) ;
#88299 = CARTESIAN_POINT ( 'NONE',  ( 12.83322425571993186, -59.99999999999995737, 42.04720346242444151 ) ) ;
#88301 =( NAMED_UNIT ( * ) PLANE_ANGLE_UNIT ( ) SI_UNIT ( $, .RADIAN. ) );
#88302 = CARTESIAN_POINT ( 'NONE',  ( -5.238409285680481808, -1.996984918271471621, 104.1169421774614108 ) ) ;
#88303 = ORIENTED_EDGE ( 'NONE', *, *, #10656, .F. ) ;
#88304 = VERTEX_POINT ( 'NONE', #5253 ) ;
#88305 = CARTESIAN_POINT ( 'NONE',  ( -25.56687214313617318, 308.5055938668078284, 10.78667975285395286 ) ) ;
#88306 = VERTEX_POINT ( 'NONE', #102347 ) ;
#88308 =( BOUNDED_SURFACE ( )  B_SPLINE_SURFACE ( 3, 2, ( 
 ( #21450, #54287, #6275 ),
 ( #104996, #47274, #53781 ),
 ( #72089, #61909, #86712 ),
 ( #45700, #87228, #46234 ) ),
 .UNSPECIFIED., .F., .F., .F. ) 
 B_SPLINE_SURFACE_WITH_KNOTS ( ( 4, 4 ),
 ( 3, 3 ),
 ( -3.469446951953614189E-18, 0.002002951328326270462 ),
 ( 0.000000000000000000, 1.000000000000000000 ),
 .UNSPECIFIED. ) 
 GEOMETRIC_REPRESENTATION_ITEM ( )  RATIONAL_B_SPLINE_SURFACE ( (
 ( 1.000000000000000000, 0.7699558187665878073, 1.000000000000000000),
 ( 1.000000000000000000, 0.7788467038584422353, 1.000000000000000000),
 ( 1.000000000000000000, 0.7876570642905440511, 1.000000000000000000),
 ( 1.000000000000000000, 0.7964405967476624326, 1.000000000000000000) ) ) 
 REPRESENTATION_ITEM ( '' )  SURFACE ( )  );
#88307 = CARTESIAN_POINT ( 'NONE',  ( 22.31815708081593641, 304.3216620908660275, 10.03816277198476037 ) ) ;
#88309 = DIRECTION ( 'NONE',  ( 0.000000000000000000, 0.000000000000000000, -1.000000000000000000 ) ) ;
#88310 = EDGE_LOOP ( 'NONE', ( #87847, #101443 ) ) ;
#88311 = EDGE_CURVE ( 'NONE', #104233, #26535, #93627, .T. ) ;
#88312 =( LENGTH_UNIT ( ) NAMED_UNIT ( * ) SI_UNIT ( .MILLI., .METRE. ) );
#88313 = CARTESIAN_POINT ( 'NONE',  ( -112.8182474800815243, -59.99999999999511147, 189.9060221141766931 ) ) ;
#88314 = CARTESIAN_POINT ( 'NONE',  ( 46.00000000000000000, 487.9611973796579605, 0.4748239133083901331 ) ) ;
#88315 = CARTESIAN_POINT ( 'NONE',  ( 76.54505153461919065, -60.00000000000001421, 189.0643905970971446 ) ) ;
#88316 = CYLINDRICAL_SURFACE ( 'NONE', #90776, 22.55262289886175964 ) ;
#88317 = SURFACE_STYLE_FILL_AREA ( #55387 ) ;
#88319 = CARTESIAN_POINT ( 'NONE',  ( 10.41105519390918843, -53.39685824552639559, 32.80285974031103535 ) ) ;
#88318 = CARTESIAN_POINT ( 'NONE',  ( -104.7861223705664599, -14.21045842199442433, 190.1679628257406875 ) ) ;
#88320 = ADVANCED_FACE ( 'NONE', ( #12790 ), #76824, .T. ) ;
#88321 = CARTESIAN_POINT ( 'NONE',  ( 102.6780276613828278, -38.00000000000000711, 166.4682704798183295 ) ) ;
#88322 = CARTESIAN_POINT ( 'NONE',  ( -8.559508646656370345, 51.83514083332403999, 1.531152949374564365 ) ) ;
#88323 = ADVANCED_FACE ( 'NONE', ( #79127 ), #3347, .T. ) ;
#88324 = CARTESIAN_POINT ( 'NONE',  ( -45.67848460884854944, -56.80937477045559802, 49.30617761660595022 ) ) ;
#88325 = CARTESIAN_POINT ( 'NONE',  ( 9.165151389911699198, 249.9999999999999432, 4.000000000000002665 ) ) ;
#88326 = EDGE_LOOP ( 'NONE', ( #18797, #59903, #97945, #30538 ) ) ;
#88327 = CARTESIAN_POINT ( 'NONE',  ( 0.7797239981822461363, 8.371946713100552273, -51.48153055130863009 ) ) ;
#88328 = CARTESIAN_POINT ( 'NONE',  ( -18.91781669292785395, 48.00000000000000000, 62.18610382930904734 ) ) ;
#88329 = MECHANICAL_DESIGN_GEOMETRIC_PRESENTATION_REPRESENTATION (  '', ( #57337 ), #33210 ) ;
#88330 = CARTESIAN_POINT ( 'NONE',  ( 3.412118697746299389, 304.8518027737318903, -10.00000000013250201 ) ) ;
#88331 = CARTESIAN_POINT ( 'NONE',  ( 6.849999999999999645, 4.618802153517001408, -8.000000000000000000 ) ) ;
#88332 = ORIENTED_EDGE ( 'NONE', *, *, #96676, .F. ) ;
#88333 = CARTESIAN_POINT ( 'NONE',  ( -10.09376787920347418, -12.27809184049766600, 17.28929750330553716 ) ) ;
#88334 = ORIENTED_EDGE ( 'NONE', *, *, #14307, .T. ) ;
#88335 = CARTESIAN_POINT ( 'NONE',  ( 105.3833277626438871, -29.99999999999387157, 194.8351416830720666 ) ) ;
#88336 = DIRECTION ( 'NONE',  ( 0.000000000000000000, -1.000000000000000000, 0.000000000000000000 ) ) ;
#88337 = AXIS2_PLACEMENT_3D ( 'NONE', #94775, #85613, #102848 ) ;
#88339 = EDGE_CURVE ( 'NONE', #85095, #11338, #103919, .T. ) ;
#88338 = CARTESIAN_POINT ( 'NONE',  ( 6.346112353299384168, 41.86049394308200533, -59.13213732590009641 ) ) ;
#88340 = FACE_BOUND ( 'NONE', #43890, .T. ) ;
#88341 = CARTESIAN_POINT ( 'NONE',  ( 92.39057177564670553, -30.00000000000000355, 102.4589548229546949 ) ) ;
#88342 = PRESENTATION_LAYER_ASSIGNMENT (  '', '', ( #24601 ) ) ;
#88343 = DIRECTION ( 'NONE',  ( 0.000000000000000000, 0.000000000000000000, 1.000000000000000000 ) ) ;
#88344 = ORIENTED_EDGE ( 'NONE', *, *, #24802, .T. ) ;
#88345 = VERTEX_POINT ( 'NONE', #14279 ) ;
#88346 = VERTEX_POINT ( 'NONE', #49291 ) ;
#88347 = DIRECTION ( 'NONE',  ( 0.3820442156512856013, 0.000000000000000000, -0.9241440457457885671 ) ) ;
#88348 = DIRECTION ( 'NONE',  ( -1.000000000000000000, -1.224606353822377258E-16, -0.000000000000000000 ) ) ;
#88349 = VECTOR ( 'NONE', #26566, 1000.000000000000000 ) ;
#88350 = CARTESIAN_POINT ( 'NONE',  ( 17.35892867067943257, 294.5707697310705839, -10.05973541782409164 ) ) ;
#88351 = ORIENTED_EDGE ( 'NONE', *, *, #75629, .F. ) ;
#88352 = DIRECTION ( 'NONE',  ( -1.000000000000000000, 0.000000000000000000, 0.000000000000000000 ) ) ;
#88353 = VERTEX_POINT ( 'NONE', #38590 ) ;
#88354 = DIRECTION ( 'NONE',  ( 1.000000000000000000, 1.224606353822377258E-16, 0.000000000000000000 ) ) ;
#88355 = CARTESIAN_POINT ( 'NONE',  ( 88.77998102494933619, -38.53862295708325547, 200.2196504074838117 ) ) ;
#88356 = CARTESIAN_POINT ( 'NONE',  ( 13.04323377975650189, 4.265506859525912020, 7.321301340633940669 ) ) ;
#88357 = CARTESIAN_POINT ( 'NONE',  ( 87.03565217808413479, -60.19692735285366325, -7.183757740799211255 ) ) ;
#88358 = CARTESIAN_POINT ( 'NONE',  ( 77.65976466551792612, -37.99999999999995737, 131.2189903408646785 ) ) ;
#88359 = CARTESIAN_POINT ( 'NONE',  ( 31.66509552703032782, 329.0881724405557520, 16.35203811063302837 ) ) ;
#88360 = CARTESIAN_POINT ( 'NONE',  ( 0.000000000000000000, 30.00000000000000000, 0.000000000000000000 ) ) ;
#88361 = DIRECTION ( 'NONE',  ( 0.000000000000000000, -1.000000000000000000, 0.000000000000000000 ) ) ;
#88362 = FACE_OUTER_BOUND ( 'NONE', #90838, .T. ) ;
#88363 = ORIENTED_EDGE ( 'NONE', *, *, #77663, .F. ) ;
#88364 = STYLED_ITEM ( 'NONE', ( #5355 ), #96508 ) ;
#88365 = CARTESIAN_POINT ( 'NONE',  ( 14.83349330513380693, 1.593028355512270962E-15, 0.000000000000000000 ) ) ;
#88367 = EDGE_CURVE ( 'NONE', #6335, #34066, #61309, .T. ) ;
#88366 = CARTESIAN_POINT ( 'NONE',  ( 16.52731600354976393, 43.98685737190850631, -87.77869701378344303 ) ) ;
#88368 = PRESENTATION_LAYER_ASSIGNMENT (  '', '', ( #102134 ) ) ;
#88369 = CARTESIAN_POINT ( 'NONE',  ( -4.557632849694865484, 143.2011664447169892, 5.000000000000000000 ) ) ;
#88370 = ORIENTED_EDGE ( 'NONE', *, *, #81791, .F. ) ;
#88371 = CYLINDRICAL_SURFACE ( 'NONE', #87191, 4.000000000000000000 ) ;
#88372 = CARTESIAN_POINT ( 'NONE',  ( -32.90087558584281879, 300.4243346777823263, 3.191413055959525291 ) ) ;
#88373 = CARTESIAN_POINT ( 'NONE',  ( -12.49723740359457658, -3.303264067464895870, -76.71011700628434937 ) ) ;
#88374 = UNCERTAINTY_MEASURE_WITH_UNIT (LENGTH_MEASURE( 1.000000000000000082E-05 ), #92104, 'distance_accuracy_value', 'NONE');
#88375 = DIRECTION ( 'NONE',  ( -1.000000000000000000, -1.224606353822377258E-16, -0.000000000000000000 ) ) ;
#88376 = CARTESIAN_POINT ( 'NONE',  ( 8.000000000000000000, -16.90624999999999645, -3.313708498984761608 ) ) ;
#88377 = CARTESIAN_POINT ( 'NONE',  ( 41.33631551152040373, -29.05874733539805632, 49.05523552014034294 ) ) ;
#88378 = EDGE_CURVE ( 'NONE', #42859, #1686, #58852, .T. ) ;
#88379 = CARTESIAN_POINT ( 'NONE',  ( 5.799999999999999822, 8.000000000000000000, 0.000000000000000000 ) ) ;
#88380 = ORIENTED_EDGE ( 'NONE', *, *, #64286, .T. ) ;
#88381 = CARTESIAN_POINT ( 'NONE',  ( 85.30112616295713224, -35.74003604604289563, 182.5928498885529052 ) ) ;
#88383 = EDGE_CURVE ( 'NONE', #41303, #22977, #78529, .T. ) ;
#88382 = DIRECTION ( 'NONE',  ( -1.000000000000000000, -1.224606353822377258E-16, -0.000000000000000000 ) ) ;
#88384 = SURFACE_STYLE_FILL_AREA ( #13931 ) ;
#88385 = ORIENTED_EDGE ( 'NONE', *, *, #64318, .T. ) ;
#88386 = CARTESIAN_POINT ( 'NONE',  ( 95.59699575574133235, -57.67169082706072913, 38.02165857417077177 ) ) ;
#88387 = CARTESIAN_POINT ( 'NONE',  ( -14.29190075645216851, 12.99999999999999289, 7.999999999999998224 ) ) ;
#88388 = CARTESIAN_POINT ( 'NONE',  ( -30.59734358679111565, 7.793378852367141896, 41.71107540015031390 ) ) ;
#88389 = CARTESIAN_POINT ( 'NONE',  ( 28.79546424415136485, 15.38851513919406777, 41.74402054108266924 ) ) ;
#88390 = CARTESIAN_POINT ( 'NONE',  ( -4.175893272572330339, -5.000000000001136868, -7.137815226410158864 ) ) ;
#88391 = CARTESIAN_POINT ( 'NONE',  ( 0.000000000000000000, 304.8518027762758038, 9.936999415352289589 ) ) ;
#88393 = CARTESIAN_POINT ( 'NONE',  ( -13.04352499521497855, 4.270345267762509778, 7.309431651496303139 ) ) ;
#88392 = CARTESIAN_POINT ( 'NONE',  ( 42.57401444030708149, 489.2306277911063717, 6.899166537239310060 ) ) ;
#88394 = EDGE_CURVE ( 'NONE', #61408, #90700, #52658, .T. ) ;
#88395 = CARTESIAN_POINT ( 'NONE',  ( 0.000000000000000000, -5.000000000000000000, 0.000000000000000000 ) ) ;
#88396 = CARTESIAN_POINT ( 'NONE',  ( 39.84233570596349949, 333.3323931548420660, 19.23895789620553032 ) ) ;
#88397 = CARTESIAN_POINT ( 'NONE',  ( -27.85247631086664200, 36.60167368073183525, -7.792110844177867257 ) ) ;
#88398 = CARTESIAN_POINT ( 'NONE',  ( -9.858548355958978604, -23.16810237002645678, -30.52285683705125052 ) ) ;
#88399 = CARTESIAN_POINT ( 'NONE',  ( -1.101454001170008912, 14.95253250404441658, -12.16137996778341268 ) ) ;
#88400 = AXIS2_PLACEMENT_3D ( 'NONE', #58057, #33818, #34893 ) ;
#88401 = EDGE_CURVE ( 'NONE', #102469, #53546, #96815, .T. ) ;
#88402 = CARTESIAN_POINT ( 'NONE',  ( -102.2211543079583294, -38.00000000000004974, 182.8469250058557805 ) ) ;
#88403 = CIRCLE ( 'NONE', #21296, 4.250000000000000000 ) ;
#88404 = EDGE_LOOP ( 'NONE', ( #26667, #4000, #1220, #59699 ) ) ;
#88405 = FILL_AREA_STYLE ('',( #63610 ) ) ;
#88406 = DIRECTION ( 'NONE',  ( -1.000000000000000000, -0.000000000000000000, -0.000000000000000000 ) ) ;
#88407 =( GEOMETRIC_REPRESENTATION_CONTEXT ( 3 ) GLOBAL_UNCERTAINTY_ASSIGNED_CONTEXT ( ( #54546 ) ) GLOBAL_UNIT_ASSIGNED_CONTEXT ( ( #1217, #17983, #9859 ) ) REPRESENTATION_CONTEXT ( 'NONE', 'WORKASPACE' ) );
#88408 = CARTESIAN_POINT ( 'NONE',  ( -23.91971553424620112, -19.70479182448596589, -33.18013212959203173 ) ) ;
#88410 = CARTESIAN_POINT ( 'NONE',  ( -57.64009741160396061, -60.22830627530903058, -30.33965759735865575 ) ) ;
#88409 = CARTESIAN_POINT ( 'NONE',  ( 14.54015256618498775, 9.738273119607207207, 0.000000000000000000 ) ) ;
#88411 = EDGE_LOOP ( 'NONE', ( #36731, #6572, #78113, #90366, #28981 ) ) ;
#88412 = CARTESIAN_POINT ( 'NONE',  ( 4.250000000000000000, 0.000000000000000000, -6.235812796514431433 ) ) ;
#88414 = ORIENTED_EDGE ( 'NONE', *, *, #12229, .T. ) ;
#88413 = CIRCLE ( 'NONE', #103880, 4.400000000000000355 ) ;
#88415 = CARTESIAN_POINT ( 'NONE',  ( 6.692588830498428898, 7.935834885954428763, -0.04058884017440173020 ) ) ;
#88416 = CARTESIAN_POINT ( 'NONE',  ( 0.000000000000000000, 0.000000000000000000, 0.000000000000000000 ) ) ;
#88417 = CARTESIAN_POINT ( 'NONE',  ( -92.53465222392649991, -60.00000000000000711, -1.764304992001874517 ) ) ;
#88418 = VERTEX_POINT ( 'NONE', #80605 ) ;
#88419 = CARTESIAN_POINT ( 'NONE',  ( 28.58349330513380337, 1.593028355512270567E-15, 0.000000000000000000 ) ) ;
#88420 = CARTESIAN_POINT ( 'NONE',  ( -7.622868062079398932, 54.26469983982431700, -1.949254839742071033 ) ) ;
#88421 = CARTESIAN_POINT ( 'NONE',  ( 100.4533534623010098, -60.28154197531982561, 195.5193666514165614 ) ) ;
#88423 = CARTESIAN_POINT ( 'NONE',  ( 5.833333333333329485, -4.000000000000003553, 103.8776713793258608 ) ) ;
#88422 = DIRECTION ( 'NONE',  ( -0.5735764363510494901, -0.8191520442889894671, 0.000000000000000000 ) ) ;
#88424 = CARTESIAN_POINT ( 'NONE',  ( -79.90040665909508277, -60.36515567690381090, 174.0697010744071065 ) ) ;
#88425 = EDGE_LOOP ( 'NONE', ( #95050, #26406, #28049, #3570, #105326 ) ) ;
#88426 = AXIS2_PLACEMENT_3D ( 'NONE', #55318, #5719, #105475 ) ;
#88427 = ORIENTED_EDGE ( 'NONE', *, *, #10486, .T. ) ;
#88428 = ORIENTED_EDGE ( 'NONE', *, *, #28365, .T. ) ;
#88429 = LINE ( 'NONE', #31278, #53481 ) ;
#88430 = VECTOR ( 'NONE', #95653, 1000.000000000000000 ) ;
#88431 = CARTESIAN_POINT ( 'NONE',  ( -5.000000000000000000, -13.82147230827991713, 10.98112731479256254 ) ) ;
#88432 =( NAMED_UNIT ( * ) PLANE_ANGLE_UNIT ( ) SI_UNIT ( $, .RADIAN. ) );
#88433 = ORIENTED_EDGE ( 'NONE', *, *, #28634, .F. ) ;
#88434 = ADVANCED_FACE ( 'NONE', ( #24015 ), #56314, .F. ) ;
#88435 = PRESENTATION_LAYER_ASSIGNMENT (  '', '', ( #526 ) ) ;
#88436 = CARTESIAN_POINT ( 'NONE',  ( 0.000000000000000000, 4.898587196589412829E-16, -4.000000000000000000 ) ) ;
#88437 = CARTESIAN_POINT ( 'NONE',  ( -96.25446706653225704, -57.62198180035323247, 204.5564252943773340 ) ) ;
#88438 = DIRECTION ( 'NONE',  ( -0.8191520442889881348, 1.003171929053520186E-16, 0.5735764363510513775 ) ) ;
#88439 = LINE ( 'NONE', #81376, #59982 ) ;
#88440 = CIRCLE ( 'NONE', #72853, 5.000000000000000000 ) ;
#88441 = DIRECTION ( 'NONE',  ( 0.000000000000000000, 1.000000000000000000, 0.000000000000000000 ) ) ;
#88442 = CARTESIAN_POINT ( 'NONE',  ( 6.849999999999999645, -4.618802153517012954, -8.000000000000001776 ) ) ;
#88443 = CARTESIAN_POINT ( 'NONE',  ( 95.18118770502717041, -60.00000000000013500, -7.509903379402337542 ) ) ;
#88444 = EDGE_CURVE ( 'NONE', #17510, #64937, #40636, .T. ) ;
#88445 = CARTESIAN_POINT ( 'NONE',  ( -64.23299091672136285, -59.99999999999999289, 125.0187485388276656 ) ) ;
#88446 = ADVANCED_FACE ( 'NONE', ( #18023 ), #5333, .F. ) ;
#88447 = CARTESIAN_POINT ( 'NONE',  ( -53.32813900909374638, -53.37880559940036562, 62.19817634995050781 ) ) ;
#88448 = ORIENTED_EDGE ( 'NONE', *, *, #20283, .T. ) ;
#88449 = CARTESIAN_POINT ( 'NONE',  ( -1.344569080228518650E-17, 21.85270131633358304, -7.000000000000011546 ) ) ;
#88450 = ORIENTED_EDGE ( 'NONE', *, *, #88636, .F. ) ;
#88451 = CARTESIAN_POINT ( 'NONE',  ( -99.57148504860369087, -37.80425350881786528, 191.2424562810986686 ) ) ;
#88452 = DIRECTION ( 'NONE',  ( 0.000000000000000000, -0.5000000000000016653, -0.8660254037844375974 ) ) ;
#88453 = ORIENTED_EDGE ( 'NONE', *, *, #44672, .F. ) ;
#88454 = CARTESIAN_POINT ( 'NONE',  ( 19.36135695977271709, 49.91008391659885035, 61.13655276434777619 ) ) ;
#88455 = CARTESIAN_POINT ( 'NONE',  ( 80.35317488720673396, -38.35617844620870187, -26.29242304138821851 ) ) ;
#88456 = CARTESIAN_POINT ( 'NONE',  ( 14.29190075645216673, 6.456385560668102208, 7.561819230143447257 ) ) ;
#88457 = DIRECTION ( 'NONE',  ( -1.000000000000000000, -1.224606353822377258E-16, -0.000000000000000000 ) ) ;
#88458 = B_SPLINE_CURVE_WITH_KNOTS ( 'NONE', 3,
 ( #99302, #92823, #1672, #75027, #99848, #58881, #17895, #13481, #37283, #20600, #28662, #96020, #52902, #78233, #21111, #11353, #86358, #12423, #77178, #4349, #85269, #94441, #36230, #79291, #69627, #12951, #45871, #62596, #70149, #45355, #3289, #78751, #29210, #103054 ),
 .UNSPECIFIED., .F., .F.,
 ( 4, 2, 2, 2, 2, 2, 2, 2, 2, 2, 2, 2, 2, 2, 2, 2, 4 ),
 ( 0.000000000000000000, 0.0007951492273476391814, 0.001590298454695278363, 0.002385447682042917544, 0.003180596909390556726, 0.003975746136738195907, 0.004770895364085835089, 0.005566044591433473403, 0.006361193818781111717, 0.007156343046128750031, 0.007951492273476388345, 0.008746641500824025792, 0.009541790728171663238, 0.01033693995551930069, 0.01113208918286693987, 0.01192723841021457558, 0.01272238763756221476 ),
 .UNSPECIFIED. ) ;
#88459 = EDGE_CURVE ( 'NONE', #91423, #91282, #34433, .T. ) ;
#88460 = CARTESIAN_POINT ( 'NONE',  ( -43.00000000000001421, 485.2629658518202973, -2.796394914059383119 ) ) ;
#88462 = CARTESIAN_POINT ( 'NONE',  ( 63.00516225510686752, -29.99999999999999289, 74.69021731496640371 ) ) ;
#88461 = UNCERTAINTY_MEASURE_WITH_UNIT (LENGTH_MEASURE( 1.000000000000000082E-05 ), #31891, 'distance_accuracy_value', 'NONE');
#88463 = DIRECTION ( 'NONE',  ( 0.000000000000000000, -1.000000000000000000, 0.000000000000000000 ) ) ;
#88464 = CARTESIAN_POINT ( 'NONE',  ( 32.62207953394533178, -5.000000000000000000, 6.123233995736768255E-16 ) ) ;
#88465 = CARTESIAN_POINT ( 'NONE',  ( -1.250037285469578707, 34.50112784842972502, 28.81831915451376602 ) ) ;
#88466 = CARTESIAN_POINT ( 'NONE',  ( -36.23446467943408322, 484.5294442009995350, -2.438443429317435740 ) ) ;
#88467 = B_SPLINE_CURVE_WITH_KNOTS ( 'NONE', 3,
 ( #99727, #19400, #27485, #60361, #91649, #51159, #51699, #44159, #2078, #93236, #84077, #1541 ),
 .UNSPECIFIED., .F., .F.,
 ( 4, 2, 2, 2, 2, 4 ),
 ( 8.414750032627943091E-17, 0.001311657711814073106, 0.002623315423628062078, 0.003279144279535067298, 0.003934973135442072084, 0.005246630847256086860 ),
 .UNSPECIFIED. ) ;
#88468 = EDGE_LOOP ( 'NONE', ( #72825, #61757 ) ) ;
#88469 = VERTEX_POINT ( 'NONE', #30779 ) ;
#88470 = CARTESIAN_POINT ( 'NONE',  ( 49.15655608998503112, -29.13270878632327054, 46.07185368943500237 ) ) ;
#88471 = CARTESIAN_POINT ( 'NONE',  ( 0.000000000000000000, 294.8518027762758038, -10.00000000000000178 ) ) ;
#88472 = DIRECTION ( 'NONE',  ( 0.000000000000000000, -1.000000000000000000, 0.000000000000000000 ) ) ;
#88473 = CARTESIAN_POINT ( 'NONE',  ( -102.1566426654864301, -38.44188724825352210, 199.6156023558743584 ) ) ;
#88474 = EDGE_LOOP ( 'NONE', ( #27901, #43987 ) ) ;
#88475 = CARTESIAN_POINT ( 'NONE',  ( 91.29669025949715433, -38.40056992187813734, -10.42823402827028190 ) ) ;
#88476 = CARTESIAN_POINT ( 'NONE',  ( 12.81150014802426362, 18.86618361353973938, -8.103187572974331232 ) ) ;
#88477 = CARTESIAN_POINT ( 'NONE',  ( -6.075687308901098760, 41.99394926078448265, -68.91429205814512216 ) ) ;
#88478 = FILL_AREA_STYLE ('',( #38355 ) ) ;
#88479 = CARTESIAN_POINT ( 'NONE',  ( 105.6700157783516829, -60.15124779082972140, 156.3737876120203794 ) ) ;
#88480 = FILL_AREA_STYLE ('',( #105702 ) ) ;
#88481 = CARTESIAN_POINT ( 'NONE',  ( 13.63130828375568981, 294.5445729804733901, -10.06530370901874250 ) ) ;
#88483 = CARTESIAN_POINT ( 'NONE',  ( 0.4033376246892543260, -7.198601258566906580, 0.5316568767328693212 ) ) ;
#88482 = AXIS2_PLACEMENT_3D ( 'NONE', #72596, #46217, #79105 ) ;
#88484 = FILL_AREA_STYLE ('',( #45899 ) ) ;
#88485 = CARTESIAN_POINT ( 'NONE',  ( 78.99695195452900975, -60.00000000000000000, 194.6422132151330118 ) ) ;
#88486 = CIRCLE ( 'NONE', #79843, 7.000000000000006217 ) ;
#88487 =( GEOMETRIC_REPRESENTATION_CONTEXT ( 3 ) GLOBAL_UNCERTAINTY_ASSIGNED_CONTEXT ( ( #4971 ) ) GLOBAL_UNIT_ASSIGNED_CONTEXT ( ( #58294, #75540, #1635 ) ) REPRESENTATION_CONTEXT ( 'NONE', 'WORKASPACE' ) );
#88488 = ORIENTED_EDGE ( 'NONE', *, *, #33542, .T. ) ;
#88489 = CARTESIAN_POINT ( 'NONE',  ( 55.72842314015646537, -56.85053476136143757, 69.22857699785234331 ) ) ;
#88490 = CARTESIAN_POINT ( 'NONE',  ( -33.47685715990249378, 300.6314875565626608, -0.6996443904386956403 ) ) ;
#88491 = CARTESIAN_POINT ( 'NONE',  ( 7.744168461338430731, 33.46254061715157491, 2.019395720771558267 ) ) ;
#88492 = CARTESIAN_POINT ( 'NONE',  ( -7.551560007654700257, 26.99089648193007562, -2.648022159607827497 ) ) ;
#88493 = ORIENTED_EDGE ( 'NONE', *, *, #102147, .T. ) ;
#88495 = CARTESIAN_POINT ( 'NONE',  ( -14.86325825540062517, 23.03589162952219382, 1.252617022373717193 ) ) ;
#88494 = CARTESIAN_POINT ( 'NONE',  ( -100.3096506332310014, -38.46452049353877101, 200.4061333699972920 ) ) ;
#88496 = CARTESIAN_POINT ( 'NONE',  ( 2.093983074874242067, -3.000000000000000444, -7.791781413346524410 ) ) ;
#88497 = CARTESIAN_POINT ( 'NONE',  ( 23.67596972946360268, 306.0428419988428459, 9.198869806892925993 ) ) ;
#88498 = CARTESIAN_POINT ( 'NONE',  ( -42.87058980226115068, 464.8475010141946768, 15.35427200435808892 ) ) ;
#88499 = CARTESIAN_POINT ( 'NONE',  ( 3.313708498984762052, -31.71874999999999645, -8.000000000000000000 ) ) ;
#88500 = CARTESIAN_POINT ( 'NONE',  ( -8.737863884124131175, -5.000000000000002665, -79.96381019768853093 ) ) ;
#88501 = EDGE_CURVE ( 'NONE', #79135, #85853, #22689, .T. ) ;
#88502 = B_SPLINE_CURVE_WITH_KNOTS ( 'NONE', 3,
 ( #99374, #72979, #24490, #82140, #89724, #40624, #40105, #64393, #90785, #16898, #73510, #66492, #98334, #105884, #48703 ),
 .UNSPECIFIED., .F., .F.,
 ( 4, 1, 1, 1, 1, 1, 1, 1, 2, 2, 4 ),
 ( 0.000000000000000000, 0.2500000000000872080, 0.3750000000001318390, 0.4375000000001538214, 0.4687500000001610934, 0.4843750000001644240, 0.4921875000001630918, 0.4960937500001587064, 0.4980468750001556533, 0.5000000000001525446, 1.000000000000000000 ),
 .UNSPECIFIED. ) ;
#88503 = CARTESIAN_POINT ( 'NONE',  ( 36.36650669486618881, 1.474610560812782335E-15, 0.000000000000000000 ) ) ;
#88504 = VERTEX_POINT ( 'NONE', #85961 ) ;
#88505 = CARTESIAN_POINT ( 'NONE',  ( 84.74071589511709135, -28.95261022299601095, 169.9338770228943076 ) ) ;
#88506 = CARTESIAN_POINT ( 'NONE',  ( 8.350191400314127321, 31.24596923992393016, -1.301042606982604532E-15 ) ) ;
#88507 = CARTESIAN_POINT ( 'NONE',  ( -34.01505262803539864, 439.9177708686792130, 24.30869736368872935 ) ) ;
#88508 = ORIENTED_EDGE ( 'NONE', *, *, #50073, .T. ) ;
#88509 = CARTESIAN_POINT ( 'NONE',  ( 7.286648454926750781E-15, 45.50000000000000711, -59.50000000000000000 ) ) ;
#88510 = CIRCLE ( 'NONE', #64493, 3.400000000000000355 ) ;
#88511 = CARTESIAN_POINT ( 'NONE',  ( 5.885102640078956782, -4.999999999999984901, -15.35622078683712743 ) ) ;
#88512 = CARTESIAN_POINT ( 'NONE',  ( 26.35354840416186661, 34.76403232285502298, -9.818490863206431385 ) ) ;
#88513 = LINE ( 'NONE', #89567, #74439 ) ;
#88514 = CARTESIAN_POINT ( 'NONE',  ( 6.201636426617084574E-15, 39.99999999999999289, -70.00365511371767013 ) ) ;
#88515 = CARTESIAN_POINT ( 'NONE',  ( -29.68315524077004497, 8.302504244945346557, -42.10535821593474282 ) ) ;
#88516 = B_SPLINE_CURVE_WITH_KNOTS ( 'NONE', 3,
 ( #52614, #3009, #35961, #36492, #45088, #77967, #63401, #41087, #98773, #33024, #40551, #55264, #46655, #4617, #79553, #16271, #13745, #24925 ),
 .UNSPECIFIED., .F., .F.,
 ( 4, 2, 2, 2, 2, 2, 2, 2, 4 ),
 ( 0.007125446813973603487, 0.007629686116325599433, 0.008133925418677596247, 0.008638164721029592194, 0.009142404023381588141, 0.009646643325733585822, 0.01015088262808558003, 0.01065512193043757772, 0.01115936123278957366 ),
 .UNSPECIFIED. ) ;
#88517 = ADVANCED_FACE ( 'NONE', ( #102110 ), #85410, .T. ) ;
#88518 = EDGE_LOOP ( 'NONE', ( #13267, #16392 ) ) ;
#88519 = CIRCLE ( 'NONE', #19658, 4.000000000000001776 ) ;
#88520 = CARTESIAN_POINT ( 'NONE',  ( 38.81963054373370881, 25.17304704673439986, 12.35078328273734805 ) ) ;
#88521 = FACE_OUTER_BOUND ( 'NONE', #97881, .T. ) ;
#88523 = CARTESIAN_POINT ( 'NONE',  ( -11.41577687521523643, 13.93101530882450589, -9.960789481687990943 ) ) ;
#88522 = DIRECTION ( 'NONE',  ( -1.000000000000000000, 0.000000000000000000, 0.000000000000000000 ) ) ;
#88524 = CARTESIAN_POINT ( 'NONE',  ( 7.188101187500001821, -22.06250000204838813, -2.977408999572650483 ) ) ;
#88525 = CARTESIAN_POINT ( 'NONE',  ( 21.51569398614867623, 294.9107018935607698, -9.987480606144499617 ) ) ;
#88526 = EDGE_CURVE ( 'NONE', #17301, #69972, #48506, .T. ) ;
#88527 = ORIENTED_EDGE ( 'NONE', *, *, #82761, .T. ) ;
#88528 = DIRECTION ( 'NONE',  ( 0.000000000000000000, -1.000000000000000000, 0.000000000000000000 ) ) ;
#88529 = CARTESIAN_POINT ( 'NONE',  ( 23.99554787606954420, 25.16759095613464225, 32.93816323708791316 ) ) ;
#88530 = CARTESIAN_POINT ( 'NONE',  ( -4.678819457397887405, 143.9212778189118751, -5.000000000000000000 ) ) ;
#88531 = ADVANCED_FACE ( 'NONE', ( #102652 ), #35599, .F. ) ;
#88532 = CARTESIAN_POINT ( 'NONE',  ( -43.21901510197800889, 436.3299561109158162, 19.40633274081965709 ) ) ;
#88533 = CARTESIAN_POINT ( 'NONE',  ( -34.92499999999994742, 1.040949779275250140E-15, -8.500000000000000000 ) ) ;
#88534 = AXIS2_PLACEMENT_3D ( 'NONE', #100501, #93497, #9349 ) ;
#88535 = VERTEX_POINT ( 'NONE', #3427 ) ;
#88536 = CARTESIAN_POINT ( 'NONE',  ( 43.86011134669068667, 435.5786695946740679, 9.518646890165630481 ) ) ;
#88537 = CARTESIAN_POINT ( 'NONE',  ( -33.00496812084397646, 465.6658704666172639, 15.15901827095664522 ) ) ;
#88538 = ORIENTED_EDGE ( 'NONE', *, *, #103239, .T. ) ;
#88539 = DIRECTION ( 'NONE',  ( -0.000000000000000000, -1.000000000000000000, -0.000000000000000000 ) ) ;
#88540 = SURFACE_STYLE_FILL_AREA ( #55602 ) ;
#88541 = PRESENTATION_STYLE_ASSIGNMENT (( #71803 ) ) ;
#88542 = CARTESIAN_POINT ( 'NONE',  ( -106.5419819426516881, -60.00000000000000711, 119.7747142723297742 ) ) ;
#88543 = DIRECTION ( 'NONE',  ( 0.000000000000000000, 0.000000000000000000, 1.000000000000000000 ) ) ;
#88544 = TOROIDAL_SURFACE ( 'NONE', #93790, 65.50000000000000000, 0.5000000000000000000 ) ;
#88545 =( NAMED_UNIT ( * ) SI_UNIT ( $, .STERADIAN. ) SOLID_ANGLE_UNIT ( ) );
#88546 = CARTESIAN_POINT ( 'NONE',  ( 16.08349330513380337, 1.593028355512270567E-15, 0.000000000000000000 ) ) ;
#88547 = DIRECTION ( 'NONE',  ( -0.000000000000000000, -0.000000000000000000, 1.000000000000000000 ) ) ;
#88548 = CARTESIAN_POINT ( 'NONE',  ( -82.82730212088782196, -46.49498115257645736, 178.5359483646249998 ) ) ;
#88549 = VERTEX_POINT ( 'NONE', #43875 ) ;
#88550 = CARTESIAN_POINT ( 'NONE',  ( 35.11650669486618170, -3.851859888774471706E-31, 4.000000000000000888 ) ) ;
#88551 = ORIENTED_EDGE ( 'NONE', *, *, #103018, .F. ) ;
#88552 =( LENGTH_UNIT ( ) NAMED_UNIT ( * ) SI_UNIT ( .MILLI., .METRE. ) );
#88553 = CARTESIAN_POINT ( 'NONE',  ( 1.000000000000000000, -59.21823443913439178, 7.425173686811099572 ) ) ;
#88554 = ADVANCED_BREP_SHAPE_REPRESENTATION ( '', ( #88996, #10728 ), #33394 ) ;
#88555 = CARTESIAN_POINT ( 'NONE',  ( -86.56691879974580672, -60.14943795851970521, 24.17102811031225684 ) ) ;
#88556 = CARTESIAN_POINT ( 'NONE',  ( 4.000000000000000888, 2.111459998529851557E-18, 0.000000000000000000 ) ) ;
#88557 =( NAMED_UNIT ( * ) PLANE_ANGLE_UNIT ( ) SI_UNIT ( $, .RADIAN. ) );
#88558 = CARTESIAN_POINT ( 'NONE',  ( 9.240146679348617553, 12.02903014932230263, -5.000000000000000888 ) ) ;
#88559 = DIRECTION ( 'NONE',  ( -1.000000000000000000, -1.224606353822377258E-16, -0.000000000000000000 ) ) ;
#88560 = CARTESIAN_POINT ( 'NONE',  ( 23.21751746555303342, 25.25267828308493989, 33.20617127781017075 ) ) ;
#88561 = CARTESIAN_POINT ( 'NONE',  ( 106.6028846201213440, -30.00000000000002487, 192.6838848496860521 ) ) ;
#88562 = CARTESIAN_POINT ( 'NONE',  ( -90.56108803656626094, -30.00000000000000711, 34.47189148671483849 ) ) ;
#88563 = CARTESIAN_POINT ( 'NONE',  ( -61.04315145770602413, -42.96496502653089067, 76.66717857525411262 ) ) ;
#88564 = EDGE_LOOP ( 'NONE', ( #105172, #47765, #2032, #53649 ) ) ;
#88565 = CARTESIAN_POINT ( 'NONE',  ( 51.81827666034978819, 39.42541842817299624, 39.69774341223477165 ) ) ;
#88566 = CARTESIAN_POINT ( 'NONE',  ( 82.32787579396226363, -60.00000000001609379, 201.4521251157181325 ) ) ;
#88567 = VERTEX_POINT ( 'NONE', #76770 ) ;
#88568 = CARTESIAN_POINT ( 'NONE',  ( 3.050709723766003911, -46.43461503410409819, 31.62373175404598769 ) ) ;
#88569 = CARTESIAN_POINT ( 'NONE',  ( 2.977408999572652260, -19.81250000204838457, 7.188101187500000044 ) ) ;
#88570 = LINE ( 'NONE', #64304, #63172 ) ;
#88571 = ORIENTED_EDGE ( 'NONE', *, *, #20820, .T. ) ;
#88572 = CARTESIAN_POINT ( 'NONE',  ( -5.656854249492379694, -27.12500000409677270, -5.656854249492380582 ) ) ;
#88573 = VERTEX_POINT ( 'NONE', #2873 ) ;
#88574 = DIRECTION ( 'NONE',  ( 0.000000000000000000, 0.000000000000000000, 1.000000000000000000 ) ) ;
#88575 = CIRCLE ( 'NONE', #55821, 3.309500000000001663 ) ;
#88576 = CARTESIAN_POINT ( 'NONE',  ( -94.73029569914376680, -59.99999999999997868, 47.21885834219733624 ) ) ;
#88577 = CARTESIAN_POINT ( 'NONE',  ( 36.73867238004162061, 390.4005144646481540, 5.886277538419430577 ) ) ;
#88578 = CARTESIAN_POINT ( 'NONE',  ( 7.188101187500000044, -24.03125000204838457, 0.000000000000000000 ) ) ;
#88579 = CARTESIAN_POINT ( 'NONE',  ( 0.000000000000000000, 0.000000000000000000, 0.000000000000000000 ) ) ;
#88580 = EDGE_CURVE ( 'NONE', #76997, #6487, #87231, .T. ) ;
#88581 = CARTESIAN_POINT ( 'NONE',  ( 37.06438722625302518, 1.482358050883964840E-15, 0.000000000000000000 ) ) ;
#88582 = DIRECTION ( 'NONE',  ( 0.000000000000000000, -1.000000000000000000, 0.000000000000000000 ) ) ;
#88583 = CARTESIAN_POINT ( 'NONE',  ( 6.145467200819017428, 48.00000000000000000, -92.99666842291193802 ) ) ;
#88584 = ADVANCED_FACE ( 'NONE', ( #69238 ), #41855, .F. ) ;
#88585 = CARTESIAN_POINT ( 'NONE',  ( 15.11650669486618881, 1.474610560812782335E-15, 0.000000000000000000 ) ) ;
#88586 = CARTESIAN_POINT ( 'NONE',  ( -40.00273928030988912, 314.7263521513793307, 2.786061341313883055 ) ) ;
#88587 = CARTESIAN_POINT ( 'NONE',  ( 30.88056822677182112, 309.1697570866494971, -8.545327163282022909 ) ) ;
#88588 = AXIS2_PLACEMENT_3D ( 'NONE', #15523, #56503, #89950 ) ;
#88589 = CARTESIAN_POINT ( 'NONE',  ( -36.22558170428006719, -46.43489304307155408, 37.39699883427675076 ) ) ;
#88590 = EDGE_LOOP ( 'NONE', ( #28628, #28632, #8548, #68887, #40160 ) ) ;
#88591 = CARTESIAN_POINT ( 'NONE',  ( -14.63464771654506791, 41.99999999996094857, -88.44359770654935460 ) ) ;
#88592 = CARTESIAN_POINT ( 'NONE',  ( 40.62864974475749591, -25.69507913308015645, 36.04227385710505160 ) ) ;
#88593 = CARTESIAN_POINT ( 'NONE',  ( -10.45706415777859455, -1.734723475976807094E-15, 13.60704923275178935 ) ) ;
#88594 = ORIENTED_EDGE ( 'NONE', *, *, #97724, .T. ) ;
#88595 = CARTESIAN_POINT ( 'NONE',  ( 33.95909125845500398, 464.3583096732872377, 17.59538848573625458 ) ) ;
#88596 = CARTESIAN_POINT ( 'NONE',  ( -66.69118985233596675, -38.33596727070246146, 120.0288781097716537 ) ) ;
#88597 = ORIENTED_EDGE ( 'NONE', *, *, #100725, .F. ) ;
#88599 = CARTESIAN_POINT ( 'NONE',  ( -29.01988888469873018, 321.8047804620298393, 14.12772110426748284 ) ) ;
#88598 = CARTESIAN_POINT ( 'NONE',  ( 6.663127973346361976, -3.846958729056464410, -6.460793508093581217 ) ) ;
#88600 = CARTESIAN_POINT ( 'NONE',  ( 15.64272365568285217, 37.16721670561516078, 22.45732330511662056 ) ) ;
#88601 = CARTESIAN_POINT ( 'NONE',  ( -34.85398657184737914, 481.6352825967676381, 14.59780011294850866 ) ) ;
#88602 = CARTESIAN_POINT ( 'NONE',  ( 6.289692432696785573, -1.240526984323783911E-13, -6.828989928337169779 ) ) ;
#88603 = CARTESIAN_POINT ( 'NONE',  ( -38.69545490169445401, 437.5444261472158587, 4.829293893630138612 ) ) ;
#88604 = CARTESIAN_POINT ( 'NONE',  ( -49.27896781154974803, 13.08675713149239250, -15.56311823694480445 ) ) ;
#88605 = CYLINDRICAL_SURFACE ( 'NONE', #36714, 5.000000000000000000 ) ;
#88606 = CARTESIAN_POINT ( 'NONE',  ( 100.7656204750565649, -60.00000000000001421, 85.52486764147262477 ) ) ;
#88607 = CARTESIAN_POINT ( 'NONE',  ( -44.08840282922849241, 485.7747746244170912, 4.178803824085661311 ) ) ;
#88608 = FACE_OUTER_BOUND ( 'NONE', #80641, .T. ) ;
#88609 = CARTESIAN_POINT ( 'NONE',  ( -34.47176506790572859, 489.5748983164075980, 11.69726377706254361 ) ) ;
#88610 = VERTEX_POINT ( 'NONE', #8049 ) ;
#88611 = CARTESIAN_POINT ( 'NONE',  ( -65.15920822928832479, -30.00000000000001066, 80.64472866489825265 ) ) ;
#88612 = ORIENTED_EDGE ( 'NONE', *, *, #48050, .F. ) ;
#88613 = CARTESIAN_POINT ( 'NONE',  ( 9.500000000000000000, -5.000000000000000000, -20.99851272547260095 ) ) ;
#88614 = CARTESIAN_POINT ( 'NONE',  ( -16.03050524006218325, 4.255071776854646437, 2.702720838600184639 ) ) ;
#88615 = CARTESIAN_POINT ( 'NONE',  ( 0.000000000000000000, 0.000000000000000000, -1.446714285714285841 ) ) ;
#88616 = CARTESIAN_POINT ( 'NONE',  ( 0.000000000000000000, 0.000000000000000000, -7.999999999999994671 ) ) ;
#88617 = CARTESIAN_POINT ( 'NONE',  ( 4.401442555609581635E-16, -25.15625000204838813, -7.188101187500000044 ) ) ;
#88618 = DIRECTION ( 'NONE',  ( 0.000000000000000000, -1.000000000000000000, 0.000000000000000000 ) ) ;
#88619 = FACE_OUTER_BOUND ( 'NONE', #10456, .T. ) ;
#88620 = CARTESIAN_POINT ( 'NONE',  ( 7.179418447820448357, 41.32597146628941687, -70.21787980165106546 ) ) ;
#88621 = VERTEX_POINT ( 'NONE', #98128 ) ;
#88622 = EDGE_CURVE ( 'NONE', #96540, #82575, #73306, .T. ) ;
#88623 = STYLED_ITEM ( 'NONE', ( #76636 ), #27981 ) ;
#88625 = VERTEX_POINT ( 'NONE', #97580 ) ;
#88624 = CARTESIAN_POINT ( 'NONE',  ( -7.500000000000007105, 40.18760986260523538, -59.65696556657620420 ) ) ;
#88626 = CARTESIAN_POINT ( 'NONE',  ( 78.92104432068852304, -56.84203907387598775, 159.0975971619027121 ) ) ;
#88627 = CARTESIAN_POINT ( 'NONE',  ( 14.63960045772751428, 2.604522098972499311, -3.217332696223609290 ) ) ;
#88628 = VERTEX_POINT ( 'NONE', #106201 ) ;
#88629 = CARTESIAN_POINT ( 'NONE',  ( -12.50000000000000533, 34.77083264068856039, -54.03046856804895270 ) ) ;
#88630 = CARTESIAN_POINT ( 'NONE',  ( -0.9524572379025817437, 13.93511301620387499, -51.31333095019984825 ) ) ;
#88631 = CARTESIAN_POINT ( 'NONE',  ( 5.082755093536324154, -11.84375000204838635, 5.082755093536326818 ) ) ;
#88632 = CARTESIAN_POINT ( 'NONE',  ( 0.000000000000000000, 0.000000000000000000, 0.000000000000000000 ) ) ;
#88633 =( BOUNDED_SURFACE ( )  B_SPLINE_SURFACE ( 3, 2, ( 
 ( #99560, #25740, #65615 ),
 ( #58595, #64560, #49418 ),
 ( #91500, #56435, #72633 ),
 ( #17610, #97427, #23588 ),
 ( #89368, #84994, #27336 ),
 ( #11616, #44545, #51002 ),
 ( #93081, #18691, #11077 ),
 ( #77434, #61260, #9482 ),
 ( #35411, #83921, #43472 ),
 ( #1926, #19777, #100100 ) ),
 .UNSPECIFIED., .F., .F., .F. ) 
 B_SPLINE_SURFACE_WITH_KNOTS ( ( 4, 2, 2, 2, 4 ),
 ( 3, 3 ),
 ( 0.002450517525418897339, 0.003060732775749464701, 0.003670948026080031630, 0.004891378526741165488, 0.007332239528063434070 ),
 ( 0.000000000000000000, 1.000000000000000000 ),
 .UNSPECIFIED. ) 
 GEOMETRIC_REPRESENTATION_ITEM ( )  RATIONAL_B_SPLINE_SURFACE ( (
 ( 1.000000000000000000, 0.7071067811865481278, 1.000000000000000000),
 ( 1.000000000000000000, 0.7344063550101938009, 1.000000000000000000),
 ( 1.000000000000000000, 0.7590375248711013212, 1.000000000000000000),
 ( 1.000000000000000000, 0.8038331608704091247, 1.000000000000000000),
 ( 1.000000000000000000, 0.8240352460866575690, 1.000000000000000000),
 ( 1.000000000000000000, 0.8791017378331893450, 1.000000000000000000),
 ( 1.000000000000000000, 0.9085032776980893621, 1.000000000000000000),
 ( 1.000000000000000000, 0.9784170511696810291, 1.000000000000000000),
 ( 1.000000000000000000, 0.9996598051696602427, 1.000000000000000000),
 ( 1.000000000000000000, 1.000000000000000000, 1.000000000000000000) ) ) 
 REPRESENTATION_ITEM ( '' )  SURFACE ( )  );
#88634 = CARTESIAN_POINT ( 'NONE',  ( -53.52971897118871425, -57.67555505732850207, 87.03092276603273092 ) ) ;
#88635 = CARTESIAN_POINT ( 'NONE',  ( 16.35737551353592067, 302.5695985197569939, 9.877143523090261112 ) ) ;
#88636 = EDGE_CURVE ( 'NONE', #64079, #69907, #18342, .T. ) ;
#88637 = ORIENTED_EDGE ( 'NONE', *, *, #72727, .F. ) ;
#88638 = CARTESIAN_POINT ( 'NONE',  ( 73.33904886068935980, 6.975173280561618775E-15, 0.000000000000000000 ) ) ;
#88639 = CARTESIAN_POINT ( 'NONE',  ( 7.500000000000007105, 40.19558899698767362, -59.64746577828605467 ) ) ;
#88640 = CARTESIAN_POINT ( 'NONE',  ( -6.500000000000000000, 2.501851166488365585, -5.848636054922033978 ) ) ;
#88641 = VERTEX_POINT ( 'NONE', #74375 ) ;
#88642 = CARTESIAN_POINT ( 'NONE',  ( -8.000000000000000000, -10.43750000409677092, -9.797174393178825657E-16 ) ) ;
#88643 = DIRECTION ( 'NONE',  ( 0.000000000000000000, 1.000000000000000000, 0.000000000000000000 ) ) ;
#88644 = CARTESIAN_POINT ( 'NONE',  ( 10.00000000000002132, 14.99999999999997335, 2.701558353794770273 ) ) ;
#88645 = CARTESIAN_POINT ( 'NONE',  ( -1.000000000000000000, -48.56827653474476136, 2.661071982226036692 ) ) ;
#88646 = EDGE_CURVE ( 'NONE', #96644, #54873, #98740, .T. ) ;
#88647 = FACE_OUTER_BOUND ( 'NONE', #73921, .T. ) ;
#88648 = DIRECTION ( 'NONE',  ( 0.000000000000000000, 1.000000000000000000, 0.000000000000000000 ) ) ;
#88649 = PRODUCT_CONTEXT ( 'NONE', #105855, 'mechanical' ) ;
#88650 = CARTESIAN_POINT ( 'NONE',  ( -10.00005432054556742, 34.00013580137913749, 0.2621623937322678510 ) ) ;
#88651 = VERTEX_POINT ( 'NONE', #92159 ) ;
#88652 = DIRECTION ( 'NONE',  ( 0.000000000000000000, -1.000000000000000000, 0.000000000000000000 ) ) ;
#88653 = CARTESIAN_POINT ( 'NONE',  ( -3.487646406148226852, 15.95332971149351842, 9.373884331925033564 ) ) ;
#88654 = CARTESIAN_POINT ( 'NONE',  ( -1.796354877921464421, 14.26916677339775319, -6.770108860242546989 ) ) ;
#88655 = AXIS2_PLACEMENT_3D ( 'NONE', #10499, #75223, #26734 ) ;
#88656 = CARTESIAN_POINT ( 'NONE',  ( -6.206025854132298569, -21.79809244015144998, -38.54595585258209667 ) ) ;
#88657 = CARTESIAN_POINT ( 'NONE',  ( -59.07834085828424264, -30.00000000000000711, 64.72383880810683365 ) ) ;
#88658 = EDGE_CURVE ( 'NONE', #84046, #50361, #88467, .T. ) ;
#88659 = CARTESIAN_POINT ( 'NONE',  ( 33.58349330513379982, 1.593028355512270567E-15, 0.000000000000000000 ) ) ;
#88660 = SPHERICAL_SURFACE ( 'NONE', #103095, 1.000000000000000000 ) ;
#88661 = ORIENTED_EDGE ( 'NONE', *, *, #81115, .F. ) ;
#88662 = DIRECTION ( 'NONE',  ( -0.000000000000000000, 1.000000000000000000, 1.224646799147353207E-16 ) ) ;
#88663 = CARTESIAN_POINT ( 'NONE',  ( 91.70293005516124651, -57.61487155903986945, 204.2876863399782508 ) ) ;
#88664 = DIRECTION ( 'NONE',  ( -0.9623543818480306822, -0.1986072300191265572, -0.1855511032627525092 ) ) ;
#88665 = EDGE_CURVE ( 'NONE', #13028, #63010, #52232, .T. ) ;
#88666 = CARTESIAN_POINT ( 'NONE',  ( 0.000000000000000000, 0.000000000000000000, 0.000000000000000000 ) ) ;
#88667 = EDGE_CURVE ( 'NONE', #87378, #99203, #92696, .T. ) ;
#88668 = CARTESIAN_POINT ( 'NONE',  ( -16.10335319434544843, 21.83248469006238679, -0.8773453446503929332 ) ) ;
#88669 = CARTESIAN_POINT ( 'NONE',  ( 0.01688885742776513946, -6.535341423375584213, 4.680456609903975718 ) ) ;
#88670 = CARTESIAN_POINT ( 'NONE',  ( -72.48404470694545410, -60.00000000000001421, 158.0047739593530309 ) ) ;
#88671 = ADVANCED_FACE ( 'NONE', ( #59283 ), #67373, .F. ) ;
#88672 = CARTESIAN_POINT ( 'NONE',  ( -43.74855578046756222, 328.6220886837048170, -1.765109843966993441 ) ) ;
#88673 = FACE_OUTER_BOUND ( 'NONE', #24999, .T. ) ;
#88674 = CARTESIAN_POINT ( 'NONE',  ( 50.94745919686198476, 50.00000000000000000, -37.05882352941176094 ) ) ;
#88675 = CARTESIAN_POINT ( 'NONE',  ( -86.18651039905068956, -24.72797755481551363, 181.0558452470112911 ) ) ;
#88677 = ADVANCED_FACE ( 'NONE', ( #25896 ), #95851, .T. ) ;
#88676 = ORIENTED_EDGE ( 'NONE', *, *, #55462, .T. ) ;
#88678 = CARTESIAN_POINT ( 'NONE',  ( 33.79394592499237859, 329.6538948152748389, -2.915499870108015035 ) ) ;
#88679 = ORIENTED_EDGE ( 'NONE', *, *, #103336, .T. ) ;
#88680 = CARTESIAN_POINT ( 'NONE',  ( -7.151217271224852290, -11.78749400445715700, -3.587901469523287368 ) ) ;
#88682 = CARTESIAN_POINT ( 'NONE',  ( -20.37278541768183615, 303.8378246129572631, -10.00297115033342266 ) ) ;
#88681 = CONICAL_SURFACE ( 'NONE', #78359, 3.400000000000000355, 0.9599310885968748153 ) ;
#88683 = CARTESIAN_POINT ( 'NONE',  ( 42.75104180402610154, 488.2556334690061703, 9.347379739029891610 ) ) ;
#88684 = DIRECTION ( 'NONE',  ( -1.000000000000000000, -1.224606353822377258E-16, -0.000000000000000000 ) ) ;
#88685 = ORIENTED_EDGE ( 'NONE', *, *, #62568, .F. ) ;
#88686 = CARTESIAN_POINT ( 'NONE',  ( 19.15934361619958537, 50.00000000000000711, 60.36969726297910199 ) ) ;
#88687 = CARTESIAN_POINT ( 'NONE',  ( 10.14990128296980210, 12.13918606557333568, 10.55440379982475108 ) ) ;
#88688 = CARTESIAN_POINT ( 'NONE',  ( 10.45706415778036025, -1.734723475976807094E-15, -13.60704923275195455 ) ) ;
#88689 = FACE_OUTER_BOUND ( 'NONE', #40583, .T. ) ;
#88690 = CARTESIAN_POINT ( 'NONE',  ( 61.70037527280209844, -30.00000000000006040, -32.45262418874342103 ) ) ;
#88691 = CARTESIAN_POINT ( 'NONE',  ( -79.30432945941426226, -39.49937122350303298, 141.5529580233551883 ) ) ;
#88692 = AXIS2_PLACEMENT_3D ( 'NONE', #51380, #83748, #2290 ) ;
#88693 = ORIENTED_EDGE ( 'NONE', *, *, #88252, .T. ) ;
#88694 = CARTESIAN_POINT ( 'NONE',  ( 43.57856552656106430, -59.99999999999991473, 62.86110226080823793 ) ) ;
#88695 = FILL_AREA_STYLE_COLOUR ( '', #90168 ) ;
#88696 = CARTESIAN_POINT ( 'NONE',  ( 101.4167185739037649, -57.63043782431127227, 203.4936600526360451 ) ) ;
#88697 = AXIS2_PLACEMENT_3D ( 'NONE', #105951, #24023, #105438 ) ;
#88698 = PRESENTATION_LAYER_ASSIGNMENT (  '', '', ( #43885 ) ) ;
#88699 = CARTESIAN_POINT ( 'NONE',  ( 0.5805565836007654523, 7.505553499465140277, 2.211437577243512467E-16 ) ) ;
#88700 = PRESENTATION_LAYER_ASSIGNMENT (  '', '', ( #33589 ) ) ;
#88701 = CARTESIAN_POINT ( 'NONE',  ( 32.73025373822441253, 313.1192488950297843, -7.568336369384137008 ) ) ;
#88702 = DIRECTION ( 'NONE',  ( -1.000000000000000000, 0.000000000000000000, 0.000000000000000000 ) ) ;
#88703 = ORIENTED_EDGE ( 'NONE', *, *, #95099, .F. ) ;
#88704 = AXIS2_PLACEMENT_3D ( 'NONE', #979, #43089, #58749 ) ;
#88705 = CARTESIAN_POINT ( 'NONE',  ( 0.000000000000000000, -1.341159125180006795, 15.80007993603364724 ) ) ;
#88706 = CARTESIAN_POINT ( 'NONE',  ( -12.50000000000000000, 1.275975811747059652, -19.12903451213154327 ) ) ;
#88708 = CARTESIAN_POINT ( 'NONE',  ( -103.1762899285966881, -45.26535789155201428, 156.3495666460457585 ) ) ;
#88707 = FACE_OUTER_BOUND ( 'NONE', #32137, .T. ) ;
#88709 = CARTESIAN_POINT ( 'NONE',  ( 5.082755093536324154, -17.84375000204838457, 5.082755093536326818 ) ) ;
#88710 = CARTESIAN_POINT ( 'NONE',  ( 43.56126634772264339, 484.2986656255879439, 0.7800160315374845554 ) ) ;
#88711 = AXIS2_PLACEMENT_3D ( 'NONE', #19317, #103370, #102298 ) ;
#88712 = CARTESIAN_POINT ( 'NONE',  ( 9.999945253488242258, 81.00013686629468168, -0.2662901834230905207 ) ) ;
#88713 = CARTESIAN_POINT ( 'NONE',  ( 5.500000000000641265, 42.00000000000000000, -59.88032989331720302 ) ) ;
#88714 = EDGE_CURVE ( 'NONE', #67595, #83791, #99216, .T. ) ;
#88715 = CARTESIAN_POINT ( 'NONE',  ( -17.85237544995465342, 45.37579490857304165, -5.050174946722908231 ) ) ;
#88716 = DIRECTION ( 'NONE',  ( 0.000000000000000000, -1.000000000000000000, 0.000000000000000000 ) ) ;
#88717 = EDGE_LOOP ( 'NONE', ( #44868, #49859, #42664, #104932, #80386, #20960 ) ) ;
#88718 = CARTESIAN_POINT ( 'NONE',  ( 14.83349330513380693, 1.593028355512270962E-15, 0.000000000000000000 ) ) ;
#88720 = CARTESIAN_POINT ( 'NONE',  ( 31.88784071051081170, -56.84613636546770721, 36.98492141617447260 ) ) ;
#88719 = CARTESIAN_POINT ( 'NONE',  ( -0.8750000000009734435, -70.58759490697451611, 13.02737050516266315 ) ) ;
#88721 = CARTESIAN_POINT ( 'NONE',  ( 24.20637929534462884, 27.76268499971478221, -31.17501708768082125 ) ) ;
#88722 = EDGE_CURVE ( 'NONE', #64980, #66178, #50618, .T. ) ;
#88723 = ORIENTED_EDGE ( 'NONE', *, *, #70293, .F. ) ;
#88724 = EDGE_LOOP ( 'NONE', ( #46949, #72654, #91359 ) ) ;
#88726 = CARTESIAN_POINT ( 'NONE',  ( 1.097170575850833218, 51.92387531005979895, 8.380158856765602238 ) ) ;
#88725 = DIRECTION ( 'NONE',  ( 1.224646799147353454E-16, 0.000000000000000000, -1.000000000000000000 ) ) ;
#88727 = CYLINDRICAL_SURFACE ( 'NONE', #56007, 1.250000000000001110 ) ;
#88728 = FILL_AREA_STYLE_COLOUR ( '', #25880 ) ;
#88729 = FACE_OUTER_BOUND ( 'NONE', #12499, .T. ) ;
#88730 = SURFACE_STYLE_FILL_AREA ( #56331 ) ;
#88731 = FACE_OUTER_BOUND ( 'NONE', #64045, .T. ) ;
#88732 = ORIENTED_EDGE ( 'NONE', *, *, #32180, .T. ) ;
#88733 = CARTESIAN_POINT ( 'NONE',  ( 61.59314311649531248, -60.00000000000001421, -35.21162133311354125 ) ) ;
#88734 = CARTESIAN_POINT ( 'NONE',  ( 23.05265313601412203, 25.28706265245096318, -33.20617127781077471 ) ) ;
#88735 = DIRECTION ( 'NONE',  ( 0.000000000000000000, 0.000000000000000000, 1.000000000000000000 ) ) ;
#88736 = PLANE ( 'NONE',  #104618 ) ;
#88737 = CARTESIAN_POINT ( 'NONE',  ( 46.77767549600488906, 13.52659353100008843, -15.64517449361694723 ) ) ;
#88738 = VERTEX_POINT ( 'NONE', #42545 ) ;
#88739 = EDGE_CURVE ( 'NONE', #69676, #89428, #17793, .T. ) ;
#88740 = PRODUCT_DEFINITION_FORMATION_WITH_SPECIFIED_SOURCE ( 'ANY', '', #12205, .NOT_KNOWN. ) ;
#88741 = EDGE_LOOP ( 'NONE', ( #40056, #79808 ) ) ;
#88742 = VERTEX_POINT ( 'NONE', #15964 ) ;
#88743 = CARTESIAN_POINT ( 'NONE',  ( 1.221913359428326018, 53.71105537643708061, 9.309427401043976147 ) ) ;
#88744 = CARTESIAN_POINT ( 'NONE',  ( 33.16846355476446462, 397.4937985473089839, 25.83636734666645651 ) ) ;
#88745 = CARTESIAN_POINT ( 'NONE',  ( -42.96462842659435211, 322.5525446679458810, -3.268891976929361398 ) ) ;
#88746 = CARTESIAN_POINT ( 'NONE',  ( -6.125000000795022714, -61.26994199106662364, 14.41094225169091558 ) ) ;
#88747 = LINE ( 'NONE', #105458, #71654 ) ;
#88748 = CARTESIAN_POINT ( 'NONE',  ( 72.85555555555556850, 3.309500000000014541, 4.052968581778174646E-16 ) ) ;
#88749 = ORIENTED_EDGE ( 'NONE', *, *, #91473, .T. ) ;
#88750 = CARTESIAN_POINT ( 'NONE',  ( -9.500616112259193002, 44.08938505136232777, 13.17116827006698543 ) ) ;
#88751 = EDGE_LOOP ( 'NONE', ( #104738, #55635, #39542, #35751 ) ) ;
#88752 = EDGE_CURVE ( 'NONE', #40774, #25026, #265, .T. ) ;
#88753 = CARTESIAN_POINT ( 'NONE',  ( 66.74444444444444002, 3.309500000000014541, 4.052968581778174646E-16 ) ) ;
#88754 = CARTESIAN_POINT ( 'NONE',  ( -50.94745919686199898, 50.00000000000000000, -37.05882352941176805 ) ) ;
#88755 = CARTESIAN_POINT ( 'NONE',  ( 32.61650669486618881, 4.898587196589413815E-16, -4.000000000000000888 ) ) ;
#88756 = DIRECTION ( 'NONE',  ( 0.3420201433256622736, 0.000000000000000000, -0.9396926207859106484 ) ) ;
#88757 = CARTESIAN_POINT ( 'NONE',  ( 65.35202525436315568, -49.90957767371891407, 92.77620802272491574 ) ) ;
#88758 = CIRCLE ( 'NONE', #66581, 4.000000000000000888 ) ;
#88759 = ORIENTED_EDGE ( 'NONE', *, *, #9063, .T. ) ;
#88760 = CARTESIAN_POINT ( 'NONE',  ( 0.000000000000000000, 43.50000000000000711, 57.86910460382442523 ) ) ;
#88761 = CARTESIAN_POINT ( 'NONE',  ( -6.085184064390054992, 10.98280286254172999, 3.463681541593110591 ) ) ;
#88762 = CARTESIAN_POINT ( 'NONE',  ( -11.25758791135831594, -57.67118876967119689, -44.34807234721190383 ) ) ;
#88763 = EDGE_CURVE ( 'NONE', #94076, #24323, #52719, .T. ) ;
#88764 = EDGE_CURVE ( 'NONE', #24268, #92963, #32711, .T. ) ;
#88765 = AXIS2_PLACEMENT_3D ( 'NONE', #27098, #52384, #51853 ) ;
#88766 = EDGE_LOOP ( 'NONE', ( #62349, #61239, #94731, #3858, #35804, #38187 ) ) ;
#88767 = FILL_AREA_STYLE ('',( #48285 ) ) ;
#88768 = CARTESIAN_POINT ( 'NONE',  ( 46.81266956378438948, 18.41561415511120714, 15.90959751601103633 ) ) ;
#88769 = AXIS2_PLACEMENT_3D ( 'NONE', #10591, #27370, #99599 ) ;
#88770 = CARTESIAN_POINT ( 'NONE',  ( 23.86650669486618881, 1.474610560812782335E-15, 0.000000000000000000 ) ) ;
#88771 = AXIS2_PLACEMENT_3D ( 'NONE', #31272, #32857, #90004 ) ;
#88772 = CARTESIAN_POINT ( 'NONE',  ( 4.898587196589412829E-16, -31.81250000409677270, -8.000000000000000000 ) ) ;
#88773 = CIRCLE ( 'NONE', #40574, 66.00000000000000000 ) ;
#88774 = CARTESIAN_POINT ( 'NONE',  ( 8.000000000000000000, -3.000000000000000000, 2.094395098902537722 ) ) ;
#88775 = AXIS2_PLACEMENT_3D ( 'NONE', #60979, #75545, #10277 ) ;
#88776 = CARTESIAN_POINT ( 'NONE',  ( 86.51826356133454965, -17.01126878319249869, 184.3016907190141467 ) ) ;
#88777 = AXIS2_PLACEMENT_3D ( 'NONE', #20819, #4048, #69848 ) ;
#88778 =( NAMED_UNIT ( * ) PLANE_ANGLE_UNIT ( ) SI_UNIT ( $, .RADIAN. ) );
#88779 = CARTESIAN_POINT ( 'NONE',  ( -9.996167984729328992, 7.505519767357340832, 4.999999999999980460 ) ) ;
#88780 = CIRCLE ( 'NONE', #40580, 3.309500000000001663 ) ;
#88781 = CARTESIAN_POINT ( 'NONE',  ( -1.126429428730187476, 7.232124035235039550, -6.344710093416086494 ) ) ;
#88782 = CARTESIAN_POINT ( 'NONE',  ( 13.25307200133307539, 303.5542396669459322, 9.873748816204125589 ) ) ;
#88783 = EDGE_LOOP ( 'NONE', ( #68695, #60604, #27967, #93764, #31880 ) ) ;
#88784 = PLANE ( 'NONE',  #102772 ) ;
#88785 = CARTESIAN_POINT ( 'NONE',  ( 33.19169623717888129, -60.00000000000000711, 44.98076713291913364 ) ) ;
#88786 = CARTESIAN_POINT ( 'NONE',  ( -99.80277137147388089, -29.99999999999998934, 186.4011847855257997 ) ) ;
#88787 = EDGE_CURVE ( 'NONE', #46291, #17539, #33084, .T. ) ;
#88788 = CARTESIAN_POINT ( 'NONE',  ( 25.21823338009918203, 1.482358050883964840E-15, 0.000000000000000000 ) ) ;
#88789 = CARTESIAN_POINT ( 'NONE',  ( 45.09405268356402985, -57.68306127209417156, 65.36625235151646507 ) ) ;
#88791 = CARTESIAN_POINT ( 'NONE',  ( 37.33349330513379982, 4.000000000000002665, 0.000000000000000000 ) ) ;
#88790 = DIRECTION ( 'NONE',  ( -1.000000000000000000, -0.000000000000000000, -0.000000000000000000 ) ) ;
#88792 = EDGE_CURVE ( 'NONE', #4416, #23008, #59678, .T. ) ;
#88793 = CARTESIAN_POINT ( 'NONE',  ( -49.53030510826501853, 39.42532954496144981, -42.40708829318106865 ) ) ;
#88794 = PRESENTATION_STYLE_ASSIGNMENT (( #82686 ) ) ;
#88795 = CARTESIAN_POINT ( 'NONE',  ( 0.000000000000000000, 3.000000000000002665, 0.000000000000000000 ) ) ;
#88796 = CARTESIAN_POINT ( 'NONE',  ( -22.96940955295018583, -60.00000000000001421, 40.68925847043787059 ) ) ;
#88797 = FILL_AREA_STYLE ('',( #55859 ) ) ;
#88798 = CARTESIAN_POINT ( 'NONE',  ( -86.68948599710770964, -20.67461466719461072, 184.9450686744756638 ) ) ;
#88799 = ADVANCED_FACE ( 'NONE', ( #58004 ), #37296, .T. ) ;
#88801 = EDGE_CURVE ( 'NONE', #20102, #79761, #98555, .T. ) ;
#88800 = VERTEX_POINT ( 'NONE', #50439 ) ;
#88802 =( NAMED_UNIT ( * ) SI_UNIT ( $, .STERADIAN. ) SOLID_ANGLE_UNIT ( ) );
#88803 = CARTESIAN_POINT ( 'NONE',  ( 99.75754961941544252, 1.030564683017419500E-14, 0.000000000000000000 ) ) ;
#88804 = CARTESIAN_POINT ( 'NONE',  ( -10.44718778294642547, -56.88425898734509190, 33.38460417480683873 ) ) ;
#88806 = CARTESIAN_POINT ( 'NONE',  ( 40.56952547639649254, 460.8933045338673082, 2.221423359587424873 ) ) ;
#88805 = CARTESIAN_POINT ( 'NONE',  ( -86.31506357673099217, -59.99999999999993605, 20.26404540652117348 ) ) ;
#88807 = ORIENTED_EDGE ( 'NONE', *, *, #83334, .T. ) ;
#88808 = CARTESIAN_POINT ( 'NONE',  ( 0.000000000000000000, 0.000000000000000000, -11.82492182392400437 ) ) ;
#88809 = CARTESIAN_POINT ( 'NONE',  ( -9.285084206833351672, -5.000000000000069278, -17.96579109464167345 ) ) ;
#88810 = CARTESIAN_POINT ( 'NONE',  ( -3.381870600466846067E-15, 46.21383923812598482, -16.24999999999995026 ) ) ;
#88811 = CARTESIAN_POINT ( 'NONE',  ( -8.000113193197767814, -80.99977361354137884, -0.2613481123984638943 ) ) ;
#88812 = CARTESIAN_POINT ( 'NONE',  ( 68.03985042304489639, -60.00000000000000000, 131.2812129801127128 ) ) ;
#88813 = CARTESIAN_POINT ( 'NONE',  ( 0.000000000000000000, 24.73290587908618932, 14.06164498842270483 ) ) ;
#88814 = VERTEX_POINT ( 'NONE', #93664 ) ;
#88815 = CARTESIAN_POINT ( 'NONE',  ( 44.10120706205769636, 485.7576699374418467, 4.111328371165819284 ) ) ;
#88816 = DIRECTION ( 'NONE',  ( -1.000000000000000000, -0.000000000000000000, -0.000000000000000000 ) ) ;
#88818 = CARTESIAN_POINT ( 'NONE',  ( 5.596957125887390028, -2.684245481662592692, 103.9718581041641698 ) ) ;
#88817 = CARTESIAN_POINT ( 'NONE',  ( 8.309829428344436053, -30.00000000000008527, 36.98670151680749996 ) ) ;
#88819 = CARTESIAN_POINT ( 'NONE',  ( 3.510275272315894757, -1.149081201640936190, 104.5952116206559737 ) ) ;
#88820 = CARTESIAN_POINT ( 'NONE',  ( -4.792515968931456705, -2.702239074782535777, 102.4138677444059766 ) ) ;
#88821 = ORIENTED_EDGE ( 'NONE', *, *, #16480, .T. ) ;
#88822 = AXIS2_PLACEMENT_3D ( 'NONE', #74173, #41811, #83333 ) ;
#88823 = CARTESIAN_POINT ( 'NONE',  ( -29.72305811207850113, 326.8793782738446794, 14.35461530513359918 ) ) ;
#88824 = VERTEX_POINT ( 'NONE', #94192 ) ;
#88825 = CARTESIAN_POINT ( 'NONE',  ( 0.000000000000000000, 1.000000000000000888, 0.000000000000000000 ) ) ;
#88826 = SURFACE_STYLE_USAGE ( .BOTH. , #106595 ) ;
#88827 = DIRECTION ( 'NONE',  ( -1.000000000000000000, -1.224606353822377258E-16, -0.000000000000000000 ) ) ;
#88828 = ORIENTED_EDGE ( 'NONE', *, *, #102744, .F. ) ;
#88829 = EDGE_CURVE ( 'NONE', #25666, #16749, #35997, .T. ) ;
#88830 = CIRCLE ( 'NONE', #59506, 3.309500000000007880 ) ;
#88831 = PRESENTATION_STYLE_ASSIGNMENT (( #104476 ) ) ;
#88832 = CARTESIAN_POINT ( 'NONE',  ( 8.113285044351216187E-15, 48.50000000000000000, -66.00000000000000000 ) ) ;
#88833 = CARTESIAN_POINT ( 'NONE',  ( -84.07952891099454007, -59.99999999997081090, 202.4448410950529933 ) ) ;
#88834 = CARTESIAN_POINT ( 'NONE',  ( 43.66147695926597549, 485.1157264602073838, -1.117513576741872683 ) ) ;
#88835 = CARTESIAN_POINT ( 'NONE',  ( 50.14918825808751990, -59.99999999999997158, 72.16795998310614380 ) ) ;
#88836 = LINE ( 'NONE', #96414, #37462 ) ;
#88837 = CARTESIAN_POINT ( 'NONE',  ( 0.7840884375884051849, 25.26123080618498307, -40.48700950034228896 ) ) ;
#88839 = CARTESIAN_POINT ( 'NONE',  ( 13.61911990997247912, -49.91571610495643796, 32.29718510433961853 ) ) ;
#88838 = CARTESIAN_POINT ( 'NONE',  ( -109.4365443207511390, -30.00000000000002487, 178.4890703142130519 ) ) ;
#88840 = CARTESIAN_POINT ( 'NONE',  ( 82.95080249199725131, -37.99999999999999289, 0.1906324524714007318 ) ) ;
#88842 = EDGE_CURVE ( 'NONE', #40774, #46319, #92366, .T. ) ;
#88841 = PRESENTATION_STYLE_ASSIGNMENT (( #72122 ) ) ;
#88843 = CARTESIAN_POINT ( 'NONE',  ( -47.01998836181715546, -32.61244973267624658, 44.20308275279673182 ) ) ;
#88844 = CARTESIAN_POINT ( 'NONE',  ( -0.7767374935270013880, 34.98060154996775140, -27.51719054460002312 ) ) ;
#88845 = MECHANICAL_DESIGN_GEOMETRIC_PRESENTATION_REPRESENTATION (  '', ( #56087 ), #45810 ) ;
#88846 = VERTEX_POINT ( 'NONE', #27910 ) ;
#88847 = CIRCLE ( 'NONE', #59604, 5.000000000000001776 ) ;
#88848 = PRESENTATION_STYLE_ASSIGNMENT (( #106611 ) ) ;
#88849 = CIRCLE ( 'NONE', #76745, 66.50000000000000000 ) ;
#88850 = CARTESIAN_POINT ( 'NONE',  ( -43.81028729233671726, 434.3199584132789255, 12.84475684849438970 ) ) ;
#88851 = AXIS2_PLACEMENT_3D ( 'NONE', #30331, #13044, #45449 ) ;
#88852 = CARTESIAN_POINT ( 'NONE',  ( -0.9888037323473499729, 17.70116029579951800, 49.73220125274776393 ) ) ;
#88853 = DIRECTION ( 'NONE',  ( -0.000000000000000000, 1.000000000000000000, -0.000000000000000000 ) ) ;
#88854 = CARTESIAN_POINT ( 'NONE',  ( 35.58361799548379167, 1.482358050883964840E-15, 0.000000000000000000 ) ) ;
#88855 = CARTESIAN_POINT ( 'NONE',  ( 31.11679462788039530, 441.4271381875185511, 23.27438508043199406 ) ) ;
#88856 = ORIENTED_EDGE ( 'NONE', *, *, #31916, .F. ) ;
#88857 = SURFACE_SIDE_STYLE ('',( #71071 ) ) ;
#88858 = ORIENTED_EDGE ( 'NONE', *, *, #27024, .F. ) ;
#88859 = CARTESIAN_POINT ( 'NONE',  ( 85.40235745944882240, -30.00000000001180567, 197.3970878040293258 ) ) ;
#88860 = CARTESIAN_POINT ( 'NONE',  ( 8.559508646656350805, 53.96349637827587031, -1.531152949374623651 ) ) ;
#88861 = CARTESIAN_POINT ( 'NONE',  ( 5.701071517278371914, 41.97507531912567202, -59.34341564409904635 ) ) ;
#88862 = CONICAL_SURFACE ( 'NONE', #56103, 3.309500000000007880, 0.9599310885968770357 ) ;
#88863 = CARTESIAN_POINT ( 'NONE',  ( -28.12328997684540610, 24.73290587908618932, 14.06164498842270838 ) ) ;
#88864 = CARTESIAN_POINT ( 'NONE',  ( 97.89651928708440209, -30.00000000000000355, 136.8046996854560291 ) ) ;
#88865 = DIRECTION ( 'NONE',  ( 1.000000000000000000, 0.000000000000000000, 0.000000000000000000 ) ) ;
#88866 = VERTEX_POINT ( 'NONE', #20359 ) ;
#88867 = EDGE_CURVE ( 'NONE', #75420, #105857, #13139, .T. ) ;
#88868 = B_SPLINE_CURVE_WITH_KNOTS ( 'NONE', 3,
 ( #52364, #92285, #18989, #36240, #51296, #84215, #43227, #76110, #51833, #84746, #26367, #41962, #74845, #74323, #24746, #82428 ),
 .UNSPECIFIED., .F., .F.,
 ( 4, 2, 2, 2, 2, 2, 2, 4 ),
 ( 0.000000000000000000, 0.0008003613409292714437, 0.001600722681858542671, 0.003201445363717083607, 0.004001806704646354400, 0.004802168045575623892, 0.005602529386504895119, 0.006402890727434164611 ),
 .UNSPECIFIED. ) ;
#88869 = ORIENTED_EDGE ( 'NONE', *, *, #17367, .T. ) ;
#88870 = ORIENTED_EDGE ( 'NONE', *, *, #3652, .F. ) ;
#88871 = CARTESIAN_POINT ( 'NONE',  ( 44.17836536378470669, 435.2619773020559819, 14.65562696767914908 ) ) ;
#88872 = CARTESIAN_POINT ( 'NONE',  ( -39.00566081833550669, 463.6621700551983167, 19.40488523433662493 ) ) ;
#88873 = ORIENTED_EDGE ( 'NONE', *, *, #71996, .T. ) ;
#88874 = DIRECTION ( 'NONE',  ( 0.000000000000000000, 1.000000000000000000, 0.000000000000000000 ) ) ;
#88875 = ORIENTED_EDGE ( 'NONE', *, *, #43625, .T. ) ;
#88876 = CARTESIAN_POINT ( 'NONE',  ( 19.34999999999999787, 1.533819458162526451E-15, 0.000000000000000000 ) ) ;
#88877 = CARTESIAN_POINT ( 'NONE',  ( 77.57546568842502666, -38.52226549919825516, 186.7529093661793240 ) ) ;
#88878 = CARTESIAN_POINT ( 'NONE',  ( 0.000000000000000000, 0.000000000000000000, 0.000000000000000000 ) ) ;
#88879 = CARTESIAN_POINT ( 'NONE',  ( 85.72732811624759108, -52.73815978549392014, -5.088828352706781466 ) ) ;
#88880 = CARTESIAN_POINT ( 'NONE',  ( 54.54809302485524114, -37.99999999999998579, 58.67176596216953044 ) ) ;
#88881 = CARTESIAN_POINT ( 'NONE',  ( 41.33081450886904662, 330.4361996080641575, 10.57783742947384908 ) ) ;
#88882 = DIRECTION ( 'NONE',  ( 0.000000000000000000, -1.000000000000000000, 0.000000000000000000 ) ) ;
#88883 = CARTESIAN_POINT ( 'NONE',  ( 95.70911704725124025, -5.000000000000020428, 0.000000000000000000 ) ) ;
#88884 = AXIS2_PLACEMENT_3D ( 'NONE', #33900, #67314, #75920 ) ;
#88885 = CARTESIAN_POINT ( 'NONE',  ( 41.66665637657543186, 334.9189789097773655, 11.60746121313486334 ) ) ;
#88886 = ORIENTED_EDGE ( 'NONE', *, *, #4616, .F. ) ;
#88887 = FILL_AREA_STYLE_COLOUR ( '', #51483 ) ;
#88888 = CARTESIAN_POINT ( 'NONE',  ( -34.73554899884743463, 462.7241937368494860, 5.242808629193801195 ) ) ;
#88889 = DIRECTION ( 'NONE',  ( 0.000000000000000000, 0.000000000000000000, -1.000000000000000000 ) ) ;
#88890 = ORIENTED_EDGE ( 'NONE', *, *, #90948, .T. ) ;
#88891 = CARTESIAN_POINT ( 'NONE',  ( -35.46814660802463237, 430.5672163472734724, 5.860357238957815795 ) ) ;
#88892 = CARTESIAN_POINT ( 'NONE',  ( -31.55816069737598184, 299.8186824367181202, 11.05464098791177463 ) ) ;
#88893 = DIRECTION ( 'NONE',  ( -1.000000000000000000, -1.224606353822377258E-16, -0.000000000000000000 ) ) ;
#88894 = DIRECTION ( 'NONE',  ( 0.000000000000000000, 0.000000000000000000, 1.000000000000000000 ) ) ;
#88895 = CARTESIAN_POINT ( 'NONE',  ( -3.313708498984765161, -17.46874999999999645, 7.999999999999998224 ) ) ;
#88896 = CARTESIAN_POINT ( 'NONE',  ( -17.95542721193044144, -24.37817513870772146, 36.37955489103553930 ) ) ;
#88897 = SURFACE_SIDE_STYLE ('',( #15529 ) ) ;
#88898 = ORIENTED_EDGE ( 'NONE', *, *, #29499, .F. ) ;
#88899 = CARTESIAN_POINT ( 'NONE',  ( 85.97695406691678954, -24.93193571675475084, 178.6345212492455516 ) ) ;
#88900 = CARTESIAN_POINT ( 'NONE',  ( 0.000000000000000000, -18.92596047533412573, -20.36976895023282097 ) ) ;
#88901 = VECTOR ( 'NONE', #20540, 1000.000000000000000 ) ;
#88902 = SURFACE_STYLE_USAGE ( .BOTH. , #12873 ) ;
#88903 = EDGE_LOOP ( 'NONE', ( #88048, #62243 ) ) ;
#88904 = CARTESIAN_POINT ( 'NONE',  ( 94.18556020815232444, -57.67258279061592674, 22.45562361954496922 ) ) ;
#88905 = CARTESIAN_POINT ( 'NONE',  ( -71.17284327374473207, -38.00000000000000711, -21.88481141223168436 ) ) ;
#88906 = CARTESIAN_POINT ( 'NONE',  ( 55.00571552735602410, 6.975173280561618775E-15, 0.000000000000000000 ) ) ;
#88907 =( NAMED_UNIT ( * ) SI_UNIT ( $, .STERADIAN. ) SOLID_ANGLE_UNIT ( ) );
#88908 = ADVANCED_FACE ( 'NONE', ( #53723 ), #85582, .T. ) ;
#88909 = AXIS2_PLACEMENT_3D ( 'NONE', #95275, #79600, #38637 ) ;
#88910 = EDGE_CURVE ( 'NONE', #28004, #87331, #88263, .T. ) ;
#88911 = AXIS2_PLACEMENT_3D ( 'NONE', #26106, #49245, #50835 ) ;
#88912 = CARTESIAN_POINT ( 'NONE',  ( -67.05072968586063098, -37.99999999999999289, 91.59218951166944578 ) ) ;
#88913 = CARTESIAN_POINT ( 'NONE',  ( 2.094395098902538610, -4.999999999999998224, -8.000000000000000000 ) ) ;
#88914 = CARTESIAN_POINT ( 'NONE',  ( 6.162888688655344005, 3.752776749732561257, -6.499999999999999112 ) ) ;
#88915 = EDGE_CURVE ( 'NONE', #56862, #35387, #54471, .T. ) ;
#88917 = CARTESIAN_POINT ( 'NONE',  ( -15.55885900989643389, 4.747722280824520524, 5.673041147144331831 ) ) ;
#88916 = CARTESIAN_POINT ( 'NONE',  ( 13.86650669486618881, 1.474610560812782335E-15, 0.000000000000000000 ) ) ;
#88918 = ORIENTED_EDGE ( 'NONE', *, *, #23962, .F. ) ;
#88919 = CARTESIAN_POINT ( 'NONE',  ( 9.581329576345360977, 294.6545431190994009, -2.865389023834811422 ) ) ;
#88920 = CONICAL_SURFACE ( 'NONE', #56151, 4.172000000000001485, 0.9599310885968750373 ) ;
#88921 = CARTESIAN_POINT ( 'NONE',  ( -12.49999999999999822, -4.999999999999999112, -9.904958390907015797 ) ) ;
#88922 = CARTESIAN_POINT ( 'NONE',  ( -28.08564602980796820, 36.49793394831486637, -8.015104271803140890 ) ) ;
#88923 = CARTESIAN_POINT ( 'NONE',  ( -6.125000000000000888, -80.00000000000000000, 14.41094225130411033 ) ) ;
#88924 = CARTESIAN_POINT ( 'NONE',  ( 0.000000000000000000, 300.0000000000000568, 0.000000000000000000 ) ) ;
#88925 = VECTOR ( 'NONE', #25468, 1000.000000000000227 ) ;
#88926 = ADVANCED_FACE ( 'NONE', ( #19295 ), #88920, .T. ) ;
#88927 = AXIS2_PLACEMENT_3D ( 'NONE', #26512, #76603, #54295 ) ;
#88928 = CARTESIAN_POINT ( 'NONE',  ( -82.80614267855605704, -38.00000000000003553, -11.81022639143571062 ) ) ;
#88929 = EDGE_CURVE ( 'NONE', #56114, #46770, #71488, .T. ) ;
#88930 = EDGE_LOOP ( 'NONE', ( #84120, #15489, #41898, #47203 ) ) ;
#88931 = DIRECTION ( 'NONE',  ( 0.000000000000000000, 0.000000000000000000, 1.000000000000000000 ) ) ;
#88932 = CARTESIAN_POINT ( 'NONE',  ( -7.488027283362990616, -15.86055150849546891, -34.99201987073333697 ) ) ;
#88933 =( BOUNDED_CURVE ( )  B_SPLINE_CURVE ( 2, ( #8928, #802, #97399, #81739, #83354, #98990, #25707, #56405, #7329 ),
 .UNSPECIFIED., .F., .F. ) 
 B_SPLINE_CURVE_WITH_KNOTS ( ( 3, 2, 2, 2, 3 ),
 ( 0.8676470588235294379, 0.8750000000000000000, 0.8823529411764705621, 0.8897058823529412352, 0.8970588235294119084 ),
 .UNSPECIFIED. ) 
 CURVE ( )  GEOMETRIC_REPRESENTATION_ITEM ( )  RATIONAL_B_SPLINE_CURVE ( ( 1.000000000000000000, 0.9238795325112867385, 1.000000000000000000, 0.9238795325112867385, 1.000000000000000000, 0.9238795325112867385, 1.000000000000000000, 0.9238795325112856283, 1.000000000000001110 ) ) 
 REPRESENTATION_ITEM ( '' )  );
#88935 = CARTESIAN_POINT ( 'NONE',  ( -60.68503947009055821, -60.22838572110379829, -29.53389179007121612 ) ) ;
#88934 = CARTESIAN_POINT ( 'NONE',  ( 21.04247164025375483, 37.86482112153537116, 10.52123582012687741 ) ) ;
#88936 = ORIENTED_EDGE ( 'NONE', *, *, #93201, .T. ) ;
#88937 = ORIENTED_EDGE ( 'NONE', *, *, #36312, .T. ) ;
#88938 = CARTESIAN_POINT ( 'NONE',  ( 11.38823185635503599, 43.21649034732992334, -14.75371867866905795 ) ) ;
#88939 = FACE_OUTER_BOUND ( 'NONE', #11046, .T. ) ;
#88940 = CARTESIAN_POINT ( 'NONE',  ( -92.38535695020712524, -60.00000000000000711, 0.3501147898381914425 ) ) ;
#88941 = ORIENTED_EDGE ( 'NONE', *, *, #94898, .T. ) ;
#88942 = CARTESIAN_POINT ( 'NONE',  ( -7.347880794884119933E-15, 0.000000000000000000, 60.00000000000000000 ) ) ;
#88943 = CARTESIAN_POINT ( 'NONE',  ( 100.1607552341765626, -52.76472588658410245, 194.0887023229978752 ) ) ;
#88944 = B_SPLINE_CURVE_WITH_KNOTS ( 'NONE', 3,
 ( #85416, #62230, #78373, #62739 ),
 .UNSPECIFIED., .F., .F.,
 ( 4, 4 ),
 ( 0.000000000000000000, 1.000000000000000000 ),
 .UNSPECIFIED. ) ;
#88946 = CARTESIAN_POINT ( 'NONE',  ( 60.14984002819952025, 6.856755485862130937E-15, 0.000000000000000000 ) ) ;
#88945 = FACE_OUTER_BOUND ( 'NONE', #15795, .T. ) ;
#88947 = AXIS2_PLACEMENT_3D ( 'NONE', #90991, #58621, #91521 ) ;
#88948 = CARTESIAN_POINT ( 'NONE',  ( -79.60123751058100083, -60.34287689035896562, 171.0025021070919138 ) ) ;
#88949 = ORIENTED_EDGE ( 'NONE', *, *, #51196, .T. ) ;
#88950 = ORIENTED_EDGE ( 'NONE', *, *, #66422, .T. ) ;
#88951 = AXIS2_PLACEMENT_3D ( 'NONE', #700, #92404, #33670 ) ;
#88952 = ORIENTED_EDGE ( 'NONE', *, *, #66910, .F. ) ;
#88953 = CARTESIAN_POINT ( 'NONE',  ( 34.88900972249397370, 464.6206820655982028, 18.69027339340997784 ) ) ;
#88954 = CARTESIAN_POINT ( 'NONE',  ( -5.963307081834163803, -13.30359940716284761, 13.46515011340851409 ) ) ;
#88955 = DIRECTION ( 'NONE',  ( 0.000000000000000000, -1.000000000000000000, 0.000000000000000000 ) ) ;
#88956 = ORIENTED_EDGE ( 'NONE', *, *, #105521, .F. ) ;
#88957 = ADVANCED_FACE ( 'NONE', ( #55811 ), #74921, .T. ) ;
#88958 = CARTESIAN_POINT ( 'NONE',  ( -31.84798727957934616, 480.8482684553740114, 11.59497121464450231 ) ) ;
#88959 = CARTESIAN_POINT ( 'NONE',  ( 0.000000000000000000, 1.499999999999992450, -61.23540616453487218 ) ) ;
#88960 = CARTESIAN_POINT ( 'NONE',  ( -102.4013124767651135, -57.63331223797548120, 203.1247769353137755 ) ) ;
#88961 = CARTESIAN_POINT ( 'NONE',  ( -6.000469943554648466, -69.00070491670500417, 0.2622423038614459245 ) ) ;
#88962 = DIRECTION ( 'NONE',  ( 0.000000000000000000, 0.000000000000000000, 1.000000000000000000 ) ) ;
#88963 = CARTESIAN_POINT ( 'NONE',  ( -28.21644434148578640, 308.7733337496239301, -9.112255642778062992 ) ) ;
#88964 = PLANE ( 'NONE',  #43405 ) ;
#88965 = CARTESIAN_POINT ( 'NONE',  ( -2.770043159915164477, -30.00000000000000355, -40.00000000000000000 ) ) ;
#88966 = EDGE_CURVE ( 'NONE', #103450, #2566, #88747, .T. ) ;
#88968 = EDGE_CURVE ( 'NONE', #96436, #70351, #26979, .T. ) ;
#88967 = CARTESIAN_POINT ( 'NONE',  ( -12.83279097724939000, -59.99999999999996447, 42.04727692947117390 ) ) ;
#88969 = CARTESIAN_POINT ( 'NONE',  ( -51.33271646286868872, -56.84205495537675290, 59.27433511503952701 ) ) ;
#88970 = DIRECTION ( 'NONE',  ( 1.000000000000000000, 1.224606353822377258E-16, 0.000000000000000000 ) ) ;
#88971 = ORIENTED_EDGE ( 'NONE', *, *, #18459, .T. ) ;
#88972 = CARTESIAN_POINT ( 'NONE',  ( -97.77229920577525490, -60.35143482894316236, 196.6193423550709838 ) ) ;
#88973 = MECHANICAL_DESIGN_GEOMETRIC_PRESENTATION_REPRESENTATION (  '', ( #106190 ), #51074 ) ;
#88974 = CARTESIAN_POINT ( 'NONE',  ( 91.09088295274877112, 1.030564683017419500E-14, 0.000000000000000000 ) ) ;
#88975 = VERTEX_POINT ( 'NONE', #54764 ) ;
#88976 = CARTESIAN_POINT ( 'NONE',  ( 19.04909562685467606, 49.60302394437223228, 61.82637030200322670 ) ) ;
#88977 =( GEOMETRIC_REPRESENTATION_CONTEXT ( 3 ) GLOBAL_UNCERTAINTY_ASSIGNED_CONTEXT ( ( #99014 ) ) GLOBAL_UNIT_ASSIGNED_CONTEXT ( ( #48405, #73205, #58650 ) ) REPRESENTATION_CONTEXT ( 'NONE', 'WORKASPACE' ) );
#88978 = CARTESIAN_POINT ( 'NONE',  ( 86.54967306013999462, -38.36251286152597828, -21.34969726277113722 ) ) ;
#88979 = CARTESIAN_POINT ( 'NONE',  ( 48.15279758643736585, 14.66099993221041231, 16.85535821593428096 ) ) ;
#88980 = CARTESIAN_POINT ( 'NONE',  ( 5.082755093536324154, -10.71875000204838457, 5.082755093536326818 ) ) ;
#88981 = CARTESIAN_POINT ( 'NONE',  ( -4.024429837834814450, 294.8082127746760079, 1.927919365218930148 ) ) ;
#88982 = DIRECTION ( 'NONE',  ( -1.000000000000000000, -1.224606353822377258E-16, -0.000000000000000000 ) ) ;
#88983 = CARTESIAN_POINT ( 'NONE',  ( 84.65080674787581927, -30.00000000000000355, 167.0029673134147572 ) ) ;
#88984 = CARTESIAN_POINT ( 'NONE',  ( -9.852227633834194975, 7.822462047239422844, 0.000000000000000000 ) ) ;
#88985 = CARTESIAN_POINT ( 'NONE',  ( 37.26845974722005650, 490.8898249940463074, 12.42613736167234961 ) ) ;
#88986 = CARTESIAN_POINT ( 'NONE',  ( -0.3344844736945739583, 35.06558596096873970, 27.29265241697899569 ) ) ;
#88987 = CIRCLE ( 'NONE', #38790, 4.000000000000001776 ) ;
#88988 = CARTESIAN_POINT ( 'NONE',  ( 3.313708498984781592, -24.78124999999998934, 7.999999999999979572 ) ) ;
#88989 = ADVANCED_FACE ( 'NONE', ( #104939 ), #42409, .T. ) ;
#88990 = ORIENTED_EDGE ( 'NONE', *, *, #84105, .T. ) ;
#88991 = ORIENTED_EDGE ( 'NONE', *, *, #18572, .T. ) ;
#88992 = CARTESIAN_POINT ( 'NONE',  ( 48.79736262066600005, -53.36142271290932371, 53.26804720879731292 ) ) ;
#88993 =( GEOMETRIC_REPRESENTATION_CONTEXT ( 3 ) GLOBAL_UNCERTAINTY_ASSIGNED_CONTEXT ( ( #29981 ) ) GLOBAL_UNIT_ASSIGNED_CONTEXT ( ( #67456, #69057, #28089 ) ) REPRESENTATION_CONTEXT ( 'NONE', 'WORKASPACE' ) );
#88994 = FACE_OUTER_BOUND ( 'NONE', #3561, .T. ) ;
#88995 = AXIS2_PLACEMENT_3D ( 'NONE', #61783, #70384, #29428 ) ;
#88996 = MANIFOLD_SOLID_BREP ( 'ThdSchPat', #24018 ) ;
#88997 = CARTESIAN_POINT ( 'NONE',  ( -6.318250223874061420E-16, 9.147862274876551680, -8.047472243342934206 ) ) ;
#88998 = ADVANCED_FACE ( 'NONE', ( #32663 ), #97514, .F. ) ;
#88999 = CARTESIAN_POINT ( 'NONE',  ( -110.5647867906232307, -38.35612385186053075, 181.7710796630721006 ) ) ;
#89000 = ORIENTED_EDGE ( 'NONE', *, *, #28390, .T. ) ;
#89001 = CARTESIAN_POINT ( 'NONE',  ( 110.0387909984985839, -38.35604073266033254, 155.0741904860052784 ) ) ;
#89002 = CARTESIAN_POINT ( 'NONE',  ( 11.41130097529988774, 18.22783037506831505, -8.549200310636470235 ) ) ;
#89003 = CARTESIAN_POINT ( 'NONE',  ( -1.128238012697766912, 300.0000000000000000, 9.936150108905552614 ) ) ;
#89004 = CARTESIAN_POINT ( 'NONE',  ( 13.50000000000000355, -6.526560492696110494, -0.8398270946102932566 ) ) ;
#89006 = CARTESIAN_POINT ( 'NONE',  ( 95.18346684494451893, -45.28272192646301164, 101.5333130734479710 ) ) ;
#89005 = VECTOR ( 'NONE', #10337, 1000.000000000000000 ) ;
#89007 = VECTOR ( 'NONE', #34657, 1000.000000000000000 ) ;
#89008 = CARTESIAN_POINT ( 'NONE',  ( 22.59351686035008910, 27.55929540978658920, 33.04221228726185444 ) ) ;
#89009 = CARTESIAN_POINT ( 'NONE',  ( -33.75641399212567961, 327.3064826613156129, -4.489452195648050647 ) ) ;
#89010 = EDGE_CURVE ( 'NONE', #31406, #95757, #79265, .T. ) ;
#89011 = CARTESIAN_POINT ( 'NONE',  ( 83.36324000638602172, -60.00000000000000711, 199.0841329743253141 ) ) ;
#89012 = AXIS2_PLACEMENT_3D ( 'NONE', #54687, #13705, #53645 ) ;
#89013 =( LENGTH_UNIT ( ) NAMED_UNIT ( * ) SI_UNIT ( .MILLI., .METRE. ) );
#89014 = VERTEX_POINT ( 'NONE', #52386 ) ;
#89015 = CARTESIAN_POINT ( 'NONE',  ( 58.31012229776316502, -22.13292565276272583, 60.29346654336805500 ) ) ;
#89016 = CARTESIAN_POINT ( 'NONE',  ( -30.82234192912234860, 298.3178147627863268, -1.235162244126318365 ) ) ;
#89017 = CARTESIAN_POINT ( 'NONE',  ( 80.00000000000000000, -52.00000000000000000, -19.09707704303353282 ) ) ;
#89018 = CARTESIAN_POINT ( 'NONE',  ( -7.897196874019792645, 26.20872795832194058, -1.302055520192085591 ) ) ;
#89019 = VERTEX_POINT ( 'NONE', #100943 ) ;
#89021 = CARTESIAN_POINT ( 'NONE',  ( -9.995943316031024040, -50.00048584071330282, 27.38809334239569182 ) ) ;
#89020 = CARTESIAN_POINT ( 'NONE',  ( -108.5122601155575381, -38.35613504444431499, 141.2758010726541613 ) ) ;
#89022 = FACE_OUTER_BOUND ( 'NONE', #25746, .T. ) ;
#89023 = CARTESIAN_POINT ( 'NONE',  ( 43.00000000000000000, 500.0000000000002274, -15.00000000000000711 ) ) ;
#89024 = DIRECTION ( 'NONE',  ( -0.000000000000000000, -1.000000000000000000, -0.000000000000000000 ) ) ;
#89025 = CARTESIAN_POINT ( 'NONE',  ( -7.188101187500001821, -9.875000002048386349, -2.977408999572651371 ) ) ;
#89026 = CARTESIAN_POINT ( 'NONE',  ( -17.49999999999996447, 48.00000000000000000, 62.61746187599676716 ) ) ;
#89027 = DIRECTION ( 'NONE',  ( 1.000000000000000000, 0.000000000000000000, 0.000000000000000000 ) ) ;
#89028 = ORIENTED_EDGE ( 'NONE', *, *, #28994, .T. ) ;
#89029 = CARTESIAN_POINT ( 'NONE',  ( 83.65262599924042775, -39.46245688817372610, 175.6971847891388165 ) ) ;
#89030 = CARTESIAN_POINT ( 'NONE',  ( 4.919733272805030921, -48.43781863848562352, 104.2477112191711086 ) ) ;
#89031 = CARTESIAN_POINT ( 'NONE',  ( 36.95466138685372925, 27.83244934716666208, 13.30748428295481922 ) ) ;
#89032 = ORIENTED_EDGE ( 'NONE', *, *, #3101, .T. ) ;
#89033 = CARTESIAN_POINT ( 'NONE',  ( -18.99999999999999289, -4.000000000000000000, -1.500000000000001332 ) ) ;
#89034 = CARTESIAN_POINT ( 'NONE',  ( 7.145220222862747939, -4.999999999999987566, -15.42794826860614954 ) ) ;
#89035 = CARTESIAN_POINT ( 'NONE',  ( 26.02782056099105645, 34.92022792041685619, -9.461560381890144811 ) ) ;
#89036 = DIRECTION ( 'NONE',  ( 0.000000000000000000, -0.7633528697427404142, -0.6459817305895909634 ) ) ;
#89037 = MECHANICAL_DESIGN_GEOMETRIC_PRESENTATION_REPRESENTATION (  '', ( #28800 ), #56275 ) ;
#89038 = DIRECTION ( 'NONE',  ( -0.000000000000000000, -0.000000000000000000, 1.000000000000000000 ) ) ;
#89039 = ORIENTED_EDGE ( 'NONE', *, *, #59621, .T. ) ;
#89040 = ADVANCED_FACE ( 'NONE', ( #33187 ), #96991, .T. ) ;
#89041 = CARTESIAN_POINT ( 'NONE',  ( -10.28624191511830155, -1.200000000000000030E-05, -12.90779740156156841 ) ) ;
#89042 = CARTESIAN_POINT ( 'NONE',  ( -0.7777777777777781232, -54.00000000000000711, 40.97837836547555668 ) ) ;
#89043 = EDGE_CURVE ( 'NONE', #87774, #58295, #30810, .T. ) ;
#89045 = CARTESIAN_POINT ( 'NONE',  ( -10.35691556261526713, 16.96077279230471646, -9.900750464959962471 ) ) ;
#89044 = CARTESIAN_POINT ( 'NONE',  ( -14.75116209839011994, 43.55504285526384933, -90.22050492866908655 ) ) ;
#89046 = EDGE_CURVE ( 'NONE', #100880, #13325, #42784, .T. ) ;
#89047 = CARTESIAN_POINT ( 'NONE',  ( 7.188101187500001821, -19.06250000204838813, -2.977408999572650483 ) ) ;
#89048 = UNCERTAINTY_MEASURE_WITH_UNIT (LENGTH_MEASURE( 1.000000000000000082E-05 ), #8046, 'distance_accuracy_value', 'NONE');
#89049 = CARTESIAN_POINT ( 'NONE',  ( -29.09632818934742104, 14.54213905807120000, -41.96777332363188151 ) ) ;
#89050 = PRESENTATION_STYLE_ASSIGNMENT (( #97647 ) ) ;
#89051 = AXIS2_PLACEMENT_3D ( 'NONE', #77525, #44637, #45170 ) ;
#89052 = AXIS2_PLACEMENT_3D ( 'NONE', #63969, #57423, #64491 ) ;
#89053 = VERTEX_POINT ( 'NONE', #13513 ) ;
#89054 = SURFACE_SIDE_STYLE ('',( #71267 ) ) ;
#89055 = EDGE_CURVE ( 'NONE', #1507, #21338, #1660, .T. ) ;
#89056 = EDGE_CURVE ( 'NONE', #2115, #45306, #72283, .T. ) ;
#89057 = CARTESIAN_POINT ( 'NONE',  ( 23.38321737095555619, 25.22051755256121197, 33.19792244304780837 ) ) ;
#89058 = CARTESIAN_POINT ( 'NONE',  ( -3.205024334892935478, 114.6873541103733203, -4.999999999999999112 ) ) ;
#89059 = CARTESIAN_POINT ( 'NONE',  ( -7.421727596595663279, -4.999999999998602007, -70.37058874442158185 ) ) ;
#89060 = CYLINDRICAL_SURFACE ( 'NONE', #15645, 8.500000000000000000 ) ;
#89061 = ORIENTED_EDGE ( 'NONE', *, *, #48050, .T. ) ;
#89062 = DIRECTION ( 'NONE',  ( 0.5735764363510440500, 0.8191520442889932418, 0.000000000000000000 ) ) ;
#89063 = VECTOR ( 'NONE', #99131, 1000.000000000000000 ) ;
#89064 = AXIS2_PLACEMENT_3D ( 'NONE', #15716, #14636, #49131 ) ;
#89065 = ORIENTED_EDGE ( 'NONE', *, *, #40084, .F. ) ;
#89066 = CARTESIAN_POINT ( 'NONE',  ( -2.499999999999944933, -22.55587783588024919, 27.64562232041509304 ) ) ;
#89067 = DIRECTION ( 'NONE',  ( 0.000000000000000000, 0.000000000000000000, 1.000000000000000000 ) ) ;
#89068 = CARTESIAN_POINT ( 'NONE',  ( -44.27708498590406805, 39.31679366924625185, -47.24726744788640076 ) ) ;
#89069 = UNCERTAINTY_MEASURE_WITH_UNIT (LENGTH_MEASURE( 1.000000000000000082E-05 ), #17184, 'distance_accuracy_value', 'NONE');
#89070 = CARTESIAN_POINT ( 'NONE',  ( -112.0871042065531498, -59.99999999999998579, 178.2000521787075229 ) ) ;
#89071 = VECTOR ( 'NONE', #17172, 1000.000000000000000 ) ;
#89072 = FACE_OUTER_BOUND ( 'NONE', #43374, .T. ) ;
#89073 = CIRCLE ( 'NONE', #82209, 4.250000000000000000 ) ;
#89074 = CARTESIAN_POINT ( 'NONE',  ( -15.02532820471274455, 41.95741948359002294, -84.73629005496447064 ) ) ;
#89075 = CONICAL_SURFACE ( 'NONE', #42567, 4.000000000000007105, 0.9599310885968835860 ) ;
#89076 = FACE_OUTER_BOUND ( 'NONE', #53833, .T. ) ;
#89078 = CARTESIAN_POINT ( 'NONE',  ( 36.14965894305566962, 491.8061723310889874, 12.56429772144723422 ) ) ;
#89077 = CARTESIAN_POINT ( 'NONE',  ( 11.99999999999999467, -5.000000000000002665, -86.57079632498522415 ) ) ;
#89079 = CARTESIAN_POINT ( 'NONE',  ( -84.83620007791539308, -28.93200143582290096, 170.9445379179137490 ) ) ;
#89080 = ORIENTED_EDGE ( 'NONE', *, *, #53539, .T. ) ;
#89081 = CIRCLE ( 'NONE', #80437, 7.000000000000000000 ) ;
#89082 = ORIENTED_EDGE ( 'NONE', *, *, #27362, .F. ) ;
#89083 = PRESENTATION_LAYER_ASSIGNMENT (  '', '', ( #8150 ) ) ;
#89084 = FACE_OUTER_BOUND ( 'NONE', #14977, .T. ) ;
#89085 = CARTESIAN_POINT ( 'NONE',  ( 32.93513049338668708, 465.6726574193326655, 10.66039033145099069 ) ) ;
#89086 = CARTESIAN_POINT ( 'NONE',  ( 40.59999999999999432, 3.309500000000003439, 4.052968581778167743E-16 ) ) ;
#89087 = CARTESIAN_POINT ( 'NONE',  ( -14.58597127886967648, 5.499146323183259355, -6.679532531462420764 ) ) ;
#89088 = CARTESIAN_POINT ( 'NONE',  ( 8.642300018710525222, 22.39467290678391009, 1.228393653933357778E-12 ) ) ;
#89089 = DIRECTION ( 'NONE',  ( 0.1269898409407502204, 0.9919025243773941236, -0.001721171576547747550 ) ) ;
#89090 = DIRECTION ( 'NONE',  ( -0.2259255479511525777, 0.3692254281732805232, 0.9014600545632787121 ) ) ;
#89091 = CARTESIAN_POINT ( 'NONE',  ( 105.9102621261374253, -29.99999999999996803, 132.9887338302407898 ) ) ;
#89092 = EDGE_CURVE ( 'NONE', #13329, #28602, #103094, .T. ) ;
#89093 = CARTESIAN_POINT ( 'NONE',  ( -94.62342829788488530, -14.21045842199438525, 80.85070941463327188 ) ) ;
#89094 = CARTESIAN_POINT ( 'NONE',  ( -61.54080906459579836, -46.44072477553419986, 79.75972302785436341 ) ) ;
#89095 = CIRCLE ( 'NONE', #90880, 5.000000000000010658 ) ;
#89096 = EDGE_LOOP ( 'NONE', ( #49312, #20861 ) ) ;
#89097 = CARTESIAN_POINT ( 'NONE',  ( -43.52996882529454581, 484.3120888848611685, 0.7833242031809297679 ) ) ;
#89098 = CARTESIAN_POINT ( 'NONE',  ( 94.27018399449993069, -60.00000000003408474, 15.95119456387866563 ) ) ;
#89099 = EDGE_LOOP ( 'NONE', ( #50958, #61293, #81886, #3232, #29566 ) ) ;
#89100 = DIRECTION ( 'NONE',  ( 0.000000000000000000, 0.000000000000000000, -1.000000000000000000 ) ) ;
#89101 = CARTESIAN_POINT ( 'NONE',  ( 7.188101187499999156, -12.12500000204838635, 2.977408999572654924 ) ) ;
#89102 = FACE_OUTER_BOUND ( 'NONE', #104475, .T. ) ;
#89103 = EDGE_LOOP ( 'NONE', ( #16942, #51199, #17519, #39144, #63304, #82525 ) ) ;
#89104 = CIRCLE ( 'NONE', #44373, 4.000000000000000888 ) ;
#89105 = DIRECTION ( 'NONE',  ( 0.000000000000000000, 0.000000000000000000, 1.000000000000000000 ) ) ;
#89106 = ORIENTED_EDGE ( 'NONE', *, *, #54459, .T. ) ;
#89107 = CYLINDRICAL_SURFACE ( 'NONE', #80305, 8.000000000000000000 ) ;
#89108 = DIRECTION ( 'NONE',  ( -1.000000000000000000, -0.000000000000000000, -0.000000000000000000 ) ) ;
#89109 = CARTESIAN_POINT ( 'NONE',  ( -85.86322845308646379, -59.99999999999998579, 200.5221374670101682 ) ) ;
#89110 = CARTESIAN_POINT ( 'NONE',  ( -3.384215095276410512, -0.8669809812618441969, 104.0501775326196707 ) ) ;
#89111 = CARTESIAN_POINT ( 'NONE',  ( 7.188101187500001821, -23.93750000204838457, -2.977408999572650483 ) ) ;
#89112 = CARTESIAN_POINT ( 'NONE',  ( 38.47428897412579119, 485.7788508071993760, -4.770630528148342542 ) ) ;
#89113 = AXIS2_PLACEMENT_3D ( 'NONE', #6762, #39682, #72557 ) ;
#89114 = CARTESIAN_POINT ( 'NONE',  ( -14.29190075645675861, 21.26710225494873185, 5.626279437267716510 ) ) ;
#89115 = CARTESIAN_POINT ( 'NONE',  ( 4.999999999994901856, -10.14931581695978657, -12.32157755740035121 ) ) ;
#89116 = CARTESIAN_POINT ( 'NONE',  ( 8.642845603823378298, -4.454434588728953592, 14.41908465074281231 ) ) ;
#89117 = CYLINDRICAL_SURFACE ( 'NONE', #87487, 9.500000000000000000 ) ;
#89118 = CARTESIAN_POINT ( 'NONE',  ( 98.58269965288447167, -59.99999999999997158, 196.3309157176815631 ) ) ;
#89119 = CARTESIAN_POINT ( 'NONE',  ( -33.64918128699429190, -60.31113787621708155, 38.51426646422538624 ) ) ;
#89120 = ORIENTED_EDGE ( 'NONE', *, *, #91473, .F. ) ;
#89121 = DIRECTION ( 'NONE',  ( 0.000000000000000000, -1.000000000000000000, 0.000000000000000000 ) ) ;
#89122 = CARTESIAN_POINT ( 'NONE',  ( 37.92194407314020310, -36.05154521609172491, 36.40098896805632478 ) ) ;
#89123 = CARTESIAN_POINT ( 'NONE',  ( 8.569529079650926917, -1.734723475976807094E-15, 14.86825985027943808 ) ) ;
#89124 = ORIENTED_EDGE ( 'NONE', *, *, #98683, .T. ) ;
#89125 = CARTESIAN_POINT ( 'NONE',  ( 95.70911704725124025, 1.016364837396684119E-14, 0.000000000000000000 ) ) ;
#89126 = CARTESIAN_POINT ( 'NONE',  ( -57.80876175898364266, -38.34424999602565975, 89.67284400224633600 ) ) ;
#89127 = ORIENTED_EDGE ( 'NONE', *, *, #80262, .F. ) ;
#89129 = DIRECTION ( 'NONE',  ( 0.000000000000000000, -1.000000000000000000, 0.000000000000000000 ) ) ;
#89128 = CARTESIAN_POINT ( 'NONE',  ( 7.298048344747715355, -5.000000000000000000, -15.50087045093206939 ) ) ;
#89130 = CARTESIAN_POINT ( 'NONE',  ( -33.21102376836596903, 438.9613914113129454, 23.92328486949907074 ) ) ;
#89131 = CARTESIAN_POINT ( 'NONE',  ( 16.14595037822613932, 12.99999999999999289, 0.000000000000000000 ) ) ;
#89132 = CARTESIAN_POINT ( 'NONE',  ( -20.00000000000000000, 12.99999999999999289, 0.000000000000000000 ) ) ;
#89133 = CARTESIAN_POINT ( 'NONE',  ( 80.97977184163765685, 5.000000000000020428, 0.000000000000000000 ) ) ;
#89135 = CIRCLE ( 'NONE', #46095, 0.9999999999999994449 ) ;
#89134 = CARTESIAN_POINT ( 'NONE',  ( 4.814352310392316703, -86.79678594103579314, -3.583053941560736089 ) ) ;
#89136 = CARTESIAN_POINT ( 'NONE',  ( -2.087655452114465682, -49.85878286479394461, 44.72580038709070749 ) ) ;
#89137 = ADVANCED_FACE ( 'NONE', ( #37315 ), #12979, .F. ) ;
#89138 = CARTESIAN_POINT ( 'NONE',  ( 93.33649174705706741, -60.00000000000001421, 35.53938046925307503 ) ) ;
#89139 = B_SPLINE_CURVE_WITH_KNOTS ( 'NONE', 3,
 ( #31455, #30927, #79960, #63807 ),
 .UNSPECIFIED., .F., .F.,
 ( 4, 4 ),
 ( 2.525795506525165703E-17, 0.0006696797651155423844 ),
 .UNSPECIFIED. ) ;
#89140 = CARTESIAN_POINT ( 'NONE',  ( -43.49283539518359731, 484.8086609925252901, 4.190314177826777176 ) ) ;
#89141 = CARTESIAN_POINT ( 'NONE',  ( -3.454253436624930451, -0.8414180287960395521, 103.7259032015043232 ) ) ;
#89142 = CARTESIAN_POINT ( 'NONE',  ( -33.32781438306703592, 490.0012478078861022, 11.19551906514951156 ) ) ;
#89143 = ORIENTED_EDGE ( 'NONE', *, *, #88966, .T. ) ;
#89144 = CARTESIAN_POINT ( 'NONE',  ( -89.88506759848812067, -30.00000000010622259, 28.44306712582588048 ) ) ;
#89145 = EDGE_LOOP ( 'NONE', ( #26429, #70094 ) ) ;
#89146 = CARTESIAN_POINT ( 'NONE',  ( -30.00000000000000000, 450.0000000000002274, 1.202422573753698876 ) ) ;
#89147 = CARTESIAN_POINT ( 'NONE',  ( -15.88092429543819151, 3.778118985513345240, 3.597070451772169442 ) ) ;
#89148 = CARTESIAN_POINT ( 'NONE',  ( 0.000000000000000000, -15.00000000000000000, -8.000000000000000000 ) ) ;
#89150 = CARTESIAN_POINT ( 'NONE',  ( -22.59351686034986528, 27.55929540978658920, -33.04221228726202497 ) ) ;
#89149 = AXIS2_PLACEMENT_3D ( 'NONE', #103548, #23179, #29698 ) ;
#89151 = CARTESIAN_POINT ( 'NONE',  ( 5.082755093536324154, -25.71875000204838813, 5.082755093536326818 ) ) ;
#89152 = DIRECTION ( 'NONE',  ( 0.000000000000000000, -1.000000000000000000, 0.000000000000000000 ) ) ;
#89153 = CARTESIAN_POINT ( 'NONE',  ( 6.872826229292755329, 41.26098029407512513, -70.68506212700772551 ) ) ;
#89154 = ORIENTED_EDGE ( 'NONE', *, *, #104735, .T. ) ;
#89155 = TOROIDAL_SURFACE ( 'NONE', #71902, 5.999999999999994671, 1.000000000000000444 ) ;
#89156 = CIRCLE ( 'NONE', #102945, 7.500000000000006217 ) ;
#89158 = ORIENTED_EDGE ( 'NONE', *, *, #55310, .T. ) ;
#89157 = DIRECTION ( 'NONE',  ( 0.000000000000000000, 1.000000000000000000, 0.000000000000000000 ) ) ;
#89159 = CARTESIAN_POINT ( 'NONE',  ( 81.28744592092785126, -36.02883678850789551, 150.3977081706462968 ) ) ;
#89160 = DIRECTION ( 'NONE',  ( 1.000000000000000000, 0.000000000000000000, 0.000000000000000000 ) ) ;
#89161 = ORIENTED_EDGE ( 'NONE', *, *, #90395, .F. ) ;
#89162 = LINE ( 'NONE', #71372, #3152 ) ;
#89163 = CARTESIAN_POINT ( 'NONE',  ( 7.934996450857311423, -88.86862456472529459, -1.050865690281774345 ) ) ;
#89164 = CARTESIAN_POINT ( 'NONE',  ( 5.082755093536324154, -14.84375000204838457, 5.082755093536326818 ) ) ;
#89165 = CARTESIAN_POINT ( 'NONE',  ( 7.896165657598944065, 26.21088868628027413, -1.307894402814546941 ) ) ;
#89166 = VECTOR ( 'NONE', #29427, 1000.000000000000227 ) ;
#89167 = CARTESIAN_POINT ( 'NONE',  ( -26.05015581842503991, -57.67603816461070920, 43.50693983564572420 ) ) ;
#89168 = CARTESIAN_POINT ( 'NONE',  ( 9.564994042045842804, 294.6554060604858591, 1.895260366468707103 ) ) ;
#89169 = VERTEX_POINT ( 'NONE', #62113 ) ;
#89170 = B_SPLINE_CURVE_WITH_KNOTS ( 'NONE', 3,
 ( #65518, #57937, #40698, #49852, #73586, #98405, #57403, #90318, #33699, #41764, #733, #66574, #102126, #75727, #76784, #28282, #20204, #69775, #102667, #61156 ),
 .UNSPECIFIED., .F., .F.,
 ( 4, 2, 2, 2, 2, 2, 2, 2, 2, 4 ),
 ( 0.007119059105098832045, 0.007623191790411414787, 0.008127324475723998395, 0.008379390818380289332, 0.008631457161036580270, 0.009135589846349162144, 0.009639722531661744018, 0.01014385521697432589, 0.01064798790228690777, 0.01115212058759948964 ),
 .UNSPECIFIED. ) ;
#89171 = SURFACE_STYLE_FILL_AREA ( #63317 ) ;
#89172 = AXIS2_PLACEMENT_3D ( 'NONE', #46474, #37889, #69698 ) ;
#89173 = DIRECTION ( 'NONE',  ( 0.000000000000000000, 1.000000000000000000, 0.000000000000000000 ) ) ;
#89174 = CARTESIAN_POINT ( 'NONE',  ( 7.398423646700466705, 41.20504349441435465, -59.67381333703970370 ) ) ;
#89175 = EDGE_CURVE ( 'NONE', #74726, #3777, #75503, .T. ) ;
#89176 = CARTESIAN_POINT ( 'NONE',  ( 48.55172137731254622, 13.85052760073793543, -16.74335408647284495 ) ) ;
#89177 = VECTOR ( 'NONE', #51953, 1000.000000000000000 ) ;
#89178 = VERTEX_POINT ( 'NONE', #103083 ) ;
#89179 = CARTESIAN_POINT ( 'NONE',  ( 4.898587196589412829E-16, -12.31250000409676915, -8.000000000000000000 ) ) ;
#89180 = CARTESIAN_POINT ( 'NONE',  ( -31.39072542170150015, -22.34702334173443816, 32.41690302228272458 ) ) ;
#89181 = CARTESIAN_POINT ( 'NONE',  ( 9.999999999999998224, 15.23416508903475375, 0.7060372491634900882 ) ) ;
#89182 = CARTESIAN_POINT ( 'NONE',  ( 30.00000000000000000, 0.000000000000000000, 0.000000000000000000 ) ) ;
#89183 = CARTESIAN_POINT ( 'NONE',  ( -8.000000000000000000, -16.24999999999999289, -9.797174393178825657E-16 ) ) ;
#89184 = CARTESIAN_POINT ( 'NONE',  ( 18.58349330513380337, -4.000000000000000888, 4.898587196589416773E-16 ) ) ;
#89185 = APPLICATION_PROTOCOL_DEFINITION ( 'draft international standard', 'automotive_design', 1998, #105855 ) ;
#89186 = CARTESIAN_POINT ( 'NONE',  ( -9.380894568449075877, 32.01130633110942370, -3.467341429141165499 ) ) ;
#89187 = ORIENTED_EDGE ( 'NONE', *, *, #29334, .T. ) ;
#89188 = CARTESIAN_POINT ( 'NONE',  ( -6.958956728584277940, -47.06078234015144091, 39.14832407461615560 ) ) ;
#89189 = CARTESIAN_POINT ( 'NONE',  ( 0.000000000000000000, 15.00000000000000000, 9.999999999999998224 ) ) ;
#89190 = AXIS2_PLACEMENT_3D ( 'NONE', #3544, #86076, #101702 ) ;
#89191 = EDGE_CURVE ( 'NONE', #58245, #82728, #12395, .T. ) ;
#89192 = FACE_BOUND ( 'NONE', #60729, .T. ) ;
#89193 = CARTESIAN_POINT ( 'NONE',  ( -59.29073024543932036, -37.24633815747250765, -34.34540174141172741 ) ) ;
#89194 = DIRECTION ( 'NONE',  ( -1.000000000000000000, 8.400342417351207405E-11, 8.400342417351195773E-11 ) ) ;
#89195 = EDGE_CURVE ( 'NONE', #12690, #22420, #73878, .T. ) ;
#89196 = VERTEX_POINT ( 'NONE', #99207 ) ;
#89197 = VECTOR ( 'NONE', #48709, 1000.000000000000000 ) ;
#89198 = CARTESIAN_POINT ( 'NONE',  ( 3.313708498984762496, -9.968750004096769146, 7.999999999999998224 ) ) ;
#89199 = CARTESIAN_POINT ( 'NONE',  ( 91.22868010984630871, -57.61353597378020197, 204.2121190900673184 ) ) ;
#89200 = CIRCLE ( 'NONE', #104733, 5.000000000000011546 ) ;
#89201 = CARTESIAN_POINT ( 'NONE',  ( 36.20419914068524747, 464.0241112302276179, 19.56059989341736127 ) ) ;
#89202 = CARTESIAN_POINT ( 'NONE',  ( -15.76925030631008262, 22.49347711647530090, 2.473099622738333281 ) ) ;
#89203 = CARTESIAN_POINT ( 'NONE',  ( 56.06921707446437608, 40.83906611471630299, -33.41757057980699130 ) ) ;
#89204 = CARTESIAN_POINT ( 'NONE',  ( -72.77643868140833661, -60.00000000000000000, 160.4837882257039041 ) ) ;
#89205 = CARTESIAN_POINT ( 'NONE',  ( -29.50756122520733271, 297.9063904818165724, 10.61050061783298126 ) ) ;
#89207 = CIRCLE ( 'NONE', #56460, 7.500000000000003553 ) ;
#89206 = CARTESIAN_POINT ( 'NONE',  ( 58.67238219402268840, 6.975173280561618775E-15, 0.000000000000000000 ) ) ;
#89208 = CARTESIAN_POINT ( 'NONE',  ( -40.75641113481592726, 360.0948485545300741, 24.37153223514695100 ) ) ;
#89209 = AXIS2_PLACEMENT_3D ( 'NONE', #88770, #14865, #38646 ) ;
#89210 = CARTESIAN_POINT ( 'NONE',  ( -85.02917054920756357, -46.57021548746553208, 187.6139099441489577 ) ) ;
#89211 = VERTEX_POINT ( 'NONE', #80371 ) ;
#89212 = CARTESIAN_POINT ( 'NONE',  ( 31.49034758424722114, 316.2669363177062110, -6.255441989756967303 ) ) ;
#89213 = ORIENTED_EDGE ( 'NONE', *, *, #6513, .T. ) ;
#89214 = CARTESIAN_POINT ( 'NONE',  ( -7.744991119775241017, -13.46438785425130824, -2.016316005557097224 ) ) ;
#89215 = CARTESIAN_POINT ( 'NONE',  ( 16.65484354297773351, 1.340359594676612611E-15, 0.000000000000000000 ) ) ;
#89216 = CARTESIAN_POINT ( 'NONE',  ( -83.87577431657142313, -52.72623505988846659, -15.45652431476665889 ) ) ;
#89217 = CARTESIAN_POINT ( 'NONE',  ( -42.38863085962758248, 465.0218298503912138, 14.26222171109765569 ) ) ;
#89218 = CARTESIAN_POINT ( 'NONE',  ( 0.000000000000000000, 2.999999999999993339, -10.00000000000000178 ) ) ;
#89219 = COLOUR_RGB ( '', 0.09019608, 0.27058824, 0.51372549) ;
#89220 = VERTEX_POINT ( 'NONE', #25372 ) ;
#89221 = CIRCLE ( 'NONE', #103002, 4.000000000000000888 ) ;
#89223 = CARTESIAN_POINT ( 'NONE',  ( -33.00000000000001421, 464.3970849722209095, 17.41240408234210335 ) ) ;
#89222 = AXIS2_PLACEMENT_3D ( 'NONE', #27560, #78184, #20551 ) ;
#89224 = CARTESIAN_POINT ( 'NONE',  ( 12.88120258102912885, 4.569062003714924991, -7.577876238213450577 ) ) ;
#89225 = CARTESIAN_POINT ( 'NONE',  ( -2.227375807149027054, -1.734723475976807094E-15, 17.01589776168603407 ) ) ;
#89226 = FACE_OUTER_BOUND ( 'NONE', #36417, .T. ) ;
#89227 = EDGE_CURVE ( 'NONE', #93158, #8148, #23778, .T. ) ;
#89228 = CARTESIAN_POINT ( 'NONE',  ( 79.45700042099618088, -60.00000000000000711, -30.99979279722015590 ) ) ;
#89229 = CARTESIAN_POINT ( 'NONE',  ( -79.84541195356943888, -22.14834539919765177, 128.4737088173135646 ) ) ;
#89230 = ORIENTED_EDGE ( 'NONE', *, *, #5905, .T. ) ;
#89231 = CARTESIAN_POINT ( 'NONE',  ( 49.67137106584178241, -60.00000000000004263, 77.31490210218785819 ) ) ;
#89232 = DIRECTION ( 'NONE',  ( -1.000000000000000000, -1.224606353822377258E-16, -0.000000000000000000 ) ) ;
#89233 = CARTESIAN_POINT ( 'NONE',  ( 80.72171367857396262, -57.51083543166566159, 199.5255592465300936 ) ) ;
#89234 = CIRCLE ( 'NONE', #44427, 4.000000000000000888 ) ;
#89235 = VECTOR ( 'NONE', #104374, 1000.000000000000000 ) ;
#89236 = DIRECTION ( 'NONE',  ( 0.000000000000000000, -1.000000000000000000, 0.000000000000000000 ) ) ;
#89237 = CARTESIAN_POINT ( 'NONE',  ( 38.74421784392040280, 310.1584125685482149, 1.633477494702207267 ) ) ;
#89238 = CARTESIAN_POINT ( 'NONE',  ( -12.81329827117308007, 8.851410091539614555, 9.103439556559704826 ) ) ;
#89239 = ORIENTED_EDGE ( 'NONE', *, *, #83718, .F. ) ;
#89240 = SURFACE_SIDE_STYLE ('',( #71441 ) ) ;
#89241 = CARTESIAN_POINT ( 'NONE',  ( -12.50000000000000000, 5.730253409965417433, -23.74922892625246362 ) ) ;
#89242 = CARTESIAN_POINT ( 'NONE',  ( -16.12471489245807987, 36.55922634087986012, 24.15021214291690299 ) ) ;
#89243 = CARTESIAN_POINT ( 'NONE',  ( -2.977408999572654480, -16.62500000204838457, 7.188101187499999156 ) ) ;
#89244 = CARTESIAN_POINT ( 'NONE',  ( 7.169303301815730833, -4.521054846639009916, -7.349897473154584304 ) ) ;
#89245 =( NAMED_UNIT ( * ) SI_UNIT ( $, .STERADIAN. ) SOLID_ANGLE_UNIT ( ) );
#89246 = CARTESIAN_POINT ( 'NONE',  ( 0.000000000000000000, 274.9999999999999432, 0.000000000000000000 ) ) ;
#89247 = EDGE_CURVE ( 'NONE', #43184, #71639, #39342, .T. ) ;
#89248 = DIRECTION ( 'NONE',  ( 0.000000000000000000, -1.000000000000000000, 0.000000000000000000 ) ) ;
#89249 = ORIENTED_EDGE ( 'NONE', *, *, #46719, .T. ) ;
#89250 = CARTESIAN_POINT ( 'NONE',  ( 0.05613245601036472715, 1.278525034529253590, 6.499999999999997335 ) ) ;
#89252 = CARTESIAN_POINT ( 'NONE',  ( 29.17198231074005577, -39.48311188039721031, 32.84881695570470583 ) ) ;
#89251 = CARTESIAN_POINT ( 'NONE',  ( -1.363517047694020823, -14.21045842199434794, 34.36840973699905533 ) ) ;
#89253 = CARTESIAN_POINT ( 'NONE',  ( 23.54757723015212179, 27.32420764371300237, -33.16469143611140424 ) ) ;
#89254 = ORIENTED_EDGE ( 'NONE', *, *, #72986, .T. ) ;
#89255 = B_SPLINE_CURVE_WITH_KNOTS ( 'NONE', 3,
 ( #104284, #77905, #28319, #78420 ),
 .UNSPECIFIED., .F., .F.,
 ( 4, 4 ),
 ( 0.0009108016474575763048, 0.009022848917173635630 ),
 .UNSPECIFIED. ) ;
#89256 = CIRCLE ( 'NONE', #32447, 0.9999999999999976685 ) ;
#89257 = ORIENTED_EDGE ( 'NONE', *, *, #36033, .F. ) ;
#89259 = CARTESIAN_POINT ( 'NONE',  ( 4.651477914329386962E-14, 52.17923068443710832, 7.749999999999496403 ) ) ;
#89258 = DIRECTION ( 'NONE',  ( -1.000000000000000000, -0.000000000000000000, -0.000000000000000000 ) ) ;
#89260 = FACE_OUTER_BOUND ( 'NONE', #75286, .T. ) ;
#89261 = CARTESIAN_POINT ( 'NONE',  ( -43.63213036653843346, 464.4895599185356900, 9.038982508269159055 ) ) ;
#89262 = CARTESIAN_POINT ( 'NONE',  ( 0.000000000000000000, 0.000000000000000000, -11.12471428571428689 ) ) ;
#89263 =( LENGTH_UNIT ( ) NAMED_UNIT ( * ) SI_UNIT ( .MILLI., .METRE. ) );
#89265 = ORIENTED_EDGE ( 'NONE', *, *, #1488, .F. ) ;
#89264 = AXIS2_PLACEMENT_3D ( 'NONE', #91135, #17246, #65778 ) ;
#89266 = EDGE_CURVE ( 'NONE', #103837, #86174, #49644, .T. ) ;
#89267 = CARTESIAN_POINT ( 'NONE',  ( 19.49680244870894441, -59.99999999999999289, -41.87632309024431976 ) ) ;
#89268 = CARTESIAN_POINT ( 'NONE',  ( 21.99079640667137880, 25.96820120819537436, -31.66518509989418106 ) ) ;
#89269 = CARTESIAN_POINT ( 'NONE',  ( 7.500000000000000000, -3.640541674360520119, -0.7158139487964582104 ) ) ;
#89270 = DIRECTION ( 'NONE',  ( -0.000000000000000000, -0.000000000000000000, -1.000000000000000000 ) ) ;
#89271 =( BOUNDED_SURFACE ( )  B_SPLINE_SURFACE ( 1, 2, ( 
 ( #10993, #91413, #20758, #95655, #96192, #53595, #21792, #103215, #79457, #4513, #12064, #61720, #12590, #36919, #102681, #37453, #104259, #87047, #30405, #21269, #38497, #36402, #44994, #86528, #20221, #78927, #70320, #29360, #71359, #53071, #94611, #62250, #29882, #28296, #5569, #88096, #77880, #45524, #70846, #13652, #95135, #62762, #46563, #63294, #78397, #13116, #22322, #55167, #54104, #37985, #46043, #14175, #5051, #103739, #54628, #85992, #87567, #77346, #3457, #69270, #102143, #61171, #94057, #3992, #69787, #28843, #23375, #7152, #82100, #56213, #90208, #16308, #49200, #56758, #72428, #39015, #63825, #8220, #89685, #40065, #30948, #64867, #15783, #97750, #105848, #32533, #47080, #48139, #39552, #22851, #41129, #55686, #33063, #74012, #89151, #15252, #48666, #24453, #40591, #106370, #88617, #31992, #64359, #47609, #98812, #14708, #81036, #23917, #94, #24966, #65933, #73472, #81551, #72942, #7672, #57287, #65403, #98295, #57821, #71896, #90744, #79979, #6095, #104798, #96714, #105332, #80505, #6625, #31476, #97226, #43255, #84244, #2239, #50784, #83696, #91811, #33582, #26060, #1160, #42180, #49740, #58916, #76139, #34134, #91289, #92855, #59452, #101494, #42720, #68609, #84776, #17931, #75068, #68054, #82649, #9801, #67007, #66461, #51326, #43780, #67539, #10861, #8749, #17398, #75613, #99337, #18469, #1713, #34666, #76669, #25514, #99889, #50273, #100419, #60523, #2782, #59999, #10340, #26584, #27646, #35189, #92320, #100951, #83176, #19023, #58369, #35731, #16862, #27108, #51862, #41656, #74543, #9274, #619, #87444, #21147, #61584, #103091, #103609, #20092, #21662, #70185, #4924, #29241, #13522, #3863, #102011, #78791, #95011, #79330, #4383, #62122, #29759, #62634, #53979, #86917, #19559, #37857, #93409, #37324, #36795, #61047, #52394, #85307, #94477, #77751, #93934, #46441, #28172, #71236, #52936, #45391, #11394, #85863, #45914, #11935, #44863, #69661, #102552, #104131, #12987, #70718, #95522, #28703, #54500, #20634, #5450, #53474, #38372, #30274, #44319, #77215, #3325, #86394, #36272, #69139, #12461, #78271, #97104, #80381, #48008, #63705, #5963, #89025, #79855, #15122, #23787, #38888, #56634 ),
 ( #96059, #8091, #80917, #106241, #65273, #6493, #72815, #57165, #98164, #7027, #64745, #56083, #39944, #90077, #71757, #47483, #96590, #64232, #106780, #16184, #32401, #89555, #105206, #73885, #97621, #105722, #72300, #30818, #24318, #104666, #49070, #40997, #31865, #23245, #15651, #88499, #55563, #22725, #81965, #48542, #31352, #81433, #73343, #14577, #63163, #7547, #40463, #22189, #55039, #39424, #87971, #14050, #46955, #18889, #50649, #75482, #43126, #76011, #9669, #26450, #65805, #51194, #32931, #83567, #50143, #488, #98682, #24836, #1024, #17270, #33457, #26975, #74411, #10735, #41524, #91683, #57690, #66332, #92188, #99215, #25379, #83051, #58236, #43650, #42582, #100288, #10213, #91165, #84114, #9143, #100814, #42054, #51734, #1575, #18339, #90613, #16722, #74938, #84651, #34538, #34004, #67412, #66874, #99760, #17799, #25931, #82518, #58788, #49611, #59317, #2110, #8621, #35061, #67929, #59859, #92730, #76539, #21534, #52804, #53863, #28567, #101886, #3739, #77082, #60918, #44734, #69011, #28046, #69534, #29633, #12338, #62508, #53344, #70593, #68474, #3199, #11802, #52264, #19961, #36142, #87310, #86264, #70054, #86792, #93804, #12863, #85730, #103485, #77622, #54367, #78141, #61992, #101365, #27518, #36669, #13393, #45264, #102426, #37191, #61451, #94346, #20508, #4263, #85178, #102960, #19434, #29123, #94884, #11263, #21024, #45782, #78656, #4794, #37734, #46314, #95394, #2650, #35597, #60395, #93272, #44194, #30690, #14450, #38766, #104535, #39299, #106114, #88895, #32266, #23122, #40337, #38251, #46835, #88376, #22058, #80790, #72179, #105085, #73217, #54916, #63578, #5840, #80251, #16058, #65143, #15524, #72700, #47364, #89951, #6902, #96987, #6358, #79736, #81308, #87842, #98041, #57037, #55964, #31226, #14988, #96468, #71631, #13925, #24191, #39824, #64110, #47882, #89434, #22606, #7422, #105598, #97492, #31740, #79206, #55441, #64626, #23650, #56504, #5328, #48417, #71114, #104002, #30149, #63033, #95931, #81835, #67287, #48940, #99631, #66203, #16594, #7959, #40866, #17143, #33336, #49483, #43005, #90487, #26861, #57560, #896, #73758, #82388, #1452, #8496, #41398, #366, #99088, #100167 ) ),
 .UNSPECIFIED., .F., .F., .F. ) 
 B_SPLINE_SURFACE_WITH_KNOTS ( ( 2, 2 ),
 ( 3, 2, 2, 2, 2, 2, 2, 2, 2, 2, 2, 2, 2, 2, 2, 2, 2, 2, 2, 2, 2, 2, 2, 2, 2, 2, 2, 2, 2, 2, 2, 2, 2, 2, 2, 2, 2, 2, 2, 2, 2, 2, 2, 2, 2, 2, 2, 2, 2, 2, 2, 2, 2, 2, 2, 2, 2, 2, 2, 2, 2, 2, 2, 2, 2, 2, 2, 2, 2, 2, 2, 2, 2, 2, 2, 2, 2, 2, 2, 2, 2, 2, 2, 2, 2, 2, 2, 2, 2, 2, 2, 2, 2, 2, 2, 2, 2, 2, 2, 2, 2, 2, 2, 2, 2, 2, 2, 2, 2, 2, 2, 2, 2, 2, 2, 2, 2, 2, 2, 2, 2, 2, 2, 2, 2, 2, 2, 2, 2, 2, 2, 2, 2, 2, 3 ),
 ( 0.000000000000000000, 1.000000000000000000 ),
 ( 0.000000000000000000, 0.007352941176470588133, 0.01470588235294117627, 0.02205882352941176613, 0.02941176470588235253, 0.03676470588235294240, 0.04411764705882353227, 0.05147058823529411520, 0.05882352941176470507, 0.06617647058823529493, 0.07352941176470588480, 0.08088235294117647467, 0.08823529411764706454, 0.09558823529411764053, 0.1029411764705882304, 0.1102941176470588203, 0.1176470588235294101, 0.1250000000000000000, 0.1323529411764705899, 0.1397058823529411797, 0.1470588235294117696, 0.1544117647058823595, 0.1617647058823529493, 0.1691176470588235392, 0.1764705882352941291, 0.1838235294117647189, 0.1911764705882352811, 0.1985294117647058709, 0.2058823529411764608, 0.2132352941176470507, 0.2205882352941176405, 0.2279411764705882304, 0.2352941176470588203, 0.2426470588235294101, 0.2500000000000000000, 0.2573529411764705621, 0.2647058823529411797, 0.2720588235294117418, 0.2794117647058823595, 0.2867647058823529216, 0.2941176470588235392, 0.3014705882352941013, 0.3088235294117647189, 0.3161764705882352811, 0.3235294117647058987, 0.3308823529411764608, 0.3382352941176470784, 0.3455882352941176405, 0.3529411764705882582, 0.3602941176470588203, 0.3676470588235294379, 0.3750000000000000000, 0.3823529411764705621, 0.3897058823529411797, 0.3970588235294117418, 0.4044117647058823595, 0.4117647058823529216, 0.4191176470588235392, 0.4264705882352941013, 0.4338235294117647189, 0.4411764705882352811, 0.4485294117647058987, 0.4558823529411764608, 0.4632352941176470784, 0.4705882352941176405, 0.4779411764705882582, 0.4852941176470588203, 0.4926470588235294379, 0.5000000000000000000, 0.5073529411764705621, 0.5147058823529411242, 0.5220588235294117974, 0.5294117647058823595, 0.5367647058823529216, 0.5441176470588234837, 0.5514705882352941568, 0.5588235294117647189, 0.5661764705882352811, 0.5735294117647058432, 0.5808823529411765163, 0.5882352941176470784, 0.5955882352941176405, 0.6029411764705882026, 0.6102941176470588758, 0.6176470588235294379, 0.6250000000000000000, 0.6323529411764705621, 0.6397058823529411242, 0.6470588235294117974, 0.6544117647058823595, 0.6617647058823529216, 0.6691176470588234837, 0.6764705882352941568, 0.6838235294117647189, 0.6911764705882352811, 0.6985294117647058432, 0.7058823529411765163, 0.7132352941176470784, 0.7205882352941176405, 0.7279411764705882026, 0.7352941176470588758, 0.7426470588235294379, 0.7500000000000000000, 0.7573529411764705621, 0.7647058823529411242, 0.7720588235294117974, 0.7794117647058823595, 0.7867647058823529216, 0.7941176470588234837, 0.8014705882352941568, 0.8088235294117647189, 0.8161764705882352811, 0.8235294117647058432, 0.8308823529411765163, 0.8382352941176470784, 0.8455882352941176405, 0.8529411764705882026, 0.8602941176470588758, 0.8676470588235294379, 0.8750000000000000000, 0.8823529411764705621, 0.8897058823529411242, 0.8970588235294117974, 0.9044117647058823595, 0.9117647058823529216, 0.9191176470588234837, 0.9264705882352941568, 0.9338235294117647189, 0.9411764705882352811, 0.9485294117647058432, 0.9558823529411765163, 0.9632352941176470784, 0.9705882352941176405, 0.9779411764705882026, 0.9804062476877506427 ),
 .UNSPECIFIED. ) 
 GEOMETRIC_REPRESENTATION_ITEM ( )  RATIONAL_B_SPLINE_SURFACE ( (
 ( 1.000000000000000000, 0.9238795325112867385, 1.000000000000000000, 0.9238795325112867385, 1.000000000000000000, 0.9238795325112867385, 1.000000000000000000, 0.9238795325112867385, 1.000000000000000000, 0.9238795325112867385, 1.000000000000000000, 0.9238795325112867385, 1.000000000000000000, 0.9238795325112867385, 1.000000000000000000, 0.9238795325112867385, 1.000000000000000000, 0.9238795325112867385, 1.000000000000000000, 0.9238795325112867385, 1.000000000000000000, 0.9238795325112867385, 1.000000000000000000, 0.9238795325112867385, 1.000000000000000000, 0.9238795325112867385, 1.000000000000000000, 0.9238795325112867385, 1.000000000000000000, 0.9238795325112867385, 1.000000000000000000, 0.9238795325112867385, 1.000000000000000000, 0.9238795325112867385, 1.000000000000000000, 0.9238795325112867385, 1.000000000000000000, 0.9238795325112867385, 1.000000000000000000, 0.9238795325112867385, 1.000000000000000000, 0.9238795325112867385, 1.000000000000000000, 0.9238795325112867385, 1.000000000000000000, 0.9238795325112867385, 1.000000000000000000, 0.9238795325112867385, 1.000000000000000000, 0.9238795325112867385, 1.000000000000000000, 0.9238795325112867385, 1.000000000000000000, 0.9238795325112867385, 1.000000000000000000, 0.9238795325112867385, 1.000000000000000000, 0.9238795325112867385, 1.000000000000000000, 0.9238795325112867385, 1.000000000000000000, 0.9238795325112867385, 1.000000000000000000, 0.9238795325112867385, 1.000000000000000000, 0.9238795325112867385, 1.000000000000000000, 0.9238795325112867385, 1.000000000000000000, 0.9238795325112867385, 1.000000000000000000, 0.9238795325112867385, 1.000000000000000000, 0.9238795325112867385, 1.000000000000000000, 0.9238795325112867385, 1.000000000000000000, 0.9238795325112867385, 1.000000000000000000, 0.9238795325112867385, 1.000000000000000000, 0.9238795325112867385, 1.000000000000000000, 0.9238795325112867385, 1.000000000000000000, 0.9238795325112867385, 1.000000000000000000, 0.9238795325112867385, 1.000000000000000000, 0.9238795325112867385, 1.000000000000000000, 0.9238795325112867385, 1.000000000000000000, 0.9238795325112867385, 1.000000000000000000, 0.9238795325112867385, 1.000000000000000000, 0.9238795325112867385, 1.000000000000000000, 0.9238795325112867385, 1.000000000000000000, 0.9238795325112867385, 1.000000000000000000, 0.9238795325112867385, 1.000000000000000000, 0.9238795325112867385, 1.000000000000000000, 0.9238795325112867385, 1.000000000000000000, 0.9238795325112867385, 1.000000000000000000, 0.9238795325112867385, 1.000000000000000000, 0.9238795325112867385, 1.000000000000000000, 0.9238795325112867385, 1.000000000000000000, 0.9238795325112867385, 1.000000000000000000, 0.9238795325112867385, 1.000000000000000000, 0.9238795325112867385, 1.000000000000000000, 0.9238795325112867385, 1.000000000000000000, 0.9238795325112867385, 1.000000000000000000, 0.9238795325112867385, 1.000000000000000000, 0.9238795325112867385, 1.000000000000000000, 0.9238795325112867385, 1.000000000000000000, 0.9238795325112867385, 1.000000000000000000, 0.9238795325112867385, 1.000000000000000000, 0.9238795325112867385, 1.000000000000000000, 0.9238795325112867385, 1.000000000000000000, 0.9238795325112867385, 1.000000000000000000, 0.9238795325112867385, 1.000000000000000000, 0.9238795325112867385, 1.000000000000000000, 0.9238795325112867385, 1.000000000000000000, 0.9238795325112867385, 1.000000000000000000, 0.9238795325112867385, 1.000000000000000000, 0.9238795325112867385, 1.000000000000000000, 0.9238795325112867385, 1.000000000000000000, 0.9238795325112867385, 1.000000000000000000, 0.9238795325112867385, 1.000000000000000000, 0.9238795325112867385, 1.000000000000000000, 0.9238795325112867385, 1.000000000000000000, 0.9238795325112867385, 1.000000000000000000, 0.9238795325112867385, 1.000000000000000000, 0.9238795325112867385, 1.000000000000000000, 0.9238795325112867385, 1.000000000000000000, 0.9238795325112867385, 1.000000000000000000, 0.9238795325112867385, 1.000000000000000000, 0.9238795325112867385, 1.000000000000000000, 0.9238795325112867385, 1.000000000000000000, 0.9238795325112867385, 1.000000000000000000, 0.9238795325112867385, 1.000000000000000000, 0.9238795325112867385, 1.000000000000000000, 0.9238795325112867385, 1.000000000000000000, 0.9238795325112867385, 1.000000000000000000, 0.9238795325112867385, 1.000000000000000000, 0.9238795325112867385, 1.000000000000000000, 0.9238795325112867385, 1.000000000000000000, 0.9238795325112867385, 1.000000000000000000, 0.9238795325112867385, 1.000000000000000000, 0.9238795325112867385, 1.000000000000000000, 0.9238795325112867385, 1.000000000000000000, 0.9238795325112867385, 1.000000000000000000, 0.9238795325112867385, 1.000000000000000000, 0.9238795325112867385, 1.000000000000000000, 0.9238795325112867385, 1.000000000000000000, 0.9238795325112867385, 1.000000000000000000, 0.9238795325112867385, 1.000000000000000000, 0.9238795325112867385, 1.000000000000000000, 0.9238795325112867385, 1.000000000000000000, 0.9238795325112867385, 1.000000000000000000, 0.9238795325112867385, 1.000000000000000000, 0.9238795325112867385, 1.000000000000000000, 0.9238795325112867385, 1.000000000000000000, 0.9238795325112867385, 1.000000000000000000, 0.9238795325112867385, 1.000000000000000000, 0.9238795325112867385, 1.000000000000000000, 0.9238795325112867385, 1.000000000000000000, 0.9238795325112867385, 1.000000000000000000, 0.9238795325112867385, 1.000000000000000000, 0.9238795325112867385, 1.000000000000000000, 0.9238795325112867385, 1.000000000000000000, 0.9238795325112867385, 1.000000000000000000, 0.9238795325112867385, 1.000000000000000000, 0.9238795325112867385, 1.000000000000000000, 0.9238795325112867385, 1.000000000000000000, 0.9238795325112867385, 1.000000000000000000, 0.9238795325112867385, 1.000000000000000000, 0.9238795325112867385, 1.000000000000000000, 0.9238795325112867385, 1.000000000000000000, 0.9238795325112867385, 1.000000000000000000, 0.9238795325112867385, 1.000000000000000000, 0.9238795325112867385, 1.000000000000000000, 0.9744806372117011950, 0.9660719911230173373),
 ( 1.000000000000000000, 0.9238795325112867385, 1.000000000000000000, 0.9238795325112867385, 1.000000000000000000, 0.9238795325112867385, 1.000000000000000000, 0.9238795325112867385, 1.000000000000000000, 0.9238795325112867385, 1.000000000000000000, 0.9238795325112867385, 1.000000000000000000, 0.9238795325112867385, 1.000000000000000000, 0.9238795325112867385, 1.000000000000000000, 0.9238795325112867385, 1.000000000000000000, 0.9238795325112867385, 1.000000000000000000, 0.9238795325112867385, 1.000000000000000000, 0.9238795325112867385, 1.000000000000000000, 0.9238795325112867385, 1.000000000000000000, 0.9238795325112867385, 1.000000000000000000, 0.9238795325112867385, 1.000000000000000000, 0.9238795325112867385, 1.000000000000000000, 0.9238795325112867385, 1.000000000000000000, 0.9238795325112867385, 1.000000000000000000, 0.9238795325112867385, 1.000000000000000000, 0.9238795325112867385, 1.000000000000000000, 0.9238795325112867385, 1.000000000000000000, 0.9238795325112867385, 1.000000000000000000, 0.9238795325112867385, 1.000000000000000000, 0.9238795325112867385, 1.000000000000000000, 0.9238795325112867385, 1.000000000000000000, 0.9238795325112867385, 1.000000000000000000, 0.9238795325112867385, 1.000000000000000000, 0.9238795325112867385, 1.000000000000000000, 0.9238795325112867385, 1.000000000000000000, 0.9238795325112867385, 1.000000000000000000, 0.9238795325112867385, 1.000000000000000000, 0.9238795325112867385, 1.000000000000000000, 0.9238795325112867385, 1.000000000000000000, 0.9238795325112867385, 1.000000000000000000, 0.9238795325112867385, 1.000000000000000000, 0.9238795325112867385, 1.000000000000000000, 0.9238795325112867385, 1.000000000000000000, 0.9238795325112867385, 1.000000000000000000, 0.9238795325112867385, 1.000000000000000000, 0.9238795325112867385, 1.000000000000000000, 0.9238795325112867385, 1.000000000000000000, 0.9238795325112867385, 1.000000000000000000, 0.9238795325112867385, 1.000000000000000000, 0.9238795325112867385, 1.000000000000000000, 0.9238795325112867385, 1.000000000000000000, 0.9238795325112867385, 1.000000000000000000, 0.9238795325112867385, 1.000000000000000000, 0.9238795325112867385, 1.000000000000000000, 0.9238795325112867385, 1.000000000000000000, 0.9238795325112867385, 1.000000000000000000, 0.9238795325112867385, 1.000000000000000000, 0.9238795325112867385, 1.000000000000000000, 0.9238795325112867385, 1.000000000000000000, 0.9238795325112867385, 1.000000000000000000, 0.9238795325112867385, 1.000000000000000000, 0.9238795325112867385, 1.000000000000000000, 0.9238795325112867385, 1.000000000000000000, 0.9238795325112867385, 1.000000000000000000, 0.9238795325112867385, 1.000000000000000000, 0.9238795325112867385, 1.000000000000000000, 0.9238795325112867385, 1.000000000000000000, 0.9238795325112867385, 1.000000000000000000, 0.9238795325112867385, 1.000000000000000000, 0.9238795325112867385, 1.000000000000000000, 0.9238795325112867385, 1.000000000000000000, 0.9238795325112867385, 1.000000000000000000, 0.9238795325112867385, 1.000000000000000000, 0.9238795325112867385, 1.000000000000000000, 0.9238795325112867385, 1.000000000000000000, 0.9238795325112867385, 1.000000000000000000, 0.9238795325112867385, 1.000000000000000000, 0.9238795325112867385, 1.000000000000000000, 0.9238795325112867385, 1.000000000000000000, 0.9238795325112867385, 1.000000000000000000, 0.9238795325112867385, 1.000000000000000000, 0.9238795325112867385, 1.000000000000000000, 0.9238795325112867385, 1.000000000000000000, 0.9238795325112867385, 1.000000000000000000, 0.9238795325112867385, 1.000000000000000000, 0.9238795325112867385, 1.000000000000000000, 0.9238795325112867385, 1.000000000000000000, 0.9238795325112867385, 1.000000000000000000, 0.9238795325112867385, 1.000000000000000000, 0.9238795325112867385, 1.000000000000000000, 0.9238795325112867385, 1.000000000000000000, 0.9238795325112867385, 1.000000000000000000, 0.9238795325112867385, 1.000000000000000000, 0.9238795325112867385, 1.000000000000000000, 0.9238795325112867385, 1.000000000000000000, 0.9238795325112867385, 1.000000000000000000, 0.9238795325112867385, 1.000000000000000000, 0.9238795325112867385, 1.000000000000000000, 0.9238795325112867385, 1.000000000000000000, 0.9238795325112867385, 1.000000000000000000, 0.9238795325112867385, 1.000000000000000000, 0.9238795325112867385, 1.000000000000000000, 0.9238795325112867385, 1.000000000000000000, 0.9238795325112867385, 1.000000000000000000, 0.9238795325112867385, 1.000000000000000000, 0.9238795325112867385, 1.000000000000000000, 0.9238795325112867385, 1.000000000000000000, 0.9238795325112867385, 1.000000000000000000, 0.9238795325112867385, 1.000000000000000000, 0.9238795325112867385, 1.000000000000000000, 0.9238795325112867385, 1.000000000000000000, 0.9238795325112867385, 1.000000000000000000, 0.9238795325112867385, 1.000000000000000000, 0.9238795325112867385, 1.000000000000000000, 0.9238795325112867385, 1.000000000000000000, 0.9238795325112867385, 1.000000000000000000, 0.9238795325112867385, 1.000000000000000000, 0.9238795325112867385, 1.000000000000000000, 0.9238795325112867385, 1.000000000000000000, 0.9238795325112867385, 1.000000000000000000, 0.9238795325112867385, 1.000000000000000000, 0.9238795325112867385, 1.000000000000000000, 0.9238795325112867385, 1.000000000000000000, 0.9238795325112867385, 1.000000000000000000, 0.9238795325112867385, 1.000000000000000000, 0.9238795325112867385, 1.000000000000000000, 0.9238795325112867385, 1.000000000000000000, 0.9238795325112867385, 1.000000000000000000, 0.9238795325112867385, 1.000000000000000000, 0.9238795325112867385, 1.000000000000000000, 0.9238795325112867385, 1.000000000000000000, 0.9238795325112867385, 1.000000000000000000, 0.9238795325112867385, 1.000000000000000000, 0.9238795325112867385, 1.000000000000000000, 0.9238795325112867385, 1.000000000000000000, 0.9238795325112867385, 1.000000000000000000, 0.9238795325112867385, 1.000000000000000000, 0.9238795325112867385, 1.000000000000000000, 0.9238795325112867385, 1.000000000000000000, 0.9744806372117011950, 0.9660719911230173373) ) ) 
 REPRESENTATION_ITEM ( '' )  SURFACE ( )  );
#89272 = ADVANCED_FACE ( 'NONE', ( #31343 ), #73335, .T. ) ;
#89273 = DIRECTION ( 'NONE',  ( 1.000000000000000000, 0.000000000000000000, -0.000000000000000000 ) ) ;
#89274 = ORIENTED_EDGE ( 'NONE', *, *, #56251, .T. ) ;
#89275 = B_SPLINE_CURVE_WITH_KNOTS ( 'NONE', 3,
 ( #7561, #15138, #48020, #63717, #80930, #7041, #32416, #81446, #23799, #39957, #72831, #32947, #65285, #56648, #24331, #97635 ),
 .UNSPECIFIED., .F., .F.,
 ( 4, 2, 2, 2, 2, 2, 2, 4 ),
 ( 4.443906512722159927E-18, 0.001337001954496015634, 0.002674003908992026064, 0.005348007817984046057, 0.006685009772480056921, 0.008022011726976066917, 0.009359013681472077781, 0.01069601563596808691 ),
 .UNSPECIFIED. ) ;
#89276 = ORIENTED_EDGE ( 'NONE', *, *, #14871, .T. ) ;
#89277 = MECHANICAL_DESIGN_GEOMETRIC_PRESENTATION_REPRESENTATION (  '', ( #4893 ), #35960 ) ;
#89278 = ORIENTED_EDGE ( 'NONE', *, *, #34126, .F. ) ;
#89279 = DIRECTION ( 'NONE',  ( 0.000000000000000000, 0.000000000000000000, 1.000000000000000000 ) ) ;
#89280 = CARTESIAN_POINT ( 'NONE',  ( 104.0908829527487711, -5.000000000000000000, 6.123233995736778115E-16 ) ) ;
#89281 = DIRECTION ( 'NONE',  ( -1.000000000000000000, -1.224606353822377258E-16, -0.000000000000000000 ) ) ;
#89282 = CARTESIAN_POINT ( 'NONE',  ( 28.58679432325043734, 310.5997541753422979, 11.78757380732785798 ) ) ;
#89283 = CARTESIAN_POINT ( 'NONE',  ( -43.81524616929482363, 329.5241525934269475, -1.558685580567496176 ) ) ;
#89284 = CARTESIAN_POINT ( 'NONE',  ( -4.810465484628549504, -64.26601022681093411, 13.02425015433478706 ) ) ;
#89285 = EDGE_CURVE ( 'NONE', #13768, #10730, #53119, .T. ) ;
#89286 = FILL_AREA_STYLE ('',( #5697 ) ) ;
#89287 = CARTESIAN_POINT ( 'NONE',  ( 0.4053525175236821210, 3.145852061456245519, -6.500000000000001776 ) ) ;
#89288 = ORIENTED_EDGE ( 'NONE', *, *, #26452, .F. ) ;
#89289 = CARTESIAN_POINT ( 'NONE',  ( -9.273762745476021863, 44.06279479628684470, 13.41996917811760781 ) ) ;
#89290 = ORIENTED_EDGE ( 'NONE', *, *, #77037, .F. ) ;
#89291 = DIRECTION ( 'NONE',  ( -0.000000000000000000, -0.000000000000000000, -1.000000000000000000 ) ) ;
#89292 = CARTESIAN_POINT ( 'NONE',  ( 17.24303157407923237, 294.5700599009814482, 9.877113118490870036 ) ) ;
#89293 = CARTESIAN_POINT ( 'NONE',  ( -40.17717846856324115, 485.8445156049142497, -4.962122411036295588 ) ) ;
#89294 = AXIS2_PLACEMENT_3D ( 'NONE', #7366, #103427, #95876 ) ;
#89295 = CARTESIAN_POINT ( 'NONE',  ( -55.25757206493887708, -60.00000000000000711, 69.43508648390772464 ) ) ;
#89296 = CARTESIAN_POINT ( 'NONE',  ( 65.80721811158888102, -22.10268982855930631, 79.50398025642166999 ) ) ;
#89297 = EDGE_CURVE ( 'NONE', #84319, #72232, #36144, .T. ) ;
#89298 = ADVANCED_FACE ( 'NONE', ( #98154 ), #15449, .T. ) ;
#89299 = ORIENTED_EDGE ( 'NONE', *, *, #35206, .T. ) ;
#89300 = CARTESIAN_POINT ( 'NONE',  ( 42.44442147538608623, 464.7190447730621941, 16.13393895236494657 ) ) ;
#89301 = CARTESIAN_POINT ( 'NONE',  ( -5.888319653649580765, 11.68640158625127512, 3.787045357069727558 ) ) ;
#89302 = CARTESIAN_POINT ( 'NONE',  ( -5.647684535521968918, -57.67118449236373579, -44.55142524122563685 ) ) ;
#89303 = ORIENTED_EDGE ( 'NONE', *, *, #33808, .T. ) ;
#89304 = LINE ( 'NONE', #80656, #79788 ) ;
#89305 = PRESENTATION_LAYER_ASSIGNMENT (  '', '', ( #106526 ) ) ;
#89306 = PRESENTATION_LAYER_ASSIGNMENT (  '', '', ( #80896 ) ) ;
#89307 = CARTESIAN_POINT ( 'NONE',  ( -36.65190467452315914, 491.8432146685187263, 12.58836626716444052 ) ) ;
#89308 = CARTESIAN_POINT ( 'NONE',  ( 8.000000000000000000, -29.09375000409677270, -3.313708498984761608 ) ) ;
#89309 = AXIS2_PLACEMENT_3D ( 'NONE', #68070, #44876, #27121 ) ;
#89310 = CARTESIAN_POINT ( 'NONE',  ( 9.989113211954187221, 246.0270072645100470, 0.5334031035449080527 ) ) ;
#89311 = CARTESIAN_POINT ( 'NONE',  ( -43.75010090113929806, 464.8337800386750018, 11.75004750934965791 ) ) ;
#89312 = CARTESIAN_POINT ( 'NONE',  ( 9.948688207305192321, 33.87023149490183727, -1.044946705213435800 ) ) ;
#89313 = CARTESIAN_POINT ( 'NONE',  ( 13.50000000000000355, 2.646256834279082870, -0.1392913482116632518 ) ) ;
#89314 = FACE_OUTER_BOUND ( 'NONE', #4918, .T. ) ;
#89315 = VERTEX_POINT ( 'NONE', #81957 ) ;
#89316 = DIRECTION ( 'NONE',  ( -1.000000000000000000, -1.224606353822377258E-16, -0.000000000000000000 ) ) ;
#89317 = DIRECTION ( 'NONE',  ( 1.000000000000000000, 1.224606353822377258E-16, 0.000000000000000000 ) ) ;
#89318 = CARTESIAN_POINT ( 'NONE',  ( 8.537483284794495475, -60.00000000000000000, 39.63655399926129519 ) ) ;
#89319 = CARTESIAN_POINT ( 'NONE',  ( -93.75466218594513634, -30.00000000000000355, 191.2470980862353542 ) ) ;
#89320 = ADVANCED_FACE ( 'NONE', ( #11255 ), #10726, .F. ) ;
#89321 = AXIS2_PLACEMENT_3D ( 'NONE', #31400, #76057, #28092 ) ;
#89322 = VECTOR ( 'NONE', #10633, 999.9999999999998863 ) ;
#89323 = CARTESIAN_POINT ( 'NONE',  ( -39.04658448874435095, 485.1639453003155609, -4.285642725068625758 ) ) ;
#89324 = CARTESIAN_POINT ( 'NONE',  ( 39.85978143129780449, -57.69245178989500999, 55.45386101768630738 ) ) ;
#89325 = EDGE_CURVE ( 'NONE', #49147, #17674, #6825, .T. ) ;
#89327 = CARTESIAN_POINT ( 'NONE',  ( -46.00000000000000000, 488.0336798547363628, -0.8984331811837280579 ) ) ;
#89326 = CARTESIAN_POINT ( 'NONE',  ( -1.250427155780938104, 25.55909391395953278, -39.65635458840486649 ) ) ;
#89328 = VECTOR ( 'NONE', #55208, 1000.000000000000000 ) ;
#89329 = CARTESIAN_POINT ( 'NONE',  ( 10.14997255787597297, -22.66085254118687331, -38.54259180169733412 ) ) ;
#89330 = CARTESIAN_POINT ( 'NONE',  ( -9.999999999999960920, 15.00000000000001066, 3.836411046841925465 ) ) ;
#89331 = CARTESIAN_POINT ( 'NONE',  ( -46.00000000000000000, 438.2055348968746102, 15.52909715636657495 ) ) ;
#89332 = CARTESIAN_POINT ( 'NONE',  ( -4.079827781214096838, -60.00000000000000000, 39.63120119151885490 ) ) ;
#89333 = APPLICATION_CONTEXT ( 'automotive_design' ) ;
#89334 = CARTESIAN_POINT ( 'NONE',  ( 12.91142918290874597, 8.665321034538903788, 9.018047713757219697 ) ) ;
#89335 = CARTESIAN_POINT ( 'NONE',  ( 35.07179216366485974, 463.5162043426228706, 19.70794395571530089 ) ) ;
#89336 = B_SPLINE_CURVE_WITH_KNOTS ( 'NONE', 3,
 ( #30601, #29554, #88288, #55358, #39737, #95317 ),
 .UNSPECIFIED., .F., .F.,
 ( 4, 2, 4 ),
 ( 0.02294124189247801621, 0.02484059228080999493, 0.02673994266914197365 ),
 .UNSPECIFIED. ) ;
#89337 = CARTESIAN_POINT ( 'NONE',  ( -86.39639614912320553, -50.14485074065887460, 191.2668530642233975 ) ) ;
#89338 = ORIENTED_EDGE ( 'NONE', *, *, #19278, .F. ) ;
#89339 = CARTESIAN_POINT ( 'NONE',  ( 17.50000000000002842, 51.99998113221720075, 59.93765433267320475 ) ) ;
#89340 = CARTESIAN_POINT ( 'NONE',  ( 29.68315524077033629, 13.47185074185905584, 42.10535821593451544 ) ) ;
#89341 = CARTESIAN_POINT ( 'NONE',  ( -11.48823353272537240, -53.40259021410059859, 32.82079992462674056 ) ) ;
#89342 = DIRECTION ( 'NONE',  ( 1.000000000000000000, 1.224606353822377258E-16, 0.000000000000000000 ) ) ;
#89343 = B_SPLINE_SURFACE_WITH_KNOTS ( 'NONE', 1, 3, ( 
 ( #39274, #64084, #63009, #87818, #20999, #88350, #38737, #94856 ),
 ( #13895, #54344, #95906, #96442, #12837, #14424, #22030, #104510 ) ),
 .UNSPECIFIED., .F., .F., .F.,
 ( 2, 2 ),
 ( 4, 2, 2, 4 ),
 ( 0.000000000000000000, 1.000000000000000000 ),
 ( 0.000000000000000000, 0.04450745600790868145, 0.06676118401186306728, 0.08901491201581737678 ),
 .UNSPECIFIED. ) ;
#89344 = CARTESIAN_POINT ( 'NONE',  ( 0.000000000000000000, -5.000000000000000888, -73.00000000000001421 ) ) ;
#89345 = EDGE_CURVE ( 'NONE', #33707, #76918, #25835, .T. ) ;
#89346 = ORIENTED_EDGE ( 'NONE', *, *, #36551, .F. ) ;
#89347 = DIRECTION ( 'NONE',  ( -1.000000000000000000, -1.224606353822377258E-16, -0.000000000000000000 ) ) ;
#89348 = COLOUR_RGB ( '', 0.08235294, 0.09019608, 0.10196078) ;
#89349 = CARTESIAN_POINT ( 'NONE',  ( -7.417322861528432121, -5.000000000002099654, -16.62528780686862717 ) ) ;
#89350 = CARTESIAN_POINT ( 'NONE',  ( -6.928203230275510549, 30.00000000000000000, 4.000000000000000000 ) ) ;
#89351 = FACE_OUTER_BOUND ( 'NONE', #89103, .T. ) ;
#89352 = CARTESIAN_POINT ( 'NONE',  ( 0.000000000000000000, 0.000000000000000000, -13.00000000000000000 ) ) ;
#89353 = CARTESIAN_POINT ( 'NONE',  ( 65.96454949761043451, -60.00000000000000000, 122.2396239898068018 ) ) ;
#89354 = EDGE_CURVE ( 'NONE', #45380, #66630, #30975, .T. ) ;
#89355 = CARTESIAN_POINT ( 'NONE',  ( -26.97491686565329161, 307.4599153070161606, -9.420584459367200125 ) ) ;
#89356 = ORIENTED_EDGE ( 'NONE', *, *, #34942, .T. ) ;
#89357 = CARTESIAN_POINT ( 'NONE',  ( 46.36650669486618881, 4.898587196589411843E-16, -4.000000000000000888 ) ) ;
#89358 = PRESENTATION_STYLE_ASSIGNMENT (( #48339 ) ) ;
#89360 = CARTESIAN_POINT ( 'NONE',  ( 0.000000000000000000, 0.000000000000000000, 5.000000000000000888 ) ) ;
#89359 = CARTESIAN_POINT ( 'NONE',  ( 37.54937173058232247, -29.99999999999994671, 45.10736187702755018 ) ) ;
#89361 = DIRECTION ( 'NONE',  ( -0.000000000000000000, 1.000000000000000000, -0.000000000000000000 ) ) ;
#89362 = CIRCLE ( 'NONE', #73787, 8.000000000000000000 ) ;
#89363 = CARTESIAN_POINT ( 'NONE',  ( -4.928386788250540995, -1.571875576847017397, 104.2441249819467686 ) ) ;
#89364 = ORIENTED_EDGE ( 'NONE', *, *, #3797, .T. ) ;
#89365 = CARTESIAN_POINT ( 'NONE',  ( -26.22871651383309910, 309.5540286940661190, 10.04294722306419807 ) ) ;
#89366 = ORIENTED_EDGE ( 'NONE', *, *, #40633, .F. ) ;
#89367 = DIRECTION ( 'NONE',  ( 0.000000000000000000, -1.000000000000000000, 0.000000000000000000 ) ) ;
#89368 = CARTESIAN_POINT ( 'NONE',  ( 3.648665620917491470, 15.00000000000000000, 9.999999999999998224 ) ) ;
#89369 = LINE ( 'NONE', #81770, #81890 ) ;
#89370 = DIRECTION ( 'NONE',  ( 0.000000000000000000, -1.000000000000000000, 0.000000000000000000 ) ) ;
#89372 = ADVANCED_FACE ( 'NONE', ( #60909 ), #10073, .T. ) ;
#89371 = EDGE_LOOP ( 'NONE', ( #44310, #65410, #45200, #28041, #84509 ) ) ;
#89373 = CARTESIAN_POINT ( 'NONE',  ( -58.90678327790172375, 48.00000000000000000, -28.11551192219426909 ) ) ;
#89374 = DIRECTION ( 'NONE',  ( 0.000000000000000000, 1.000000000000000000, 0.000000000000000000 ) ) ;
#89375 = CARTESIAN_POINT ( 'NONE',  ( -96.27974869280906489, -60.00000000000978417, 205.0145893238625092 ) ) ;
#89376 = CARTESIAN_POINT ( 'NONE',  ( 6.585530689845733754, -4.023059358968673394, -6.500000000000002665 ) ) ;
#89377 = CARTESIAN_POINT ( 'NONE',  ( 75.01455921003739036, -59.99999999999997868, 181.4220384249936444 ) ) ;
#89378 = CARTESIAN_POINT ( 'NONE',  ( 43.86560043478110060, 486.1043823555136214, 5.341761608528310390 ) ) ;
#89379 = CARTESIAN_POINT ( 'NONE',  ( 1.010662029212957780, 25.34442020277418450, -40.25335562281891555 ) ) ;
#89381 = CARTESIAN_POINT ( 'NONE',  ( 17.60034620493656377, -25.55031154538487215, 28.43495793658222581 ) ) ;
#89380 = CARTESIAN_POINT ( 'NONE',  ( -104.4188068117427264, -29.99999999999997868, 196.2181340123987923 ) ) ;
#89382 = AXIS2_PLACEMENT_3D ( 'NONE', #101239, #93141, #1987 ) ;
#89383 = CARTESIAN_POINT ( 'NONE',  ( 83.27655652115849705, -38.00000000000000711, -5.287797665593598317 ) ) ;
#89384 = CARTESIAN_POINT ( 'NONE',  ( 0.3347578696900010420, 53.41133083292604766, -10.20729091610875905 ) ) ;
#89385 = CARTESIAN_POINT ( 'NONE',  ( -44.69002865036945593, -36.07507680361931079, 42.37332714719177318 ) ) ;
#89386 = DIRECTION ( 'NONE',  ( -1.000000000000000000, -1.224606353822377258E-16, -0.000000000000000000 ) ) ;
#89387 = ORIENTED_EDGE ( 'NONE', *, *, #18377, .T. ) ;
#89388 = DIRECTION ( 'NONE',  ( 0.000000000000000000, 0.000000000000000000, 1.000000000000000000 ) ) ;
#89389 = TOROIDAL_SURFACE ( 'NONE', #99685, 7.500000000000000888, 5.000000000000000000 ) ;
#89390 = LINE ( 'NONE', #32763, #87025 ) ;
#89391 = FACE_OUTER_BOUND ( 'NONE', #29092, .T. ) ;
#89392 = DIRECTION ( 'NONE',  ( 0.000000000000000000, 0.000000000000000000, -1.000000000000000000 ) ) ;
#89393 = CARTESIAN_POINT ( 'NONE',  ( 5.477432325710314132, -6.835204644295279408, 2.459915882346691340 ) ) ;
#89394 = CARTESIAN_POINT ( 'NONE',  ( 35.76320840016588676, 388.4727839510825333, 5.610592865731860002 ) ) ;
#89395 = ORIENTED_EDGE ( 'NONE', *, *, #14073, .F. ) ;
#89396 = CARTESIAN_POINT ( 'NONE',  ( 4.399054598113104397, -48.11244280224734382, 102.7269706464928021 ) ) ;
#89397 = EDGE_LOOP ( 'NONE', ( #66914, #86112, #57517, #48980 ) ) ;
#89398 = CARTESIAN_POINT ( 'NONE',  ( 96.49954056570551586, -29.99999999997318767, 199.8705361785111450 ) ) ;
#89399 = DIRECTION ( 'NONE',  ( 1.000000000000000000, 1.224606353822377258E-16, 0.000000000000000000 ) ) ;
#89400 = CARTESIAN_POINT ( 'NONE',  ( 6.916165809215955917, 41.81554757990602411, -59.83173451229081508 ) ) ;
#89401 = CARTESIAN_POINT ( 'NONE',  ( 100.2850625226886621, -30.00000000000001066, 156.5047868331033385 ) ) ;
#89402 = EDGE_CURVE ( 'NONE', #71171, #39671, #56546, .T. ) ;
#89403 = CARTESIAN_POINT ( 'NONE',  ( 7.414346147791995634, 102.3541084233773262, -3.010818766110535005 ) ) ;
#89404 = ORIENTED_EDGE ( 'NONE', *, *, #82761, .F. ) ;
#89405 = AXIS2_PLACEMENT_3D ( 'NONE', #85100, #11186, #82974 ) ;
#89406 = ORIENTED_EDGE ( 'NONE', *, *, #40555, .F. ) ;
#89407 = ORIENTED_EDGE ( 'NONE', *, *, #89462, .T. ) ;
#89409 = AXIS2_PLACEMENT_3D ( 'NONE', #26354, #67306, #75373 ) ;
#89408 = CARTESIAN_POINT ( 'NONE',  ( -32.28552837373647577, 464.7648866755938002, 15.30384310834765671 ) ) ;
#89410 = CARTESIAN_POINT ( 'NONE',  ( -1.000000000000000222, -5.000000000000000000, -14.14213562373095101 ) ) ;
#89411 = CARTESIAN_POINT ( 'NONE',  ( -42.00745990515054018, 464.8754194883779860, 15.22999261134830284 ) ) ;
#89412 = ADVANCED_FACE ( 'NONE', ( #42576 ), #2103, .F. ) ;
#89414 = EDGE_LOOP ( 'NONE', ( #20566, #88886, #31790, #70016 ) ) ;
#89413 = VECTOR ( 'NONE', #67522, 1000.000000000000000 ) ;
#89415 = CONICAL_SURFACE ( 'NONE', #53227, 4.172000000000009479, 0.9599310885968813656 ) ;
#89416 = ORIENTED_EDGE ( 'NONE', *, *, #56990, .F. ) ;
#89417 = CARTESIAN_POINT ( 'NONE',  ( 18.58349330513380693, 1.593028355512270962E-15, 0.000000000000000000 ) ) ;
#89418 = CARTESIAN_POINT ( 'NONE',  ( 83.66693253132321217, -38.78100776230738234, 197.5407986867839725 ) ) ;
#89419 = CARTESIAN_POINT ( 'NONE',  ( 10.12940370570886373, 12.28737531179036857, 10.56278064024531282 ) ) ;
#89420 = CARTESIAN_POINT ( 'NONE',  ( 86.80186013151742941, -38.00000000000003553, 188.4282799762682998 ) ) ;
#89421 = CARTESIAN_POINT ( 'NONE',  ( 29.71096116145698218, 314.7497564551254641, 12.83474296151334748 ) ) ;
#89422 = CARTESIAN_POINT ( 'NONE',  ( 0.000000000000000000, 0.000000000000000000, 0.000000000000000000 ) ) ;
#89423 = VECTOR ( 'NONE', #62326, 1000.000000000000000 ) ;
#89424 = FACE_OUTER_BOUND ( 'NONE', #88930, .T. ) ;
#89425 = CARTESIAN_POINT ( 'NONE',  ( 65.03872891708842019, -4.000000000000000000, 0.000000000000000000 ) ) ;
#89426 = CARTESIAN_POINT ( 'NONE',  ( -5.833333333333327708, -46.00000000000000000, 103.8776713793258608 ) ) ;
#89427 = CARTESIAN_POINT ( 'NONE',  ( -4.839255126185086020, 7.222890253225617840, 5.000000000000000000 ) ) ;
#89428 = VERTEX_POINT ( 'NONE', #84106 ) ;
#89429 = CARTESIAN_POINT ( 'NONE',  ( -35.51695525948886711, 413.2530085246343674, 6.941884492246507499 ) ) ;
#89431 = CARTESIAN_POINT ( 'NONE',  ( -25.69622924537841868, 305.2338348851055230, 10.47102872775464100 ) ) ;
#89430 =( LENGTH_UNIT ( ) NAMED_UNIT ( * ) SI_UNIT ( .MILLI., .METRE. ) );
#89432 = LINE ( 'NONE', #6355, #3726 ) ;
#89433 = UNCERTAINTY_MEASURE_WITH_UNIT (LENGTH_MEASURE( 1.000000000000000082E-05 ), #709, 'distance_accuracy_value', 'NONE');
#89434 = CARTESIAN_POINT ( 'NONE',  ( 3.313708498984762052, -13.71874999999999112, -8.000000000000000000 ) ) ;
#89435 = CARTESIAN_POINT ( 'NONE',  ( -6.118049227779695620, -18.82936832617644640, 35.12770106459590380 ) ) ;
#89436 =( BOUNDED_SURFACE ( )  B_SPLINE_SURFACE ( 3, 2, ( 
 ( #53619, #47107, #29387 ),
 ( #12090, #22352, #95158 ),
 ( #21290, #69810, #46589 ),
 ( #46071, #55197, #88125 ),
 ( #61743, #94639, #14205 ),
 ( #20784, #86554, #5077 ),
 ( #38011, #16341, #88644 ),
 ( #82130, #105877, #6654 ),
 ( #89181, #47636, #23402 ),
 ( #65433, #15282, #80536 ) ),
 .UNSPECIFIED., .F., .F., .F. ) 
 B_SPLINE_SURFACE_WITH_KNOTS ( ( 4, 2, 2, 2, 4 ),
 ( 3, 3 ),
 ( 0.002450517525418899507, 0.003060732775749471640, 0.003670948026080044207, 0.004891378526741188906, 0.007332239528063478305 ),
 ( 0.000000000000000000, 1.000000000000000000 ),
 .UNSPECIFIED. ) 
 GEOMETRIC_REPRESENTATION_ITEM ( )  RATIONAL_B_SPLINE_SURFACE ( (
 ( 1.000000000000000000, 0.7071067811865470176, 1.000000000000000000),
 ( 1.000000000000000000, 0.7344063550101938009, 1.000000000000000000),
 ( 1.000000000000000000, 0.7590375248711010991, 1.000000000000000000),
 ( 1.000000000000000000, 0.8038331608704093467, 1.000000000000000000),
 ( 1.000000000000000000, 0.8240352460866127160, 1.000000000000000000),
 ( 1.000000000000000000, 0.8791017378332789400, 1.000000000000000000),
 ( 1.000000000000000000, 0.9085032776980890290, 1.000000000000000000),
 ( 1.000000000000000000, 0.9784170511696812511, 1.000000000000000000),
 ( 1.000000000000000000, 0.9996598051696619081, 1.000000000000000000),
 ( 1.000000000000000000, 1.000000000000000000, 1.000000000000000000) ) ) 
 REPRESENTATION_ITEM ( '' )  SURFACE ( )  );
#89437 = CARTESIAN_POINT ( 'NONE',  ( -7.500000000000006217, 39.99999999999122480, -59.88032989330939415 ) ) ;
#89438 = DIRECTION ( 'NONE',  ( 1.224646799147351482E-16, 0.000000000000000000, -1.000000000000000000 ) ) ;
#89440 = VERTEX_POINT ( 'NONE', #69002 ) ;
#89439 =( BOUNDED_SURFACE ( )  B_SPLINE_SURFACE ( 2, 3, ( 
 ( #78266, #59992, #86389, #44314, #82780, #100946, #77208, #28698, #2776, #93404, #69656, #43776, #85857, #35726, #12456, #52390, #10856, #85302, #94470, #36267, #8882, #102547, #11388, #35184, #41787, #92852, #45385, #61042, #52931, #101489, #19018, #74669, #4378, #37318, #70180, #93929, #11930, #25101, #3320, #57957, #27641, #69134, #90882, #28166, #16997, #49874, #51859, #22720, #23240, #30270, #4919, #55558, #14572, #38367, #88494, #30813, #96055, #47478, #31347, #95517, #37851, #71231, #80376, #70714, #103604, #71752, #95007, #12982, #56078, #96586, #63159, #22183, #64227, #7022, #97099, #62117, #104661, #6488, #38883, #72294, #79326, #39419, #55034, #79850, #29755, #53973, #105201, #63699, #89020, #62629, #87966, #104127, #48003, #14046, #15116, #46950, #5959, #78786, #21658, #80911, #39939, #103086, #29236, #21142, #86912, #45910, #54494, #87439, #13516, #46436, #5445, #64740, #7542, #90608, #56629, #33452, #24831, #65268, #99210, #57160, #72810, #16717, #97616, #89550, #83046, #82513, #8086, #40991, #91159, #1019, #17265, #31860, #49606, #66327, #57685, #25374 ),
 ( #81428, #23781, #8616, #41519, #74406, #48537, #73880, #49065, #42049, #106775, #483, #81960, #98677, #15646, #40458, #9138, #74933, #32926, #65800, #58230, #50138, #105717, #24313, #90072, #16179, #73338, #106236, #32395, #98158, #2367, #78391, #76261, #76790, #20212, #29353, #69263, #77872, #35312, #86520, #68176, #4507, #37444, #69782, #62245, #20753, #27770, #70313, #2895, #53066, #102674, #85985, #101072, #10985, #53591, #12057, #95129, #10458, #45517, #44986, #94605, #61713, #27232, #36913, #12583, #44444, #51981, #103208, #60645, #92983, #68731, #21261, #11514, #54098, #60118, #43377, #77338, #19144, #52516, #84898, #28836, #43902, #85432, #35855, #102135, #3449, #101615, #93531, #19677, #36396, #3984, #28289, #61164, #94050, #7145, #78920, #54619, #89144, #64860, #48132, #55160, #14701, #5562, #5044, #72421, #38491, #97743, #104251, #23368, #95650, #79451, #96185, #47073, #80497, #39008, #31468, #30399, #22845, #105842, #96708, #46557, #104791, #23910, #79973, #6618, #6090, #87042, #87561, #37978, #81029, #46037, #71352, #55678, #31986, #71887, #47602, #70839 ),
 ( #39544, #13110, #97220, #63285, #40057, #22314, #88611, #105325, #64351, #103731, #13644, #56206, #15245, #29877, #62754, #72934, #21785, #88089, #14169, #30940, #63818, #67001, #90737, #98288, #34127, #74004, #32526, #8212, #1706, #57814, #1154, #81543, #17925, #16853, #40584, #98805, #15776, #75061, #58910, #24960, #50777, #8742, #49734, #7666, #83169, #24446, #90202, #25506, #41650, #73466, #99882, #83690, #48659, #57279, #91804, #34661, #9796, #82641, #91284, #82093, #106361, #42174, #41121, #67533, #87, #26054, #65396, #74536, #16302, #613, #49193, #17392, #33056, #33576, #100413, #56750, #89678, #65926, #42712, #66455, #99331, #75607, #58363, #50267, #9267, #28164, #44857, #76133, #20085, #92313, #11386, #2233, #101487, #27102, #27638, #60517, #61577, #35182, #52388, #4376, #70178, #37316, #92850, #77746, #10854, #77206, #69654, #19551, #93402, #26578, #61040, #3857, #68048, #52929, #18464, #44312, #100944, #85300, #59990, #3318, #36263, #94468, #19015, #35724, #69132, #85855, #102005, #36788, #76662, #93927, #45383, #11928, #51857, #102545, #59446, #28696 ) ),
 .UNSPECIFIED., .F., .F., .F. ) 
 B_SPLINE_SURFACE_WITH_KNOTS ( ( 3, 3 ),
 ( 4, 2, 2, 2, 2, 2, 2, 2, 2, 2, 2, 2, 2, 2, 2, 2, 2, 2, 2, 2, 2, 2, 2, 2, 2, 2, 2, 2, 2, 2, 2, 2, 2, 2, 2, 2, 2, 2, 2, 2, 2, 2, 2, 2, 2, 2, 2, 2, 2, 2, 2, 2, 2, 2, 2, 2, 2, 2, 2, 2, 2, 2, 2, 2, 2, 2, 2, 4 ),
 ( 0.000000000000000000, 1.000000000000000000 ),
 ( 0.000000000000000000, 0.01154064568618346810, 0.02308129137236693620, 0.03462193705855040604, 0.04616258274473387241, 0.06924387411710081208, 0.09232516548946774482, 0.1038658111756512181, 0.1154064568618346776, 0.1211767797049264211, 0.1269471025480181647, 0.1327174253911098945, 0.1356025868126557454, 0.1384877482342016242, 0.1399303289449745635, 0.1413729096557475029, 0.1420942000111339587, 0.1428154903665204145, 0.1431761355442136563, 0.1435367807219068981, 0.1442580710772933539, 0.1457006517880662932, 0.1464219421434527491, 0.1471432324988392049, 0.1485858132096121442, 0.1493071035649986000, 0.1500283939203850836, 0.1503890390980783254, 0.1507496842757715672, 0.1509300068646181880, 0.1511103294534648089, 0.1512004907478881055, 0.1512906520423114021, 0.1514709746311580230, 0.1518316198088512370, 0.1521922649865444788, 0.1529135553419309623, 0.1543561360527038739, 0.1557987167634768133, 0.1586838781850226643, 0.1615690396065685430, 0.1673393624496602727, 0.1731096852927520025, 0.1846503309789354896, 0.2077316223513024362, 0.2308129137236693551, 0.2769754964684032483, 0.3000567878407701672, 0.3231380792131370860, 0.3346787248993205455, 0.3404490477424122474, 0.3462193705855040049, 0.3491045320070498836, 0.3519896934285957624, 0.3534322741393687295, 0.3548748548501416411, 0.3563174355609145527, 0.3570387259163010363, 0.3573993710939942781, 0.3577600162716875198, 0.3581206614493807616, 0.3584813066270740034, 0.3592025969824604870, 0.3606451776932333986, 0.3620877584040063102, 0.3635303391147792773, 0.3664155005363251005, 0.3693006619578709793 ),
 .UNSPECIFIED. ) 
 GEOMETRIC_REPRESENTATION_ITEM ( )  RATIONAL_B_SPLINE_SURFACE ( (
 ( 1.000000000000000000, 1.000000000000000000, 1.000000000000000000, 1.000000000000000000, 1.000000000000000000, 1.000000000000000000, 1.000000000000000000, 1.000000000000000000, 1.000000000000000000, 1.000000000000000000, 1.000000000000000000, 1.000000000000000000, 1.000000000000000000, 1.000000000000000000, 1.000000000000000000, 1.000000000000000000, 1.000000000000000000, 1.000000000000000000, 1.000000000000000000, 1.000000000000000000, 1.000000000000000000, 1.000000000000000000, 1.000000000000000000, 1.000000000000000000, 1.000000000000000000, 1.000000000000000000, 1.000000000000000000, 1.000000000000000000, 1.000000000000000000, 1.000000000000000000, 1.000000000000000000, 1.000000000000000000, 1.000000000000000000, 1.000000000000000000, 1.000000000000000000, 1.000000000000000000, 1.000000000000000000, 1.000000000000000000, 1.000000000000000000, 1.000000000000000000, 1.000000000000000000, 1.000000000000000000, 1.000000000000000000, 1.000000000000000000, 1.000000000000000000, 1.000000000000000000, 1.000000000000000000, 1.000000000000000000, 1.000000000000000000, 1.000000000000000000, 1.000000000000000000, 1.000000000000000000, 1.000000000000000000, 1.000000000000000000, 1.000000000000000000, 1.000000000000000000, 1.000000000000000000, 1.000000000000000000, 1.000000000000000000, 1.000000000000000000, 1.000000000000000000, 1.000000000000000000, 1.000000000000000000, 1.000000000000000000, 1.000000000000000000, 1.000000000000000000, 1.000000000000000000, 1.000000000000000000, 1.000000000000000000, 1.000000000000000000, 1.000000000000000000, 1.000000000000000000, 1.000000000000000000, 1.000000000000000000, 1.000000000000000000, 1.000000000000000000, 1.000000000000000000, 1.000000000000000000, 1.000000000000000000, 1.000000000000000000, 1.000000000000000000, 1.000000000000000000, 1.000000000000000000, 1.000000000000000000, 1.000000000000000000, 1.000000000000000000, 1.000000000000000000, 1.000000000000000000, 1.000000000000000000, 1.000000000000000000, 1.000000000000000000, 1.000000000000000000, 1.000000000000000000, 1.000000000000000000, 1.000000000000000000, 1.000000000000000000, 1.000000000000000000, 1.000000000000000000, 1.000000000000000000, 1.000000000000000000, 1.000000000000000000, 1.000000000000000000, 1.000000000000000000, 1.000000000000000000, 1.000000000000000000, 1.000000000000000000, 1.000000000000000000, 1.000000000000000000, 1.000000000000000000, 1.000000000000000000, 1.000000000000000000, 1.000000000000000000, 1.000000000000000000, 1.000000000000000000, 1.000000000000000000, 1.000000000000000000, 1.000000000000000000, 1.000000000000000000, 1.000000000000000000, 1.000000000000000000, 1.000000000000000000, 1.000000000000000000, 1.000000000000000000, 1.000000000000000000, 1.000000000000000000, 1.000000000000000000, 1.000000000000000000, 1.000000000000000000, 1.000000000000000000, 1.000000000000000000, 1.000000000000000000, 1.000000000000000000, 1.000000000000000000, 1.000000000000000000, 1.000000000000000000, 1.000000000000000000),
 ( 1.857142857142858317, 1.857142857142858317, 1.857142857142858317, 1.857142857142858317, 1.857142857142858317, 1.857142857142858317, 1.857142857142858317, 1.857142857142858317, 1.857142857142858317, 1.857142857142858317, 1.857142857142858317, 1.857142857142858317, 1.857142857142858317, 1.857142857142858317, 1.857142857142858317, 1.857142857142858317, 1.857142857142858317, 1.857142857142858317, 1.857142857142858317, 1.857142857142858317, 1.857142857142858317, 1.857142857142858317, 1.857142857142858317, 1.857142857142858317, 1.857142857142858317, 1.857142857142858317, 1.857142857142858317, 1.857142857142858317, 1.857142857142858317, 1.857142857142858317, 1.857142857142858317, 1.857142857142858317, 1.857142857142858317, 1.857142857142858317, 1.857142857142858317, 1.857142857142858317, 1.857142857142858317, 1.857142857142858317, 1.857142857142858317, 1.857142857142858317, 1.857142857142858317, 1.857142857142858317, 1.857142857142858317, 1.857142857142858317, 1.857142857142858317, 1.857142857142858317, 1.857142857142858317, 1.857142857142858317, 1.857142857142858317, 1.857142857142858317, 1.857142857142858317, 1.857142857142858317, 1.857142857142858317, 1.857142857142858317, 1.857142857142858317, 1.857142857142858317, 1.857142857142858317, 1.857142857142858317, 1.857142857142858317, 1.857142857142858317, 1.857142857142858317, 1.857142857142858317, 1.857142857142858317, 1.857142857142858317, 1.857142857142858317, 1.857142857142858317, 1.857142857142858317, 1.857142857142858317, 1.857142857142858317, 1.857142857142858317, 1.857142857142858317, 1.857142857142858317, 1.857142857142858317, 1.857142857142858317, 1.857142857142858317, 1.857142857142858317, 1.857142857142858317, 1.857142857142858317, 1.857142857142858317, 1.857142857142858317, 1.857142857142858317, 1.857142857142858317, 1.857142857142858317, 1.857142857142858317, 1.857142857142858317, 1.857142857142858317, 1.857142857142858317, 1.857142857142858317, 1.857142857142858317, 1.857142857142858317, 1.857142857142858317, 1.857142857142858317, 1.857142857142858317, 1.857142857142858317, 1.857142857142858317, 1.857142857142858317, 1.857142857142859205, 1.857142857142859205, 1.857142857142857428, 1.857142857142857428, 1.857142857142855430, 1.857142857142855430, 1.857142857142858317, 1.857142857142858317, 1.857142857142858317, 1.857142857142858317, 1.857142857142858317, 1.857142857142858317, 1.857142857142858317, 1.857142857142858317, 1.857142857142858317, 1.857142857142858317, 1.857142857142858317, 1.857142857142858317, 1.857142857142858317, 1.857142857142858317, 1.857142857142860981, 1.857142857142860981, 1.857142857142858317, 1.857142857142858317, 1.857142857142858317, 1.857142857142858317, 1.857142857142858317, 1.857142857142858317, 1.857142857142858317, 1.857142857142858317, 1.857142857142858317, 1.857142857142858317, 1.857142857142858317, 1.857142857142858317, 1.857142857142858317, 1.857142857142858317, 1.857142857142858317, 1.857142857142858317, 1.857142857142858317, 1.857142857142858317),
 ( 1.000000000000000000, 1.000000000000000000, 1.000000000000000000, 1.000000000000000000, 1.000000000000000000, 1.000000000000000000, 1.000000000000000000, 1.000000000000000000, 1.000000000000000000, 1.000000000000000000, 1.000000000000000000, 1.000000000000000000, 1.000000000000000000, 1.000000000000000000, 1.000000000000000000, 1.000000000000000000, 1.000000000000000000, 1.000000000000000000, 1.000000000000000000, 1.000000000000000000, 1.000000000000000000, 1.000000000000000000, 1.000000000000000000, 1.000000000000000000, 1.000000000000000000, 1.000000000000000000, 1.000000000000000000, 1.000000000000000000, 1.000000000000000000, 1.000000000000000000, 1.000000000000000000, 1.000000000000000000, 1.000000000000000000, 1.000000000000000000, 1.000000000000000000, 1.000000000000000000, 1.000000000000000000, 1.000000000000000000, 1.000000000000000000, 1.000000000000000000, 1.000000000000000000, 1.000000000000000000, 1.000000000000000000, 1.000000000000000000, 1.000000000000000000, 1.000000000000000000, 1.000000000000000000, 1.000000000000000000, 1.000000000000000000, 1.000000000000000000, 1.000000000000000000, 1.000000000000000000, 1.000000000000000000, 1.000000000000000000, 1.000000000000000000, 1.000000000000000000, 1.000000000000000000, 1.000000000000000000, 1.000000000000000000, 1.000000000000000000, 1.000000000000000000, 1.000000000000000000, 1.000000000000000000, 1.000000000000000000, 1.000000000000000000, 1.000000000000000000, 1.000000000000000000, 1.000000000000000000, 1.000000000000000000, 1.000000000000000000, 1.000000000000000000, 1.000000000000000000, 1.000000000000000000, 1.000000000000000000, 1.000000000000000000, 1.000000000000000000, 1.000000000000000000, 1.000000000000000000, 1.000000000000000000, 1.000000000000000000, 1.000000000000000000, 1.000000000000000000, 1.000000000000000000, 1.000000000000000000, 1.000000000000000000, 1.000000000000000000, 1.000000000000000000, 1.000000000000000000, 1.000000000000000000, 1.000000000000000000, 1.000000000000000000, 1.000000000000000000, 1.000000000000000000, 1.000000000000000000, 1.000000000000000000, 1.000000000000000000, 1.000000000000000000, 1.000000000000000000, 1.000000000000000000, 1.000000000000000000, 1.000000000000000000, 1.000000000000000000, 1.000000000000000000, 1.000000000000000000, 1.000000000000000000, 1.000000000000000000, 1.000000000000000000, 1.000000000000000000, 1.000000000000000000, 1.000000000000000000, 1.000000000000000000, 1.000000000000000000, 1.000000000000000000, 1.000000000000000000, 1.000000000000000000, 1.000000000000000000, 1.000000000000000000, 1.000000000000000000, 1.000000000000000000, 1.000000000000000000, 1.000000000000000000, 1.000000000000000000, 1.000000000000000000, 1.000000000000000000, 1.000000000000000000, 1.000000000000000000, 1.000000000000000000, 1.000000000000000000, 1.000000000000000000, 1.000000000000000000, 1.000000000000000000, 1.000000000000000000, 1.000000000000000000, 1.000000000000000000, 1.000000000000000000, 1.000000000000000000) ) ) 
 REPRESENTATION_ITEM ( '' )  SURFACE ( )  );
#89441 = CARTESIAN_POINT ( 'NONE',  ( 85.78618341410623316, -28.50839767291424565, 180.2823363360693918 ) ) ;
#89442 = CYLINDRICAL_SURFACE ( 'NONE', #98058, 5.000000000000000888 ) ;
#89443 = AXIS2_PLACEMENT_3D ( 'NONE', #54534, #22758, #37359 ) ;
#89444 = ORIENTED_EDGE ( 'NONE', *, *, #10812, .F. ) ;
#89445 = CARTESIAN_POINT ( 'NONE',  ( 95.27829797562213798, -57.67182506141622866, 35.15692822873978685 ) ) ;
#89446 = CARTESIAN_POINT ( 'NONE',  ( 35.41405072744154836, 437.5080630478382204, 4.889382217447025170 ) ) ;
#89447 = DIRECTION ( 'NONE',  ( -0.000000000000000000, -1.000000000000000000, -0.000000000000000000 ) ) ;
#89448 = EDGE_CURVE ( 'NONE', #87331, #4789, #83562, .T. ) ;
#89449 = CARTESIAN_POINT ( 'NONE',  ( 29.27130674176784808, 18.74791880384170284, 39.67321021315746066 ) ) ;
#89450 = CARTESIAN_POINT ( 'NONE',  ( -8.922269033015549411, -5.000000000000000000, -5.219866590717671784 ) ) ;
#89451 = CARTESIAN_POINT ( 'NONE',  ( 0.000000000000000000, 8.660254037844390851, -0.9999999999999974465 ) ) ;
#89452 = EDGE_CURVE ( 'NONE', #101117, #81828, #68980, .T. ) ;
#89454 = CARTESIAN_POINT ( 'NONE',  ( -13.95941059228342951, 6.934767921800601975, 7.968035485162160647 ) ) ;
#89453 = DIRECTION ( 'NONE',  ( -0.000000000000000000, 1.000000000000000000, 0.000000000000000000 ) ) ;
#89455 = ORIENTED_EDGE ( 'NONE', *, *, #37286, .F. ) ;
#89456 = CARTESIAN_POINT ( 'NONE',  ( 42.29361012145520249, 486.6953289214418419, 8.720858923656924944 ) ) ;
#89457 = CARTESIAN_POINT ( 'NONE',  ( -12.50000000000000711, -4.999999999999999112, -55.73109925765189843 ) ) ;
#89458 = CARTESIAN_POINT ( 'NONE',  ( -27.26370785122089302, 36.83104668818905481, -7.556984339686001917 ) ) ;
#89459 = CARTESIAN_POINT ( 'NONE',  ( 9.999999999999998224, 15.23416508903533817, -0.7060372491625556135 ) ) ;
#89460 = STYLED_ITEM ( 'NONE', ( #13027 ), #40448 ) ;
#89461 = AXIS2_PLACEMENT_3D ( 'NONE', #21904, #87154, #55797 ) ;
#89462 = EDGE_CURVE ( 'NONE', #31692, #77337, #15225, .T. ) ;
#89463 = CARTESIAN_POINT ( 'NONE',  ( -102.0620737423919593, -38.00000000000000711, 183.9277168086509846 ) ) ;
#89464 = EDGE_LOOP ( 'NONE', ( #60117, #88637, #10711, #16116 ) ) ;
#89465 = CARTESIAN_POINT ( 'NONE',  ( -5.385673916453012744, -4.336808689942017736E-16, 15.34388420865771785 ) ) ;
#89466 = CARTESIAN_POINT ( 'NONE',  ( 0.3173508448886522837, 5.375634714784615298, -6.689127551062009402 ) ) ;
#89467 = CARTESIAN_POINT ( 'NONE',  ( -6.557141181177008171, -15.75010798306612081, -35.04602174276683257 ) ) ;
#89469 = CARTESIAN_POINT ( 'NONE',  ( -56.97006370568202982, -21.76999005371631313, -23.90107951094816485 ) ) ;
#89468 = CARTESIAN_POINT ( 'NONE',  ( -1.101454001170010244, 14.95253250404441836, -0.8386200322165883181 ) ) ;
#89470 = EDGE_CURVE ( 'NONE', #77294, #103513, #25924, .T. ) ;
#89471 = ORIENTED_EDGE ( 'NONE', *, *, #63735, .T. ) ;
#89472 = VECTOR ( 'NONE', #43988, 1000.000000000000000 ) ;
#89473 = ORIENTED_EDGE ( 'NONE', *, *, #39210, .T. ) ;
#89474 = CARTESIAN_POINT ( 'NONE',  ( 0.1061556211655338700, -4.836380039389421626, 4.623144047065555817 ) ) ;
#89475 = AXIS2_PLACEMENT_3D ( 'NONE', #42241, #66529, #99400 ) ;
#89476 = FACE_OUTER_BOUND ( 'NONE', #13242, .T. ) ;
#89477 = CARTESIAN_POINT ( 'NONE',  ( -92.65990761677430498, -60.00000000000002132, -3.893849931707503043 ) ) ;
#89478 = ORIENTED_EDGE ( 'NONE', *, *, #42810, .T. ) ;
#89479 = CARTESIAN_POINT ( 'NONE',  ( 4.699999999999999289, 6.499999999999999112, 0.000000000000000000 ) ) ;
#89480 = CARTESIAN_POINT ( 'NONE',  ( -9.981544566921638051, 15.23274035658503145, 0.7016502453916984017 ) ) ;
#89481 = CARTESIAN_POINT ( 'NONE',  ( 97.77191385463773088, -60.34768693918523041, 196.6186543819742383 ) ) ;
#89483 = CARTESIAN_POINT ( 'NONE',  ( -17.86532138382085932, 45.30096510830348677, 5.720552158557736355 ) ) ;
#89482 = CARTESIAN_POINT ( 'NONE',  ( 0.000000000000000000, 0.000000000000000000, 0.000000000000000000 ) ) ;
#89484 = AXIS2_PLACEMENT_3D ( 'NONE', #44956, #71325, #70805 ) ;
#89485 = CARTESIAN_POINT ( 'NONE',  ( -84.31906800682108383, -22.12972036364938333, 154.7647679128914433 ) ) ;
#89486 = ORIENTED_EDGE ( 'NONE', *, *, #2529, .T. ) ;
#89487 = VERTEX_POINT ( 'NONE', #19425 ) ;
#89488 = EDGE_LOOP ( 'NONE', ( #98536, #52174, #106319, #43449, #60974, #46724 ) ) ;
#89489 = DIRECTION ( 'NONE',  ( -0.000000000000000000, -1.000000000000000000, -0.000000000000000000 ) ) ;
#89490 = CARTESIAN_POINT ( 'NONE',  ( -6.031968554556153883, -14.91855978929569559, 14.31416968664639988 ) ) ;
#89491 = ORIENTED_EDGE ( 'NONE', *, *, #77026, .F. ) ;
#89492 = CARTESIAN_POINT ( 'NONE',  ( 47.33349330513379982, 1.593028355512270567E-15, 0.000000000000000000 ) ) ;
#89493 = CARTESIAN_POINT ( 'NONE',  ( -66.76860190796567451, 46.03420836107012093, -33.38430095398284436 ) ) ;
#89494 = CARTESIAN_POINT ( 'NONE',  ( -9.926810856659439963, 15.46725112412266512, -1.404490565848994343 ) ) ;
#89495 = CARTESIAN_POINT ( 'NONE',  ( -103.1324900820093262, -57.63586870064128931, 202.7914362107620434 ) ) ;
#89496 = CARTESIAN_POINT ( 'NONE',  ( -9.789044728060147804, 294.6486233851416614, -2.043184600577789833 ) ) ;
#89497 = VECTOR ( 'NONE', #34010, 1000.000000000000000 ) ;
#89498 = CARTESIAN_POINT ( 'NONE',  ( 83.86866073052654258, 1.030564683017419500E-14, 0.000000000000000000 ) ) ;
#89499 = CARTESIAN_POINT ( 'NONE',  ( -1.219798531186343959, 25.50106792483703089, 39.81686016623014979 ) ) ;
#89500 = CARTESIAN_POINT ( 'NONE',  ( 1.249971410579568287, 27.80243479384745342, -39.34029123867090050 ) ) ;
#89501 = CARTESIAN_POINT ( 'NONE',  ( -34.13564290404001156, -60.00000000000002132, -42.84076297484070039 ) ) ;
#89502 = CARTESIAN_POINT ( 'NONE',  ( 0.000000000000000000, 0.000000000000000000, -13.00000000000000000 ) ) ;
#89503 = CARTESIAN_POINT ( 'NONE',  ( -52.60481344042765528, -60.31495398866518087, 63.32391407137016870 ) ) ;
#89504 = CIRCLE ( 'NONE', #75715, 4.000000000000001776 ) ;
#89505 = DIRECTION ( 'NONE',  ( -1.000000000000000000, -0.000000000000000000, -0.000000000000000000 ) ) ;
#89506 = ORIENTED_EDGE ( 'NONE', *, *, #31258, .F. ) ;
#89507 = CARTESIAN_POINT ( 'NONE',  ( -99.46713752920656759, -52.77532478499336577, 194.5109139038963235 ) ) ;
#89508 = CARTESIAN_POINT ( 'NONE',  ( -1.487796992739244706, 297.5563421048641999, -10.00151720974388603 ) ) ;
#89509 = AXIS2_PLACEMENT_3D ( 'NONE', #19355, #27437, #43049 ) ;
#89510 = ORIENTED_EDGE ( 'NONE', *, *, #44294, .F. ) ;
#89511 = CARTESIAN_POINT ( 'NONE',  ( -16.91747028431907296, 34.95463172523481177, -21.80698433968594685 ) ) ;
#89512 = CARTESIAN_POINT ( 'NONE',  ( 98.76629783378818672, -38.35591045133333665, 81.67967853887255103 ) ) ;
#89513 = DIRECTION ( 'NONE',  ( 0.5735764363510470476, -0.8191520442889911324, 1.003171929053524007E-16 ) ) ;
#89514 = CARTESIAN_POINT ( 'NONE',  ( 6.815830331203684977, 1.210606185736183200E-13, -6.171384342982610072 ) ) ;
#89515 = FILL_AREA_STYLE ('',( #55518 ) ) ;
#89516 = CARTESIAN_POINT ( 'NONE',  ( 0.5805565836007664515, -7.505553499465142053, -1.357586595304856736E-16 ) ) ;
#89518 = CARTESIAN_POINT ( 'NONE',  ( 85.25533141069878695, -30.00000000000000355, 172.6891169115829996 ) ) ;
#89517 = UNCERTAINTY_MEASURE_WITH_UNIT (LENGTH_MEASURE( 1.000000000000000082E-05 ), #714, 'distance_accuracy_value', 'NONE');
#89519 = CARTESIAN_POINT ( 'NONE',  ( 35.62683129835268403, 491.6879615318113110, 12.48649695628193257 ) ) ;
#89520 = CARTESIAN_POINT ( 'NONE',  ( -28.43338544108043919, 12.59781646960431623, 40.78060993930063205 ) ) ;
#89521 = EDGE_CURVE ( 'NONE', #98765, #99690, #29071, .T. ) ;
#89522 = DIRECTION ( 'NONE',  ( 0.000000000000000000, -1.000000000000000000, 0.000000000000000000 ) ) ;
#89523 = EDGE_CURVE ( 'NONE', #28165, #77405, #94780, .T. ) ;
#89524 = ORIENTED_EDGE ( 'NONE', *, *, #7549, .F. ) ;
#89525 = VERTEX_POINT ( 'NONE', #87302 ) ;
#89526 = CARTESIAN_POINT ( 'NONE',  ( 50.43109628883428286, -53.36716467480742665, 56.24163232349562946 ) ) ;
#89527 = CARTESIAN_POINT ( 'NONE',  ( 5.668940197363838251, 41.88723871811491506, -59.02759513106027356 ) ) ;
#89528 = CONICAL_SURFACE ( 'NONE', #44736, 3.309500000000001663, 0.9599310885968770357 ) ;
#89529 = MANIFOLD_SOLID_BREP ( 'IDChamferFar', #58397 ) ;
#89530 = CARTESIAN_POINT ( 'NONE',  ( 9.635740931621784355, 51.40895863168635316, 2.124525052985154261 ) ) ;
#89531 = EDGE_CURVE ( 'NONE', #93228, #87882, #58516, .T. ) ;
#89532 = ORIENTED_EDGE ( 'NONE', *, *, #77919, .F. ) ;
#89533 = CARTESIAN_POINT ( 'NONE',  ( -91.98980923544721122, -38.35482474950386944, 34.70844003865646954 ) ) ;
#89534 = ORIENTED_EDGE ( 'NONE', *, *, #34188, .F. ) ;
#89535 = CARTESIAN_POINT ( 'NONE',  ( 28.21386086657646075, 34.30365941694820719, -8.223977910641220745 ) ) ;
#89536 = CARTESIAN_POINT ( 'NONE',  ( 92.03920658769411034, -38.35407107957195905, 35.11563712653246228 ) ) ;
#89537 = CARTESIAN_POINT ( 'NONE',  ( 10.52016239807662856, 10.30073425343680782, -10.32006978720601786 ) ) ;
#89538 = CARTESIAN_POINT ( 'NONE',  ( 101.1120282019177239, -52.71709064890642082, 130.0501827644169452 ) ) ;
#89539 = SURFACE_STYLE_FILL_AREA ( #31332 ) ;
#89540 = CARTESIAN_POINT ( 'NONE',  ( -32.11029369521102694, 318.6955982813968262, -5.641370532960698014 ) ) ;
#89541 = CARTESIAN_POINT ( 'NONE',  ( 80.42679257503434087, -59.99999999999999289, 196.4953341280405539 ) ) ;
#89542 = EDGE_CURVE ( 'NONE', #53479, #78094, #101263, .T. ) ;
#89543 = CARTESIAN_POINT ( 'NONE',  ( 61.85555555555556140, 6.915964383211875250E-15, 0.000000000000000000 ) ) ;
#89544 = ORIENTED_EDGE ( 'NONE', *, *, #22127, .T. ) ;
#89545 = CARTESIAN_POINT ( 'NONE',  ( 56.34713570575822672, -25.61535964347525152, 57.53183839505768304 ) ) ;
#89546 = SURFACE_STYLE_FILL_AREA ( #17791 ) ;
#89547 = CARTESIAN_POINT ( 'NONE',  ( 9.301012663197237629, -52.69978924280226096, 23.32537848786287782 ) ) ;
#89548 = VECTOR ( 'NONE', #61398, 1000.000000000000000 ) ;
#89549 = ORIENTED_EDGE ( 'NONE', *, *, #87990, .F. ) ;
#89551 = CARTESIAN_POINT ( 'NONE',  ( -14.47578207976464526, 21.82911064463434059, 4.800479567661631641 ) ) ;
#89550 = CARTESIAN_POINT ( 'NONE',  ( -88.28902640317532757, -38.37280356866271092, -19.18740266668778460 ) ) ;
#89552 = CARTESIAN_POINT ( 'NONE',  ( -42.69811214730272297, 434.9611672192513652, 18.34625614733208820 ) ) ;
#89553 = CARTESIAN_POINT ( 'NONE',  ( 0.000000000000000000, -46.00000000000000000, 112.0000000000000000 ) ) ;
#89554 = CARTESIAN_POINT ( 'NONE',  ( 0.000000000000000000, 43.19193163660326462, 0.000000000000000000 ) ) ;
#89555 = CARTESIAN_POINT ( 'NONE',  ( -3.313708498984760720, -33.03125000000000000, -8.000000000000000000 ) ) ;
#89556 =( NAMED_UNIT ( * ) PLANE_ANGLE_UNIT ( ) SI_UNIT ( $, .RADIAN. ) );
#89557 = COLOUR_RGB ( '', 0.09019608, 0.27058824, 0.51372549) ;
#89558 = CARTESIAN_POINT ( 'NONE',  ( -37.56673239365863282, -1.200000000000000030E-05, -13.45617127781024891 ) ) ;
#89559 = ORIENTED_EDGE ( 'NONE', *, *, #93477, .T. ) ;
#89560 = CARTESIAN_POINT ( 'NONE',  ( 85.20513743252166705, -25.43210005301644472, 169.0098029066481331 ) ) ;
#89561 = CARTESIAN_POINT ( 'NONE',  ( 67.22793774957824553, 6.975173280561618775E-15, 0.000000000000000000 ) ) ;
#89562 = CARTESIAN_POINT ( 'NONE',  ( -35.77486673446257726, 439.5646605908588072, 23.98731056691347874 ) ) ;
#89563 = ORIENTED_EDGE ( 'NONE', *, *, #12795, .F. ) ;
#89564 = DIRECTION ( 'NONE',  ( 0.000000000000000000, 1.000000000000000000, 0.000000000000000000 ) ) ;
#89565 = CARTESIAN_POINT ( 'NONE',  ( 6.016266904915582359, -5.000000000005062617, -16.21640811047284814 ) ) ;
#89566 = DIRECTION ( 'NONE',  ( -1.000000000000000000, -1.224606353822377258E-16, -0.000000000000000000 ) ) ;
#89567 = CARTESIAN_POINT ( 'NONE',  ( -16.64348903516517098, -1.200000000000000030E-05, 4.157797401561652784 ) ) ;
#89568 = CARTESIAN_POINT ( 'NONE',  ( 0.000000000000000000, 0.000000000000000000, -8.900000000000000355 ) ) ;
#89569 = CARTESIAN_POINT ( 'NONE',  ( -28.43345358724999983, 12.59863739772598024, -40.78014218160733861 ) ) ;
#89570 =( BOUNDED_SURFACE ( )  B_SPLINE_SURFACE ( 3, 2, ( 
 ( #13828, #53252, #46740 ),
 ( #79630, #12240, #5747 ),
 ( #78568, #62411, #13292 ),
 ( #85626, #30053, #95305 ) ),
 .UNSPECIFIED., .F., .F., .F. ) 
 B_SPLINE_SURFACE_WITH_KNOTS ( ( 4, 4 ),
 ( 3, 3 ),
 ( 0.01539444365212560770, 0.01716277291647040973 ),
 ( 0.1628431039857609064, 1.000000000000000000 ),
 .UNSPECIFIED. ) 
 GEOMETRIC_REPRESENTATION_ITEM ( )  RATIONAL_B_SPLINE_SURFACE ( (
 ( 0.9201425306416459726, 0.7548024220745122026, 1.000000000000000000),
 ( 0.9252298807393682933, 0.7704228259270666790, 1.000000000000000000),
 ( 0.9301471562783281133, 0.7855210260307374792, 1.000000000000000000),
 ( 0.9349020401063605767, 0.8001206121097657054, 1.000000000000000000) ) ) 
 REPRESENTATION_ITEM ( '' )  SURFACE ( )  );
#89571 = CIRCLE ( 'NONE', #63719, 2.000000000000000000 ) ;
#89572 = VERTEX_POINT ( 'NONE', #54907 ) ;
#89573 = ADVANCED_FACE ( 'NONE', ( #62497 ), #30142, .F. ) ;
#89574 = FILL_AREA_STYLE_COLOUR ( '', #102293 ) ;
#89575 = AXIS2_PLACEMENT_3D ( 'NONE', #21814, #72451, #54654 ) ;
#89576 = CARTESIAN_POINT ( 'NONE',  ( 7.551892080562057075, 108.0098770253938341, 2.647003822403973583 ) ) ;
#89577 = CARTESIAN_POINT ( 'NONE',  ( 0.8397591720178106955, 25.95816433063382789, 38.57052554651150444 ) ) ;
#89578 = EDGE_CURVE ( 'NONE', #33604, #1839, #70046, .T. ) ;
#89579 = EDGE_CURVE ( 'NONE', #69179, #49340, #78648, .T. ) ;
#89581 = CARTESIAN_POINT ( 'NONE',  ( -10.13027397392433926, 12.28049385479850741, -10.56248067576192362 ) ) ;
#89580 = CARTESIAN_POINT ( 'NONE',  ( -22.57777066253796505, -27.40074420488135942, 37.49751158013248897 ) ) ;
#89582 = VECTOR ( 'NONE', #20335, 1000.000000000000000 ) ;
#89583 = CARTESIAN_POINT ( 'NONE',  ( 5.082755093536324154, -13.34375000204838457, 5.082755093536326818 ) ) ;
#89584 = CARTESIAN_POINT ( 'NONE',  ( -28.72970484482200604, 18.79180695567417203, -40.04448862869271153 ) ) ;
#89585 = PRESENTATION_LAYER_ASSIGNMENT (  '', '', ( #96454 ) ) ;
#89586 = ORIENTED_EDGE ( 'NONE', *, *, #17145, .F. ) ;
#89587 = CARTESIAN_POINT ( 'NONE',  ( -17.50000000000007461, 50.00318699355199925, 59.98279283212356461 ) ) ;
#89588 = DIRECTION ( 'NONE',  ( -0.000000000000000000, -0.000000000000000000, -1.000000000000000000 ) ) ;
#89589 = CARTESIAN_POINT ( 'NONE',  ( -4.313686681661103250, 141.0184800401511325, -5.000000000000000888 ) ) ;
#89590 = CARTESIAN_POINT ( 'NONE',  ( -8.641101172624390259, -5.000000000000001776, -72.37542516940096959 ) ) ;
#89591 = FACE_OUTER_BOUND ( 'NONE', #3010, .T. ) ;
#89592 = EDGE_CURVE ( 'NONE', #63934, #70305, #25587, .T. ) ;
#89593 = ORIENTED_EDGE ( 'NONE', *, *, #29950, .F. ) ;
#89594 = CARTESIAN_POINT ( 'NONE',  ( 11.42048730496502706, 13.43064252417310556, -10.00000000000007994 ) ) ;
#89595 = CARTESIAN_POINT ( 'NONE',  ( 73.59428447264397732, -4.000000000000000000, 0.000000000000000000 ) ) ;
#89596 = ORIENTED_EDGE ( 'NONE', *, *, #5015, .F. ) ;
#89597 = CIRCLE ( 'NONE', #37986, 1.000000000000001332 ) ;
#89598 = EDGE_CURVE ( 'NONE', #85984, #89196, #21424, .T. ) ;
#89599 = FILL_AREA_STYLE ('',( #56676 ) ) ;
#89600 = DIRECTION ( 'NONE',  ( 0.000000000000000000, 0.000000000000000000, 1.000000000000000000 ) ) ;
#89601 = CARTESIAN_POINT ( 'NONE',  ( 4.651477914329386962E-14, 52.17923068443710832, 7.749999999999496403 ) ) ;
#89602 = CARTESIAN_POINT ( 'NONE',  ( -112.2163655317416868, -59.99999999999998579, 171.0452993802184096 ) ) ;
#89603 = CARTESIAN_POINT ( 'NONE',  ( 29.27137781856704990, 18.74786498819648983, -39.67318581983496983 ) ) ;
#89604 = CARTESIAN_POINT ( 'NONE',  ( -17.35892867067943257, 294.5707697310705839, -10.05973541782409342 ) ) ;
#89605 = FACE_OUTER_BOUND ( 'NONE', #26195, .T. ) ;
#89606 = CARTESIAN_POINT ( 'NONE',  ( -14.91858118607497019, 1.255821567010171884E-17, 15.00000000000000000 ) ) ;
#89607 = EDGE_CURVE ( 'NONE', #12516, #97744, #4703, .T. ) ;
#89609 = CARTESIAN_POINT ( 'NONE',  ( 29.99999999999482014, 487.5694517063741955, 6.760539803216031984 ) ) ;
#89608 = CARTESIAN_POINT ( 'NONE',  ( 1.570796324976846403, -5.000000000000002665, -97.00000000000000000 ) ) ;
#89610 = CARTESIAN_POINT ( 'NONE',  ( -81.66238495618624427, -57.04855356713849091, 183.2407446992486086 ) ) ;
#89611 = VERTEX_POINT ( 'NONE', #40857 ) ;
#89612 = FACE_OUTER_BOUND ( 'NONE', #27142, .T. ) ;
#89613 = EDGE_LOOP ( 'NONE', ( #91465, #88448, #64485, #57744, #79824, #100547 ) ) ;
#89614 = ORIENTED_EDGE ( 'NONE', *, *, #32747, .T. ) ;
#89615 = DIRECTION ( 'NONE',  ( 0.000000000000000000, 0.000000000000000000, 1.000000000000000000 ) ) ;
#89616 =( NAMED_UNIT ( * ) SI_UNIT ( $, .STERADIAN. ) SOLID_ANGLE_UNIT ( ) );
#89617 = CIRCLE ( 'NONE', #67302, 5.000000000000010658 ) ;
#89618 = CARTESIAN_POINT ( 'NONE',  ( -6.657117369358112491, 304.7445948672375948, 8.914202651909654662 ) ) ;
#89619 = CARTESIAN_POINT ( 'NONE',  ( -15.64030048137867190, 6.456385560667921020, -7.561819230143237647 ) ) ;
#89620 = CARTESIAN_POINT ( 'NONE',  ( 8.020869781902053575, 47.74450561243712343, -5.000000000000000888 ) ) ;
#89621 = CARTESIAN_POINT ( 'NONE',  ( 1.191759989000068964, -5.000000000000000000, -98.00009052017544775 ) ) ;
#89622 = CARTESIAN_POINT ( 'NONE',  ( -43.46689911038857446, 485.4921130118004271, 4.095024577345737882 ) ) ;
#89623 = CARTESIAN_POINT ( 'NONE',  ( 114.4521715241705664, -60.00000000000002842, 166.3966616003652348 ) ) ;
#89624 = CARTESIAN_POINT ( 'NONE',  ( -108.8241353627135055, -30.00000000000001421, 157.0475095860343515 ) ) ;
#89625 = CARTESIAN_POINT ( 'NONE',  ( -62.49919243722554540, -18.63627675925726734, 68.78216434012247760 ) ) ;
#89626 = ORIENTED_EDGE ( 'NONE', *, *, #53764, .T. ) ;
#89627 = CARTESIAN_POINT ( 'NONE',  ( -43.65875038008589115, 484.6130917689293369, 3.255992392461536600 ) ) ;
#89628 = CARTESIAN_POINT ( 'NONE',  ( 112.7800843278198073, -59.99999999999997158, 146.3612206852396014 ) ) ;
#89629 = EDGE_LOOP ( 'NONE', ( #40825, #12562, #61382, #17495, #22115 ) ) ;
#89630 = CARTESIAN_POINT ( 'NONE',  ( 2.033923692053578591, -49.91572940536237013, 32.20638245996861571 ) ) ;
#89631 = CARTESIAN_POINT ( 'NONE',  ( -5.082755093536326818, -12.59375000204838635, 5.082755093536325042 ) ) ;
#89632 = DIRECTION ( 'NONE',  ( 0.000000000000000000, 0.000000000000000000, 1.000000000000000000 ) ) ;
#89633 = ORIENTED_EDGE ( 'NONE', *, *, #61176, .T. ) ;
#89634 = CARTESIAN_POINT ( 'NONE',  ( 37.54559764570182523, 464.1143081516207189, 19.43664670202678835 ) ) ;
#89635 = ORIENTED_EDGE ( 'NONE', *, *, #79577, .F. ) ;
#89636 = CARTESIAN_POINT ( 'NONE',  ( 10.11650669486618881, -3.999999999999998224, 0.000000000000000000 ) ) ;
#89637 = CARTESIAN_POINT ( 'NONE',  ( 7.188101187500000044, -28.53125000204838813, 0.000000000000000000 ) ) ;
#89638 = CARTESIAN_POINT ( 'NONE',  ( -91.91408097602798932, -60.00000000000000000, 202.3452444908770929 ) ) ;
#89639 = SURFACE_STYLE_FILL_AREA ( #24406 ) ;
#89640 = CARTESIAN_POINT ( 'NONE',  ( 7.188101187499999156, -27.12500000204838457, 2.977408999572654924 ) ) ;
#89641 = AXIS2_PLACEMENT_3D ( 'NONE', #62890, #46687, #62365 ) ;
#89642 = CARTESIAN_POINT ( 'NONE',  ( 33.11369981515476013, 485.0096198691156815, 0.6282636062398145871 ) ) ;
#89643 = CARTESIAN_POINT ( 'NONE',  ( -11.44242801400452159, 13.21397695474668943, 10.00000000000005507 ) ) ;
#89644 = CARTESIAN_POINT ( 'NONE',  ( -10.86775040529106562, -4.994308969803370246, -12.56807544649716135 ) ) ;
#89645 = VECTOR ( 'NONE', #6078, 1000.000000000000000 ) ;
#89646 = CARTESIAN_POINT ( 'NONE',  ( -43.66595852442649317, 384.2000512634306233, 15.34658628582926454 ) ) ;
#89647 = ADVANCED_FACE ( 'NONE', ( #31216 ), #30821, .T. ) ;
#89648 = CARTESIAN_POINT ( 'NONE',  ( 86.71109173531407066, -60.00000000000004974, -11.42213278536460486 ) ) ;
#89649 = CARTESIAN_POINT ( 'NONE',  ( -31.31696575628595269, -22.13776733473083169, 30.43610477315223406 ) ) ;
#89650 = AXIS2_PLACEMENT_3D ( 'NONE', #81329, #72716, #23674 ) ;
#89651 = ADVANCED_FACE ( 'NONE', ( #48930 ), #16050, .T. ) ;
#89652 = CARTESIAN_POINT ( 'NONE',  ( -1.238932115526321320, -50.00000000000000000, 101.3452916561192296 ) ) ;
#89653 = CARTESIAN_POINT ( 'NONE',  ( 39.81835848735108385, -53.34354282573661976, 41.56692554013707763 ) ) ;
#89654 = CARTESIAN_POINT ( 'NONE',  ( 16.75187969033571989, -1.200000000000000030E-05, 23.05698433968582961 ) ) ;
#89655 = ORIENTED_EDGE ( 'NONE', *, *, #25097, .F. ) ;
#89656 = EDGE_CURVE ( 'NONE', #8869, #54015, #15298, .T. ) ;
#89657 = CARTESIAN_POINT ( 'NONE',  ( -7.414346147791998298, 87.64589157662267382, -3.010818766110534561 ) ) ;
#89658 = EDGE_CURVE ( 'NONE', #90326, #45699, #27949, .T. ) ;
#89659 = CIRCLE ( 'NONE', #12111, 12.00000000000003908 ) ;
#89660 = CARTESIAN_POINT ( 'NONE',  ( -59.09117307917458106, -38.34357130299601835, 93.55555875830225432 ) ) ;
#89661 = ORIENTED_EDGE ( 'NONE', *, *, #14782, .F. ) ;
#89663 = CARTESIAN_POINT ( 'NONE',  ( 45.17824257314219949, 354.4244853104167987, 3.762393652172960845 ) ) ;
#89662 = CARTESIAN_POINT ( 'NONE',  ( -4.000000000000000000, 0.000000000000000000, -0.02540000000000007530 ) ) ;
#89664 = CARTESIAN_POINT ( 'NONE',  ( 0.000000000000000000, 0.000000000000000000, -1.175078176076019387 ) ) ;
#89665 = FACE_OUTER_BOUND ( 'NONE', #78635, .T. ) ;
#89666 = DIRECTION ( 'NONE',  ( 0.000000000000000000, 1.000000000000000000, -0.000000000000000000 ) ) ;
#89667 = CARTESIAN_POINT ( 'NONE',  ( -38.75664172650044748, 25.16721717615375908, 12.59822445845297700 ) ) ;
#89668 = CARTESIAN_POINT ( 'NONE',  ( 4.905018583967755141, -87.02359985679682097, -3.459768807258293055 ) ) ;
#89669 = CARTESIAN_POINT ( 'NONE',  ( 29.83349330513380337, 1.593028355512270567E-15, 0.000000000000000000 ) ) ;
#89670 = ADVANCED_FACE ( 'NONE', ( #89944 ), #73801, .T. ) ;
#89671 = AXIS2_PLACEMENT_3D ( 'NONE', #83919, #60734, #12151 ) ;
#89672 = CARTESIAN_POINT ( 'NONE',  ( 100.7785506732187883, -59.99999999999999289, 85.60081394660342369 ) ) ;
#89673 = CARTESIAN_POINT ( 'NONE',  ( -4.874120320015572716, -52.04554131839427811, 40.12882148314245256 ) ) ;
#89674 = ADVANCED_FACE ( 'NONE', ( #55953 ), #3222, .F. ) ;
#89675 = CARTESIAN_POINT ( 'NONE',  ( -48.02835407290534420, 16.78162100668604495, -14.35535821593460248 ) ) ;
#89676 = CARTESIAN_POINT ( 'NONE',  ( -16.14595037822616419, 12.99999999999999289, 0.000000000000000000 ) ) ;
#89677 = ORIENTED_EDGE ( 'NONE', *, *, #59971, .T. ) ;
#89678 = CARTESIAN_POINT ( 'NONE',  ( -99.67836086284214048, -30.00000000000002132, 186.8797784846947252 ) ) ;
#89679 = ORIENTED_EDGE ( 'NONE', *, *, #99818, .T. ) ;
#89680 = CARTESIAN_POINT ( 'NONE',  ( 42.61650669486618881, -3.851859888774471706E-31, 4.000000000000000888 ) ) ;
#89681 = CARTESIAN_POINT ( 'NONE',  ( -16.01290064681822045, 3.743845801208044222, -0.6463026410129599775 ) ) ;
#89682 = CARTESIAN_POINT ( 'NONE',  ( 8.986743721226838844, 15.43298062744137056, -6.150437581724646990E-13 ) ) ;
#89683 = CARTESIAN_POINT ( 'NONE',  ( 0.000000000000000000, 115.0000000000000000, -10.00000000000000000 ) ) ;
#89684 = CARTESIAN_POINT ( 'NONE',  ( -22.65274949039500285, 28.20149500596347281, -30.83785112677304951 ) ) ;
#89685 = CARTESIAN_POINT ( 'NONE',  ( 5.082755093536324154, -27.21875000204838813, 5.082755093536326818 ) ) ;
#89686 = CIRCLE ( 'NONE', #103456, 4.000000000000000000 ) ;
#89687 = FILL_AREA_STYLE_COLOUR ( '', #29548 ) ;
#89688 = CARTESIAN_POINT ( 'NONE',  ( 7.044112035629908064, 41.04202961785853887, -70.72791777926931900 ) ) ;
#89689 = VERTEX_POINT ( 'NONE', #48408 ) ;
#89691 = EDGE_LOOP ( 'NONE', ( #40297, #77166, #77590 ) ) ;
#89690 = CARTESIAN_POINT ( 'NONE',  ( 27.33349330513380693, -4.000000000000000000, 4.898587196589415787E-16 ) ) ;
#89692 = CARTESIAN_POINT ( 'NONE',  ( 83.58678869323294691, -18.68415770015456090, 145.1632175728272784 ) ) ;
#89693 = CARTESIAN_POINT ( 'NONE',  ( -5.500000000000316192, 41.99999999999999289, -59.88032989331280476 ) ) ;
#89694 = FACE_OUTER_BOUND ( 'NONE', #46745, .T. ) ;
#89695 = ORIENTED_EDGE ( 'NONE', *, *, #29602, .F. ) ;
#89696 = CARTESIAN_POINT ( 'NONE',  ( -61.31073388236533361, 50.00000000000000711, 14.70371094580587723 ) ) ;
#89697 = CARTESIAN_POINT ( 'NONE',  ( -14.24890542152424544, 2.189729425908971017, 4.659254830001311021 ) ) ;
#89698 = CARTESIAN_POINT ( 'NONE',  ( -2.977408999572650039, -12.68750000204838280, -7.188101187500000933 ) ) ;
#89699 = CARTESIAN_POINT ( 'NONE',  ( 7.412906595240166929, 27.35811727147745387, 3.014362223629234894 ) ) ;
#89700 = CARTESIAN_POINT ( 'NONE',  ( -69.72050231116651275, -57.68271840123205862, 152.1212729744891590 ) ) ;
#89701 = CARTESIAN_POINT ( 'NONE',  ( -31.53898857890735030, 437.3650977026285886, 21.86279335866149509 ) ) ;
#89702 = ADVANCED_BREP_SHAPE_REPRESENTATION ( '', ( #16251, #10728 ), #105516 ) ;
#89703 = ORIENTED_EDGE ( 'NONE', *, *, #61379, .F. ) ;
#89704 = VECTOR ( 'NONE', #103970, 1000.000000000000227 ) ;
#89705 = B_SPLINE_CURVE_WITH_KNOTS ( 'NONE', 3,
 ( #21722, #6021, #20691, #63756, #54032, #104188, #70246, #37386, #94540, #13581, #4984, #78854, #79389, #95067, #103669, #103148, #38432, #104725, #88028, #14107, #55617, #5507, #21202, #14633, #86975, #87500, #47542, #13046, #30878, #47013, #38946, #45976, #80440, #71823, #37912, #29816 ),
 .UNSPECIFIED., .F., .F.,
 ( 4, 2, 2, 2, 2, 2, 2, 2, 2, 2, 2, 2, 2, 2, 2, 2, 2, 4 ),
 ( 0.01291936762762759677, 0.01372441420841340708, 0.01452946078919921911, 0.01533450736998502942, 0.01613955395077084146, 0.01694460053155665349, 0.01774964711234246206, 0.01855469369312827410, 0.01935974027391408614, 0.02016478685469989818, 0.02096983343548571022, 0.02177488001627151878, 0.02257992659705733082, 0.02338497317784313939, 0.02419001975862895143, 0.02459254304902185745, 0.02499506633941476347, 0.02580011292020053387 ),
 .UNSPECIFIED. ) ;
#89706 = PLANE ( 'NONE',  #14769 ) ;
#89707 = MANIFOLD_SOLID_BREP ( 'Fillet5', #72181 ) ;
#89708 = CARTESIAN_POINT ( 'NONE',  ( 7.495923973900548098, 40.46140423765491079, -59.65192238623429688 ) ) ;
#89709 = EDGE_CURVE ( 'NONE', #62772, #81897, #23967, .T. ) ;
#89710 = CARTESIAN_POINT ( 'NONE',  ( 0.8402286030463997912, 34.96037729579965969, -27.57089172558451295 ) ) ;
#89711 = EDGE_LOOP ( 'NONE', ( #44000, #71671, #68335, #37976 ) ) ;
#89712 = CARTESIAN_POINT ( 'NONE',  ( 5.082755093536325930, -29.46875000204838813, -5.082755093536325042 ) ) ;
#89713 = CARTESIAN_POINT ( 'NONE',  ( -33.70810140226702600, -23.45504108715438107, 33.05596252965560211 ) ) ;
#89714 = CARTESIAN_POINT ( 'NONE',  ( -38.97368692663644651, 491.1629893710622241, 12.12582181740389053 ) ) ;
#89715 = CARTESIAN_POINT ( 'NONE',  ( 0.6421110334426624044, 51.32541146260925302, -10.07566082288705367 ) ) ;
#89716 = CARTESIAN_POINT ( 'NONE',  ( -9.699016383038308931, 88.17638171448342632, 2.444973590251037443 ) ) ;
#89717 = CARTESIAN_POINT ( 'NONE',  ( 33.12944332324993013, 439.4248878830265994, 23.85028906779293933 ) ) ;
#89718 = SHAPE_DEFINITION_REPRESENTATION ( #5361, #52881 ) ;
#89719 = CARTESIAN_POINT ( 'NONE',  ( 49.03380706566427705, 8.971284072415114608, 14.85953237006425276 ) ) ;
#89720 = EDGE_LOOP ( 'NONE', ( #41664, #57419, #58085, #10506 ) ) ;
#89721 = CARTESIAN_POINT ( 'NONE',  ( 10.69660278669753417, 43.19295133451930724, 15.34151949443403140 ) ) ;
#89722 = AXIS2_PLACEMENT_3D ( 'NONE', #89553, #31863, #15649 ) ;
#89723 = PRESENTATION_STYLE_ASSIGNMENT (( #6664 ) ) ;
#89724 = CARTESIAN_POINT ( 'NONE',  ( 13.65239908362034171, 42.97563514209416979, -91.73105433446922063 ) ) ;
#89725 = AXIS2_PLACEMENT_3D ( 'NONE', #45645, #27377, #52121 ) ;
#89726 = DIRECTION ( 'NONE',  ( -0.5735764363510512664, 0.8191520442889881348, 1.003171929053520309E-16 ) ) ;
#89727 = DIRECTION ( 'NONE',  ( 0.000000000000000000, -1.000000000000000000, 0.000000000000000000 ) ) ;
#89728 = CARTESIAN_POINT ( 'NONE',  ( 14.75116205807806402, 43.55504283729542436, -90.22050498408901831 ) ) ;
#89729 = ORIENTED_EDGE ( 'NONE', *, *, #90120, .T. ) ;
#89730 = VECTOR ( 'NONE', #89453, 1000.000000000000000 ) ;
#89731 = DIRECTION ( 'NONE',  ( -0.5735764363510494901, -0.8191520442889894671, 0.000000000000000000 ) ) ;
#89732 = CARTESIAN_POINT ( 'NONE',  ( 106.6191002599640143, -57.65239554408994138, 200.4187991428152600 ) ) ;
#89733 = AXIS2_PLACEMENT_3D ( 'NONE', #77735, #70167, #29226 ) ;
#89734 = ADVANCED_FACE ( 'NONE', ( #41392 ), #6673, .F. ) ;
#89736 = CARTESIAN_POINT ( 'NONE',  ( 37.54559764570471003, 464.1143081516196389, 19.43664670202597833 ) ) ;
#89735 = VECTOR ( 'NONE', #4797, 1000.000000000000000 ) ;
#89737 = DIRECTION ( 'NONE',  ( -1.000000000000000000, -1.224606353822377258E-16, -0.000000000000000000 ) ) ;
#89738 = CARTESIAN_POINT ( 'NONE',  ( 7.347880794884118356E-15, 47.00000000000000000, -60.00000000000000000 ) ) ;
#89739 = CARTESIAN_POINT ( 'NONE',  ( -74.01186676100478223, -60.00000000000000000, 172.3432513155285619 ) ) ;
#89740 = CARTESIAN_POINT ( 'NONE',  ( -29.07128654445882887, 296.9339959557834163, -9.548856946221640385 ) ) ;
#89741 = EDGE_CURVE ( 'NONE', #26814, #67329, #33327, .T. ) ;
#89742 = CARTESIAN_POINT ( 'NONE',  ( -45.48126212248870814, 413.7349014071057240, 8.309231847991947362 ) ) ;
#89743 = CARTESIAN_POINT ( 'NONE',  ( -85.91487385093410012, -32.00067969521617783, 183.3906813362126798 ) ) ;
#89744 = ORIENTED_EDGE ( 'NONE', *, *, #73268, .F. ) ;
#89745 = CARTESIAN_POINT ( 'NONE',  ( 27.49382079585014793, 308.0021161605097291, -9.293432125849182768 ) ) ;
#89746 = EDGE_LOOP ( 'NONE', ( #2921, #77050, #69619, #73310, #81220, #51368 ) ) ;
#89747 = FACE_OUTER_BOUND ( 'NONE', #39787, .T. ) ;
#89748 = CARTESIAN_POINT ( 'NONE',  ( -6.581905802744468126, 41.48827110272019780, -70.61906944529594909 ) ) ;
#89749 = CARTESIAN_POINT ( 'NONE',  ( -87.01158373004948032, -60.18652252783364531, -5.598645846854314101 ) ) ;
#89750 = CIRCLE ( 'NONE', #75958, 8.000000000000000000 ) ;
#89751 = DIRECTION ( 'NONE',  ( -1.000000000000000000, -1.224606353822377258E-16, -0.000000000000000000 ) ) ;
#89752 = DIRECTION ( 'NONE',  ( 0.000000000000000000, 0.000000000000000000, -1.000000000000000000 ) ) ;
#89753 = VERTEX_POINT ( 'NONE', #15518 ) ;
#89754 = VECTOR ( 'NONE', #97973, 1000.000000000000000 ) ;
#89755 =( NAMED_UNIT ( * ) SI_UNIT ( $, .STERADIAN. ) SOLID_ANGLE_UNIT ( ) );
#89756 = CARTESIAN_POINT ( 'NONE',  ( 11.90409330339966409, 21.49301302430015070, -7.268787543711042076 ) ) ;
#89757 = CARTESIAN_POINT ( 'NONE',  ( 22.23822744035697241, -8.673617379884035472E-16, -2.910977163136222678 ) ) ;
#89758 = CARTESIAN_POINT ( 'NONE',  ( -35.52295374289839458, 436.6489517640831650, 4.915275271775389143 ) ) ;
#89759 = CARTESIAN_POINT ( 'NONE',  ( 47.46761990717632784, -14.21045842199427511, -33.06011575854734730 ) ) ;
#89760 = STYLED_ITEM ( 'NONE', ( #52125 ), #103525 ) ;
#89761 = CARTESIAN_POINT ( 'NONE',  ( -80.60696305975868370, -18.68079635666938643, 129.0832030291728927 ) ) ;
#89762 = EDGE_LOOP ( 'NONE', ( #41310, #66522, #406, #48756 ) ) ;
#89763 = CARTESIAN_POINT ( 'NONE',  ( 52.56736687853028656, -59.99999999999993605, 85.36620364727897936 ) ) ;
#89764 = CARTESIAN_POINT ( 'NONE',  ( 7.212994264445061532, 87.01711344340040455, 3.463766307298585811 ) ) ;
#89765 = CARTESIAN_POINT ( 'NONE',  ( 88.05830098754434232, -57.66964593057830513, -24.45951718257569496 ) ) ;
#89766 = CARTESIAN_POINT ( 'NONE',  ( 28.35193698574008181, 34.21473308898948318, 8.617696936426447962 ) ) ;
#89767 = DIRECTION ( 'NONE',  ( 0.000000000000000000, 1.000000000000000000, 0.000000000000000000 ) ) ;
#89768 = ORIENTED_EDGE ( 'NONE', *, *, #9474, .F. ) ;
#89769 = DIRECTION ( 'NONE',  ( -0.9090909090909089496, 0.000000000000000000, 0.4165977904505313578 ) ) ;
#89770 = PRESENTATION_STYLE_ASSIGNMENT (( #179 ) ) ;
#89771 = CARTESIAN_POINT ( 'NONE',  ( 15.56705434506301522, 43.91951069372706939, 6.063903585636011506 ) ) ;
#89772 = CARTESIAN_POINT ( 'NONE',  ( -7.188101187500002709, -16.81250000204838457, 2.977408999572648707 ) ) ;
#89773 = CARTESIAN_POINT ( 'NONE',  ( 43.65809794933323218, 484.6141936383338020, 3.261896584721304393 ) ) ;
#89774 = CARTESIAN_POINT ( 'NONE',  ( 9.221249107921748234, 83.95178628501514595, 3.869340886054257300 ) ) ;
#89775 = CARTESIAN_POINT ( 'NONE',  ( -3.313708498984765161, -13.15625000409676915, 7.999999999999998224 ) ) ;
#89776 = ORIENTED_EDGE ( 'NONE', *, *, #69638, .T. ) ;
#89777 = ADVANCED_FACE ( 'NONE', ( #6349 ), #58344, .T. ) ;
#89778 = CARTESIAN_POINT ( 'NONE',  ( -7.084743457969951308, 40.92373752417397270, -70.77066391255284827 ) ) ;
#89780 = CARTESIAN_POINT ( 'NONE',  ( 29.78856322856827177, -39.48450492069009954, 33.06000570913132464 ) ) ;
#89779 = CARTESIAN_POINT ( 'NONE',  ( -8.555246586836847911, -60.00000000000005684, 41.98716887921269603 ) ) ;
#89781 = CARTESIAN_POINT ( 'NONE',  ( -23.97876356160471900, 25.74925960686173809, 30.95194294911825850 ) ) ;
#89782 = ORIENTED_EDGE ( 'NONE', *, *, #23958, .F. ) ;
#89783 = EDGE_CURVE ( 'NONE', #76580, #45933, #41103, .T. ) ;
#89784 = ADVANCED_FACE ( 'NONE', ( #42453 ), #101387, .T. ) ;
#89785 = ORIENTED_EDGE ( 'NONE', *, *, #104133, .F. ) ;
#89787 = DIRECTION ( 'NONE',  ( 0.000000000000000000, -1.000000000000000000, 0.000000000000000000 ) ) ;
#89786 = LINE ( 'NONE', #48767, #60744 ) ;
#89788 = CARTESIAN_POINT ( 'NONE',  ( 86.17777777777776294, 1.023464760207051730E-14, 0.000000000000000000 ) ) ;
#89789 = DIRECTION ( 'NONE',  ( 0.000000000000000000, 0.000000000000000000, 1.000000000000000000 ) ) ;
#89790 = CARTESIAN_POINT ( 'NONE',  ( 6.503418564380250899, 41.93912275385427080, -68.91429206611401526 ) ) ;
#89791 = CARTESIAN_POINT ( 'NONE',  ( 1.250573470519673158, 45.68617730187271775, 17.65550772099327759 ) ) ;
#89792 = DIRECTION ( 'NONE',  ( 0.000000000000000000, 0.000000000000000000, 1.000000000000000000 ) ) ;
#89793 = EDGE_LOOP ( 'NONE', ( #88176, #30897, #96423, #64143, #26200, #81369 ) ) ;
#89794 = CARTESIAN_POINT ( 'NONE',  ( 8.249451541537798249, -60.00000000000000000, -42.48302917854579164 ) ) ;
#89795 = DIRECTION ( 'NONE',  ( 0.9090909090909090606, 0.000000000000000000, -0.4165977904505313578 ) ) ;
#89796 = MECHANICAL_DESIGN_GEOMETRIC_PRESENTATION_REPRESENTATION (  '', ( #15707 ), #103567 ) ;
#89798 = CARTESIAN_POINT ( 'NONE',  ( -15.54886886242640998, -0.9489809227296597260, 14.97197842136719181 ) ) ;
#89797 = VECTOR ( 'NONE', #52802, 1000.000000000000000 ) ;
#89799 = EDGE_CURVE ( 'NONE', #31549, #85235, #99081, .T. ) ;
#89800 = DIRECTION ( 'NONE',  ( 1.000000000000000000, 0.000000000000000000, 0.000000000000000000 ) ) ;
#89801 = CONICAL_SURFACE ( 'NONE', #96643, 5.000000000000001776, 0.9599310885968803664 ) ;
#89802 = ADVANCED_FACE ( 'NONE', ( #9013 ), #35469, .F. ) ;
#89803 = CARTESIAN_POINT ( 'NONE',  ( 46.97259151695090651, 12.59255281441344110, -16.28847157548977265 ) ) ;
#89804 = VERTEX_POINT ( 'NONE', #59188 ) ;
#89805 = ORIENTED_EDGE ( 'NONE', *, *, #86267, .T. ) ;
#89806 = ORIENTED_EDGE ( 'NONE', *, *, #90298, .T. ) ;
#89807 = CARTESIAN_POINT ( 'NONE',  ( 0.3382013191121669982, 53.40883116819954068, 10.21491085553634726 ) ) ;
#89808 = CARTESIAN_POINT ( 'NONE',  ( 30.04542631808804387, 41.08154980029332393, -66.19663379991389718 ) ) ;
#89809 = CARTESIAN_POINT ( 'NONE',  ( 33.10942959112523454, 427.0911879376557181, 25.12314773043819827 ) ) ;
#89811 = CIRCLE ( 'NONE', #15721, 4.000000000000001776 ) ;
#89810 = CARTESIAN_POINT ( 'NONE',  ( -44.90174202792449165, 347.4042625033331433, 2.362512452797935758 ) ) ;
#89812 = CARTESIAN_POINT ( 'NONE',  ( -2.361588828579537225, -69.88257940272585245, 13.19812034727280370 ) ) ;
#89813 = CARTESIAN_POINT ( 'NONE',  ( -44.19305039087728915, 485.5049587488591101, 3.133877349347021557 ) ) ;
#89814 =( NAMED_UNIT ( * ) SI_UNIT ( $, .STERADIAN. ) SOLID_ANGLE_UNIT ( ) );
#89815 = ORIENTED_EDGE ( 'NONE', *, *, #47517, .F. ) ;
#89816 = CARTESIAN_POINT ( 'NONE',  ( 30.75880901179687044, 7.960713337733333894, 41.50491223544427299 ) ) ;
#89817 = CIRCLE ( 'NONE', #72558, 4.172000000000001485 ) ;
#89818 = ORIENTED_EDGE ( 'NONE', *, *, #20511, .F. ) ;
#89819 = FACE_OUTER_BOUND ( 'NONE', #83438, .T. ) ;
#89820 = CARTESIAN_POINT ( 'NONE',  ( -25.60851123651793415, 48.00000000000000000, -75.29411764705882604 ) ) ;
#89821 = CARTESIAN_POINT ( 'NONE',  ( -38.04320146006180181, -60.00000000000000711, 41.36025795104787051 ) ) ;
#89822 = CARTESIAN_POINT ( 'NONE',  ( 65.58602450514189286, -25.57852054671029762, 80.66737998054381364 ) ) ;
#89823 = ORIENTED_EDGE ( 'NONE', *, *, #35152, .F. ) ;
#89824 = CARTESIAN_POINT ( 'NONE',  ( 4.999999998541157176, -46.36031008665895570, 40.27905619190705977 ) ) ;
#89825 = CARTESIAN_POINT ( 'NONE',  ( 0.000000000000000000, 0.000000000000000000, -2.296599999999999753 ) ) ;
#89826 = CARTESIAN_POINT ( 'NONE',  ( -28.02803974396783815, -57.67115643259209889, -43.15031372974605972 ) ) ;
#89827 = VERTEX_POINT ( 'NONE', #76950 ) ;
#89828 = AXIS2_PLACEMENT_3D ( 'NONE', #91994, #102751, #86595 ) ;
#89829 =( NAMED_UNIT ( * ) SI_UNIT ( $, .STERADIAN. ) SOLID_ANGLE_UNIT ( ) );
#89830 = DIRECTION ( 'NONE',  ( -1.000000000000000000, -1.224606353822377258E-16, -0.000000000000000000 ) ) ;
#89831 = AXIS2_PLACEMENT_3D ( 'NONE', #21107, #63115, #12947 ) ;
#89832 = CARTESIAN_POINT ( 'NONE',  ( -35.00143047691628340, 490.1822567707091594, 12.08765882792895852 ) ) ;
#89833 = ADVANCED_FACE ( 'NONE', ( #50011 ), #18740, .T. ) ;
#89834 = CIRCLE ( 'NONE', #62289, 74.46152422706630603 ) ;
#89835 = CARTESIAN_POINT ( 'NONE',  ( 8.000000000000000000, -32.09375000409677625, -3.313708498984761608 ) ) ;
#89836 = CARTESIAN_POINT ( 'NONE',  ( -10.00000000000000000, -5.000000000000000000, 2.617993873628187806 ) ) ;
#89837 = CARTESIAN_POINT ( 'NONE',  ( 33.00000000000002842, 489.5971041675261404, 10.80646835458719224 ) ) ;
#89838 = CARTESIAN_POINT ( 'NONE',  ( 8.929771841637641927, 1.482358050883964840E-15, 0.000000000000000000 ) ) ;
#89839 = CARTESIAN_POINT ( 'NONE',  ( -10.00002837221254559, 7.499959371255492613, 0.000000000000000000 ) ) ;
#89840 = DIRECTION ( 'NONE',  ( 0.000000000000000000, -1.000000000000000000, 0.000000000000000000 ) ) ;
#89841 = CARTESIAN_POINT ( 'NONE',  ( -1.927070765752276982, -29.99999999999998934, -7.651354226332538921 ) ) ;
#89842 = ORIENTED_EDGE ( 'NONE', *, *, #34331, .F. ) ;
#89843 = FACE_OUTER_BOUND ( 'NONE', #16235, .T. ) ;
#89844 = DIRECTION ( 'NONE',  ( 1.000000000000000000, 0.000000000000000000, 0.000000000000000000 ) ) ;
#89845 = CARTESIAN_POINT ( 'NONE',  ( 12.16851236901548461, -60.00000000000000000, 39.68953834586075402 ) ) ;
#89846 = CARTESIAN_POINT ( 'NONE',  ( -96.88846608153241391, -29.99999999999999289, 191.1171794686087537 ) ) ;
#89847 = EDGE_CURVE ( 'NONE', #87652, #66563, #63520, .T. ) ;
#89848 = CARTESIAN_POINT ( 'NONE',  ( 0.000000000000000000, 0.000000000000000000, 0.000000000000000000 ) ) ;
#89849 = CARTESIAN_POINT ( 'NONE',  ( 46.38270258108293120, -57.68171275033647305, 68.22110787291272516 ) ) ;
#89851 = CARTESIAN_POINT ( 'NONE',  ( 16.64348903516512834, -1.200000000000000030E-05, -6.657797401561770911 ) ) ;
#89850 = CARTESIAN_POINT ( 'NONE',  ( -0.08409598735685096249, 26.07813853931758175, -38.24999999999999289 ) ) ;
#89852 = CARTESIAN_POINT ( 'NONE',  ( 14.73658302030201916, -23.99622960207933176, -38.53156179264232151 ) ) ;
#89853 = CARTESIAN_POINT ( 'NONE',  ( -21.12363372865564770, -60.00000000000000000, 40.37864402363731386 ) ) ;
#89854 = LINE ( 'NONE', #264, #62373 ) ;
#89855 = EDGE_CURVE ( 'NONE', #8913, #102936, #27376, .T. ) ;
#89856 = CARTESIAN_POINT ( 'NONE',  ( 1.100705560355868640, 45.52331009687405583, -18.11393409840396274 ) ) ;
#89857 = CARTESIAN_POINT ( 'NONE',  ( -86.95901752989097133, -39.09618168350279177, 189.0029776537705004 ) ) ;
#89858 = AXIS2_PLACEMENT_3D ( 'NONE', #88632, #33080, #72958 ) ;
#89859 = VERTEX_POINT ( 'NONE', #82915 ) ;
#89860 = CARTESIAN_POINT ( 'NONE',  ( 17.50000000000007105, 51.60805965402359163, 62.32523305738168773 ) ) ;
#89861 = CARTESIAN_POINT ( 'NONE',  ( 10.25662953440644110, -12.00964996486999325, 17.46101989419365452 ) ) ;
#89862 = CARTESIAN_POINT ( 'NONE',  ( -10.30264850706973334, -42.95776240863717277, 31.06144808585462158 ) ) ;
#89863 = FACE_OUTER_BOUND ( 'NONE', #66934, .T. ) ;
#89864 = AXIS2_PLACEMENT_3D ( 'NONE', #1161, #74013, #33064 ) ;
#89865 = EDGE_CURVE ( 'NONE', #1287, #42289, #41921, .T. ) ;
#89867 = CARTESIAN_POINT ( 'NONE',  ( 1.737810032903332802, -69.62561923041629086, 12.84439221602053571 ) ) ;
#89866 = DIRECTION ( 'NONE',  ( 0.000000000000000000, 0.000000000000000000, 1.000000000000000000 ) ) ;
#89868 = VERTEX_POINT ( 'NONE', #42998 ) ;
#89869 = SURFACE_SIDE_STYLE ('',( #24104 ) ) ;
#89870 = CARTESIAN_POINT ( 'NONE',  ( -7.007554382054896891, -4.192628124816097035, -17.12907408883408422 ) ) ;
#89871 = CARTESIAN_POINT ( 'NONE',  ( 16.75187969033571989, 34.25544727262119693, 24.30698433968583316 ) ) ;
#89872 = CARTESIAN_POINT ( 'NONE',  ( 34.62348220644697960, 301.9590946549885189, -0.3855663969161592930 ) ) ;
#89873 = CARTESIAN_POINT ( 'NONE',  ( 4.571008445750557314, -47.80671748343183936, 102.5889671997070849 ) ) ;
#89874 = CIRCLE ( 'NONE', #88121, 4.000000000000001776 ) ;
#89875 = FILL_AREA_STYLE_COLOUR ( '', #59901 ) ;
#89876 = CARTESIAN_POINT ( 'NONE',  ( 73.51917576782351205, -60.00000000000002132, 167.3794919118397502 ) ) ;
#89877 = CARTESIAN_POINT ( 'NONE',  ( -45.48003679188781234, 379.8448106960472614, 7.220331889307936457 ) ) ;
#89878 = ORIENTED_EDGE ( 'NONE', *, *, #73688, .T. ) ;
#89879 = CARTESIAN_POINT ( 'NONE',  ( -7.558582284419547825, -29.99999999999999289, 1.912896512380730218 ) ) ;
#89880 = CARTESIAN_POINT ( 'NONE',  ( 18.58349330513380693, 1.593028355512270962E-15, 0.000000000000000000 ) ) ;
#89881 = CARTESIAN_POINT ( 'NONE',  ( -34.67263685778915061, 485.1278622359849919, -2.016271555160150886 ) ) ;
#89882 = CARTESIAN_POINT ( 'NONE',  ( 3.996139059897768409, 136.8746867953503852, -5.000000000000000888 ) ) ;
#89883 = ORIENTED_EDGE ( 'NONE', *, *, #20611, .F. ) ;
#89884 = EDGE_CURVE ( 'NONE', #43, #10331, #77284, .T. ) ;
#89885 = CARTESIAN_POINT ( 'NONE',  ( -23.17107764268310888, 305.7664649652382423, 10.13667392129760536 ) ) ;
#89886 = EDGE_LOOP ( 'NONE', ( #48569, #50971, #65884, #104612, #72219 ) ) ;
#89887 = CARTESIAN_POINT ( 'NONE',  ( 33.94783393359897161, 484.1261039197349305, 1.321740980884978267 ) ) ;
#89888 =( BOUNDED_SURFACE ( )  B_SPLINE_SURFACE ( 3, 2, ( 
 ( #32805, #82923, #41929 ),
 ( #83448, #66744, #34416 ),
 ( #1993, #59730, #50535 ),
 ( #42459, #24714, #92606 ),
 ( #75351, #18217, #51068 ),
 ( #34940, #67810, #45664 ),
 ( #93687, #76955, #35477 ),
 ( #44610, #78025, #76416 ) ),
 .UNSPECIFIED., .F., .F., .F. ) 
 B_SPLINE_SURFACE_WITH_KNOTS ( ( 4, 2, 2, 4 ),
 ( 3, 3 ),
 ( 0.03861844051980970610, 0.04325213341840641879, 0.04556897986770477860, 0.04788582631700313841 ),
 ( 0.000000000000000000, 1.000000000000000000 ),
 .UNSPECIFIED. ) 
 GEOMETRIC_REPRESENTATION_ITEM ( )  RATIONAL_B_SPLINE_SURFACE ( (
 ( 1.000000000000000000, 0.8047781759831924564, 1.000000000000000000),
 ( 1.000000000000000000, 0.8123762462804489104, 1.000000000000000000),
 ( 1.000000000000000000, 0.8190659850617495463, 1.000000000000000000),
 ( 1.000000000000000000, 0.8191937571013252484, 1.000000000000000000),
 ( 1.000000000000000000, 0.8176092952780751322, 1.000000000000000000),
 ( 1.000000000000000000, 0.8122962088596183960, 1.000000000000000000),
 ( 1.000000000000000000, 0.8086311330828166444, 1.000000000000000000),
 ( 1.000000000000000000, 0.8047712282214323221, 1.000000000000000000) ) ) 
 REPRESENTATION_ITEM ( '' )  SURFACE ( )  );
#89889 = FILL_AREA_STYLE ('',( #39758 ) ) ;
#89890 = ORIENTED_EDGE ( 'NONE', *, *, #97741, .T. ) ;
#89891 = CARTESIAN_POINT ( 'NONE',  ( 52.56483885390522914, 49.99999999999999289, -38.23529411764705799 ) ) ;
#89892 = CARTESIAN_POINT ( 'NONE',  ( 5.000000000000000000, -14.03284112244661941, 9.638321536847527682 ) ) ;
#89893 = CARTESIAN_POINT ( 'NONE',  ( -46.26700095126739853, -60.00000000001953282, 68.87414247443797422 ) ) ;
#89894 = CARTESIAN_POINT ( 'NONE',  ( 44.15102752603837644, 435.2229927719864122, 14.45803418847442146 ) ) ;
#89895 = CARTESIAN_POINT ( 'NONE',  ( 80.47396527936437849, -59.99999999999998579, 196.5700788117762272 ) ) ;
#89896 = STYLED_ITEM ( 'NONE', ( #86228 ), #93490 ) ;
#89898 = CARTESIAN_POINT ( 'NONE',  ( 14.88179425905683040, -60.35850697746405302, 34.08740321138691343 ) ) ;
#89897 = CARTESIAN_POINT ( 'NONE',  ( -106.9542266815933829, -14.21045842199434084, 174.0135369018153995 ) ) ;
#89900 = CARTESIAN_POINT ( 'NONE',  ( 82.51400834001795204, -38.00000000000000000, 7.859624698400971887 ) ) ;
#89899 = PRODUCT_DEFINITION_CONTEXT ( 'detailed design', #63831, 'design' ) ;
#89901 = CARTESIAN_POINT ( 'NONE',  ( 0.6441586697988379573, 54.23817744608182778, -7.915922717621211468 ) ) ;
#89902 = CARTESIAN_POINT ( 'NONE',  ( -45.40034815561197235, -29.15988752944468132, 41.32649748755925856 ) ) ;
#89903 = VECTOR ( 'NONE', #45047, 1000.000000000000000 ) ;
#89904 = DIRECTION ( 'NONE',  ( -0.000000000000000000, -1.000000000000000000, -0.000000000000000000 ) ) ;
#89905 = VERTEX_POINT ( 'NONE', #2520 ) ;
#89906 =( LENGTH_UNIT ( ) NAMED_UNIT ( * ) SI_UNIT ( .MILLI., .METRE. ) );
#89907 = DIRECTION ( 'NONE',  ( -1.000000000000000000, -0.000000000000000000, -0.000000000000000000 ) ) ;
#89908 = CARTESIAN_POINT ( 'NONE',  ( 29.45362385905110969, 325.9253963054578662, 15.14270878922920716 ) ) ;
#89909 = CARTESIAN_POINT ( 'NONE',  ( 9.797174393178825657E-16, 0.000000000000000000, -8.000000000000000000 ) ) ;
#89910 = CARTESIAN_POINT ( 'NONE',  ( 0.000000000000000000, 4.898587196589412829E-16, -4.000000000000000000 ) ) ;
#89911 = CARTESIAN_POINT ( 'NONE',  ( 28.76346532419124458, 309.5219921958590135, -8.933260212751790164 ) ) ;
#89912 = ORIENTED_EDGE ( 'NONE', *, *, #1716, .T. ) ;
#89913 = CARTESIAN_POINT ( 'NONE',  ( 5.238409285680604377, -48.00301508172830722, 104.1169421774613539 ) ) ;
#89914 = VERTEX_POINT ( 'NONE', #26854 ) ;
#89915 = CARTESIAN_POINT ( 'NONE',  ( 55.77201978694041884, -30.00000000000000000, 79.48271800460260295 ) ) ;
#89916 = CARTESIAN_POINT ( 'NONE',  ( 46.96405579082752979, 13.62080378033664196, 14.94667195310829122 ) ) ;
#89917 = CARTESIAN_POINT ( 'NONE',  ( 45.94900261086841198, 3.851859888774471706E-31, 5.000000000000001776 ) ) ;
#89919 = ADVANCED_FACE ( 'NONE', ( #67282 ), #74806, .T. ) ;
#89918 = SURFACE_STYLE_USAGE ( .BOTH. , #22569 ) ;
#89920 = CARTESIAN_POINT ( 'NONE',  ( 97.88837943941081221, -30.00000000000000000, 136.7472917770585070 ) ) ;
#89921 = EDGE_CURVE ( 'NONE', #34686, #30914, #11825, .T. ) ;
#89922 = CARTESIAN_POINT ( 'NONE',  ( 7.045965687440312486, 103.6960753621396378, 3.790395326974321133 ) ) ;
#89923 = ORIENTED_EDGE ( 'NONE', *, *, #37911, .F. ) ;
#89924 = EDGE_LOOP ( 'NONE', ( #67453, #17182, #102328, #106235, #2389 ) ) ;
#89925 = ORIENTED_EDGE ( 'NONE', *, *, #47857, .F. ) ;
#89926 = CARTESIAN_POINT ( 'NONE',  ( 9.797174393178825657E-16, 115.0000000000000000, 8.000000000000000000 ) ) ;
#89927 = CARTESIAN_POINT ( 'NONE',  ( 23.21751746555303342, 25.98869614573808207, 30.70617127781016720 ) ) ;
#89928 = EDGE_CURVE ( 'NONE', #34210, #49122, #103155, .T. ) ;
#89929 = CARTESIAN_POINT ( 'NONE',  ( 32.33349330513380693, 1.593028355512270962E-15, 0.000000000000000000 ) ) ;
#89930 = ORIENTED_EDGE ( 'NONE', *, *, #29665, .T. ) ;
#89931 = DIRECTION ( 'NONE',  ( 0.000000000000000000, -1.000000000000000000, 0.000000000000000000 ) ) ;
#89932 = EDGE_LOOP ( 'NONE', ( #103406, #42537, #90992 ) ) ;
#89933 = DIRECTION ( 'NONE',  ( -1.000000000000000000, -0.000000000000000000, -0.000000000000000000 ) ) ;
#89934 = CARTESIAN_POINT ( 'NONE',  ( 81.59556071043041925, -38.84188875790712103, 195.3954600456527260 ) ) ;
#89935 = CARTESIAN_POINT ( 'NONE',  ( 13.53516154045776076, 7.599662942191373283, 8.420555603062727101 ) ) ;
#89936 = CARTESIAN_POINT ( 'NONE',  ( 29.55500230678722673, 314.0625905908086111, 12.66100350989708012 ) ) ;
#89937 = DIRECTION ( 'NONE',  ( 0.000000000000000000, 0.000000000000000000, -1.000000000000000000 ) ) ;
#89938 = DIRECTION ( 'NONE',  ( -1.000000000000000000, -0.000000000000000000, -0.000000000000000000 ) ) ;
#89939 = B_SPLINE_CURVE_WITH_KNOTS ( 'NONE', 3,
 ( #44355, #95043, #86953, #100985, #77249, #35770, #85341, #102588, #60553, #3365, #60031, #35223, #36827, #21179, #11969, #10892 ),
 .UNSPECIFIED., .F., .F.,
 ( 4, 2, 2, 2, 2, 2, 2, 4 ),
 ( 4.525475972510097653E-17, 0.001025531879885757452, 0.001538297819828604628, 0.002051063759771452021, 0.002563829699714299196, 0.003076595639657146372, 0.003589361579599994415, 0.004102127519542841591 ),
 .UNSPECIFIED. ) ;
#89940 = AXIS2_PLACEMENT_3D ( 'NONE', #74825, #75904, #90497 ) ;
#89941 = CARTESIAN_POINT ( 'NONE',  ( -40.90837589347040648, 460.4813280201778412, 2.460853848286399082 ) ) ;
#89942 = CONICAL_SURFACE ( 'NONE', #100255, 4.172000000000009479, 0.9599310885968813656 ) ;
#89943 = CARTESIAN_POINT ( 'NONE',  ( -4.188755055078890344, -48.42812442300444076, 102.8981131900555113 ) ) ;
#89944 = FACE_OUTER_BOUND ( 'NONE', #47849, .T. ) ;
#89945 = CYLINDRICAL_SURFACE ( 'NONE', #10882, 7.000000000000000000 ) ;
#89946 = ORIENTED_EDGE ( 'NONE', *, *, #76903, .F. ) ;
#89947 = CARTESIAN_POINT ( 'NONE',  ( 1.898667928446299280, -49.86745472351331188, 102.2341000961458803 ) ) ;
#89948 = CARTESIAN_POINT ( 'NONE',  ( -27.29693123059870885, 296.4603777880672055, 2.286005658668618601 ) ) ;
#89949 = CARTESIAN_POINT ( 'NONE',  ( 7.465530826735402137, 54.30101273655428429, -2.153335479310952039 ) ) ;
#89950 = DIRECTION ( 'NONE',  ( 0.000000000000000000, -1.000000000000000000, 0.000000000000000000 ) ) ;
#89951 = CARTESIAN_POINT ( 'NONE',  ( 8.000000000000000000, -15.49999999999999289, 0.000000000000000000 ) ) ;
#89952 = CARTESIAN_POINT ( 'NONE',  ( -11.19867756180316576, -20.63762499452760579, 35.45502084197963200 ) ) ;
#89953 = CIRCLE ( 'NONE', #103738, 5.000000000000002665 ) ;
#89954 = VECTOR ( 'NONE', #6252, 1000.000000000000000 ) ;
#89955 = CARTESIAN_POINT ( 'NONE',  ( 3.267219863862204754, 300.0925129258962443, 9.454287392228017950 ) ) ;
#89956 = EDGE_CURVE ( 'NONE', #102890, #99463, #91555, .T. ) ;
#89957 = APPLICATION_CONTEXT ( 'automotive_design' ) ;
#89958 = VERTEX_POINT ( 'NONE', #67801 ) ;
#89959 = CARTESIAN_POINT ( 'NONE',  ( 86.22304159983994509, -21.27469319544424664, 177.9707522126931565 ) ) ;
#89960 = EDGE_CURVE ( 'NONE', #34382, #84395, #20529, .T. ) ;
#89961 = CARTESIAN_POINT ( 'NONE',  ( 0.000000000000000000, -19.99999999999998934, 0.000000000000000000 ) ) ;
#89962 = CARTESIAN_POINT ( 'NONE',  ( -9.609486011791419813, 143.0915023496522451, 5.000000000000004441 ) ) ;
#89963 = ORIENTED_EDGE ( 'NONE', *, *, #30298, .F. ) ;
#89964 = CARTESIAN_POINT ( 'NONE',  ( 91.18366750016291178, -57.66344145994273873, -20.65528270058285543 ) ) ;
#89965 = CARTESIAN_POINT ( 'NONE',  ( 34.47678062874017968, 437.1474145881098252, 5.468662283308795224 ) ) ;
#89966 = CARTESIAN_POINT ( 'NONE',  ( -14.29190075645216851, 12.99999999999999289, 0.000000000000000000 ) ) ;
#89967 = CARTESIAN_POINT ( 'NONE',  ( 28.49094055106857581, 13.12977990610423085, 40.46781900651338049 ) ) ;
#89968 = CARTESIAN_POINT ( 'NONE',  ( -80.85862215050043744, -29.99999999999999645, 6.799607089790798753 ) ) ;
#89969 = ADVANCED_FACE ( 'NONE', ( #84525 ), #66196, .T. ) ;
#89970 = CIRCLE ( 'NONE', #8960, 5.000000000000002665 ) ;
#89971 = AXIS2_PLACEMENT_3D ( 'NONE', #15761, #81527, #69117 ) ;
#89972 = CARTESIAN_POINT ( 'NONE',  ( -77.67718612014897417, -38.00000000000005684, 131.3029103090800049 ) ) ;
#89973 = CARTESIAN_POINT ( 'NONE',  ( -8.000000000000000000, -4.999999999999998224, -2.094395098902523955 ) ) ;
#89974 = CARTESIAN_POINT ( 'NONE',  ( -3.096526599377911193, 6.872473572140713749, 2.349104707051923644E-15 ) ) ;
#89976 = CARTESIAN_POINT ( 'NONE',  ( 46.84999999999999432, 3.309500000000003439, 0.000000000000000000 ) ) ;
#89975 = CARTESIAN_POINT ( 'NONE',  ( 7.500000000000007105, 39.99999999999998579, -68.91429205785453860 ) ) ;
#89977 = CARTESIAN_POINT ( 'NONE',  ( 45.59999999999999432, 3.309500000000003439, 0.000000000000000000 ) ) ;
#89978 = CARTESIAN_POINT ( 'NONE',  ( -16.32395179134260843, 43.58768466397686581, -6.626586996422831888 ) ) ;
#89979 = CARTESIAN_POINT ( 'NONE',  ( 5.909259836070535954, -81.13722795757931294, -1.072443315311454981 ) ) ;
#89980 = CARTESIAN_POINT ( 'NONE',  ( 9.999999999999857891, 15.00000000000006750, -3.648665620917497243 ) ) ;
#89981 = CIRCLE ( 'NONE', #76189, 1.000000000000016209 ) ;
#89982 = CARTESIAN_POINT ( 'NONE',  ( -100.3203616992955602, -38.00000000000001421, 190.0301232681506178 ) ) ;
#89983 = EDGE_LOOP ( 'NONE', ( #48552, #81042, #88869, #61724 ) ) ;
#89984 = DIRECTION ( 'NONE',  ( -1.000000000000000000, 0.000000000000000000, -0.000000000000000000 ) ) ;
#89985 = FILL_AREA_STYLE_COLOUR ( '', #48654 ) ;
#89986 = CARTESIAN_POINT ( 'NONE',  ( 7.703928834700305650, -4.447865386531949738, -7.917997657324739258 ) ) ;
#89987 = CARTESIAN_POINT ( 'NONE',  ( -32.71804766712359935, -22.58455031971449500, -31.71287671542873809 ) ) ;
#89988 = EDGE_CURVE ( 'NONE', #33529, #98095, #4927, .T. ) ;
#89990 = CARTESIAN_POINT ( 'NONE',  ( -53.90259159284356372, -47.40884937127464127, -29.08431734911702193 ) ) ;
#89989 = DIRECTION ( 'NONE',  ( -1.000000000000000000, -0.000000000000000000, -0.000000000000000000 ) ) ;
#89991 = ORIENTED_EDGE ( 'NONE', *, *, #85692, .T. ) ;
#89992 = VERTEX_POINT ( 'NONE', #10089 ) ;
#89993 = DIRECTION ( 'NONE',  ( -1.000000000000000000, 0.000000000000000000, 0.000000000000000000 ) ) ;
#89994 = CARTESIAN_POINT ( 'NONE',  ( -5.656854249492379694, -29.93749999999999645, -5.656854249492380582 ) ) ;
#89995 = CYLINDRICAL_SURFACE ( 'NONE', #23651, 5.000000000000002665 ) ;
#89996 = EDGE_CURVE ( 'NONE', #94271, #4153, #37064, .T. ) ;
#89997 = CARTESIAN_POINT ( 'NONE',  ( -49.90941830484705832, -60.00000000000000711, -37.92245557729972205 ) ) ;
#89999 = EDGE_CURVE ( 'NONE', #60237, #32972, #102833, .T. ) ;
#89998 = ORIENTED_EDGE ( 'NONE', *, *, #82464, .F. ) ;
#90000 = CARTESIAN_POINT ( 'NONE',  ( 51.09436811768170372, -36.01308660601653600, -27.73089587904936693 ) ) ;
#90001 = DIRECTION ( 'NONE',  ( 0.000000000000000000, 1.000000000000000000, 0.000000000000000000 ) ) ;
#90002 = CARTESIAN_POINT ( 'NONE',  ( 97.64984543025403241, -37.74050600311834103, 192.6344482948218513 ) ) ;
#90003 = CIRCLE ( 'NONE', #21380, 7.500000000000000888 ) ;
#90005 = DIRECTION ( 'NONE',  ( 0.000000000000000000, -1.000000000000000000, 0.000000000000000000 ) ) ;
#90004 = DIRECTION ( 'NONE',  ( 0.000000000000000000, -1.000000000000000000, 0.000000000000000000 ) ) ;
#90006 = ORIENTED_EDGE ( 'NONE', *, *, #48925, .T. ) ;
#90007 = ORIENTED_EDGE ( 'NONE', *, *, #44725, .F. ) ;
#90008 = VECTOR ( 'NONE', #79763, 1000.000000000000000 ) ;
#90009 = ORIENTED_EDGE ( 'NONE', *, *, #17028, .F. ) ;
#90010 = CARTESIAN_POINT ( 'NONE',  ( 29.42291439507181749, 324.0459798135065057, 13.67000796727436374 ) ) ;
#90011 = CARTESIAN_POINT ( 'NONE',  ( -4.999999999999440448, -15.32190040641671303, 13.82401333429963231 ) ) ;
#90012 =( LENGTH_UNIT ( ) NAMED_UNIT ( * ) SI_UNIT ( .MILLI., .METRE. ) );
#90013 = ORIENTED_EDGE ( 'NONE', *, *, #86397, .F. ) ;
#90014 = CARTESIAN_POINT ( 'NONE',  ( -18.99999999999999289, -4.000000000000000000, -1.500000000000000000 ) ) ;
#90015 = DIRECTION ( 'NONE',  ( 0.000000000000000000, 1.000000000000000000, 0.000000000000000000 ) ) ;
#90016 = CARTESIAN_POINT ( 'NONE',  ( -7.000000000000000000, 8.572527594031471218E-16, -6.724735318933162453 ) ) ;
#90017 = CARTESIAN_POINT ( 'NONE',  ( -44.31189620312834876, -57.68384900168454976, 63.67342368891909388 ) ) ;
#90018 = CARTESIAN_POINT ( 'NONE',  ( -7.188101187500002709, -31.81250000204839168, 2.977408999572648707 ) ) ;
#90019 = CARTESIAN_POINT ( 'NONE',  ( -4.165977904505308693, 16.00000000000000000, 9.090909090909091717 ) ) ;
#90020 = CARTESIAN_POINT ( 'NONE',  ( -0.4143833371980254476, 26.05270874984543639, 38.31770394904153676 ) ) ;
#90021 = CARTESIAN_POINT ( 'NONE',  ( 0.000000000000000000, 15.00000000000000000, -9.999999999999998224 ) ) ;
#90022 = CARTESIAN_POINT ( 'NONE',  ( -71.63495682827519317, -59.99999999999997868, -34.46936934826943855 ) ) ;
#90023 = DIRECTION ( 'NONE',  ( 0.000000000000000000, -1.000000000000000000, 0.000000000000000000 ) ) ;
#90024 = CARTESIAN_POINT ( 'NONE',  ( -51.98423175508690974, -36.04436685186517053, 52.98251616644076023 ) ) ;
#90025 = CARTESIAN_POINT ( 'NONE',  ( 2.454882126627601302, 21.02146602321183622, -6.559358972060581827 ) ) ;
#90026 = B_SPLINE_CURVE_WITH_KNOTS ( 'NONE', 3,
 ( #84052, #91625, #17735, #99155, #50594, #35003, #74872, #960, #26395, #9610 ),
 .UNSPECIFIED., .F., .F.,
 ( 4, 2, 2, 2, 4 ),
 ( 0.000000000000000000, 0.001993803085173304328, 0.003987606170346608657, 0.005981409255519911684, 0.007975212340693215579 ),
 .UNSPECIFIED. ) ;
#90027 = VERTEX_POINT ( 'NONE', #30023 ) ;
#90028 = CARTESIAN_POINT ( 'NONE',  ( -98.77881222975014452, -45.25002549436672439, 193.4356104138574608 ) ) ;
#90029 = CARTESIAN_POINT ( 'NONE',  ( -0.3333649190976236132, 51.28285977629721515, 10.20765125107239690 ) ) ;
#90030 = VERTEX_POINT ( 'NONE', #103364 ) ;
#90031 = CARTESIAN_POINT ( 'NONE',  ( -17.73896008590444140, 43.18065877884676951, 6.032786456716696222 ) ) ;
#90032 = CARTESIAN_POINT ( 'NONE',  ( 90.65106265292511978, -38.40367301679646772, -14.05939008884039687 ) ) ;
#90033 = CARTESIAN_POINT ( 'NONE',  ( 8.559508646656350805, -1.200000000000000030E-05, -1.531152949374623873 ) ) ;
#90034 = CARTESIAN_POINT ( 'NONE',  ( -5.623207912502805605, 51.29174090390986152, -8.497605637484657137 ) ) ;
#90035 = DIRECTION ( 'NONE',  ( -1.000000000000000000, -1.224606353822377258E-16, -0.000000000000000000 ) ) ;
#90036 = CARTESIAN_POINT ( 'NONE',  ( 83.83835625336350006, -30.00000000000001066, 159.6014582805543114 ) ) ;
#90037 = VECTOR ( 'NONE', #63586, 1000.000000000000000 ) ;
#90038 = CARTESIAN_POINT ( 'NONE',  ( 34.98071605569023745, 490.8360413343243067, 11.88490725385638669 ) ) ;
#90039 = CARTESIAN_POINT ( 'NONE',  ( -29.59437054465040262, 13.24940423479644735, 39.60535821593506256 ) ) ;
#90040 = EDGE_CURVE ( 'NONE', #92392, #32665, #27862, .T. ) ;
#90041 = CARTESIAN_POINT ( 'NONE',  ( -6.826425371444816648, 2.641426549045764016, -6.344843397090114578 ) ) ;
#90042 = STYLED_ITEM ( 'NONE', ( #70469 ), #19059 ) ;
#90043 = ORIENTED_EDGE ( 'NONE', *, *, #100975, .T. ) ;
#90044 = ORIENTED_EDGE ( 'NONE', *, *, #61958, .T. ) ;
#90045 = CARTESIAN_POINT ( 'NONE',  ( 50.66589989479253830, -18.73013578598424544, 44.89221390001991807 ) ) ;
#90046 = AXIS2_PLACEMENT_3D ( 'NONE', #61849, #12728, #21924 ) ;
#90047 = CARTESIAN_POINT ( 'NONE',  ( 6.232335497085285780, 41.74193314002017985, -58.83489653296142308 ) ) ;
#90048 = EDGE_CURVE ( 'NONE', #17301, #1547, #106528, .T. ) ;
#90049 = CARTESIAN_POINT ( 'NONE',  ( 0.000000000000000000, 0.000000000000000000, -5.703399999999999359 ) ) ;
#90050 =( BOUNDED_SURFACE ( )  B_SPLINE_SURFACE ( 3, 2, ( 
 ( #99999, #26167, #91397 ),
 ( #24031, #106490, #42291 ),
 ( #83813, #105957, #34244 ),
 ( #83286, #50374, #15898 ) ),
 .UNSPECIFIED., .F., .F., .F. ) 
 B_SPLINE_SURFACE_WITH_KNOTS ( ( 4, 4 ),
 ( 3, 3 ),
 ( -2.023121253857951274E-15, 0.0002622513198896260392 ),
 ( 0.000000000000000000, 1.000000000000000000 ),
 .UNSPECIFIED. ) 
 GEOMETRIC_REPRESENTATION_ITEM ( )  RATIONAL_B_SPLINE_SURFACE ( (
 ( 1.000000000000000000, 0.7874655377939502321, 1.000000000000000000),
 ( 1.000000000000000000, 0.7887353030063457560, 1.000000000000000000),
 ( 1.000000000000000000, 0.7900011776560428300, 1.000000000000000000),
 ( 1.000000000000000000, 0.7912633096140608835, 1.000000000000000000) ) ) 
 REPRESENTATION_ITEM ( '' )  SURFACE ( )  );
#90051 = VERTEX_POINT ( 'NONE', #5199 ) ;
#90052 = CARTESIAN_POINT ( 'NONE',  ( -99.13475156731828974, -38.35568229781205218, 83.36745941595933118 ) ) ;
#90053 = ORIENTED_EDGE ( 'NONE', *, *, #5394, .T. ) ;
#90054 = CARTESIAN_POINT ( 'NONE',  ( 37.38561277374697056, 1.340359594676612611E-15, 0.000000000000000000 ) ) ;
#90055 = CARTESIAN_POINT ( 'NONE',  ( 90.93190340128646199, -38.35213422126950888, 22.02682049786888996 ) ) ;
#90056 = CARTESIAN_POINT ( 'NONE',  ( 11.52703303463460749, 20.62217656626097551, -7.985623555383951633 ) ) ;
#90057 = CARTESIAN_POINT ( 'NONE',  ( -7.500000000000000888, -3.000671055698259870, -20.99923901233272971 ) ) ;
#90058 = CARTESIAN_POINT ( 'NONE',  ( 98.39798496753780910, -60.15124137177372887, 105.6244202628760291 ) ) ;
#90059 = CARTESIAN_POINT ( 'NONE',  ( -16.80223567637828452, 43.70004508566929502, -4.157797401561437844 ) ) ;
#90060 = FILL_AREA_STYLE_COLOUR ( '', #77391 ) ;
#90061 = CARTESIAN_POINT ( 'NONE',  ( -30.45624637448644023, 312.7340192834439563, -8.144926979512700171 ) ) ;
#90063 = AXIS2_PLACEMENT_3D ( 'NONE', #7147, #89, #33058 ) ;
#90062 = CARTESIAN_POINT ( 'NONE',  ( 1.227477900293065805, -69.63323560895928210, 12.78939886615606447 ) ) ;
#90064 = CARTESIAN_POINT ( 'NONE',  ( 75.57301170064098983, -60.00000000000000711, 184.8856015330856906 ) ) ;
#90065 = CARTESIAN_POINT ( 'NONE',  ( 17.67376586503952041, 45.00000000000000711, 62.91491236097121487 ) ) ;
#90066 = EDGE_LOOP ( 'NONE', ( #25772, #88508, #38696, #9711, #31769, #19136 ) ) ;
#90067 = CARTESIAN_POINT ( 'NONE',  ( 58.13224282022872558, -25.60471780380888163, 61.38686201737864678 ) ) ;
#90068 = FACE_OUTER_BOUND ( 'NONE', #88326, .T. ) ;
#90069 = EDGE_CURVE ( 'NONE', #105140, #105711, #75650, .T. ) ;
#90070 = DIRECTION ( 'NONE',  ( 0.000000000000000000, -1.000000000000000000, 0.000000000000000000 ) ) ;
#90071 = DIRECTION ( 'NONE',  ( 0.000000000000000000, 0.000000000000000000, 1.000000000000000000 ) ) ;
#90073 = CARTESIAN_POINT ( 'NONE',  ( -9.981808881366681874, -50.02775323464795321, 27.65604031336897251 ) ) ;
#90072 = CARTESIAN_POINT ( 'NONE',  ( -78.09727535895957828, -30.00000000009066170, 183.0935977092201483 ) ) ;
#90074 = CARTESIAN_POINT ( 'NONE',  ( -40.84855644196625235, 369.2103136256716311, 25.49516658059198804 ) ) ;
#90075 = CARTESIAN_POINT ( 'NONE',  ( 21.52280673074376338, 305.1198653818534581, 8.994423587666668496 ) ) ;
#90076 = CARTESIAN_POINT ( 'NONE',  ( -40.44926925267034079, 464.0738508500458011, 18.39527504910404687 ) ) ;
#90077 = CARTESIAN_POINT ( 'NONE',  ( 3.313708498984762496, -33.78125000000000000, 7.999999999999998224 ) ) ;
#90078 = CARTESIAN_POINT ( 'NONE',  ( -8.000000000000000000, 0.000000000000000000, -5.575057142857143155 ) ) ;
#90079 = EDGE_CURVE ( 'NONE', #39480, #89019, #103236, .T. ) ;
#90081 = B_SPLINE_CURVE_WITH_KNOTS ( 'NONE', 3,
 ( #82363, #64082, #7933, #81282 ),
 .UNSPECIFIED., .F., .F.,
 ( 4, 4 ),
 ( 0.000000000000000000, 0.0001439741052586902467 ),
 .UNSPECIFIED. ) ;
#90080 = CARTESIAN_POINT ( 'NONE',  ( 0.000000000000000000, 0.000000000000000000, 100.0000000000000000 ) ) ;
#90082 = VECTOR ( 'NONE', #9095, 1000.000000000000000 ) ;
#90083 = EDGE_LOOP ( 'NONE', ( #54737, #94631, #2556, #82368, #5876, #63196, #6906 ) ) ;
#90084 = CARTESIAN_POINT ( 'NONE',  ( 81.58455456068359979, -57.02865422085555025, 182.7966820730144377 ) ) ;
#90085 = CARTESIAN_POINT ( 'NONE',  ( 5.000000000000000888, -15.60834519661176856, -6.449721054204996307 ) ) ;
#90086 = CARTESIAN_POINT ( 'NONE',  ( 33.20902353462182788, 484.6199955813546580, 4.299886535038632829 ) ) ;
#90087 = ORIENTED_EDGE ( 'NONE', *, *, #12276, .T. ) ;
#90088 = AXIS2_PLACEMENT_3D ( 'NONE', #53756, #36559, #45155 ) ;
#90089 = DIRECTION ( 'NONE',  ( 0.000000000000000000, -1.000000000000000000, -0.000000000000000000 ) ) ;
#90090 = CARTESIAN_POINT ( 'NONE',  ( 7.340594533187418946, -3.410200195908025478, -18.44125947282588385 ) ) ;
#90091 = CARTESIAN_POINT ( 'NONE',  ( 26.12342974137753870, 34.87054449434884162, -9.597107001362633838 ) ) ;
#90092 = CARTESIAN_POINT ( 'NONE',  ( 0.000000000000000000, 50.00000000000000000, -97.00000000000000000 ) ) ;
#90093 = CARTESIAN_POINT ( 'NONE',  ( 7.500000000000001776, -4.330127018922199866, -0.9999999999999974465 ) ) ;
#90094 = PRESENTATION_LAYER_ASSIGNMENT (  '', '', ( #7392 ) ) ;
#90095 = CARTESIAN_POINT ( 'NONE',  ( -44.21332904831282917, 435.2494715644501184, 14.45449769377396976 ) ) ;
#90096 = EDGE_CURVE ( 'NONE', #54633, #29666, #36059, .T. ) ;
#90097 = SURFACE_SIDE_STYLE ('',( #26466 ) ) ;
#90098 = CARTESIAN_POINT ( 'NONE',  ( 37.56673239365870387, 25.75719283951018923, 10.95617127780998956 ) ) ;
#90099 = DIRECTION ( 'NONE',  ( -1.000000000000000000, 0.000000000000000000, 0.000000000000000000 ) ) ;
#90101 = CARTESIAN_POINT ( 'NONE',  ( -10.65573454473422998, 18.19277052736382672, -9.438289383338396732 ) ) ;
#90100 = CARTESIAN_POINT ( 'NONE',  ( -9.350002378314655971, -19.95346413354524628, 35.32894845137520434 ) ) ;
#90102 = CARTESIAN_POINT ( 'NONE',  ( -2.977408999572650039, -12.68750000204838280, -7.188101187500001821 ) ) ;
#90103 = CARTESIAN_POINT ( 'NONE',  ( -28.89099332366777872, 40.83906611472644954, 58.53034795361808307 ) ) ;
#90104 = LINE ( 'NONE', #58818, #29432 ) ;
#90105 = ORIENTED_EDGE ( 'NONE', *, *, #32326, .F. ) ;
#90106 = CARTESIAN_POINT ( 'NONE',  ( -17.50000000000034106, 49.99999999999979394, 59.82664205501249910 ) ) ;
#90107 = AXIS2_PLACEMENT_3D ( 'NONE', #95808, #87717, #44069 ) ;
#90108 = CARTESIAN_POINT ( 'NONE',  ( 24.32698811271407635, 25.20814661221487896, 32.55533594236108286 ) ) ;
#90109 = CARTESIAN_POINT ( 'NONE',  ( -7.844405524234906224, 79.54154322733928950, 0.000000000000000000 ) ) ;
#90110 = CIRCLE ( 'NONE', #69431, 12.00000000000001066 ) ;
#90111 = CARTESIAN_POINT ( 'NONE',  ( -7.500000000000001776, -4.999999999999998224, -68.91429205785460965 ) ) ;
#90112 = EDGE_CURVE ( 'NONE', #56343, #76051, #68886, .T. ) ;
#90113 = CARTESIAN_POINT ( 'NONE',  ( 2.499999999999973799, -24.66556253578214708, -30.98417860745333741 ) ) ;
#90114 =( GEOMETRIC_REPRESENTATION_CONTEXT ( 3 ) GLOBAL_UNCERTAINTY_ASSIGNED_CONTEXT ( ( #6786 ) ) GLOBAL_UNIT_ASSIGNED_CONTEXT ( ( #63979, #34814, #76288 ) ) REPRESENTATION_CONTEXT ( 'NONE', 'WORKASPACE' ) );
#90115 = EDGE_LOOP ( 'NONE', ( #88218, #101736, #62966, #10139 ) ) ;
#90116 = CARTESIAN_POINT ( 'NONE',  ( -4.656749229489884456, -86.31760408126429240, -3.785628640239149689 ) ) ;
#90117 = DIRECTION ( 'NONE',  ( -1.000000000000000000, -1.224606353822377258E-16, -0.000000000000000000 ) ) ;
#90118 = CIRCLE ( 'NONE', #41930, 4.000000000000007105 ) ;
#90119 = ORIENTED_EDGE ( 'NONE', *, *, #28138, .F. ) ;
#90120 = EDGE_CURVE ( 'NONE', #2681, #6495, #8443, .T. ) ;
#90121 = EDGE_CURVE ( 'NONE', #99989, #75460, #49785, .T. ) ;
#90122 = SURFACE_STYLE_USAGE ( .BOTH. , #81470 ) ;
#90123 = SURFACE_SIDE_STYLE ('',( #32446 ) ) ;
#90124 = CARTESIAN_POINT ( 'NONE',  ( -33.11567503806781332, 40.69458692646632159, -62.11412838755995836 ) ) ;
#90125 = CARTESIAN_POINT ( 'NONE',  ( -98.42509890393606042, -59.99999999999997868, 71.54236955077431048 ) ) ;
#90126 = DIRECTION ( 'NONE',  ( -1.000000000000000000, -0.000000000000000000, -0.000000000000000000 ) ) ;
#90127 = CARTESIAN_POINT ( 'NONE',  ( -6.624059643703564149, 294.7379298340728724, -10.02420444108935449 ) ) ;
#90128 = CARTESIAN_POINT ( 'NONE',  ( 4.678819457397437986, 8.078722181090837395, 5.000000000000000000 ) ) ;
#90129 = DIRECTION ( 'NONE',  ( -0.000000000000000000, -0.000000000000000000, -1.000000000000000000 ) ) ;
#90131 = CARTESIAN_POINT ( 'NONE',  ( 30.00000000000004619, 486.7222546968084771, 5.239171024090038209 ) ) ;
#90130 = CARTESIAN_POINT ( 'NONE',  ( -7.374560640982810611, -5.000000000000002665, -94.59600210748614302 ) ) ;
#90132 = CARTESIAN_POINT ( 'NONE',  ( -84.52672161841623222, -32.42574458993667719, 173.3582839768502311 ) ) ;
#90133 = VERTEX_POINT ( 'NONE', #86140 ) ;
#90135 =( NAMED_UNIT ( * ) SI_UNIT ( $, .STERADIAN. ) SOLID_ANGLE_UNIT ( ) );
#90134 = B_SPLINE_CURVE_WITH_KNOTS ( 'NONE', 3,
 ( #77634, #46848, #46331, #36685, #102974 ),
 .UNSPECIFIED., .F., .F.,
 ( 4, 1, 4 ),
 ( 0.000000000000000000, 0.003752776749732568331, 0.007505553499465136662 ),
 .UNSPECIFIED. ) ;
#90136 = EDGE_CURVE ( 'NONE', #77528, #23955, #100449, .T. ) ;
#90137 = ORIENTED_EDGE ( 'NONE', *, *, #13817, .T. ) ;
#90138 = VERTEX_POINT ( 'NONE', #52669 ) ;
#90139 = DIRECTION ( 'NONE',  ( 0.000000000000000000, -1.000000000000000000, 0.000000000000000000 ) ) ;
#90140 = CARTESIAN_POINT ( 'NONE',  ( 33.49627437231217186, 465.2401082455917845, 8.307162268779238801 ) ) ;
#90141 = VERTEX_POINT ( 'NONE', #28437 ) ;
#90142 = CARTESIAN_POINT ( 'NONE',  ( -3.318393640953817503, 303.8518027741603191, 9.936999414637822881 ) ) ;
#90143 = CARTESIAN_POINT ( 'NONE',  ( 57.45015997180046696, -4.000000000000000000, 4.898587196589421703E-16 ) ) ;
#90144 = CARTESIAN_POINT ( 'NONE',  ( 9.439578326262742181, 10.07476781607968341, -4.999999999999079847 ) ) ;
#90145 = DIRECTION ( 'NONE',  ( 0.000000000000000000, 0.000000000000000000, -1.000000000000000000 ) ) ;
#90146 = DIRECTION ( 'NONE',  ( -1.000000000000000000, -1.224606353822377258E-16, -0.000000000000000000 ) ) ;
#90147 = CARTESIAN_POINT ( 'NONE',  ( 107.0562500300223974, -29.99999999999996803, 141.2193814890308374 ) ) ;
#90148 = CARTESIAN_POINT ( 'NONE',  ( -110.6385074381434066, -60.00000000000007816, 195.8055798097608147 ) ) ;
#90149 = CARTESIAN_POINT ( 'NONE',  ( -62.81242157416450311, -25.58369064279834504, 72.96567011718758522 ) ) ;
#90150 = VERTEX_POINT ( 'NONE', #61323 ) ;
#90151 = CARTESIAN_POINT ( 'NONE',  ( 0.000000000000000000, 6.928203230275505220, -4.000000000000007105 ) ) ;
#90152 = CARTESIAN_POINT ( 'NONE',  ( 94.28611985541716933, -59.99999999997079669, 7.686723608328764890 ) ) ;
#90153 = ORIENTED_EDGE ( 'NONE', *, *, #4277, .T. ) ;
#90154 = CARTESIAN_POINT ( 'NONE',  ( 13.66213079746738934, -56.44306380163116188, 23.93919572553859609 ) ) ;
#90155 = CARTESIAN_POINT ( 'NONE',  ( -7.188101187500000044, -15.78125000204838635, -8.802885111219163269E-16 ) ) ;
#90156 = AXIS2_PLACEMENT_3D ( 'NONE', #37955, #91328, #78175 ) ;
#90157 = CARTESIAN_POINT ( 'NONE',  ( -9.500000000000003553, -5.000000000000000000, -68.91429205785459544 ) ) ;
#90158 = ORIENTED_EDGE ( 'NONE', *, *, #80496, .F. ) ;
#90159 = CARTESIAN_POINT ( 'NONE',  ( 0.000000000000000000, 0.000000000000000000, 8.000000000000000000 ) ) ;
#90160 = ORIENTED_EDGE ( 'NONE', *, *, #21161, .F. ) ;
#90161 = FACE_OUTER_BOUND ( 'NONE', #93957, .T. ) ;
#90162 = CARTESIAN_POINT ( 'NONE',  ( -7.188101187500000933, -29.37500000204838457, -2.977408999572651371 ) ) ;
#90163 = CARTESIAN_POINT ( 'NONE',  ( -111.9086460000415144, -59.99999999999997158, 180.9596613643843455 ) ) ;
#90164 = CARTESIAN_POINT ( 'NONE',  ( 9.821751540093583088, -57.46817456407566027, 25.10730599066359758 ) ) ;
#90165 = CARTESIAN_POINT ( 'NONE',  ( -7.188101187500002709, -29.18750000204839523, 2.977408999572648707 ) ) ;
#90166 = LINE ( 'NONE', #74502, #99891 ) ;
#90167 = CARTESIAN_POINT ( 'NONE',  ( 17.86591196048134478, 43.17255793597502134, -5.719226232856852832 ) ) ;
#90168 = COLOUR_RGB ( '', 0.08235294, 0.09019608, 0.10196078) ;
#90169 = CARTESIAN_POINT ( 'NONE',  ( -11.66952397775300909, 15.93506242127414652, 9.561843478809398889 ) ) ;
#90170 = CARTESIAN_POINT ( 'NONE',  ( -11.04277565600957800, -4.986087508017872594, -12.57685066306310162 ) ) ;
#90171 = FILL_AREA_STYLE_COLOUR ( '', #14090 ) ;
#90172 = CARTESIAN_POINT ( 'NONE',  ( 9.147394621530509085, -3.304799994669868735, 14.67325677361586322 ) ) ;
#90173 = CARTESIAN_POINT ( 'NONE',  ( -24.46939029779962027, 27.46660112286069833, 31.99934855281016155 ) ) ;
#90174 = EDGE_CURVE ( 'NONE', #105973, #9396, #54934, .T. ) ;
#90175 = CARTESIAN_POINT ( 'NONE',  ( 106.4219938862113821, -60.00000000000001421, 168.4123002066837955 ) ) ;
#90176 = CARTESIAN_POINT ( 'NONE',  ( -32.29403280988383784, -29.08578870323540499, 32.09562443352605499 ) ) ;
#90177 = DIRECTION ( 'NONE',  ( -1.000000000000000000, -0.000000000000000000, -0.000000000000000000 ) ) ;
#90178 = AXIS2_PLACEMENT_3D ( 'NONE', #103741, #96717, #22324 ) ;
#90179 = CARTESIAN_POINT ( 'NONE',  ( 38.96479555484809509, -56.80366364879377272, 41.53497084807919748 ) ) ;
#90180 = DIRECTION ( 'NONE',  ( 0.000000000000000000, 1.000000000000000000, 0.000000000000000000 ) ) ;
#90181 = ORIENTED_EDGE ( 'NONE', *, *, #83379, .T. ) ;
#90182 = EDGE_CURVE ( 'NONE', #37530, #46925, #63975, .T. ) ;
#90183 = CARTESIAN_POINT ( 'NONE',  ( -7.344505440741527558, 87.44618927298706978, -3.175463080953002226 ) ) ;
#90184 = CARTESIAN_POINT ( 'NONE',  ( -84.12347576869696297, -38.75549085414967010, 197.8715174774602588 ) ) ;
#90185 = ORIENTED_EDGE ( 'NONE', *, *, #40161, .F. ) ;
#90187 = CARTESIAN_POINT ( 'NONE',  ( 45.50145573691759182, 405.2496736015978627, 8.430338687477670234 ) ) ;
#90186 = DIRECTION ( 'NONE',  ( -1.000000000000000000, -1.224606353822377258E-16, -0.000000000000000000 ) ) ;
#90188 = CARTESIAN_POINT ( 'NONE',  ( -10.53539113526819015, 10.21274928881584998, 10.31347537521849311 ) ) ;
#90189 = CARTESIAN_POINT ( 'NONE',  ( 15.53259594841288127, 37.09623604092399773, 22.76975648258493123 ) ) ;
#90190 = CARTESIAN_POINT ( 'NONE',  ( 6.466227039643135832, 2.668354129823745868, 6.840182550749494439 ) ) ;
#90191 = CARTESIAN_POINT ( 'NONE',  ( 32.15166163075728178, 486.0589784586659903, 5.199393881400817818 ) ) ;
#90192 = CARTESIAN_POINT ( 'NONE',  ( -37.62251730745837364, 437.3427388312646826, 4.535622330043170614 ) ) ;
#90193 = CARTESIAN_POINT ( 'NONE',  ( -27.95570841088265368, 315.0023162612367287, 11.41332481783935826 ) ) ;
#90194 = CARTESIAN_POINT ( 'NONE',  ( -5.656854249492381470, -25.25000000409677270, 5.656854249492379694 ) ) ;
#90195 = CARTESIAN_POINT ( 'NONE',  ( 110.4910188636535935, -59.99999999999997868, 147.4617906836925272 ) ) ;
#90196 = CARTESIAN_POINT ( 'NONE',  ( 87.04245038058458306, 1.016364837396684119E-14, 0.000000000000000000 ) ) ;
#90197 =( BOUNDED_SURFACE ( )  B_SPLINE_SURFACE ( 3, 2, ( 
 ( #97952, #24101, #14358 ),
 ( #56943, #13308, #9457 ),
 ( #57474, #59105, #49926 ),
 ( #99535, #66653, #41309 ),
 ( #17048, #91985, #83892 ),
 ( #75257, #25712, #8934 ),
 ( #18123, #98995, #50978 ),
 ( #1359, #91472, #100607 ),
 ( #34321, #58012, #75803 ),
 ( #809, #42912, #67197 ),
 ( #33242, #8405, #41838 ),
 ( #90400, #66115, #58574 ),
 ( #17588, #10005, #49386 ),
 ( #40773, #74724, #33777 ),
 ( #82834, #26767, #74194 ),
 ( #32718, #26242, #1898 ),
 ( #50448, #274, #81744 ),
 ( #34853, #16502, #83359 ),
 ( #42371, #100074, #67721 ),
 ( #89867, #65587, #98474 ),
 ( #25159, #15973, #82296 ),
 ( #90938, #48851, #7866 ) ),
 .UNSPECIFIED., .F., .F., .F. ) 
 B_SPLINE_SURFACE_WITH_KNOTS ( ( 4, 2, 2, 2, 2, 2, 2, 2, 2, 2, 4 ),
 ( 3, 3 ),
 ( 9.575673587391975161E-16, 0.003256072800435538209, 0.004884109200652828747, 0.005698127400761473366, 0.006512145600870118851, 0.007326163800978764337, 0.008140182001087408956, 0.009768218401304699927, 0.01058223660141334455, 0.01139625480152198916, 0.01302429120173928014 ),
 ( 0.000000000000000000, 1.000000000000000000 ),
 .UNSPECIFIED. ) 
 GEOMETRIC_REPRESENTATION_ITEM ( )  RATIONAL_B_SPLINE_SURFACE ( (
 ( 1.000000000000000000, 0.8477912478910073490, 1.000000000000000000),
 ( 1.000000000000000000, 0.8670434152227779467, 1.000000000000000000),
 ( 1.000000000000000000, 0.8843226860176298665, 1.000000000000000000),
 ( 1.000000000000000000, 0.9072812172742162895, 1.000000000000000000),
 ( 1.000000000000000000, 0.9144387507582195651, 1.000000000000000000),
 ( 1.000000000000000000, 0.9243937791762486533, 1.000000000000000000),
 ( 1.000000000000000000, 0.9275815810102141512, 1.000000000000000000),
 ( 1.000000000000000000, 0.9336849299333107588, 1.000000000000000000),
 ( 1.000000000000000000, 0.9366082457614915979, 1.000000000000000000),
 ( 1.000000000000000000, 0.9420647132138212365, 1.000000000000000000),
 ( 1.000000000000000000, 0.9446105283158728882, 1.000000000000000000),
 ( 1.000000000000000000, 0.9493321006897598169, 1.000000000000000000),
 ( 1.000000000000000000, 0.9515192386868923657, 1.000000000000000000),
 ( 1.000000000000000000, 0.9574223867891574757, 1.000000000000000000),
 ( 1.000000000000000000, 0.9604696041222584579, 1.000000000000000000),
 ( 1.000000000000000000, 0.9638146532777485120, 1.000000000000000000),
 ( 1.000000000000000000, 0.9646961637823425750, 1.000000000000000000),
 ( 1.000000000000000000, 0.9660383415586468736, 1.000000000000000000),
 ( 1.000000000000000000, 0.9665040966128550792, 1.000000000000000000),
 ( 1.000000000000000000, 0.9673053536378352080, 1.000000000000000000),
 ( 1.000000000000000000, 0.9670582897025716829, 1.000000000000000000),
 ( 1.000000000000000000, 0.9661530732048717596, 1.000000000000000000) ) ) 
 REPRESENTATION_ITEM ( '' )  SURFACE ( )  );
#90198 = AXIS2_PLACEMENT_3D ( 'NONE', #67660, #16985, #8872 ) ;
#90199 = DIRECTION ( 'NONE',  ( 0.000000000000000000, 1.000000000000000000, -0.000000000000000000 ) ) ;
#90200 = EDGE_LOOP ( 'NONE', ( #86455, #67131, #46532, #28605, #28016 ) ) ;
#90201 = EDGE_CURVE ( 'NONE', #34748, #14310, #63450, .T. ) ;
#90202 = CARTESIAN_POINT ( 'NONE',  ( -93.75210457069380254, -29.99999999999987210, 191.2467940272817657 ) ) ;
#90203 = ORIENTED_EDGE ( 'NONE', *, *, #35625, .F. ) ;
#90204 = CARTESIAN_POINT ( 'NONE',  ( -9.113097280746998763, -54.26319141364687937, 31.11721482942555639 ) ) ;
#90205 = CARTESIAN_POINT ( 'NONE',  ( -15.51015326907006830, 2.604283801340433691, -0.3849796309549803897 ) ) ;
#90206 = CARTESIAN_POINT ( 'NONE',  ( 16.14595037814516587, 20.48432867205317365, 4.554748808022611506 ) ) ;
#90207 = CARTESIAN_POINT ( 'NONE',  ( 9.253817200599833370, 28.70007270083139161, -3.791916801615163202 ) ) ;
#90208 = CARTESIAN_POINT ( 'NONE',  ( -5.082755093536325042, -27.96875000204838457, -5.082755093536325930 ) ) ;
#90209 = DIRECTION ( 'NONE',  ( -0.5735764363510510444, -0.8191520442889883569, 0.000000000000000000 ) ) ;
#90210 = ADVANCED_FACE ( 'NONE', ( #106522 ), #96344, .F. ) ;
#90211 = CARTESIAN_POINT ( 'NONE',  ( 7.358395007876660898, 41.06696377170784729, -70.11547971526088929 ) ) ;
#90212 = VERTEX_POINT ( 'NONE', #6774 ) ;
#90214 = ORIENTED_EDGE ( 'NONE', *, *, #54374, .T. ) ;
#90213 = DIRECTION ( 'NONE',  ( 0.000000000000000000, 1.000000000000000000, 0.000000000000000000 ) ) ;
#90215 = CARTESIAN_POINT ( 'NONE',  ( 81.03589328419950277, -42.96753771842250558, 157.4344923703873746 ) ) ;
#90216 = CARTESIAN_POINT ( 'NONE',  ( -6.075724000949984216, 41.99394325426889196, -59.86320218788793568 ) ) ;
#90217 = ORIENTED_EDGE ( 'NONE', *, *, #8335, .F. ) ;
#90218 = DIRECTION ( 'NONE',  ( -1.000000000000000000, -1.224606353822377258E-16, -0.000000000000000000 ) ) ;
#90219 = CARTESIAN_POINT ( 'NONE',  ( 7.619753052866895970, -88.17451502807176666, -2.447276542590447246 ) ) ;
#90220 = CARTESIAN_POINT ( 'NONE',  ( 2.977408999572652260, -14.93750000204838457, 7.188101187500000044 ) ) ;
#90221 = DIRECTION ( 'NONE',  ( 0.000000000000000000, -1.000000000000000000, 0.000000000000000000 ) ) ;
#90222 = CARTESIAN_POINT ( 'NONE',  ( 61.66664358393324363, -59.99999999999998579, -29.25180319347440516 ) ) ;
#90223 = CARTESIAN_POINT ( 'NONE',  ( -33.09586041880449159, 373.7026161310072325, 24.17050744075106294 ) ) ;
#90224 = SURFACE_STYLE_FILL_AREA ( #65422 ) ;
#90225 = ORIENTED_EDGE ( 'NONE', *, *, #25794, .F. ) ;
#90227 = B_SPLINE_CURVE_WITH_KNOTS ( 'NONE', 3,
 ( #63249, #69744, #96142, #20716, #70274, #62208, #5007, #21748, #94015, #54584, #21227, #22275, #70799, #53554, #87523, #95606 ),
 .UNSPECIFIED., .F., .F.,
 ( 4, 2, 2, 2, 2, 2, 2, 4 ),
 ( 0.000000000000000000, 0.0005175470994303207851, 0.001035094198860641570, 0.001552641298290962247, 0.002070188397721283140, 0.002587735497151604034, 0.003105282596581924494, 0.004140376795442568016 ),
 .UNSPECIFIED. ) ;
#90226 = CIRCLE ( 'NONE', #74727, 13.00000000000003730 ) ;
#90228 = B_SPLINE_CURVE_WITH_KNOTS ( 'NONE', 3,
 ( #91701, #66890, #42067, #99229, #67427, #25397, #26465, #8637, #50665, #1045, #9690, #17286, #50161, #41538, #74954, #42600, #74428, #58253, #504, #91181 ),
 .UNSPECIFIED., .F., .F.,
 ( 4, 2, 2, 2, 2, 2, 2, 2, 2, 4 ),
 ( 0.000000000000000000, 0.002366343802433873607, 0.003549515703650809543, 0.004732687604867745479, 0.005915859506084680981, 0.007099031407301617351, 0.007690617357910085536, 0.008282203308518552853, 0.008873789259127021906, 0.009465375209735490958 ),
 .UNSPECIFIED. ) ;
#90229 = FACE_OUTER_BOUND ( 'NONE', #5820, .T. ) ;
#90230 = MANIFOLD_SOLID_BREP ( 'Cut-Extrude1', #20583 ) ;
#90231 = CARTESIAN_POINT ( 'NONE',  ( 7.229692759409445557, 41.58551695089550293, -59.68506492437333577 ) ) ;
#90232 = CARTESIAN_POINT ( 'NONE',  ( 16.36650669486618881, 4.898587196589413815E-16, -4.000000000000000888 ) ) ;
#90233 = B_SPLINE_CURVE_WITH_KNOTS ( 'NONE', 3,
 ( #18479, #85321, #9814, #52402 ),
 .UNSPECIFIED., .F., .F.,
 ( 4, 4 ),
 ( 5.204170427930421283E-18, 0.001831984915194801279 ),
 .UNSPECIFIED. ) ;
#90234 = CARTESIAN_POINT ( 'NONE',  ( 4.401442555609581635E-16, -30.78125000204838813, -7.188101187500000044 ) ) ;
#90235 = CARTESIAN_POINT ( 'NONE',  ( 24.39419124516655657, -28.62692427288619257, 38.06577721013648130 ) ) ;
#90236 = CARTESIAN_POINT ( 'NONE',  ( -40.03783884386260894, 489.2292324564466526, 11.31445617789379554 ) ) ;
#90237 = STYLED_ITEM ( 'NONE', ( #82560 ), #55172 ) ;
#90238 = DIRECTION ( 'NONE',  ( -1.000000000000000000, -0.000000000000000000, -0.000000000000000000 ) ) ;
#90239 = CARTESIAN_POINT ( 'NONE',  ( 36.41995684994217441, 439.0104540407872378, 23.96542090717511186 ) ) ;
#90240 = AXIS2_PLACEMENT_3D ( 'NONE', #106162, #81355, #7466 ) ;
#90241 = APPLICATION_PROTOCOL_DEFINITION ( 'draft international standard', 'automotive_design', 1998, #50704 ) ;
#90242 = CARTESIAN_POINT ( 'NONE',  ( 5.799999999999999822, 4.618802153517003184, -8.000000000000000000 ) ) ;
#90243 = ORIENTED_EDGE ( 'NONE', *, *, #50717, .F. ) ;
#90244 = FACE_OUTER_BOUND ( 'NONE', #79772, .T. ) ;
#90245 = AXIS2_PLACEMENT_3D ( 'NONE', #97303, #96277, #71432 ) ;
#90246 = DIRECTION ( 'NONE',  ( -1.000000000000000000, -0.000000000000000000, -0.000000000000000000 ) ) ;
#90247 = FILL_AREA_STYLE_COLOUR ( '', #63067 ) ;
#90248 = CARTESIAN_POINT ( 'NONE',  ( 14.01509066308681817, 42.58675651380951166, -91.23243584937777939 ) ) ;
#90249 = EDGE_CURVE ( 'NONE', #95728, #16669, #31098, .T. ) ;
#90250 = VERTEX_POINT ( 'NONE', #48283 ) ;
#90251 = EDGE_CURVE ( 'NONE', #34066, #92851, #98437, .T. ) ;
#90252 = CARTESIAN_POINT ( 'NONE',  ( 32.10528697966009304, 486.1671898930079578, 5.449875171705039989 ) ) ;
#90253 = CARTESIAN_POINT ( 'NONE',  ( 110.8284296095286408, -57.67014611720160389, 194.4637431536222607 ) ) ;
#90254 = EDGE_CURVE ( 'NONE', #99250, #46570, #72750, .T. ) ;
#90255 = CARTESIAN_POINT ( 'NONE',  ( 36.27064846733442494, 463.5381974806701919, 19.67843218035151054 ) ) ;
#90256 = CARTESIAN_POINT ( 'NONE',  ( 2.653887821103243727, 14.84905342050943311, 6.480402264000274748 ) ) ;
#90257 = FACE_OUTER_BOUND ( 'NONE', #23346, .T. ) ;
#90258 = CARTESIAN_POINT ( 'NONE',  ( 28.89099332371403861, 40.83906611472283288, 58.53034795359498332 ) ) ;
#90259 = CARTESIAN_POINT ( 'NONE',  ( -75.39763943359314169, -59.99999999999999289, 183.8902267106653596 ) ) ;
#90260 = CARTESIAN_POINT ( 'NONE',  ( -40.61216075948964033, 351.1469683695276558, 22.89433108575548914 ) ) ;
#90261 = CARTESIAN_POINT ( 'NONE',  ( -40.95420997525301487, 387.0967036739339164, 27.26945002580065136 ) ) ;
#90262 = CARTESIAN_POINT ( 'NONE',  ( -83.43770954620740099, -60.98761413718671065, 191.4432686340473140 ) ) ;
#90264 = EDGE_LOOP ( 'NONE', ( #97650, #69575, #45365, #99017, #104745 ) ) ;
#90263 = AXIS2_PLACEMENT_3D ( 'NONE', #35486, #41940, #75905 ) ;
#90265 = CARTESIAN_POINT ( 'NONE',  ( 27.36727613921635083, 306.5270185924862858, -9.405951803952929069 ) ) ;
#90266 = EDGE_CURVE ( 'NONE', #32321, #35136, #31535, .T. ) ;
#90267 = AXIS2_PLACEMENT_3D ( 'NONE', #101237, #93679, #51060 ) ;
#90268 = VERTEX_POINT ( 'NONE', #54647 ) ;
#90269 = CARTESIAN_POINT ( 'NONE',  ( 48.10000000000000142, 0.000000000000000000, 3.309499999999999886 ) ) ;
#90270 = CARTESIAN_POINT ( 'NONE',  ( 6.851679529983103610E-15, 22.97884757028485225, -55.94820918777160301 ) ) ;
#90271 = COLOUR_RGB ( '', 0.31764706, 0.68627451, 0.89019608) ;
#90272 = CARTESIAN_POINT ( 'NONE',  ( -83.09759193211895933, -37.81164733650378196, -2.431872990241325638 ) ) ;
#90273 = DIRECTION ( 'NONE',  ( 2.742080092235280244E-17, 0.000000000000000000, -1.000000000000000000 ) ) ;
#90274 = CARTESIAN_POINT ( 'NONE',  ( 33.52307692307692122, 1.411358822780289120E-15, 0.000000000000000000 ) ) ;
#90275 = ORIENTED_EDGE ( 'NONE', *, *, #28052, .T. ) ;
#90276 = CARTESIAN_POINT ( 'NONE',  ( 6.463481858019718196, 7.246446802359423067, -1.128819432756289487 ) ) ;
#90277 = CARTESIAN_POINT ( 'NONE',  ( 11.77417553695194208, 6.803368766693943748, -9.098819535938051928 ) ) ;
#90278 = CARTESIAN_POINT ( 'NONE',  ( 17.01589776168603407, -1.734723475976807094E-15, 2.227375807149028386 ) ) ;
#90279 = CARTESIAN_POINT ( 'NONE',  ( 32.99999999999997158, 464.4386723251831768, 6.308603495333048983 ) ) ;
#90280 = CARTESIAN_POINT ( 'NONE',  ( -24.89493309229959195, -29.99999999999998934, -38.80368402536839056 ) ) ;
#90281 = CARTESIAN_POINT ( 'NONE',  ( -76.96556261419941336, -39.49594249891509889, 129.2692312102975905 ) ) ;
#90282 = ORIENTED_EDGE ( 'NONE', *, *, #1198, .F. ) ;
#90283 = CARTESIAN_POINT ( 'NONE',  ( 37.39695856105412730, -59.99999999999995737, 52.44754946039245880 ) ) ;
#90284 = DIRECTION ( 'NONE',  ( -1.000000000000000000, -1.224606353822377258E-16, -0.000000000000000000 ) ) ;
#90285 = CARTESIAN_POINT ( 'NONE',  ( 93.86154337525294977, -57.67558731759218205, 9.050589446141858119 ) ) ;
#90286 = EDGE_LOOP ( 'NONE', ( #28612, #77191, #3799, #7993 ) ) ;
#90287 = DIRECTION ( 'NONE',  ( 0.000000000000000000, 0.000000000000000000, 1.000000000000000000 ) ) ;
#90288 = CARTESIAN_POINT ( 'NONE',  ( 55.00571552735602410, 6.975173280561618775E-15, 0.000000000000000000 ) ) ;
#90289 = ORIENTED_EDGE ( 'NONE', *, *, #17824, .F. ) ;
#90290 = DIRECTION ( 'NONE',  ( -1.000000000000000000, -1.224606353822377258E-16, -0.000000000000000000 ) ) ;
#90291 = CARTESIAN_POINT ( 'NONE',  ( 6.849999999999999645, 0.000000000000000000, 0.000000000000000000 ) ) ;
#90292 = CARTESIAN_POINT ( 'NONE',  ( -2.977408999572654480, -19.62500000204838457, 7.188101187499999156 ) ) ;
#90293 = CARTESIAN_POINT ( 'NONE',  ( 2.325424218456834335, -7.317669739338271917, -7.030005583190792606 ) ) ;
#90294 = CARTESIAN_POINT ( 'NONE',  ( 9.380871178326117388, 82.98883620201672784, 3.467392232194206780 ) ) ;
#90295 = CARTESIAN_POINT ( 'NONE',  ( 9.036570576874959571, 10.37119081301007917, -12.86120860535742416 ) ) ;
#90296 = CARTESIAN_POINT ( 'NONE',  ( -7.500000000000000000, 4.730921838224019460, -7.493596905200499592 ) ) ;
#90297 = CARTESIAN_POINT ( 'NONE',  ( 2.354743324221998613, 48.00000000000000711, -99.86073547176458476 ) ) ;
#90298 = EDGE_CURVE ( 'NONE', #65026, #59863, #62473, .T. ) ;
#90299 = AXIS2_PLACEMENT_3D ( 'NONE', #105549, #103044, #6306 ) ;
#90300 = ORIENTED_EDGE ( 'NONE', *, *, #57569, .T. ) ;
#90301 = CARTESIAN_POINT ( 'NONE',  ( -6.763062896852164663, 41.48827110272769403, -70.48955655162545497 ) ) ;
#90303 = CARTESIAN_POINT ( 'NONE',  ( 31.08139726357473975, -53.37705209072197476, 36.01296622256593594 ) ) ;
#90302 = CARTESIAN_POINT ( 'NONE',  ( -12.83279097724939000, -59.99999999999996447, 42.04727692947117390 ) ) ;
#90304 = CARTESIAN_POINT ( 'NONE',  ( -32.62553167428460199, 485.9570050037687565, 7.214059741198010300 ) ) ;
#90305 = ORIENTED_EDGE ( 'NONE', *, *, #93988, .F. ) ;
#90306 = EDGE_CURVE ( 'NONE', #86309, #45881, #10356, .T. ) ;
#90307 = EDGE_CURVE ( 'NONE', #84910, #80282, #20609, .T. ) ;
#90308 = EDGE_LOOP ( 'NONE', ( #31508, #70708, #97397, #105975, #96028 ) ) ;
#90310 = CARTESIAN_POINT ( 'NONE',  ( 1.009208733680683423, 51.97703478562248591, 8.244597349404022779 ) ) ;
#90309 = FILL_AREA_STYLE ('',( #57395 ) ) ;
#90311 = DIRECTION ( 'NONE',  ( -1.000000000000000000, 0.000000000000000000, 0.000000000000000000 ) ) ;
#90312 = STYLED_ITEM ( 'NONE', ( #74979 ), #55444 ) ;
#90313 = DIRECTION ( 'NONE',  ( 0.000000000000000000, 0.000000000000000000, 1.000000000000000000 ) ) ;
#90314 = CARTESIAN_POINT ( 'NONE',  ( 0.000000000000000000, 0.000000000000000000, 0.000000000000000000 ) ) ;
#90315 = CARTESIAN_POINT ( 'NONE',  ( 0.07724506424403219940, 12.91535575337014308, -51.75000000000000000 ) ) ;
#90316 = ORIENTED_EDGE ( 'NONE', *, *, #69143, .T. ) ;
#90317 = CARTESIAN_POINT ( 'NONE',  ( 32.98329542059315855, -60.00000000000001421, -40.55872363790090418 ) ) ;
#90318 = CARTESIAN_POINT ( 'NONE',  ( -11.38830949524098912, 45.34487012134832895, -14.75357462089496252 ) ) ;
#90319 = PRESENTATION_LAYER_ASSIGNMENT (  '', '', ( #48951 ) ) ;
#90320 = CARTESIAN_POINT ( 'NONE',  ( 29.99999999999375078, 464.1513975948316784, 11.53706206233560394 ) ) ;
#90321 = CARTESIAN_POINT ( 'NONE',  ( 46.00000000000000000, 461.7880546943557079, 10.79349299898485448 ) ) ;
#90322 = CARTESIAN_POINT ( 'NONE',  ( 47.29368197624711456, 13.12573487771098613, -14.58950938768722771 ) ) ;
#90323 = ORIENTED_EDGE ( 'NONE', *, *, #95037, .F. ) ;
#90324 = EDGE_CURVE ( 'NONE', #2640, #104315, #97218, .T. ) ;
#90325 = CARTESIAN_POINT ( 'NONE',  ( 0.000000000000000000, 6.123233995736770227E-16, -5.000000000000002665 ) ) ;
#90326 = VERTEX_POINT ( 'NONE', #52951 ) ;
#90327 = ORIENTED_EDGE ( 'NONE', *, *, #98957, .T. ) ;
#90328 = CARTESIAN_POINT ( 'NONE',  ( 1.002517492551115330, 54.10386726457789308, 8.249092293095747763 ) ) ;
#90329 = CARTESIAN_POINT ( 'NONE',  ( 51.48757442383971039, 38.95383793068618417, -37.45149417477087184 ) ) ;
#90330 = CARTESIAN_POINT ( 'NONE',  ( -36.80474084615011776, 28.12598060908854336, 11.20119898579589801 ) ) ;
#90331 = CARTESIAN_POINT ( 'NONE',  ( 33.07276483573664905, 438.9325140356084489, 23.89537236861388081 ) ) ;
#90332 = CARTESIAN_POINT ( 'NONE',  ( -35.77761637803537553, 327.7250599313179578, -3.907684277836948716 ) ) ;
#90333 = CARTESIAN_POINT ( 'NONE',  ( -2.429940952537731125, -69.36428444796445092, 12.93557570994918571 ) ) ;
#90334 = DIRECTION ( 'NONE',  ( -1.000000000000000000, 0.000000000000000000, 0.000000000000000000 ) ) ;
#90335 = CARTESIAN_POINT ( 'NONE',  ( 12.50000000000000711, 34.92454988980409780, -54.26535491090573515 ) ) ;
#90336 = VERTEX_POINT ( 'NONE', #62138 ) ;
#90337 = EDGE_CURVE ( 'NONE', #23078, #6036, #72199, .T. ) ;
#90338 = DIRECTION ( 'NONE',  ( 1.000000000000000000, 1.224606353822377258E-16, 0.000000000000000000 ) ) ;
#90339 = ORIENTED_EDGE ( 'NONE', *, *, #101646, .F. ) ;
#90340 = CARTESIAN_POINT ( 'NONE',  ( -6.827804075409870777, -2.999999999999648281, -71.19745151638491620 ) ) ;
#90341 = CARTESIAN_POINT ( 'NONE',  ( -52.56483885390524335, 49.99999999999999289, -38.23529411764707220 ) ) ;
#90342 = SURFACE_STYLE_USAGE ( .BOTH. , #65006 ) ;
#90343 = EDGE_CURVE ( 'NONE', #46768, #46516, #92067, .T. ) ;
#90344 = CARTESIAN_POINT ( 'NONE',  ( -50.19342719663330143, -60.00000000000001421, 58.08342307450251241 ) ) ;
#90345 = CARTESIAN_POINT ( 'NONE',  ( 64.36790054385453175, -39.48203839976437735, 84.34053321678844384 ) ) ;
#90346 = CIRCLE ( 'NONE', #43831, 1.000000000000006439 ) ;
#90347 = ORIENTED_EDGE ( 'NONE', *, *, #31090, .F. ) ;
#90348 = CARTESIAN_POINT ( 'NONE',  ( 8.334564508160873686, 38.95383793066860534, 63.67138272020815748 ) ) ;
#90349 = AXIS2_PLACEMENT_3D ( 'NONE', #24980, #42733, #33597 ) ;
#90350 = CARTESIAN_POINT ( 'NONE',  ( -39.15148982810983824, -57.67118160050520004, -41.75192649668374401 ) ) ;
#90351 = B_SPLINE_CURVE_WITH_KNOTS ( 'NONE', 3,
 ( #80090, #30519, #95763, #13760, #63416, #22437, #88206, #9374, #49304, #9920, #67111, #16423, #1817, #42288, #82753, #17509, #18040, #41230, #42827, #91394, #26164, #83809, #75723, #8855, #98916, #99454, #1276, #99996, #90315, #25627 ),
 .UNSPECIFIED., .F., .F.,
 ( 4, 2, 2, 2, 2, 2, 2, 2, 2, 2, 2, 2, 2, 2, 4 ),
 ( 0.006610199206806503976, 0.006841026956352766995, 0.007071854705899030015, 0.007533510204991551718, 0.007995165704084072553, 0.008456821203176593388, 0.009380132201361635058, 0.01030344319954667673, 0.01122675419773171146, 0.01215006519591674272, 0.01261172069500925835, 0.01307337619410177225, 0.01353503169319428615, 0.01376585944274054743, 0.01399668719228680698 ),
 .UNSPECIFIED. ) ;
#90352 = AXIS2_PLACEMENT_3D ( 'NONE', #58543, #27278, #10504 ) ;
#90354 = ORIENTED_EDGE ( 'NONE', *, *, #89046, .F. ) ;
#90353 = PRESENTATION_LAYER_ASSIGNMENT (  '', '', ( #21473 ) ) ;
#90355 = CARTESIAN_POINT ( 'NONE',  ( 4.250000000000000000, 0.000000000000000000, -1.971869939371574620 ) ) ;
#90356 = CARTESIAN_POINT ( 'NONE',  ( 5.453780363133834186, 52.04077698858505130, -6.031152949374485317 ) ) ;
#90357 = CARTESIAN_POINT ( 'NONE',  ( 6.281175601187045210, -7.505553499465143830, -3.129864801432403538E-16 ) ) ;
#90358 = CARTESIAN_POINT ( 'NONE',  ( 4.898587196589412829E-16, -25.81250000409677270, -8.000000000000000000 ) ) ;
#90359 = CARTESIAN_POINT ( 'NONE',  ( 0.000000000000000000, 5.629165124598848990, 3.250000000000002220 ) ) ;
#90360 = CARTESIAN_POINT ( 'NONE',  ( 33.13096700375007941, 488.4252353401654432, 9.689492805996717806 ) ) ;
#90361 = DIRECTION ( 'NONE',  ( -1.000000000000000000, -0.000000000000000000, -0.000000000000000000 ) ) ;
#90362 = CARTESIAN_POINT ( 'NONE',  ( -10.11206553723566159, 7.339953826372351386, 0.000000000000000000 ) ) ;
#90363 = LINE ( 'NONE', #40745, #60251 ) ;
#90364 =( NAMED_UNIT ( * ) PLANE_ANGLE_UNIT ( ) SI_UNIT ( $, .RADIAN. ) );
#90365 = FILL_AREA_STYLE_COLOUR ( '', #2226 ) ;
#90366 = ORIENTED_EDGE ( 'NONE', *, *, #59305, .F. ) ;
#90367 =( NAMED_UNIT ( * ) SI_UNIT ( $, .STERADIAN. ) SOLID_ANGLE_UNIT ( ) );
#90368 = CARTESIAN_POINT ( 'NONE',  ( -17.49999999999997513, 45.00000000000000711, -500000.0000000000582 ) ) ;
#90369 = CARTESIAN_POINT ( 'NONE',  ( 12.79681648763941304, -60.00000000000000711, 39.70851819966105012 ) ) ;
#90370 = CARTESIAN_POINT ( 'NONE',  ( -94.85800629167543718, -30.00000000000000711, 191.3397425934319642 ) ) ;
#90371 = AXIS2_PLACEMENT_3D ( 'NONE', #101637, #101100, #92465 ) ;
#90372 = EDGE_CURVE ( 'NONE', #73090, #27223, #76573, .T. ) ;
#90373 = DIRECTION ( 'NONE',  ( 1.000000000000000000, 1.224606353822377258E-16, 0.000000000000000000 ) ) ;
#90374 = CARTESIAN_POINT ( 'NONE',  ( 72.46120011609563960, -57.66624515346453705, 176.5848336718106850 ) ) ;
#90376 = CARTESIAN_POINT ( 'NONE',  ( -9.646908473743026846, 53.40519435939982174, 3.403286223225750362 ) ) ;
#90375 = CARTESIAN_POINT ( 'NONE',  ( 15.84496339826243272, -1.752972784076425317, 14.89969185729413859 ) ) ;
#90377 = EDGE_CURVE ( 'NONE', #32846, #71961, #101507, .T. ) ;
#90378 = EDGE_CURVE ( 'NONE', #82760, #20011, #82520, .T. ) ;
#90379 = CARTESIAN_POINT ( 'NONE',  ( 23.61215506847839407, -27.18552302756052086, -38.41032867837353137 ) ) ;
#90380 = CARTESIAN_POINT ( 'NONE',  ( -0.6412850917382576510, 43.23485188436026050, 18.57615738839334085 ) ) ;
#90382 = VECTOR ( 'NONE', #100353, 999.9999999999998863 ) ;
#90381 = UNCERTAINTY_MEASURE_WITH_UNIT (LENGTH_MEASURE( 1.000000000000000082E-05 ), #69919, 'distance_accuracy_value', 'NONE');
#90383 = CARTESIAN_POINT ( 'NONE',  ( -45.99999999999999289, 436.0213184034681717, 14.35141020368342879 ) ) ;
#90384 = CARTESIAN_POINT ( 'NONE',  ( -8.449011944071282088, -59.99999999999999289, 39.63593633568572017 ) ) ;
#90385 = AXIS2_PLACEMENT_3D ( 'NONE', #9356, #44414, #51425 ) ;
#90386 = AXIS2_PLACEMENT_3D ( 'NONE', #61235, #94119, #61780 ) ;
#90387 = CARTESIAN_POINT ( 'NONE',  ( -32.22120753352784561, 464.6691781026584636, 10.60621122532581140 ) ) ;
#90388 = CARTESIAN_POINT ( 'NONE',  ( 5.974456367264334036E-20, 45.30391365246044444, -18.75000000000000355 ) ) ;
#90389 = CONICAL_SURFACE ( 'NONE', #43893, 3.309500000000007880, 0.9599310885968770357 ) ;
#90390 = CARTESIAN_POINT ( 'NONE',  ( -87.22177126902033706, -35.38517059622223115, 188.6312149666980531 ) ) ;
#90391 = VERTEX_POINT ( 'NONE', #2801 ) ;
#90392 = CARTESIAN_POINT ( 'NONE',  ( 19.48979057729710718, 49.99890399319816936, 60.12824249908596386 ) ) ;
#90393 = DIRECTION ( 'NONE',  ( 1.000000000000000000, 1.224606353822377258E-16, 0.000000000000000000 ) ) ;
#90394 = CARTESIAN_POINT ( 'NONE',  ( -7.280080666583438997, -60.36582059539835399, 33.94095750819536761 ) ) ;
#90395 = EDGE_CURVE ( 'NONE', #34804, #32781, #104987, .T. ) ;
#90396 = EDGE_CURVE ( 'NONE', #7054, #6978, #38046, .T. ) ;
#90397 = PRESENTATION_LAYER_ASSIGNMENT (  '', '', ( #69778 ) ) ;
#90398 = CARTESIAN_POINT ( 'NONE',  ( 12.61650669486618881, -3.851859888774471706E-31, 4.000000000000000888 ) ) ;
#90400 = CARTESIAN_POINT ( 'NONE',  ( 4.004501244502223223, -67.47611191202615544, 13.13598341573225703 ) ) ;
#90399 = CARTESIAN_POINT ( 'NONE',  ( -97.47674776263787066, -60.00000000000000000, 196.6139650356533934 ) ) ;
#90401 = VERTEX_POINT ( 'NONE', #82399 ) ;
#90402 = CARTESIAN_POINT ( 'NONE',  ( 0.000000000000000000, 0.000000000000000000, 0.000000000000000000 ) ) ;
#90403 = CARTESIAN_POINT ( 'NONE',  ( -6.617039711671010238, -4.368567403894508594, -16.80329192430648888 ) ) ;
#90404 = CARTESIAN_POINT ( 'NONE',  ( -7.743982712349856357, 33.46213014760736826, 2.020119794285908377 ) ) ;
#90405 = CARTESIAN_POINT ( 'NONE',  ( 29.43919633169317862, 307.1812765748473453, -9.021906422362246047 ) ) ;
#90406 = CARTESIAN_POINT ( 'NONE',  ( 4.448407490268952991, -48.03096409756968654, 102.6871849564181218 ) ) ;
#90407 = CARTESIAN_POINT ( 'NONE',  ( -6.944371705245973025, -84.46100308575455529, -3.972324460300566962 ) ) ;
#90408 = FACE_OUTER_BOUND ( 'NONE', #6196, .T. ) ;
#90409 = CARTESIAN_POINT ( 'NONE',  ( 106.7878191156923293, -14.21045842199435150, 165.8358245669431597 ) ) ;
#90410 = CARTESIAN_POINT ( 'NONE',  ( 11.08349330513380160, 1.593028355512270567E-15, 0.000000000000000000 ) ) ;
#90411 = ORIENTED_EDGE ( 'NONE', *, *, #25850, .F. ) ;
#90412 = LINE ( 'NONE', #16515, #77469 ) ;
#90413 = CARTESIAN_POINT ( 'NONE',  ( -9.646032546913161809, 253.0128032847436828, 2.644051433538248119 ) ) ;
#90414 =( NAMED_UNIT ( * ) PLANE_ANGLE_UNIT ( ) SI_UNIT ( $, .RADIAN. ) );
#90415 = CARTESIAN_POINT ( 'NONE',  ( -34.25540317603608997, 485.0620278916507573, -1.482526247037498246 ) ) ;
#90416 = CARTESIAN_POINT ( 'NONE',  ( 43.56723210060331297, 370.0879074500739989, 13.88321950767064017 ) ) ;
#90417 = CARTESIAN_POINT ( 'NONE',  ( 43.69871659247140627, 464.4396234996452790, 7.060974336473465840 ) ) ;
#90418 = ORIENTED_EDGE ( 'NONE', *, *, #78918, .T. ) ;
#90419 = UNCERTAINTY_MEASURE_WITH_UNIT (LENGTH_MEASURE( 1.000000000000000082E-05 ), #3003, 'distance_accuracy_value', 'NONE');
#90420 = CARTESIAN_POINT ( 'NONE',  ( -22.09048636024830259, 305.2882331017710840, 9.030984930783928277 ) ) ;
#90421 = ORIENTED_EDGE ( 'NONE', *, *, #2232, .F. ) ;
#90422 = CARTESIAN_POINT ( 'NONE',  ( 35.56870672589202087, 485.2859037185882016, -2.957003582718795709 ) ) ;
#90423 = CIRCLE ( 'NONE', #61186, 4.000000000000001776 ) ;
#90424 =( NAMED_UNIT ( * ) PLANE_ANGLE_UNIT ( ) SI_UNIT ( $, .RADIAN. ) );
#90425 = CARTESIAN_POINT ( 'NONE',  ( 9.523267564284003228, 45.61198619316643743, 15.16070064068354739 ) ) ;
#90426 = EDGE_LOOP ( 'NONE', ( #758, #52236 ) ) ;
#90427 = CARTESIAN_POINT ( 'NONE',  ( 52.56483885390522204, 48.00000000000000000, -38.23529411764705799 ) ) ;
#90428 = CARTESIAN_POINT ( 'NONE',  ( 12.61650669486618881, 1.474610560812782335E-15, 0.000000000000000000 ) ) ;
#90429 = CARTESIAN_POINT ( 'NONE',  ( -72.28463938464267358, -59.99999999997559286, 178.7115098145620777 ) ) ;
#90430 = CARTESIAN_POINT ( 'NONE',  ( 43.79026230967847511, 435.5799286522100147, 9.443751109679228151 ) ) ;
#90431 = ORIENTED_EDGE ( 'NONE', *, *, #91599, .T. ) ;
#90432 = CARTESIAN_POINT ( 'NONE',  ( 91.86097484301993177, -60.00000000000001421, 13.21028115448139317 ) ) ;
#90434 = CARTESIAN_POINT ( 'NONE',  ( 17.88298539565740342, -39.47322924647534848, 30.78448731433081420 ) ) ;
#90433 = CARTESIAN_POINT ( 'NONE',  ( -106.4855387602377732, -14.21045842199444564, 182.1782270149441558 ) ) ;
#90435 = ADVANCED_FACE ( 'NONE', ( #57568 ), #55971, .F. ) ;
#90436 = CARTESIAN_POINT ( 'NONE',  ( -39.33899073937549673, -42.97721915985697194, 38.92032525959593414 ) ) ;
#90437 = CARTESIAN_POINT ( 'NONE',  ( 11.89131030317610183, 3.851859888774471706E-31, 5.000000000000001776 ) ) ;
#90438 = ORIENTED_EDGE ( 'NONE', *, *, #91691, .T. ) ;
#90439 = FILL_AREA_STYLE_COLOUR ( '', #18589 ) ;
#90440 = CARTESIAN_POINT ( 'NONE',  ( 16.10103474921838540, 21.87197452378524787, -0.4486278773448218460 ) ) ;
#90441 = CARTESIAN_POINT ( 'NONE',  ( 19.70764564238371719, 304.7954121406193622, 9.925013215726785631 ) ) ;
#90442 = CARTESIAN_POINT ( 'NONE',  ( 0.000000000000000000, 5.629165124598842773, -3.250000000000011990 ) ) ;
#90443 = CARTESIAN_POINT ( 'NONE',  ( -8.000000000000000000, -28.53125000409677270, -3.313708498984762496 ) ) ;
#90444 = CARTESIAN_POINT ( 'NONE',  ( -32.07049714173062682, 486.4381577779643635, 6.103659696309225779 ) ) ;
#90445 = ORIENTED_EDGE ( 'NONE', *, *, #68960, .T. ) ;
#90446 = B_SPLINE_CURVE_WITH_KNOTS ( 'NONE', 3,
 ( #10299, #76626, #58876, #100375, #43738, #52896, #92818, #101452, #91768, #3286, #17890, #28129 ),
 .UNSPECIFIED., .F., .F.,
 ( 4, 2, 2, 2, 2, 4 ),
 ( 0.0005290297149009433276, 0.001465496285715521931, 0.002401962856530100426, 0.003338429427344679137, 0.003806662712751983455, 0.004274895998159287773 ),
 .UNSPECIFIED. ) ;
#90447 = ORIENTED_EDGE ( 'NONE', *, *, #42902, .T. ) ;
#90448 = CARTESIAN_POINT ( 'NONE',  ( 77.53488771745220731, -30.00000000000000711, -16.24820434784860979 ) ) ;
#90449 = CARTESIAN_POINT ( 'NONE',  ( 47.18533784750991344, 13.30762177597463847, 14.68117529621389750 ) ) ;
#90450 = UNCERTAINTY_MEASURE_WITH_UNIT (LENGTH_MEASURE( 1.000000000000000082E-05 ), #54479, 'distance_accuracy_value', 'NONE');
#90451 = CARTESIAN_POINT ( 'NONE',  ( 13.50000000000000533, -7.794228634059977345, -1.205771365940065953 ) ) ;
#90452 = LINE ( 'NONE', #16564, #3245 ) ;
#90453 = CARTESIAN_POINT ( 'NONE',  ( 98.41709237619858186, -30.00000000000000000, 140.5531095731581956 ) ) ;
#90454 = CARTESIAN_POINT ( 'NONE',  ( 29.08076923076923137, 1.411358822780289120E-15, 0.000000000000000000 ) ) ;
#90455 = ORIENTED_EDGE ( 'NONE', *, *, #67903, .T. ) ;
#90456 = ORIENTED_EDGE ( 'NONE', *, *, #36004, .T. ) ;
#90457 = ORIENTED_EDGE ( 'NONE', *, *, #66887, .F. ) ;
#90458 = DIRECTION ( 'NONE',  ( -1.000000000000000000, -0.000000000000000000, -0.000000000000000000 ) ) ;
#90459 = CARTESIAN_POINT ( 'NONE',  ( 23.21751746555303342, 25.25267828308493989, 33.20617127781017075 ) ) ;
#90460 = TOROIDAL_SURFACE ( 'NONE', #105910, 10.00000000000000000, 5.000000000000000000 ) ;
#90461 = CARTESIAN_POINT ( 'NONE',  ( -42.20540931547580499, 464.9254549434357386, 14.73500713293301168 ) ) ;
#90462 = ORIENTED_EDGE ( 'NONE', *, *, #56368, .T. ) ;
#90463 = CARTESIAN_POINT ( 'NONE',  ( 42.55949806392587931, 435.1558328882682645, 18.91815692826296313 ) ) ;
#90464 = VERTEX_POINT ( 'NONE', #24721 ) ;
#90465 = CARTESIAN_POINT ( 'NONE',  ( 40.34715123528543046, 1.340359594676612611E-15, 0.000000000000000000 ) ) ;
#90466 = CARTESIAN_POINT ( 'NONE',  ( 84.35232594345727364, -38.74306589926045774, 198.0791177174846496 ) ) ;
#90467 = CARTESIAN_POINT ( 'NONE',  ( 32.39363610230712709, 435.1530561269337909, 14.92612657118719888 ) ) ;
#90468 = PRESENTATION_LAYER_ASSIGNMENT (  '', '', ( #30187 ) ) ;
#90469 = CARTESIAN_POINT ( 'NONE',  ( 35.43884268025067286, 303.9034792765622797, 4.025496658314922094 ) ) ;
#90470 = COLOUR_RGB ( '', 0.66274510, 0.83137255, 0.94901961) ;
#90471 = CARTESIAN_POINT ( 'NONE',  ( 44.45120377230470865, 484.8901964262618094, 4.471885531210140208 ) ) ;
#90472 = AXIS2_PLACEMENT_3D ( 'NONE', #50325, #65990, #91861 ) ;
#90473 = ADVANCED_FACE ( 'NONE', ( #73766 ), #91044, .T. ) ;
#90474 = CARTESIAN_POINT ( 'NONE',  ( 0.000000000000000000, -5.629165124598850767, -3.249999999999999556 ) ) ;
#90475 = VECTOR ( 'NONE', #55517, 1000.000000000000000 ) ;
#90476 = AXIS2_PLACEMENT_3D ( 'NONE', #100304, #17814, #58805 ) ;
#90477 = DIRECTION ( 'NONE',  ( -1.000000000000000000, -1.224606353822377258E-16, -0.000000000000000000 ) ) ;
#90478 = CARTESIAN_POINT ( 'NONE',  ( -4.680975426248548565, -47.58422982932144407, 103.4780497728483368 ) ) ;
#90479 = CARTESIAN_POINT ( 'NONE',  ( 33.00540147335379260, 487.4196752801331627, 9.523982417622169905 ) ) ;
#90480 = CARTESIAN_POINT ( 'NONE',  ( -4.404139836249539641, 10.09840216323677708, 5.000000000000000888 ) ) ;
#90481 = EDGE_LOOP ( 'NONE', ( #85056, #42755, #92037 ) ) ;
#90482 = CARTESIAN_POINT ( 'NONE',  ( 6.644028492724104673, 7.802520252160765502, -5.627655413974009852E-13 ) ) ;
#90483 = CARTESIAN_POINT ( 'NONE',  ( -28.52151309506147925, 297.0551483322281570, 2.417936164087576945 ) ) ;
#90484 = CARTESIAN_POINT ( 'NONE',  ( 0.000000000000000000, -4.000000000000003553, 119.0000000000000142 ) ) ;
#90485 = UNCERTAINTY_MEASURE_WITH_UNIT (LENGTH_MEASURE( 1.000000000000000082E-05 ), #54746, 'distance_accuracy_value', 'NONE');
#90486 =( NAMED_UNIT ( * ) PLANE_ANGLE_UNIT ( ) SI_UNIT ( $, .RADIAN. ) );
#90487 = CARTESIAN_POINT ( 'NONE',  ( 8.000000000000000000, -10.90624999999999112, -3.313708498984761608 ) ) ;
#90488 = CARTESIAN_POINT ( 'NONE',  ( 2.333519804815400889, -18.10848410825153110, 35.01514424201566555 ) ) ;
#90489 = CARTESIAN_POINT ( 'NONE',  ( 5.720759824257057424, 297.8120955430345589, 8.219233466110658526 ) ) ;
#90490 = SURFACE_STYLE_USAGE ( .BOTH. , #88897 ) ;
#90491 = ORIENTED_EDGE ( 'NONE', *, *, #17687, .F. ) ;
#90492 = CARTESIAN_POINT ( 'NONE',  ( 85.31123991943051976, -46.55852039550524779, 188.2316344986979004 ) ) ;
#90493 = FILL_AREA_STYLE_COLOUR ( '', #44655 ) ;
#90494 = CARTESIAN_POINT ( 'NONE',  ( -9.291504855474395086, 140.5441818688510693, 6.367976583174694128E-13 ) ) ;
#90495 = ORIENTED_EDGE ( 'NONE', *, *, #21149, .F. ) ;
#90496 = CARTESIAN_POINT ( 'NONE',  ( 94.51265451826158426, -57.66905794854115186, -1.775134423264453698 ) ) ;
#90497 = DIRECTION ( 'NONE',  ( 0.000000000000000000, 0.000000000000000000, 1.000000000000000000 ) ) ;
#90498 = CARTESIAN_POINT ( 'NONE',  ( 29.27049653814518848, 13.57913911089070780, 39.67351191892522877 ) ) ;
#90499 = VECTOR ( 'NONE', #66484, 1000.000000000000114 ) ;
#90500 = CARTESIAN_POINT ( 'NONE',  ( -81.59220867401275257, -30.00000000000000355, -7.144273055932939265 ) ) ;
#90501 = CARTESIAN_POINT ( 'NONE',  ( -61.30120358801738689, -38.00000000000001421, 74.93692602774881095 ) ) ;
#90502 = LINE ( 'NONE', #74308, #3208 ) ;
#90503 = DIRECTION ( 'NONE',  ( 0.000000000000000000, -1.000000000000000000, 0.000000000000000000 ) ) ;
#90505 = CARTESIAN_POINT ( 'NONE',  ( -32.90756164719182664, 485.1133553471440791, 5.490574211026766349 ) ) ;
#90504 =( LENGTH_UNIT ( ) NAMED_UNIT ( * ) SI_UNIT ( .MILLI., .METRE. ) );
#90506 = CARTESIAN_POINT ( 'NONE',  ( 0.000000000000000000, 0.000000000000000000, -0.02540000000000007530 ) ) ;
#90507 = CARTESIAN_POINT ( 'NONE',  ( -28.77727207546517363, 18.82954237789026308, 39.99083609194100575 ) ) ;
#90508 = FACE_OUTER_BOUND ( 'NONE', #75362, .T. ) ;
#90509 = CARTESIAN_POINT ( 'NONE',  ( -34.47211195129267480, 489.5752767497882587, 11.69752549375507655 ) ) ;
#90510 = CARTESIAN_POINT ( 'NONE',  ( -22.20476351154805172, 26.05629838265183906, 31.21875911480587718 ) ) ;
#90511 = CARTESIAN_POINT ( 'NONE',  ( 32.82691535583472842, 485.1045372766795367, 1.724905475515025266 ) ) ;
#90512 = VECTOR ( 'NONE', #44899, 1000.000000000000000 ) ;
#90513 = ORIENTED_EDGE ( 'NONE', *, *, #99726, .F. ) ;
#90514 = CARTESIAN_POINT ( 'NONE',  ( 6.445370176741570312, -4.584736124523163703, -5.738941594273955893 ) ) ;
#90515 = DIRECTION ( 'NONE',  ( 0.000000000000000000, 1.000000000000000000, 0.000000000000000000 ) ) ;
#90516 = CARTESIAN_POINT ( 'NONE',  ( -7.897196874019794421, 81.20872795832194413, -1.302055520192082705 ) ) ;
#90517 = EDGE_CURVE ( 'NONE', #13955, #80654, #102388, .T. ) ;
#90518 = CARTESIAN_POINT ( 'NONE',  ( 0.000000000000000000, 0.000000000000000000, 0.000000000000000000 ) ) ;
#90519 = ADVANCED_FACE ( 'NONE', ( #103626 ), #31747, .T. ) ;
#90521 = CARTESIAN_POINT ( 'NONE',  ( -73.58024007755891205, -60.22810801993039576, -24.87566229692106390 ) ) ;
#90520 = DIRECTION ( 'NONE',  ( 0.000000000000000000, -1.000000000000000000, 0.000000000000000000 ) ) ;
#90522 = AXIS2_PLACEMENT_3D ( 'NONE', #89543, #99750, #99202 ) ;
#90523 = VERTEX_POINT ( 'NONE', #50024 ) ;
#90524 = ORIENTED_EDGE ( 'NONE', *, *, #38007, .F. ) ;
#90525 = CARTESIAN_POINT ( 'NONE',  ( -27.10511071441183262, 34.47735702144344572, 10.05698433968616001 ) ) ;
#90526 =( GEOMETRIC_REPRESENTATION_CONTEXT ( 3 ) GLOBAL_UNCERTAINTY_ASSIGNED_CONTEXT ( ( #21116 ) ) GLOBAL_UNIT_ASSIGNED_CONTEXT ( ( #29470, #28400, #38088 ) ) REPRESENTATION_CONTEXT ( 'NONE', 'WORKASPACE' ) );
#90527 = CARTESIAN_POINT ( 'NONE',  ( 10.28624191511809371, 43.99263840937192782, -12.90779740156171407 ) ) ;
#90528 = PRESENTATION_STYLE_ASSIGNMENT (( #9065 ) ) ;
#90529 = AXIS2_PLACEMENT_3D ( 'NONE', #21456, #53274, #85651 ) ;
#90530 = CARTESIAN_POINT ( 'NONE',  ( -33.44424537694998634, -59.99999999999999289, -40.50270220663588105 ) ) ;
#90531 = EDGE_LOOP ( 'NONE', ( #15217, #44226 ) ) ;
#90532 = DIRECTION ( 'NONE',  ( 1.000000000000000000, 0.000000000000000000, 0.000000000000000000 ) ) ;
#90533 = CIRCLE ( 'NONE', #25119, 4.172000000000009479 ) ;
#90534 = CARTESIAN_POINT ( 'NONE',  ( -9.730604568514243269, 294.6502803634054999, -2.323175618299882395 ) ) ;
#90535 = CIRCLE ( 'NONE', #9596, 4.000000000000001776 ) ;
#90536 = CARTESIAN_POINT ( 'NONE',  ( 96.46995715361335044, -52.82112724768406053, 195.4050685382941595 ) ) ;
#90537 = STYLED_ITEM ( 'NONE', ( #30877 ), #35733 ) ;
#90539 = DIRECTION ( 'NONE',  ( 0.000000000000000000, 1.000000000000000000, 0.000000000000000000 ) ) ;
#90538 = SURFACE_STYLE_USAGE ( .BOTH. , #47408 ) ;
#90540 = ORIENTED_EDGE ( 'NONE', *, *, #93433, .F. ) ;
#90541 = ORIENTED_EDGE ( 'NONE', *, *, #96554, .T. ) ;
#90542 = VECTOR ( 'NONE', #34688, 1000.000000000000000 ) ;
#90543 = VERTEX_POINT ( 'NONE', #8502 ) ;
#90544 = CARTESIAN_POINT ( 'NONE',  ( 32.13660303513785976, 374.7216330957919013, 24.09117032669768932 ) ) ;
#90545 = CARTESIAN_POINT ( 'NONE',  ( -5.000000000000000000, -13.83542193917759633, 11.07282995724388286 ) ) ;
#90546 = CARTESIAN_POINT ( 'NONE',  ( 15.51806636169577658, 46.21009754484516208, 4.857304170327764403 ) ) ;
#90547 = ORIENTED_EDGE ( 'NONE', *, *, #82861, .F. ) ;
#90548 = CARTESIAN_POINT ( 'NONE',  ( -42.57704743493911081, 486.1612337113410263, 7.852296464539654686 ) ) ;
#90549 = DIRECTION ( 'NONE',  ( -0.000000000000000000, -0.000000000000000000, 1.000000000000000000 ) ) ;
#90550 = CARTESIAN_POINT ( 'NONE',  ( -30.00000000000000000, -54.00000000000000711, 27.11721482942554928 ) ) ;
#90551 = CARTESIAN_POINT ( 'NONE',  ( -15.40724846713353813, -57.67135988443339301, 41.78154393163084279 ) ) ;
#90552 = CARTESIAN_POINT ( 'NONE',  ( -5.082755093536326818, -28.71875000204838813, 5.082755093536325042 ) ) ;
#90553 = CARTESIAN_POINT ( 'NONE',  ( 80.40000000000000568, 1.023464760207051730E-14, 0.000000000000000000 ) ) ;
#90554 = CARTESIAN_POINT ( 'NONE',  ( -0.3342441623883664614, 25.18324729327973444, 40.70740451072503419 ) ) ;
#90555 = CARTESIAN_POINT ( 'NONE',  ( 0.7781286854980117296, 27.39149973645235647, -40.48175932167306001 ) ) ;
#90556 = CARTESIAN_POINT ( 'NONE',  ( 24.50706706878033359, -14.21045842199442077, -36.19515235953155496 ) ) ;
#90557 = CARTESIAN_POINT ( 'NONE',  ( -1.363517047694020823, -14.21045842199434794, 34.36840973699905533 ) ) ;
#90558 = EDGE_CURVE ( 'NONE', #47418, #34348, #23661, .T. ) ;
#90559 = CARTESIAN_POINT ( 'NONE',  ( -51.69204177676629541, -60.31069149989181000, 61.32316516767149039 ) ) ;
#90560 = FACE_OUTER_BOUND ( 'NONE', #73797, .T. ) ;
#90561 = ORIENTED_EDGE ( 'NONE', *, *, #17773, .F. ) ;
#90562 = CARTESIAN_POINT ( 'NONE',  ( -98.44269825977914934, -37.74221500662412865, 192.2764363897139219 ) ) ;
#90563 = CARTESIAN_POINT ( 'NONE',  ( -1.798224084866679950, 298.0247695552619689, -10.00218504963178567 ) ) ;
#90564 = CARTESIAN_POINT ( 'NONE',  ( 15.88393779855022281, -1.939575830182636684, 14.87604252415763106 ) ) ;
#90565 = ORIENTED_EDGE ( 'NONE', *, *, #33609, .F. ) ;
#90566 = CARTESIAN_POINT ( 'NONE',  ( -17.26387333831402060, 43.28639006945349621, 6.496095472997780007 ) ) ;
#90567 = CARTESIAN_POINT ( 'NONE',  ( 72.31813523599501536, -38.32585783385900413, 147.7857233425339132 ) ) ;
#90568 = CARTESIAN_POINT ( 'NONE',  ( 28.09999999999999787, 3.309500000000003439, 0.000000000000000000 ) ) ;
#90569 = CARTESIAN_POINT ( 'NONE',  ( 89.64643850830432825, 1.030564683017419500E-14, 0.000000000000000000 ) ) ;
#90570 = CARTESIAN_POINT ( 'NONE',  ( 81.26467260280679739, 1.016364837396684119E-14, 0.000000000000000000 ) ) ;
#90571 = CIRCLE ( 'NONE', #4420, 6.500000000000000888 ) ;
#90572 = SURFACE_STYLE_FILL_AREA ( #43091 ) ;
#90574 = CARTESIAN_POINT ( 'NONE',  ( 85.25619601544318016, -29.99999999999999645, 172.6969293775904077 ) ) ;
#90573 = UNCERTAINTY_MEASURE_WITH_UNIT (LENGTH_MEASURE( 1.000000000000000082E-05 ), #100043, 'distance_accuracy_value', 'NONE');
#90575 = CARTESIAN_POINT ( 'NONE',  ( 37.62595466100196262, 491.2446780561975856, 12.18850516984599786 ) ) ;
#90576 = ADVANCED_FACE ( 'NONE', ( #56513 ), #89442, .F. ) ;
#90577 = CARTESIAN_POINT ( 'NONE',  ( -32.12958771267418712, 464.7275665249413805, 11.12424126545828784 ) ) ;
#90578 = EDGE_CURVE ( 'NONE', #67063, #3603, #75236, .T. ) ;
#90579 = CARTESIAN_POINT ( 'NONE',  ( -34.42195163688415960, 484.1350747783264410, 0.1342865971146420812 ) ) ;
#90580 = ORIENTED_EDGE ( 'NONE', *, *, #66819, .F. ) ;
#90581 = VERTEX_POINT ( 'NONE', #76423 ) ;
#90582 = CARTESIAN_POINT ( 'NONE',  ( 52.65259415171738766, -46.43731922596889206, 58.09906300711125482 ) ) ;
#90583 = CARTESIAN_POINT ( 'NONE',  ( -8.844479576175121593, 302.6213365498747407, -10.03676384835056723 ) ) ;
#90584 = MANIFOLD_SOLID_BREP ( 'ThdSchPat', #51464 ) ;
#90585 = CARTESIAN_POINT ( 'NONE',  ( 36.59027416739721872, 27.99615698493870397, -12.99074957500551086 ) ) ;
#90586 = VERTEX_POINT ( 'NONE', #83996 ) ;
#90587 = CARTESIAN_POINT ( 'NONE',  ( -92.83006309950484081, -38.35493895758955318, 42.01425766727841449 ) ) ;
#90588 = VERTEX_POINT ( 'NONE', #93155 ) ;
#90589 = CARTESIAN_POINT ( 'NONE',  ( 28.35825693584814644, 34.17671750055550461, -8.950286295360427857 ) ) ;
#90590 = CARTESIAN_POINT ( 'NONE',  ( 90.85051015719332668, -38.35148808657510955, 20.42926060149419243 ) ) ;
#90591 = CARTESIAN_POINT ( 'NONE',  ( 13.68200042800751426, 22.81115111118363004, 2.014803622706606845 ) ) ;
#90592 = CARTESIAN_POINT ( 'NONE',  ( 96.80527538515720209, -45.28275837559359474, 111.1125581287882227 ) ) ;
#90593 = DIRECTION ( 'NONE',  ( 0.000000000000000000, -0.000000000000000000, 1.000000000000000000 ) ) ;
#90594 = PRESENTATION_STYLE_ASSIGNMENT (( #16164 ) ) ;
#90595 = CARTESIAN_POINT ( 'NONE',  ( -35.11084318070448518, 353.0208097076877607, 2.079257881123132812 ) ) ;
#90596 = CARTESIAN_POINT ( 'NONE',  ( 1.797535115058627619, -69.58639455773389670, 12.85324246208445587 ) ) ;
#90597 = CARTESIAN_POINT ( 'NONE',  ( 74.84954895605289948, -60.00000000000000000, 180.1045722148651862 ) ) ;
#90598 = EDGE_CURVE ( 'NONE', #44553, #58472, #57277, .T. ) ;
#90599 = CONICAL_SURFACE ( 'NONE', #87217, 4.000000000000001776, 0.9599310885968808105 ) ;
#90600 = DIRECTION ( 'NONE',  ( 0.000000000000000000, 1.000000000000000000, 0.000000000000000000 ) ) ;
#90601 = ORIENTED_EDGE ( 'NONE', *, *, #45674, .F. ) ;
#90602 = CARTESIAN_POINT ( 'NONE',  ( 62.08318622917204266, -25.58606428081736439, 71.03334541717022432 ) ) ;
#90603 = EDGE_CURVE ( 'NONE', #31791, #61442, #11148, .T. ) ;
#90604 = CARTESIAN_POINT ( 'NONE',  ( -26.11633329837163942, 295.8773401828905207, -9.779540871743899189 ) ) ;
#90605 = CARTESIAN_POINT ( 'NONE',  ( 9.113097280746996987, -54.00000000000000711, 31.11721482942554928 ) ) ;
#90606 = STYLED_ITEM ( 'NONE', ( #95407 ), #63990 ) ;
#90607 = CARTESIAN_POINT ( 'NONE',  ( -8.817541433524096917, -5.000000000000000000, -16.91981367016228788 ) ) ;
#90609 = CARTESIAN_POINT ( 'NONE',  ( 12.61650669486618881, 4.000000000000003553, 4.898587196589414801E-16 ) ) ;
#90608 = CARTESIAN_POINT ( 'NONE',  ( -90.56781767776030279, -38.40338341477720974, -14.35555322263740585 ) ) ;
#90610 = CARTESIAN_POINT ( 'NONE',  ( -33.15912019476756001, 406.2462808298095069, 25.90171796155655670 ) ) ;
#90611 = CARTESIAN_POINT ( 'NONE',  ( 91.09088295274877112, 1.030564683017419500E-14, 0.000000000000000000 ) ) ;
#90612 = CARTESIAN_POINT ( 'NONE',  ( 92.53532739719321398, 1.030564683017419500E-14, 0.000000000000000000 ) ) ;
#90613 = CARTESIAN_POINT ( 'NONE',  ( 7.999999999999998224, -26.09374999999999289, 3.313708498984766493 ) ) ;
#90614 = AXIS2_PLACEMENT_3D ( 'NONE', #35338, #16053, #52005 ) ;
#90615 = CARTESIAN_POINT ( 'NONE',  ( -17.49999999999996447, 44.85000000000000853, 62.61746187599676716 ) ) ;
#90616 = EDGE_CURVE ( 'NONE', #97678, #63571, #106605, .T. ) ;
#90617 = AXIS2_PLACEMENT_3D ( 'NONE', #18854, #26945, #43093 ) ;
#90618 = AXIS2_PLACEMENT_3D ( 'NONE', #98791, #26561, #73992 ) ;
#90619 = AXIS2_PLACEMENT_3D ( 'NONE', #572, #99293, #8174 ) ;
#90620 = AXIS2_PLACEMENT_3D ( 'NONE', #33127, #8285, #16377 ) ;
#90621 = EDGE_LOOP ( 'NONE', ( #16149, #96849, #35379 ) ) ;
#90622 = CARTESIAN_POINT ( 'NONE',  ( 85.50308900661609357, -25.30960514552327112, 172.5786385089847386 ) ) ;
#90623 = CARTESIAN_POINT ( 'NONE',  ( 43.46689911038831156, 485.4921130118007113, 4.095024577346795702 ) ) ;
#90624 = CARTESIAN_POINT ( 'NONE',  ( -41.71452336584287934, 436.0710517509322131, 20.70662328852571576 ) ) ;
#90625 = VERTEX_POINT ( 'NONE', #84539 ) ;
#90626 = DIRECTION ( 'NONE',  ( 0.000000000000000000, 0.000000000000000000, 1.000000000000000000 ) ) ;
#90627 = ADVANCED_FACE ( 'NONE', ( #43543 ), #3371, .T. ) ;
#90628 = LINE ( 'NONE', #16733, #23503 ) ;
#90629 = CARTESIAN_POINT ( 'NONE',  ( -32.91521444485699277, 465.6822365171608453, 10.74527606630527110 ) ) ;
#90630 = SURFACE_SIDE_STYLE ('',( #23800 ) ) ;
#90631 = CIRCLE ( 'NONE', #99228, 7.000000000000000000 ) ;
#90632 = CARTESIAN_POINT ( 'NONE',  ( -28.43946827300288049, 12.73388556380908376, -40.70676336658363681 ) ) ;
#90633 = FACE_OUTER_BOUND ( 'NONE', #96776, .T. ) ;
#90634 = DIRECTION ( 'NONE',  ( -1.000000000000000000, -1.224606353822377258E-16, -0.000000000000000000 ) ) ;
#90636 = CARTESIAN_POINT ( 'NONE',  ( -14.97914546934171653, 22.21797506316305615, 3.886805437593018553 ) ) ;
#90635 = CARTESIAN_POINT ( 'NONE',  ( -22.05550015032907041, -27.05256809874309099, 37.35158853590624517 ) ) ;
#90637 = CARTESIAN_POINT ( 'NONE',  ( 5.082755093536325930, -12.96875000204838280, -5.082755093536325042 ) ) ;
#90638 = CARTESIAN_POINT ( 'NONE',  ( -9.165151389911679658, 104.9999999999999858, -4.000000000000001776 ) ) ;
#90639 = PLANE ( 'NONE',  #44887 ) ;
#90640 = ORIENTED_EDGE ( 'NONE', *, *, #29535, .T. ) ;
#90641 = VECTOR ( 'NONE', #25177, 1000.000000000000000 ) ;
#90642 = CARTESIAN_POINT ( 'NONE',  ( -18.92174722983623525, 48.90933038776066155, 62.13887004286765858 ) ) ;
#90643 = CARTESIAN_POINT ( 'NONE',  ( 23.54609889741162121, 25.19605094436382231, 33.16507022216291034 ) ) ;
#90644 = VECTOR ( 'NONE', #86485, 1000.000000000000000 ) ;
#90645 = CARTESIAN_POINT ( 'NONE',  ( 36.87655955837855970, 438.2068510013162950, 3.933030107424718924 ) ) ;
#90646 = DIRECTION ( 'NONE',  ( -0.000000000000000000, -0.000000000000000000, 1.000000000000000000 ) ) ;
#90647 = EDGE_CURVE ( 'NONE', #24844, #70018, #92899, .T. ) ;
#90649 = CARTESIAN_POINT ( 'NONE',  ( 49.54707403498029805, -21.77003194717852352, -25.65727647574667714 ) ) ;
#90648 = DIRECTION ( 'NONE',  ( -1.000000000000000000, -1.224606353822377258E-16, -0.000000000000000000 ) ) ;
#90650 = ORIENTED_EDGE ( 'NONE', *, *, #6744, .T. ) ;
#90651 = CARTESIAN_POINT ( 'NONE',  ( -5.728413875956868573, -88.58064226453400636, 1.802282772585248605 ) ) ;
#90652 = CARTESIAN_POINT ( 'NONE',  ( -4.961791431619821502, 52.14601839267029249, 6.072164406264656478 ) ) ;
#90653 = ORIENTED_EDGE ( 'NONE', *, *, #59475, .T. ) ;
#90654 = EDGE_CURVE ( 'NONE', #70575, #100942, #34221, .T. ) ;
#90655 = CARTESIAN_POINT ( 'NONE',  ( 36.84999999999999432, -3.309499999999999886, 4.475777889183790779E-16 ) ) ;
#90656 = DIRECTION ( 'NONE',  ( 0.000000000000000000, 0.000000000000000000, 1.000000000000000000 ) ) ;
#90657 = CARTESIAN_POINT ( 'NONE',  ( -21.47524434066147947, 41.77809834471024431, -77.71550088237076181 ) ) ;
#90658 = CARTESIAN_POINT ( 'NONE',  ( -95.68557296049533534, -59.99999999999999289, 53.88884937414592002 ) ) ;
#90659 = CARTESIAN_POINT ( 'NONE',  ( 28.94969860575612230, 18.87958371857671835, -39.84024749387450015 ) ) ;
#90660 = CYLINDRICAL_SURFACE ( 'NONE', #43659, 5.000000000000002665 ) ;
#90661 = LINE ( 'NONE', #50195, #77901 ) ;
#90662 = DIRECTION ( 'NONE',  ( -1.000000000000000000, -1.224606353822377258E-16, -0.000000000000000000 ) ) ;
#90664 = CARTESIAN_POINT ( 'NONE',  ( -15.35634750254357428, 2.988828671322287800, 2.785065577037467488 ) ) ;
#90663 = CARTESIAN_POINT ( 'NONE',  ( -10.48543666094732352, -5.000000000000002665, -78.95657223722187723 ) ) ;
#90665 = CARTESIAN_POINT ( 'NONE',  ( -84.11688277119964141, -32.48829956650884299, 169.3662770803418027 ) ) ;
#90667 = CIRCLE ( 'NONE', #52791, 4.000000000000000000 ) ;
#90666 = B_SPLINE_CURVE_WITH_KNOTS ( 'NONE', 3,
 ( #28908, #61784, #14242, #47150 ),
 .UNSPECIFIED., .F., .F.,
 ( 4, 4 ),
 ( 0.000000000000000000, 0.0002045283294076029920 ),
 .UNSPECIFIED. ) ;
#90668 = ORIENTED_EDGE ( 'NONE', *, *, #80996, .F. ) ;
#90669 = SURFACE_SIDE_STYLE ('',( #55613 ) ) ;
#90670 = ORIENTED_EDGE ( 'NONE', *, *, #56144, .F. ) ;
#90671 = ORIENTED_EDGE ( 'NONE', *, *, #93629, .F. ) ;
#90672 = CYLINDRICAL_SURFACE ( 'NONE', #4389, 9.000000000000000000 ) ;
#90673 = EDGE_CURVE ( 'NONE', #38824, #50441, #67130, .T. ) ;
#90675 = DIRECTION ( 'NONE',  ( 0.000000000000000000, 0.000000000000000000, -1.000000000000000000 ) ) ;
#90674 = AXIS2_PLACEMENT_3D ( 'NONE', #51498, #67168, #9426 ) ;
#90676 = ORIENTED_EDGE ( 'NONE', *, *, #5155, .F. ) ;
#90677 = DIRECTION ( 'NONE',  ( 0.000000000000000000, 0.000000000000000000, 1.000000000000000000 ) ) ;
#90678 = CYLINDRICAL_SURFACE ( 'NONE', #85746, 1.000000000000000888 ) ;
#90679 = CARTESIAN_POINT ( 'NONE',  ( 57.45015997180046696, 6.975173280561618775E-15, 0.000000000000000000 ) ) ;
#90680 = CARTESIAN_POINT ( 'NONE',  ( -7.934996450857313199, -61.13137543527469830, -1.050865690281778120 ) ) ;
#90681 = PRESENTATION_LAYER_ASSIGNMENT (  '', '', ( #44195 ) ) ;
#90682 = CARTESIAN_POINT ( 'NONE',  ( -1.009236793202067828, 54.10523466797827297, 8.245009025653098789 ) ) ;
#90683 = CYLINDRICAL_SURFACE ( 'NONE', #98504, 35.82893434829263413 ) ;
#90684 = CARTESIAN_POINT ( 'NONE',  ( 106.2140667560022536, -14.21045842199435860, 184.2067176257025380 ) ) ;
#90685 = CARTESIAN_POINT ( 'NONE',  ( -111.5324017304388207, -60.00000000000003553, 193.8614060841614730 ) ) ;
#90686 = EDGE_CURVE ( 'NONE', #66543, #20623, #84378, .T. ) ;
#90687 = CARTESIAN_POINT ( 'NONE',  ( -62.08384294452462626, -25.58717909351559072, 71.03563272662908901 ) ) ;
#90688 = ORIENTED_EDGE ( 'NONE', *, *, #72104, .F. ) ;
#90689 = CARTESIAN_POINT ( 'NONE',  ( 54.95211584722589748, 38.95432885569419312, -32.68840303539023040 ) ) ;
#90690 = CARTESIAN_POINT ( 'NONE',  ( 94.50843613628299522, -59.99999999999023714, -13.93139703282171382 ) ) ;
#90691 = AXIS2_PLACEMENT_3D ( 'NONE', #4115, #94189, #13774 ) ;
#90693 = ORIENTED_EDGE ( 'NONE', *, *, #97789, .T. ) ;
#90692 = AXIS2_PLACEMENT_3D ( 'NONE', #100371, #25829, #58683 ) ;
#90694 = CARTESIAN_POINT ( 'NONE',  ( 3.009920775786005365, -32.51036453576112706, 29.30336538357065379 ) ) ;
#90695 = CARTESIAN_POINT ( 'NONE',  ( -103.1107698907982666, -52.71038489674184291, 144.4341237230532329 ) ) ;
#90697 = TOROIDAL_SURFACE ( 'NONE', #57962, 12.00000000000001066, 3.000000000000000000 ) ;
#90696 = CARTESIAN_POINT ( 'NONE',  ( 7.188101187499999156, -10.62500000204838813, 2.977408999572654924 ) ) ;
#90698 = ORIENTED_EDGE ( 'NONE', *, *, #3064, .F. ) ;
#90699 = CARTESIAN_POINT ( 'NONE',  ( 7.122964895856751077, -30.00000000000000355, -0.9654893961775683486 ) ) ;
#90700 = VERTEX_POINT ( 'NONE', #53232 ) ;
#90701 = CARTESIAN_POINT ( 'NONE',  ( -5.724587470723463412E-14, -15.58845726811991561, -1.205771365940065953 ) ) ;
#90703 = VECTOR ( 'NONE', #28198, 1000.000000000000000 ) ;
#90702 = CARTESIAN_POINT ( 'NONE',  ( -75.65743859592900833, -59.99999999999997868, 185.4139711062220783 ) ) ;
#90704 =( NAMED_UNIT ( * ) PLANE_ANGLE_UNIT ( ) SI_UNIT ( $, .RADIAN. ) );
#90705 = CARTESIAN_POINT ( 'NONE',  ( -5.082755093536325042, -18.96875000204838457, -5.082755093536325930 ) ) ;
#90706 = CARTESIAN_POINT ( 'NONE',  ( 36.41079454256790626, 485.4442866794557858, -3.629012552425965765 ) ) ;
#90707 = CIRCLE ( 'NONE', #89012, 4.000000000000001776 ) ;
#90708 =( LENGTH_UNIT ( ) NAMED_UNIT ( * ) SI_UNIT ( .MILLI., .METRE. ) );
#90709 = CARTESIAN_POINT ( 'NONE',  ( -6.533875647324832059, 53.62318002580641974, -7.075595340869824668 ) ) ;
#90710 = CARTESIAN_POINT ( 'NONE',  ( 13.50000000000000711, 3.304540750553667028, -12.77799806994943310 ) ) ;
#90711 = SURFACE_STYLE_FILL_AREA ( #23881 ) ;
#90712 = EDGE_CURVE ( 'NONE', #16098, #91737, #56783, .T. ) ;
#90713 = CARTESIAN_POINT ( 'NONE',  ( -23.29983671023154912, 28.09898118347551588, 30.70617127781060063 ) ) ;
#90714 = CARTESIAN_POINT ( 'NONE',  ( 18.71538461538461462, -4.171999999999999709, 0.000000000000000000 ) ) ;
#90715 = CARTESIAN_POINT ( 'NONE',  ( -32.98079388240127230, -53.37464682946390582, 36.89136972320321917 ) ) ;
#90716 = CARTESIAN_POINT ( 'NONE',  ( -3.678498789084922116, -48.98362606748378312, 104.0112638849150812 ) ) ;
#90717 = CARTESIAN_POINT ( 'NONE',  ( 41.71345372385450645, -53.34109301277966608, 43.41992601474273528 ) ) ;
#90718 = ORIENTED_EDGE ( 'NONE', *, *, #65872, .T. ) ;
#90719 = DIRECTION ( 'NONE',  ( -1.000000000000000000, -0.000000000000000000, -0.000000000000000000 ) ) ;
#90720 = CARTESIAN_POINT ( 'NONE',  ( -78.97285025244843837, -38.69040606023478546, 190.9764379862736803 ) ) ;
#90721 = EDGE_LOOP ( 'NONE', ( #25803, #58414, #37029, #8698, #46248, #41122 ) ) ;
#90723 = CARTESIAN_POINT ( 'NONE',  ( 30.55228927099183522, 298.7536840786443690, 10.80461237140096209 ) ) ;
#90722 = CYLINDRICAL_SURFACE ( 'NONE', #57224, 4.000000000000000888 ) ;
#90724 = CARTESIAN_POINT ( 'NONE',  ( 42.36833565741010688, -59.99999999999995026, 45.73954733928472649 ) ) ;
#90725 = CARTESIAN_POINT ( 'NONE',  ( -48.55396075288191327, 8.676907163023333425, -16.74236275264532381 ) ) ;
#90726 = CARTESIAN_POINT ( 'NONE',  ( 5.818834259648335561, 0.6677920147389573291, 6.499999999999999112 ) ) ;
#90727 = CARTESIAN_POINT ( 'NONE',  ( 6.581905806972325301, 41.48827110309209587, -70.61906944721928880 ) ) ;
#90728 = CARTESIAN_POINT ( 'NONE',  ( -38.66383876797932828, 25.31560946603492113, 11.52610263331877505 ) ) ;
#90729 = CARTESIAN_POINT ( 'NONE',  ( 4.696906829037973630, -86.43998147487897654, -3.734050370377307360 ) ) ;
#90730 = CARTESIAN_POINT ( 'NONE',  ( 17.89487417552031445, 45.31800925772327560, 5.467316602108490464 ) ) ;
#90731 = CIRCLE ( 'NONE', #94201, 3.309500000000001663 ) ;
#90732 = CARTESIAN_POINT ( 'NONE',  ( 110.9494655861507937, -60.00000000000000711, 151.6493514595819647 ) ) ;
#90733 = CARTESIAN_POINT ( 'NONE',  ( 0.06809871960542319969, -6.146186931204438153, -5.354491962338079780 ) ) ;
#90734 = CARTESIAN_POINT ( 'NONE',  ( -6.943926999490789953, -65.53300992626145671, -3.973092371898546915 ) ) ;
#90735 = ORIENTED_EDGE ( 'NONE', *, *, #18071, .F. ) ;
#90736 = EDGE_CURVE ( 'NONE', #38226, #36198, #70595, .T. ) ;
#90737 = CARTESIAN_POINT ( 'NONE',  ( -85.97253845739234634, -30.00000000000002132, 178.5979368392352455 ) ) ;
#90738 = VERTEX_POINT ( 'NONE', #61334 ) ;
#90739 = CARTESIAN_POINT ( 'NONE',  ( -43.00000000000000000, 450.0000000000002274, 13.20242257375370976 ) ) ;
#90740 = LINE ( 'NONE', #26057, #89005 ) ;
#90741 = CARTESIAN_POINT ( 'NONE',  ( 7.849089830966804904, 81.65314728018610424, 5.000000000002456702 ) ) ;
#90742 = CARTESIAN_POINT ( 'NONE',  ( 26.51901951938406654, 308.1855417876873844, 10.94630820763295453 ) ) ;
#90743 = CARTESIAN_POINT ( 'NONE',  ( -23.05189055320584046, 27.41800202946304310, -33.19783182242394304 ) ) ;
#90744 = CARTESIAN_POINT ( 'NONE',  ( -7.188101187500000044, -23.28125000204838457, -8.802885111219163269E-16 ) ) ;
#90745 = CARTESIAN_POINT ( 'NONE',  ( 13.37207953394533355, 1.482358050883964840E-15, 0.000000000000000000 ) ) ;
#90747 = EDGE_CURVE ( 'NONE', #24651, #25439, #20674, .T. ) ;
#90746 = CARTESIAN_POINT ( 'NONE',  ( 7.255115585955611124, 41.55406142676530834, -69.27528320264251249 ) ) ;
#90748 =( REPRESENTATION_RELATIONSHIP ('NONE','NONE', #69581, #25516 ) REPRESENTATION_RELATIONSHIP_WITH_TRANSFORMATION ( #26088 )SHAPE_REPRESENTATION_RELATIONSHIP( ) );
#90750 = ORIENTED_EDGE ( 'NONE', *, *, #75544, .F. ) ;
#90749 = CARTESIAN_POINT ( 'NONE',  ( 3.857142857142850545, -1.200583151104938517, 103.1763305333244318 ) ) ;
#90751 = CARTESIAN_POINT ( 'NONE',  ( 83.35798400553088072, -25.61440315765044673, 152.1571764916998006 ) ) ;
#90752 = CARTESIAN_POINT ( 'NONE',  ( -54.43501200699899556, 38.95383793068867817, -33.39731814188755976 ) ) ;
#90753 = CONICAL_SURFACE ( 'NONE', #63194, 3.309499999999999886, 0.7853981633974710386 ) ;
#90754 = CARTESIAN_POINT ( 'NONE',  ( 9.842984802582135373, 88.59069590475651523, 1.781981959250505732 ) ) ;
#90755 = ORIENTED_EDGE ( 'NONE', *, *, #19349, .F. ) ;
#90756 = EDGE_CURVE ( 'NONE', #83228, #3104, #104866, .T. ) ;
#90757 = DIRECTION ( 'NONE',  ( 0.000000000000000000, -1.000000000000000000, 0.000000000000000000 ) ) ;
#90758 = CARTESIAN_POINT ( 'NONE',  ( -0.8430352374540970306, 13.67053680931865678, -51.42626865055270713 ) ) ;
#90759 = CARTESIAN_POINT ( 'NONE',  ( 47.40949999999999420, 0.000000000000000000, 0.000000000000000000 ) ) ;
#90760 = CARTESIAN_POINT ( 'NONE',  ( 7.986539162393897939, 26.02672828942547412, -0.5321833565149868273 ) ) ;
#90761 = CARTESIAN_POINT ( 'NONE',  ( -2.567709512550288231, -59.99999999999997158, -36.87296048416308736 ) ) ;
#90762 = CARTESIAN_POINT ( 'NONE',  ( -24.52277916217002129, 304.2494540235151135, 10.24385320776191399 ) ) ;
#90763 = CARTESIAN_POINT ( 'NONE',  ( -7.499999896686553313, -3.000070742345582797, -20.99858933621946733 ) ) ;
#90764 = ORIENTED_EDGE ( 'NONE', *, *, #74259, .F. ) ;
#90765 = VECTOR ( 'NONE', #86713, 1000.000000000000000 ) ;
#90766 = CIRCLE ( 'NONE', #20220, 4.000000000000001776 ) ;
#90767 = DIRECTION ( 'NONE',  ( 0.000000000000000000, 1.000000000000000000, 0.000000000000000000 ) ) ;
#90768 = CARTESIAN_POINT ( 'NONE',  ( 27.57459505079161843, 18.64284798592546011, -26.76870628200340008 ) ) ;
#90769 = CARTESIAN_POINT ( 'NONE',  ( 86.97298709575052555, -42.77486660283044984, 189.9043035977022100 ) ) ;
#90770 = DIRECTION ( 'NONE',  ( -1.000000000000000000, 0.000000000000000000, 0.000000000000000000 ) ) ;
#90771 = CARTESIAN_POINT ( 'NONE',  ( -4.912107334123172464, -8.720202445280490267, 6.401601164861591364 ) ) ;
#90772 = CARTESIAN_POINT ( 'NONE',  ( 32.17570300886618639, -33.85735722696470873, 41.96334411972644318 ) ) ;
#90773 = CIRCLE ( 'NONE', #32188, 4.000000000000000888 ) ;
#90774 = FACE_OUTER_BOUND ( 'NONE', #54008, .T. ) ;
#90775 = AXIS2_PLACEMENT_3D ( 'NONE', #28904, #45579, #36459 ) ;
#90776 = AXIS2_PLACEMENT_3D ( 'NONE', #47302, #97436, #83263 ) ;
#90777 = LINE ( 'NONE', #68086, #94783 ) ;
#90778 = EDGE_CURVE ( 'NONE', #17393, #63739, #55008, .T. ) ;
#90779 = CARTESIAN_POINT ( 'NONE',  ( 38.91686277342078171, 438.0826785806304997, 23.13445567070433384 ) ) ;
#90780 = APPLICATION_PROTOCOL_DEFINITION ( 'draft international standard', 'automotive_design', 1998, #4599 ) ;
#90781 = CARTESIAN_POINT ( 'NONE',  ( 48.02835407290544367, 9.771516447483593382, 16.85535821593427386 ) ) ;
#90782 = ORIENTED_EDGE ( 'NONE', *, *, #77636, .T. ) ;
#90783 = CARTESIAN_POINT ( 'NONE',  ( 0.000000000000000000, -30.00000000000000000, 0.000000000000000000 ) ) ;
#90784 = AXIS2_PLACEMENT_3D ( 'NONE', #88546, #105774, #41575 ) ;
#90785 = CARTESIAN_POINT ( 'NONE',  ( 13.45452273892127870, 42.85594303034280017, -92.00308933281662860 ) ) ;
#90786 = DIRECTION ( 'NONE',  ( 0.000000000000000000, 0.000000000000000000, 1.000000000000000000 ) ) ;
#90787 = CARTESIAN_POINT ( 'NONE',  ( 0.000000000000000000, 0.000000000000000000, 4.000000000000000000 ) ) ;
#90788 = EDGE_CURVE ( 'NONE', #63262, #58013, #5829, .T. ) ;
#90789 = ORIENTED_EDGE ( 'NONE', *, *, #19217, .F. ) ;
#90790 = CARTESIAN_POINT ( 'NONE',  ( 37.40949999999997289, 4.898587196589414801E-16, -4.000000000000001776 ) ) ;
#90791 = FACE_OUTER_BOUND ( 'NONE', #12874, .T. ) ;
#90792 = CARTESIAN_POINT ( 'NONE',  ( 100.6493391994169713, -57.67098493463386433, 72.97180361904253232 ) ) ;
#90793 = EDGE_CURVE ( 'NONE', #16424, #60319, #58509, .T. ) ;
#90794 = CARTESIAN_POINT ( 'NONE',  ( 36.52561726181321689, 463.3029834606174973, 20.13286708880512776 ) ) ;
#90795 = CARTESIAN_POINT ( 'NONE',  ( 2.455632601332660148, 14.68453990184912428, 6.559068799100592706 ) ) ;
#90796 = CARTESIAN_POINT ( 'NONE',  ( -5.000000000000000000, 0.000000000000000000, -2.868028571428571372 ) ) ;
#90797 = CARTESIAN_POINT ( 'NONE',  ( 1.227754105814699780E-15, 67.05096163904791240, 10.02537308446410691 ) ) ;
#90798 = CARTESIAN_POINT ( 'NONE',  ( -76.39489477947479656, -59.99999999999998579, 188.5198920997321181 ) ) ;
#90799 = CARTESIAN_POINT ( 'NONE',  ( -30.55228927099183522, 298.7536840786443690, 10.80461237140096209 ) ) ;
#90800 = DIRECTION ( 'NONE',  ( -1.000000000000000000, 0.000000000000000000, 0.000000000000000000 ) ) ;
#90801 = CARTESIAN_POINT ( 'NONE',  ( -42.35263604938428017, 50.00000000000000000, 46.99568999588436924 ) ) ;
#90802 = CARTESIAN_POINT ( 'NONE',  ( -86.28510748321916424, -21.13358643084282562, 179.4914488576992539 ) ) ;
#90803 = ORIENTED_EDGE ( 'NONE', *, *, #3549, .F. ) ;
#90804 = CARTESIAN_POINT ( 'NONE',  ( 29.18041179959944387, 310.2186600874167084, -8.763845530462663902 ) ) ;
#90805 = VECTOR ( 'NONE', #17530, 1000.000000000000000 ) ;
#90806 = ORIENTED_EDGE ( 'NONE', *, *, #81192, .F. ) ;
#90807 = CARTESIAN_POINT ( 'NONE',  ( 16.08349330513380337, 1.593028355512270567E-15, 0.000000000000000000 ) ) ;
#90808 = EDGE_CURVE ( 'NONE', #47413, #64398, #80885, .T. ) ;
#90809 = CARTESIAN_POINT ( 'NONE',  ( -111.8964183755431918, 22.97884757028484870, 55.94820918777157459 ) ) ;
#90810 = CARTESIAN_POINT ( 'NONE',  ( -82.83571923027355410, -37.76998749466422822, -11.56981727052722952 ) ) ;
#90811 = DIRECTION ( 'NONE',  ( 0.9605097441494802046, 0.000000000000000000, -0.2782463501897193825 ) ) ;
#90812 = CARTESIAN_POINT ( 'NONE',  ( 37.40949999999997289, 0.000000000000000000, 0.000000000000000000 ) ) ;
#90813 = CARTESIAN_POINT ( 'NONE',  ( -5.479219201945285889, 5.339799775453948349, -5.000000000000000888 ) ) ;
#90814 = DIRECTION ( 'NONE',  ( 0.000000000000000000, 1.000000000000000000, 0.000000000000000000 ) ) ;
#90815 = CARTESIAN_POINT ( 'NONE',  ( 6.315918964083451215, 41.33387245947155719, -58.37026373930601864 ) ) ;
#90817 = AXIS2_PLACEMENT_3D ( 'NONE', #60859, #53288, #93749 ) ;
#90816 = CARTESIAN_POINT ( 'NONE',  ( -14.86825985027621755, -1.734723475976807094E-15, 8.569529079659670145 ) ) ;
#90818 = SURFACE_STYLE_FILL_AREA ( #106447 ) ;
#90819 = CARTESIAN_POINT ( 'NONE',  ( 2.851859124854637884, -60.00000000000000711, -45.00000000000000711 ) ) ;
#90820 = CARTESIAN_POINT ( 'NONE',  ( -80.26835608370822683, -22.15024438636563531, 130.4779458602490081 ) ) ;
#90821 = ORIENTED_EDGE ( 'NONE', *, *, #67403, .F. ) ;
#90822 = CARTESIAN_POINT ( 'NONE',  ( 61.00101809772601769, -14.21045842199439591, 86.19763211990357377 ) ) ;
#90823 = CARTESIAN_POINT ( 'NONE',  ( 8.000113193197767814, 89.00022638645860695, -0.2613481123984641719 ) ) ;
#90824 = CARTESIAN_POINT ( 'NONE',  ( 113.9092013170919984, -57.67115667734820050, 163.3307494887165205 ) ) ;
#90825 = ORIENTED_EDGE ( 'NONE', *, *, #61755, .T. ) ;
#90826 = CARTESIAN_POINT ( 'NONE',  ( 33.52307692307692122, -4.171999999999999709, 5.616230220889763424E-16 ) ) ;
#90827 = AXIS2_PLACEMENT_3D ( 'NONE', #17426, #15817, #16894 ) ;
#90828 = CARTESIAN_POINT ( 'NONE',  ( 0.000000000000000000, 24.35682532067546902, 0.000000000000000000 ) ) ;
#90829 = ORIENTED_EDGE ( 'NONE', *, *, #41160, .T. ) ;
#90830 = MECHANICAL_DESIGN_GEOMETRIC_PRESENTATION_REPRESENTATION (  '', ( #95986 ), #23706 ) ;
#90831 = CARTESIAN_POINT ( 'NONE',  ( -7.000000000000000000, 8.572527594031473190E-16, -8.125150395352576993 ) ) ;
#90832 = LINE ( 'NONE', #16947, #61760 ) ;
#90833 = CARTESIAN_POINT ( 'NONE',  ( 15.55735228453472274, 44.07604505559044838, 4.783429685249553920 ) ) ;
#90834 = CARTESIAN_POINT ( 'NONE',  ( -7.188101187500000044, -10.90625000204838457, -8.802885111219163269E-16 ) ) ;
#90835 = DIRECTION ( 'NONE',  ( -0.9995674975569972531, 0.02876390015618488644, 0.006120120541885859695 ) ) ;
#90836 =( BOUNDED_CURVE ( )  B_SPLINE_CURVE ( 2, ( #21115, #88988, #54461, #71201, #104632, #30237, #23214, #46410, #78757 ),
 .UNSPECIFIED., .F., .F. ) 
 B_SPLINE_CURVE_WITH_KNOTS ( ( 3, 2, 2, 2, 3 ),
 ( 0.3970588235294117974, 0.4044117647058824150, 0.4117647058823530326, 0.4191176470588236502, 0.4264705882352942123 ),
 .UNSPECIFIED. ) 
 CURVE ( )  GEOMETRIC_REPRESENTATION_ITEM ( )  RATIONAL_B_SPLINE_CURVE ( ( 0.9999999999999994449, 0.9238795325112872936, 1.000000000000000000, 0.9238795325112867385, 1.000000000000000000, 0.9238795325112867385, 1.000000000000000000, 0.9238795325112856283, 1.000000000000001110 ) ) 
 REPRESENTATION_ITEM ( '' )  );
#90837 = CARTESIAN_POINT ( 'NONE',  ( -7.500000000000000000, -4.652405105468744750, -7.929127756970858698 ) ) ;
#90838 = EDGE_LOOP ( 'NONE', ( #67991, #39355, #26715 ) ) ;
#90839 = CARTESIAN_POINT ( 'NONE',  ( -7.113472013431297647, 40.00000000006956924, -71.00901315851918127 ) ) ;
#90840 = VECTOR ( 'NONE', #78189, 1000.000000000000000 ) ;
#90841 = AXIS2_PLACEMENT_3D ( 'NONE', #15182, #73404, #22252 ) ;
#90842 = CARTESIAN_POINT ( 'NONE',  ( 30.66882219077799121, -32.54285829269771568, 32.11411510472900233 ) ) ;
#90843 = CARTESIAN_POINT ( 'NONE',  ( 26.59373630444105885, 307.2488738721764889, -8.467865159397765851 ) ) ;
#90844 = VERTEX_POINT ( 'NONE', #31106 ) ;
#90845 = CARTESIAN_POINT ( 'NONE',  ( -0.8340869376443533767, 18.10461962298600724, 49.56574745738932819 ) ) ;
#90846 = VERTEX_POINT ( 'NONE', #106534 ) ;
#90847 = CIRCLE ( 'NONE', #59837, 11.00000000000001066 ) ;
#90849 = CARTESIAN_POINT ( 'NONE',  ( -7.996135855215158905, -4.999999999999999112, 6.145819459795549555 ) ) ;
#90848 = DIRECTION ( 'NONE',  ( -1.000000000000000000, -1.224606353822377258E-16, -0.000000000000000000 ) ) ;
#90850 = FACE_OUTER_BOUND ( 'NONE', #64081, .T. ) ;
#90851 = CARTESIAN_POINT ( 'NONE',  ( -15.38346597837744767, 302.5568188537556580, -10.06270105311703844 ) ) ;
#90852 = VECTOR ( 'NONE', #71679, 1000.000000000000000 ) ;
#90853 = CIRCLE ( 'NONE', #44351, 4.250000000000000000 ) ;
#90854 = CARTESIAN_POINT ( 'NONE',  ( -33.74977848768426725, 477.7786480585253344, 4.002244379145985853 ) ) ;
#90855 = DIRECTION ( 'NONE',  ( 0.5735764363510491570, -0.8191520442889895781, 1.003171929053522035E-16 ) ) ;
#90856 = CARTESIAN_POINT ( 'NONE',  ( -35.72584807339683977, 463.6218724463183207, 19.50045127626819763 ) ) ;
#90857 = ORIENTED_EDGE ( 'NONE', *, *, #93126, .T. ) ;
#90858 = CARTESIAN_POINT ( 'NONE',  ( 92.74063705008857994, -60.00000000000000000, -6.517803209784806207 ) ) ;
#90859 = CARTESIAN_POINT ( 'NONE',  ( -9.204171687489189679, 45.78377104600745895, 14.80353108812683871 ) ) ;
#90860 = CARTESIAN_POINT ( 'NONE',  ( 32.31726413982377011, 464.7724101315872076, 15.30491388830120236 ) ) ;
#90861 = CARTESIAN_POINT ( 'NONE',  ( 18.69420657816679210, 304.6310092840336097, -10.04693110555011160 ) ) ;
#90862 = CARTESIAN_POINT ( 'NONE',  ( 61.11682663846713837, -4.000000000000000000, 4.898587196589421703E-16 ) ) ;
#90863 = VERTEX_POINT ( 'NONE', #48817 ) ;
#90864 = ADVANCED_FACE ( 'NONE', ( #15406 ), #63992, .F. ) ;
#90865 = EDGE_CURVE ( 'NONE', #46183, #59988, #25825, .T. ) ;
#90866 = CARTESIAN_POINT ( 'NONE',  ( -4.582575694955839829, 16.00000000000000000, 10.00000000000000000 ) ) ;
#90867 = ORIENTED_EDGE ( 'NONE', *, *, #43042, .T. ) ;
#90868 = ORIENTED_EDGE ( 'NONE', *, *, #91862, .F. ) ;
#90869 = CYLINDRICAL_SURFACE ( 'NONE', #67590, 4.000000000000000000 ) ;
#90870 = CARTESIAN_POINT ( 'NONE',  ( 6.222742520105472686, -3.584500230190552639, -6.791463481567638460 ) ) ;
#90871 = CARTESIAN_POINT ( 'NONE',  ( 7.907996613752301229, 3.055722423191984838, -7.792112796859424151 ) ) ;
#90872 = CARTESIAN_POINT ( 'NONE',  ( 26.78666884061847853, 306.6412577338363690, 10.80680221502309912 ) ) ;
#90873 = CARTESIAN_POINT ( 'NONE',  ( 82.69522727347742830, -37.85838301434696973, 3.610110074265372226 ) ) ;
#90874 = CARTESIAN_POINT ( 'NONE',  ( -45.37852524047085723, 369.5271474663848039, 5.963215168293914736 ) ) ;
#90875 = CARTESIAN_POINT ( 'NONE',  ( -4.911511084989005127, -63.26970332188709989, 12.93090383856629444 ) ) ;
#90876 = ORIENTED_EDGE ( 'NONE', *, *, #7508, .T. ) ;
#90878 = ADVANCED_FACE ( 'NONE', ( #73630 ), #61994, .T. ) ;
#90877 = CARTESIAN_POINT ( 'NONE',  ( 30.77294675439390659, 10.36444884528815180, 40.23167857000779435 ) ) ;
#90879 = ORIENTED_EDGE ( 'NONE', *, *, #61439, .T. ) ;
#90880 = AXIS2_PLACEMENT_3D ( 'NONE', #18877, #51720, #84635 ) ;
#90881 = CARTESIAN_POINT ( 'NONE',  ( 9.169403562584983902, 51.60716162735785417, -1.678691385831598604 ) ) ;
#90882 = CARTESIAN_POINT ( 'NONE',  ( -89.32918359285039855, -38.52324389788776671, 200.4084188219295868 ) ) ;
#90883 = CARTESIAN_POINT ( 'NONE',  ( 41.90617369998742703, 464.5440823313534793, 16.88098358180886294 ) ) ;
#90884 = AXIS2_PLACEMENT_3D ( 'NONE', #69113, #68583, #28144 ) ;
#90886 = ORIENTED_EDGE ( 'NONE', *, *, #22955, .F. ) ;
#90885 = FACE_BOUND ( 'NONE', #88474, .T. ) ;
#90887 = CARTESIAN_POINT ( 'NONE',  ( 64.03519573087221772, -49.91008808719962531, 88.80839993703304458 ) ) ;
#90888 = ORIENTED_EDGE ( 'NONE', *, *, #97029, .F. ) ;
#90889 = EDGE_CURVE ( 'NONE', #9677, #105570, #6785, .T. ) ;
#90890 = CONICAL_SURFACE ( 'NONE', #104652, 3.309500000000007880, 0.9599310885968770357 ) ;
#90891 = CARTESIAN_POINT ( 'NONE',  ( -7.188101187500000044, -28.90625000204838813, -8.802885111219163269E-16 ) ) ;
#90892 = CARTESIAN_POINT ( 'NONE',  ( -81.27538057784241232, -57.67119034933180188, -29.50368748078413361 ) ) ;
#90893 = EDGE_CURVE ( 'NONE', #76468, #51522, #16475, .T. ) ;
#90894 = EDGE_LOOP ( 'NONE', ( #14842, #36648, #61078, #90347, #67704, #58757 ) ) ;
#90895 = CARTESIAN_POINT ( 'NONE',  ( -10.00000000000000178, 0.000000000000000000, -9.999999999999998224 ) ) ;
#90896 = CONICAL_SURFACE ( 'NONE', #71866, 3.309500000000007880, 0.9599310885968770357 ) ;
#90897 = CARTESIAN_POINT ( 'NONE',  ( -34.12349128637492157, 490.8027302422244134, 11.84948222508912430 ) ) ;
#90899 = CARTESIAN_POINT ( 'NONE',  ( -16.64348903516517098, 43.75610143575153899, 4.157797401561652784 ) ) ;
#90898 = B_SPLINE_CURVE_WITH_KNOTS ( 'NONE', 3,
 ( #81464, #18375, #10768, #37231, #18927, #19467, #28080, #2689, #70092, #3774, #100856, #76574, #92766, #102996, #28610, #77661, #61493, #44231, #11841, #36178, #4296, #102463, #12373, #44772, #35640, #62027, #36709, #3234, #27556, #69046, #29155, #27015, #101402, #43164 ),
 .UNSPECIFIED., .F., .F.,
 ( 4, 2, 2, 2, 2, 2, 2, 2, 2, 2, 2, 2, 2, 2, 2, 2, 4 ),
 ( 0.000000000000000000, 0.0007899309203816051251, 0.001579861840763210250, 0.002369792761144815484, 0.003159723681526420500, 0.003949654601908025517, 0.004739585522289630967, 0.005529516442671235550, 0.006319447363052841000, 0.007109378283434446451, 0.007899309203816051034, 0.008689240124197656484, 0.009479171044579261934, 0.01026910196496086738, 0.01105903288534247110, 0.01184896380572407655, 0.01263889472610568200 ),
 .UNSPECIFIED. ) ;
#90900 = CARTESIAN_POINT ( 'NONE',  ( -8.000000000000000000, -21.03125000409677625, -3.313708498984762496 ) ) ;
#90901 = CARTESIAN_POINT ( 'NONE',  ( -10.00000000000000178, -15.00000000000000000, -9.999999999999998224 ) ) ;
#90902 = FACE_OUTER_BOUND ( 'NONE', #48222, .T. ) ;
#90903 = DIRECTION ( 'NONE',  ( -1.000000000000000000, -1.224606353822377258E-16, -0.000000000000000000 ) ) ;
#90904 = B_SPLINE_CURVE_WITH_KNOTS ( 'NONE', 3,
 ( #86585, #36979, #94116, #15174, #61230, #31915 ),
 .UNSPECIFIED., .F., .F.,
 ( 4, 2, 4 ),
 ( 0.000000000000000000, 0.0003491763592121711088, 0.0006983527184243422175 ),
 .UNSPECIFIED. ) ;
#90905 = AXIS2_PLACEMENT_3D ( 'NONE', #47756, #103371, #55834 ) ;
#90906 = CARTESIAN_POINT ( 'NONE',  ( -5.914126066640156942, 4.617998735621883455, 4.999999999999999112 ) ) ;
#90907 = CYLINDRICAL_SURFACE ( 'NONE', #67150, 5.000000000000002665 ) ;
#90908 = DIRECTION ( 'NONE',  ( 1.000000000000000000, 0.000000000000000000, 0.000000000000000000 ) ) ;
#90909 = CARTESIAN_POINT ( 'NONE',  ( -2.838086098462165197, -29.99999999999999289, -7.435270884616921983 ) ) ;
#90910 = EDGE_LOOP ( 'NONE', ( #91227, #90009 ) ) ;
#90911 = CARTESIAN_POINT ( 'NONE',  ( 33.00000000000000000, 463.5362553048592531, 6.739467187734345721 ) ) ;
#90912 = FILL_AREA_STYLE ('',( #57991 ) ) ;
#90913 = CARTESIAN_POINT ( 'NONE',  ( -5.000000000000000888, -58.90829880881958047, 11.71896219753489810 ) ) ;
#90914 = CARTESIAN_POINT ( 'NONE',  ( -91.28316960610226261, -30.00000000000000000, 190.6086971429253651 ) ) ;
#90915 = ADVANCED_FACE ( 'NONE', ( #98961 ), #97917, .F. ) ;
#90916 = CARTESIAN_POINT ( 'NONE',  ( 38.31446012149793745, 25.47195784124091844, -11.19161216425135308 ) ) ;
#90917 = CIRCLE ( 'NONE', #4766, 12.00000000000000711 ) ;
#90918 = CARTESIAN_POINT ( 'NONE',  ( 63.16835690643451784, -57.67863152263677051, 119.1560271867259928 ) ) ;
#90920 = CARTESIAN_POINT ( 'NONE',  ( -8.881211395233728823, 53.58339314524378239, 3.999935137841994504 ) ) ;
#90919 = CARTESIAN_POINT ( 'NONE',  ( 0.000000000000000000, 0.000000000000000000, -8.574621033218877031 ) ) ;
#90921 = ADVANCED_FACE ( 'NONE', ( #43940 ), #89528, .T. ) ;
#90922 = EDGE_CURVE ( 'NONE', #9659, #41772, #43023, .T. ) ;
#90923 = CARTESIAN_POINT ( 'NONE',  ( 23.78672531768528842, -27.25131086482705456, -38.40582345290683008 ) ) ;
#90924 = CARTESIAN_POINT ( 'NONE',  ( -27.10511071441192144, 34.47735702144345282, -10.05698433968589178 ) ) ;
#90925 = CARTESIAN_POINT ( 'NONE',  ( -43.37962327791924366, -60.00000000000000711, 57.54474475887785445 ) ) ;
#90926 = AXIS2_PLACEMENT_3D ( 'NONE', #87489, #33373, #105250 ) ;
#90927 = CONICAL_SURFACE ( 'NONE', #44430, 5.000000000000000000, 0.9599310885968804774 ) ;
#90928 =( GEOMETRIC_REPRESENTATION_CONTEXT ( 3 ) GLOBAL_UNCERTAINTY_ASSIGNED_CONTEXT ( ( #9549 ) ) GLOBAL_UNIT_ASSIGNED_CONTEXT ( ( #65546, #97902, #98948 ) ) REPRESENTATION_CONTEXT ( 'NONE', 'WORKASPACE' ) );
#90929 = CARTESIAN_POINT ( 'NONE',  ( 14.29190075645216496, 21.26710225494213802, 5.626279437277409201 ) ) ;
#90930 = CARTESIAN_POINT ( 'NONE',  ( 0.000000000000000000, 0.000000000000000000, 5.000000000000000000 ) ) ;
#90931 = CARTESIAN_POINT ( 'NONE',  ( -86.66824802271996475, -46.47689432800410003, 190.4879100785292394 ) ) ;
#90932 = VERTEX_POINT ( 'NONE', #43416 ) ;
#90933 = CARTESIAN_POINT ( 'NONE',  ( 17.50000000000028422, 50.00000000000154898, 59.64162155654624797 ) ) ;
#90934 = CARTESIAN_POINT ( 'NONE',  ( 11.96261933146057821, -7.078120104440478677, 19.72315005431197221 ) ) ;
#90935 = CARTESIAN_POINT ( 'NONE',  ( -9.314508772266908210, -49.92099836516761258, 32.21320177879483282 ) ) ;
#90936 = CARTESIAN_POINT ( 'NONE',  ( -6.236082950926880919, 41.88001960641946653, -59.13168064570682247 ) ) ;
#90938 = CARTESIAN_POINT ( 'NONE',  ( 0.9999999999999993339, -69.59657292934915063, 12.76848391599223120 ) ) ;
#90937 = CARTESIAN_POINT ( 'NONE',  ( 19.00000000000001066, -4.000000000000000000, -1.500000000000001332 ) ) ;
#90939 = ORIENTED_EDGE ( 'NONE', *, *, #49800, .F. ) ;
#90940 = EDGE_CURVE ( 'NONE', #7512, #23483, #104997, .T. ) ;
#90941 = CARTESIAN_POINT ( 'NONE',  ( 8.455951367436818379E-15, 13.70447791526914294, 49.24999999999998579 ) ) ;
#90942 = AXIS2_PLACEMENT_3D ( 'NONE', #14608, #89588, #47519 ) ;
#90943 = CARTESIAN_POINT ( 'NONE',  ( -7.101747359475742982, -4.047770588416829796, -17.37629258578624203 ) ) ;
#90944 = CARTESIAN_POINT ( 'NONE',  ( 16.42488309403321978, 34.33240771944122116, 24.27441078751466108 ) ) ;
#90945 = CARTESIAN_POINT ( 'NONE',  ( 34.02613438762318054, 301.2396209895970856, -0.5563051883781007234 ) ) ;
#90947 = MANIFOLD_SOLID_BREP ( 'ThdSchPat', #49764 ) ;
#90946 = DIRECTION ( 'NONE',  ( -1.000000000000000000, -0.000000000000000000, -0.000000000000000000 ) ) ;
#90948 = EDGE_CURVE ( 'NONE', #73449, #13600, #30968, .T. ) ;
#90949 = CARTESIAN_POINT ( 'NONE',  ( -7.551560007654698481, -81.99089648193009339, -2.648022159607833270 ) ) ;
#90950 = DIRECTION ( 'NONE',  ( 0.000000000000000000, 1.000000000000000000, 0.000000000000000000 ) ) ;
#90951 = PRESENTATION_LAYER_ASSIGNMENT (  '', '', ( #16888 ) ) ;
#90952 = CARTESIAN_POINT ( 'NONE',  ( 114.4521715241705664, -60.00000000000002842, 166.3966616003652348 ) ) ;
#90953 = CARTESIAN_POINT ( 'NONE',  ( 91.09088295274877112, 1.030564683017419500E-14, 0.000000000000000000 ) ) ;
#90954 = ORIENTED_EDGE ( 'NONE', *, *, #51196, .F. ) ;
#90955 = CARTESIAN_POINT ( 'NONE',  ( 0.000000000000000000, 4.898587196589413815E-16, -4.000000000000000888 ) ) ;
#90956 = DIRECTION ( 'NONE',  ( 0.000000000000000000, 1.000000000000000000, 0.000000000000000000 ) ) ;
#90957 = DIRECTION ( 'NONE',  ( 0.000000000000000000, 0.000000000000000000, 1.000000000000000000 ) ) ;
#90958 = EDGE_CURVE ( 'NONE', #39308, #47158, #50946, .T. ) ;
#90960 = AXIS2_PLACEMENT_3D ( 'NONE', #96959, #63547, #80228 ) ;
#90959 = CARTESIAN_POINT ( 'NONE',  ( 3.363233428609735398, 30.69038356566756676, -4.999999999999999112 ) ) ;
#90961 = CARTESIAN_POINT ( 'NONE',  ( 24.83349330513380693, 1.593028355512270962E-15, 0.000000000000000000 ) ) ;
#90962 = ORIENTED_EDGE ( 'NONE', *, *, #5169, .T. ) ;
#90963 = CARTESIAN_POINT ( 'NONE',  ( 6.800000000000000711, 0.000000000000000000, 0.000000000000000000 ) ) ;
#90964 = ORIENTED_EDGE ( 'NONE', *, *, #5276, .T. ) ;
#90965 = CARTESIAN_POINT ( 'NONE',  ( 34.88071508727530556, 485.0161356477989898, -0.9861291933420458511 ) ) ;
#90966 = DIRECTION ( 'NONE',  ( -0.3048027540940034252, 0.4519649026942579861, 0.8383453988835869453 ) ) ;
#90967 = ORIENTED_EDGE ( 'NONE', *, *, #52326, .F. ) ;
#90968 = CARTESIAN_POINT ( 'NONE',  ( -39.04923757935653583, 48.00000000000000000, 52.30342408741262972 ) ) ;
#90969 = CARTESIAN_POINT ( 'NONE',  ( 5.000000000000000000, -14.50704001784992059, 12.23934196172798394 ) ) ;
#90970 = CARTESIAN_POINT ( 'NONE',  ( -72.81278058970477218, -59.99999999999997868, 182.9869454968206526 ) ) ;
#90971 = ORIENTED_EDGE ( 'NONE', *, *, #27185, .F. ) ;
#90972 = CARTESIAN_POINT ( 'NONE',  ( 91.85330244269961497, -59.99999999999997158, 11.80756330073621818 ) ) ;
#90974 = CARTESIAN_POINT ( 'NONE',  ( 14.66643285550703268, -46.43468913974415813, 31.75579674561490506 ) ) ;
#90973 = CARTESIAN_POINT ( 'NONE',  ( -74.10870907870054225, -60.00000000000004974, 189.8079394841834073 ) ) ;
#90976 = CARTESIAN_POINT ( 'NONE',  ( 82.45602942012469327, -37.99999999999996447, -12.86876314179797731 ) ) ;
#90975 = UNCERTAINTY_MEASURE_WITH_UNIT (LENGTH_MEASURE( 1.000000000000000082E-05 ), #100830, 'distance_accuracy_value', 'NONE');
#90977 = DIRECTION ( 'NONE',  ( 0.000000000000000000, 0.000000000000000000, 1.000000000000000000 ) ) ;
#90978 = AXIS2_PLACEMENT_3D ( 'NONE', #57650, #35026, #59816 ) ;
#90979 = CARTESIAN_POINT ( 'NONE',  ( -40.91703361344463730, -32.61193104857954239, 37.87439492575138900 ) ) ;
#90980 = CYLINDRICAL_SURFACE ( 'NONE', #7447, 4.000000000000000000 ) ;
#90981 = ORIENTED_EDGE ( 'NONE', *, *, #1542, .T. ) ;
#90982 = DIRECTION ( 'NONE',  ( -1.000000000000000000, -0.000000000000000000, -0.000000000000000000 ) ) ;
#90983 = FACE_BOUND ( 'NONE', #44943, .T. ) ;
#90984 = CARTESIAN_POINT ( 'NONE',  ( 40.73878143178837519, 486.4834083601638213, 16.46716573231486436 ) ) ;
#90985 =( NAMED_UNIT ( * ) PLANE_ANGLE_UNIT ( ) SI_UNIT ( $, .RADIAN. ) );
#90986 = FACE_OUTER_BOUND ( 'NONE', #78536, .T. ) ;
#90987 = CARTESIAN_POINT ( 'NONE',  ( -32.01266203147167744, 486.7692091651749138, 6.765869859085228200 ) ) ;
#90988 = ORIENTED_EDGE ( 'NONE', *, *, #37286, .T. ) ;
#90989 = CARTESIAN_POINT ( 'NONE',  ( 4.725902370230407712, -47.47364726308473593, 103.4500010546506417 ) ) ;
#90990 = CIRCLE ( 'NONE', #10056, 5.000000000000011546 ) ;
#90991 = CARTESIAN_POINT ( 'NONE',  ( 9.999999999999998224, -15.00000000000000000, -9.999999999999998224 ) ) ;
#90992 = ORIENTED_EDGE ( 'NONE', *, *, #72686, .T. ) ;
#90993 = CARTESIAN_POINT ( 'NONE',  ( 77.15469530005194088, -30.00000000000000711, -16.53926888306029852 ) ) ;
#90994 = CARTESIAN_POINT ( 'NONE',  ( 46.79842100651300996, 13.68672532571792821, 15.36912611011920582 ) ) ;
#90995 = CARTESIAN_POINT ( 'NONE',  ( 9.035703905990981610, -10.37169118567828541, -0.1149164202474967089 ) ) ;
#90996 = DIRECTION ( 'NONE',  ( 0.000000000000000000, -1.000000000000000000, 0.000000000000000000 ) ) ;
#90997 = CARTESIAN_POINT ( 'NONE',  ( 80.76008078732601803, -30.00000000000000355, 12.10041964063638531 ) ) ;
#90998 = B_SPLINE_CURVE_WITH_KNOTS ( 'NONE', 3,
 ( #90451, #48905, #81799, #90995, #8987, #82354 ),
 .UNSPECIFIED., .F., .F.,
 ( 4, 2, 4 ),
 ( 2.380729204595406704E-07, 0.003943479449179617714, 0.007886720825438776200 ),
 .UNSPECIFIED. ) ;
#90999 = CARTESIAN_POINT ( 'NONE',  ( 7.151217271224852290, 103.2125059955428554, -3.587901469523284259 ) ) ;
#91000 = ORIENTED_EDGE ( 'NONE', *, *, #99230, .F. ) ;
#91001 = EDGE_CURVE ( 'NONE', #29277, #3543, #17556, .T. ) ;
#91002 = ORIENTED_EDGE ( 'NONE', *, *, #38471, .T. ) ;
#91003 = VERTEX_POINT ( 'NONE', #2937 ) ;
#91004 = VECTOR ( 'NONE', #17734, 1000.000000000000000 ) ;
#91005 = CARTESIAN_POINT ( 'NONE',  ( 0.4988340113754565208, 3.871605243940355656, -8.000000000000000000 ) ) ;
#91006 = CARTESIAN_POINT ( 'NONE',  ( 43.40156817619795504, 435.0518544018561329, 15.31415127482170035 ) ) ;
#91007 = AXIS2_PLACEMENT_3D ( 'NONE', #58726, #83512, #961 ) ;
#91008 = DIRECTION ( 'NONE',  ( 0.000000000000000000, -1.000000000000000000, 0.000000000000000000 ) ) ;
#91009 = MECHANICAL_DESIGN_GEOMETRIC_PRESENTATION_REPRESENTATION (  '', ( #18647 ), #6593 ) ;
#91010 = CARTESIAN_POINT ( 'NONE',  ( -42.75106025684119260, 464.8151298349279728, 15.61142817803142790 ) ) ;
#91012 = VECTOR ( 'NONE', #76531, 1000.000000000000000 ) ;
#91011 = CARTESIAN_POINT ( 'NONE',  ( -31.60000081795433857, 345.3413446759684007, 19.62217261211241137 ) ) ;
#91013 = EDGE_CURVE ( 'NONE', #21082, #31057, #20020, .T. ) ;
#91014 = CARTESIAN_POINT ( 'NONE',  ( 7.681258945454893382E-14, -1.200000000000000030E-05, 39.50000000000000000 ) ) ;
#91015 = ORIENTED_EDGE ( 'NONE', *, *, #25650, .F. ) ;
#91017 = EDGE_CURVE ( 'NONE', #77573, #62254, #43100, .T. ) ;
#91016 = CARTESIAN_POINT ( 'NONE',  ( 9.797372177749755551, 108.4650949484756239, 2.014953862275849605 ) ) ;
#91018 = ORIENTED_EDGE ( 'NONE', *, *, #23480, .T. ) ;
#91019 = DIRECTION ( 'NONE',  ( -1.000000000000000000, -0.000000000000000000, -0.000000000000000000 ) ) ;
#91020 = CARTESIAN_POINT ( 'NONE',  ( 85.38575775096529696, -38.67724262594119011, 198.7153968702330928 ) ) ;
#91021 = CARTESIAN_POINT ( 'NONE',  ( 6.169949891408688103, 6.308465495019028424, -2.073417244830852990 ) ) ;
#91022 = CARTESIAN_POINT ( 'NONE',  ( 31.73931315321975433, 299.2822593833305405, 2.924664567257585723 ) ) ;
#91023 = CARTESIAN_POINT ( 'NONE',  ( -3.400000000000000355, 4.163799117101001052E-16, -8.000000000000000000 ) ) ;
#91024 = EDGE_CURVE ( 'NONE', #101821, #49452, #68909, .T. ) ;
#91025 = FILL_AREA_STYLE_COLOUR ( '', #45867 ) ;
#91026 = B_SPLINE_CURVE_WITH_KNOTS ( 'NONE', 3,
 ( #26269, #92014, #18150, #10034, #42941, #75830, #96292, #22417 ),
 .UNSPECIFIED., .F., .F.,
 ( 4, 2, 2, 4 ),
 ( 0.000000000000000000, 0.2500000000000053291, 0.5000000000000106581, 1.000000000000000000 ),
 .UNSPECIFIED. ) ;
#91027 = EDGE_CURVE ( 'NONE', #63428, #53314, #86165, .T. ) ;
#91028 = ADVANCED_FACE ( 'NONE', ( #52550 ), #59844, .T. ) ;
#91029 = CARTESIAN_POINT ( 'NONE',  ( -42.23079339798741927, 460.7352525929354101, 2.726051457480709761 ) ) ;
#91030 = CARTESIAN_POINT ( 'NONE',  ( 42.69425402696286653, 372.2145364761282167, 18.00764261570441604 ) ) ;
#91031 = CARTESIAN_POINT ( 'NONE',  ( 6.800000000000000711, 0.000000000000000000, 0.000000000000000000 ) ) ;
#91032 = DIRECTION ( 'NONE',  ( 0.000000000000000000, -1.000000000000000000, 0.000000000000000000 ) ) ;
#91033 = ORIENTED_EDGE ( 'NONE', *, *, #69198, .T. ) ;
#91035 = CARTESIAN_POINT ( 'NONE',  ( -27.69739594536710214, 296.8485875735327113, 10.37266411860409221 ) ) ;
#91034 = CARTESIAN_POINT ( 'NONE',  ( 0.000000000000000000, 0.000000000000000000, 0.000000000000000000 ) ) ;
#91036 = DIRECTION ( 'NONE',  ( -1.000000000000000000, 0.000000000000000000, 0.000000000000000000 ) ) ;
#91037 = CARTESIAN_POINT ( 'NONE',  ( -46.00000000000000000, 438.0652200859154846, 14.81161132415559223 ) ) ;
#91038 = CARTESIAN_POINT ( 'NONE',  ( -3.400000000000000355, 4.163799117101001052E-16, -0.7408754770741831086 ) ) ;
#91039 = CARTESIAN_POINT ( 'NONE',  ( 33.09999999999999432, 1.533819458162526451E-15, 0.000000000000000000 ) ) ;
#91040 = CARTESIAN_POINT ( 'NONE',  ( 6.928203230275507885, -65.00000000000000000, 4.000000000000002665 ) ) ;
#91041 = CARTESIAN_POINT ( 'NONE',  ( 4.699999999999999289, -7.505553499465137612, 3.546421054897781431E-16 ) ) ;
#91042 = CARTESIAN_POINT ( 'NONE',  ( 86.18625139326670137, -24.72646195496230703, 181.0545054023034481 ) ) ;
#91043 =( GEOMETRIC_REPRESENTATION_CONTEXT ( 3 ) GLOBAL_UNCERTAINTY_ASSIGNED_CONTEXT ( ( #35425 ) ) GLOBAL_UNIT_ASSIGNED_CONTEXT ( ( #73187, #81809, #101217 ) ) REPRESENTATION_CONTEXT ( 'NONE', 'WORKASPACE' ) );
#91044 = CYLINDRICAL_SURFACE ( 'NONE', #6758, 5.000000000000000888 ) ;
#91045 = CARTESIAN_POINT ( 'NONE',  ( 27.99999999999999645, 0.000000000000000000, 0.000000000000000000 ) ) ;
#91046 = ORIENTED_EDGE ( 'NONE', *, *, #52159, .T. ) ;
#91047 = CARTESIAN_POINT ( 'NONE',  ( 93.58048534552796127, -57.65383078522462057, -15.61220460149725575 ) ) ;
#91048 = FACE_OUTER_BOUND ( 'NONE', #6466, .T. ) ;
#91049 = DIRECTION ( 'NONE',  ( -3.673940397442057649E-17, 0.000000000000000000, -1.000000000000000000 ) ) ;
#91050 = CARTESIAN_POINT ( 'NONE',  ( 8.000000000000000000, -18.49999999999999289, 0.000000000000000000 ) ) ;
#91051 = CARTESIAN_POINT ( 'NONE',  ( -81.58955636323381100, -30.00000000000000711, -7.351077512096740207 ) ) ;
#91052 = B_SPLINE_CURVE_WITH_KNOTS ( 'NONE', 3,
 ( #24360, #23288, #89066, #14618 ),
 .UNSPECIFIED., .F., .F.,
 ( 4, 4 ),
 ( 0.000000000000000000, 0.01132017942645960167 ),
 .UNSPECIFIED. ) ;
#91053 = CONICAL_SURFACE ( 'NONE', #11798, 4.000000000000001776, 0.9599310885968808105 ) ;
#91054 =( LENGTH_UNIT ( ) NAMED_UNIT ( * ) SI_UNIT ( .MILLI., .METRE. ) );
#91055 = CARTESIAN_POINT ( 'NONE',  ( 22.45459161911025348, 27.61281158839761574, -32.95901622140775089 ) ) ;
#91056 = CARTESIAN_POINT ( 'NONE',  ( -46.00000000000000000, 500.0000000000002274, 0.000000000000000000 ) ) ;
#91058 = CARTESIAN_POINT ( 'NONE',  ( 0.000000000000000000, 0.000000000000000000, 5.000000000000002665 ) ) ;
#91057 = CARTESIAN_POINT ( 'NONE',  ( -32.88333705524179607, 439.7317646416724415, 24.13381181826117583 ) ) ;
#91059 = EDGE_CURVE ( 'NONE', #34601, #5811, #5079, .T. ) ;
#91060 = DIRECTION ( 'NONE',  ( 0.000000000000000000, 0.000000000000000000, 1.000000000000000000 ) ) ;
#91061 = CARTESIAN_POINT ( 'NONE',  ( -31.56707703923818187, 439.0034412535504771, 23.33584616512316501 ) ) ;
#91062 = CARTESIAN_POINT ( 'NONE',  ( 4.472135954999579610, -85.00000000000000000, 4.000000000000001776 ) ) ;
#91063 = CARTESIAN_POINT ( 'NONE',  ( -22.25750210340301649, 26.06517743502978846, 31.15121832242501299 ) ) ;
#91064 = DIRECTION ( 'NONE',  ( -0.5735764363510510444, -0.8191520442889883569, 0.000000000000000000 ) ) ;
#91065 = B_SPLINE_CURVE_WITH_KNOTS ( 'NONE', 3,
 ( #83035, #1558, #35047, #19415, #52249, #85159, #100798, #26958, #25359, #92712, #99744, #17782, #9126, #68455, #34523, #74918, #59840, #1002 ),
 .UNSPECIFIED., .F., .F.,
 ( 4, 2, 2, 2, 2, 2, 2, 2, 4 ),
 ( 0.007258363042094923348, 0.007762330413277810856, 0.008266297784460696629, 0.008770265155643584137, 0.009274232526826471645, 0.009778199898009359153, 0.01028216726919224666, 0.01078613464037513243, 0.01129010201155801994 ),
 .UNSPECIFIED. ) ;
#91066 = AXIS2_PLACEMENT_3D ( 'NONE', #10036, #106055, #97982 ) ;
#91067 = CARTESIAN_POINT ( 'NONE',  ( 83.28888888888889142, 1.023464760207051730E-14, 0.000000000000000000 ) ) ;
#91068 = EDGE_LOOP ( 'NONE', ( #51113, #17474 ) ) ;
#91069 = CARTESIAN_POINT ( 'NONE',  ( 6.880814520906024079, 9.211466042846859992, 1.310034959478669547 ) ) ;
#91070 = DIRECTION ( 'NONE',  ( -0.000000000000000000, -1.000000000000000000, -0.000000000000000000 ) ) ;
#91071 = CARTESIAN_POINT ( 'NONE',  ( -7.619753052866896859, 81.82548497192826176, -2.447276542590445914 ) ) ;
#91072 = CARTESIAN_POINT ( 'NONE',  ( -55.69463391236389782, -28.61016029938631533, -26.37040716894560077 ) ) ;
#91073 = ADVANCED_FACE ( 'NONE', ( #94088 ), #41313, .T. ) ;
#91075 = CARTESIAN_POINT ( 'NONE',  ( -68.19771576902743959, -21.77019576768154252, -20.22133746935010024 ) ) ;
#91074 = LINE ( 'NONE', #82430, #17439 ) ;
#91076 = ORIENTED_EDGE ( 'NONE', *, *, #89043, .F. ) ;
#91077 = FILL_AREA_STYLE_COLOUR ( '', #56491 ) ;
#91078 = ORIENTED_EDGE ( 'NONE', *, *, #65697, .T. ) ;
#91079 = CARTESIAN_POINT ( 'NONE',  ( 4.142849616820252293E-15, 27.68727484027578356, 33.82893434829263413 ) ) ;
#91080 = EDGE_CURVE ( 'NONE', #5811, #84521, #93062, .T. ) ;
#91081 = DIRECTION ( 'NONE',  ( -1.000000000000000000, -1.224606353822377258E-16, -0.000000000000000000 ) ) ;
#91082 = CARTESIAN_POINT ( 'NONE',  ( -67.48012074439532171, -60.00000000000000000, -33.40833613135792035 ) ) ;
#91083 = ORIENTED_EDGE ( 'NONE', *, *, #8935, .T. ) ;
#91084 = CARTESIAN_POINT ( 'NONE',  ( 65.56157315575767086, -37.85303547496034327, -24.10004436282220297 ) ) ;
#91085 = CARTESIAN_POINT ( 'NONE',  ( -9.090810276835252779, 294.6686654934159151, -4.204479076929215076 ) ) ;
#91086 = STYLED_ITEM ( 'NONE', ( #88794 ), #40131 ) ;
#91087 = CARTESIAN_POINT ( 'NONE',  ( 102.5332414093125379, -60.18420180869041047, 193.5345815919327492 ) ) ;
#91089 = CARTESIAN_POINT ( 'NONE',  ( -16.64348903516517098, 45.60392139269950462, 6.657797401561654560 ) ) ;
#91088 = CARTESIAN_POINT ( 'NONE',  ( 31.43263229211846266, -31.27596996767818993, 32.16362705870713512 ) ) ;
#91090 = ADVANCED_FACE ( 'NONE', ( #38523 ), #69811, .F. ) ;
#91091 = ORIENTED_EDGE ( 'NONE', *, *, #13899, .T. ) ;
#91092 = ORIENTED_EDGE ( 'NONE', *, *, #65003, .F. ) ;
#91093 = ORIENTED_EDGE ( 'NONE', *, *, #54776, .T. ) ;
#91094 = CARTESIAN_POINT ( 'NONE',  ( 29.58258320683665232, 319.4038838472506541, 13.76509249064623752 ) ) ;
#91095 = CARTESIAN_POINT ( 'NONE',  ( 15.65186372275026017, 46.18633577147563329, 4.642160826816592589 ) ) ;
#91096 = ORIENTED_EDGE ( 'NONE', *, *, #73513, .T. ) ;
#91097 = CARTESIAN_POINT ( 'NONE',  ( -43.17378635869611259, 487.6240912981934343, 8.491167829017486568 ) ) ;
#91098 = SURFACE_SIDE_STYLE ('',( #2589 ) ) ;
#91099 = CIRCLE ( 'NONE', #75521, 7.000000000000000000 ) ;
#91100 = CARTESIAN_POINT ( 'NONE',  ( 4.699999999999999289, 3.752776749732553263, -6.499999999999999112 ) ) ;
#91101 = CARTESIAN_POINT ( 'NONE',  ( -47.68231610104891871, -57.68007204195236426, 71.30078553503261674 ) ) ;
#91102 = CARTESIAN_POINT ( 'NONE',  ( 7.188101187500001821, -32.56250000204838813, -2.977408999572650483 ) ) ;
#91103 = CARTESIAN_POINT ( 'NONE',  ( 6.837824896291514243, 3.947820044545422569, -6.564402953523715389 ) ) ;
#91104 = AXIS2_PLACEMENT_3D ( 'NONE', #56522, #31757, #72715 ) ;
#91105 = DIRECTION ( 'NONE',  ( 0.5735764363510462704, 0.8191520442889915765, 0.000000000000000000 ) ) ;
#91106 = CARTESIAN_POINT ( 'NONE',  ( 43.00000000000000000, 450.0000000000002274, 13.20242257375370976 ) ) ;
#91107 = CARTESIAN_POINT ( 'NONE',  ( 34.13661050418165388, -59.99999999999998579, -42.84071489294807122 ) ) ;
#91108 = CARTESIAN_POINT ( 'NONE',  ( 6.249999999999998224, 6.928203230275505220, 4.000000000000006217 ) ) ;
#91109 = CIRCLE ( 'NONE', #104880, 5.000000000000001776 ) ;
#91110 = CARTESIAN_POINT ( 'NONE',  ( -51.42996021425486219, -36.04690667729754949, 52.01100956484014404 ) ) ;
#91111 = MECHANICAL_DESIGN_GEOMETRIC_PRESENTATION_REPRESENTATION (  '', ( #101414 ), #30844 ) ;
#91112 = DIRECTION ( 'NONE',  ( -1.000000000000000000, -1.224606353822377258E-16, -0.000000000000000000 ) ) ;
#91113 = VERTEX_POINT ( 'NONE', #78421 ) ;
#91114 = CARTESIAN_POINT ( 'NONE',  ( -97.51575089595564805, -45.25067345593495105, 193.9083865710881014 ) ) ;
#91115 = DIRECTION ( 'NONE',  ( -1.000000000000000000, -0.000000000000000000, -0.000000000000000000 ) ) ;
#91116 = AXIS2_PLACEMENT_3D ( 'NONE', #8836, #41741, #705 ) ;
#91117 = CARTESIAN_POINT ( 'NONE',  ( 13.08519678395057184, 1.516754868601839501, 14.92392294744104575 ) ) ;
#91118 = ORIENTED_EDGE ( 'NONE', *, *, #75125, .T. ) ;
#91119 = CARTESIAN_POINT ( 'NONE',  ( -16.96405139844710064, 43.37130063886583997, 6.627052614058375646 ) ) ;
#91120 = AXIS2_PLACEMENT_3D ( 'NONE', #14687, #96696, #63808 ) ;
#91121 = CARTESIAN_POINT ( 'NONE',  ( 85.87629844180868588, -38.64549821753008985, 199.0215093646828279 ) ) ;
#91122 = CARTESIAN_POINT ( 'NONE',  ( 2.785715769379251079E-15, -7.693917458112937702, -6.460793508093594539 ) ) ;
#91123 = CARTESIAN_POINT ( 'NONE',  ( 34.35000000000000142, 1.533819458162526451E-15, 0.000000000000000000 ) ) ;
#91124 = DIRECTION ( 'NONE',  ( -1.000000000000000000, 0.000000000000000000, 0.000000000000000000 ) ) ;
#91125 = CARTESIAN_POINT ( 'NONE',  ( -11.85444436800005263, 42.00000000000000000, 90.56128410203886858 ) ) ;
#91126 = CARTESIAN_POINT ( 'NONE',  ( 84.03161318001124869, -30.00000000000000000, 161.2884451932859520 ) ) ;
#91127 = B_SPLINE_SURFACE_WITH_KNOTS ( 'NONE', 1, 3, ( 
 ( #63805, #105311, #15230, #64335, #31453, #31970, #7133, #40044, #47058, #40569, #32511, #22300, #98274, #15762, #72918, #105828, #56738, #89663, #24432, #57264, #55146, #90187, #46543, #79958, #79436, #38994, #38474, #71340 ),
 ( #104235, #30383, #63272, #49174, #91269, #597, #90723, #10319, #57799, #100927, #24946, #75042, #41108, #16837, #75593, #49719, #82627, #33562, #8729, #27088, #99867, #83673, #100397, #41637, #67517, #74520, #84224, #66438 ) ),
 .UNSPECIFIED., .F., .F., .F.,
 ( 2, 2 ),
 ( 4, 2, 2, 2, 2, 2, 2, 2, 2, 2, 2, 2, 2, 4 ),
 ( 0.000000000000000000, 1.000000000000000000 ),
 ( 0.08901491201581737678, 0.1032490540155679704, 0.1174831960153185778, 0.1317173380150691853, 0.1459514800148197788, 0.1744197640143299588, 0.2028880480138401388, 0.2598246160128514504, 0.3167611840118632616, 0.4306343200098861623, 0.5445074560079088410, 0.6583805920059359051, 0.7722537280039543095, 1.000000000000000000 ),
 .UNSPECIFIED. ) ;
#91128 = CARTESIAN_POINT ( 'NONE',  ( 35.91982565306800979, 490.8454349930378271, 12.40602332252425377 ) ) ;
#91129 = CARTESIAN_POINT ( 'NONE',  ( -34.84533357024655231, 490.9234226268542898, 11.68321824384988972 ) ) ;
#91130 = FACE_OUTER_BOUND ( 'NONE', #37436, .T. ) ;
#91131 = ORIENTED_EDGE ( 'NONE', *, *, #69696, .T. ) ;
#91132 = ORIENTED_EDGE ( 'NONE', *, *, #103254, .F. ) ;
#91133 = CARTESIAN_POINT ( 'NONE',  ( 52.51395162811751050, -36.03863491630684024, 53.95531543791132378 ) ) ;
#91134 = CARTESIAN_POINT ( 'NONE',  ( -4.925922214360547891, 301.1861782522827866, -10.01402241915593372 ) ) ;
#91135 = CARTESIAN_POINT ( 'NONE',  ( 0.000000000000000000, 0.000000000000000000, -12.97459999999999525 ) ) ;
#91136 = EDGE_CURVE ( 'NONE', #99943, #65781, #60678, .T. ) ;
#91137 = VERTEX_POINT ( 'NONE', #28872 ) ;
#91138 = CARTESIAN_POINT ( 'NONE',  ( -90.66024329338046073, -38.34389756899053481, 8.992944879562799088 ) ) ;
#91139 = VERTEX_POINT ( 'NONE', #3488 ) ;
#91140 = DIRECTION ( 'NONE',  ( 0.000000000000000000, 1.000000000000000000, 0.000000000000000000 ) ) ;
#91141 = CARTESIAN_POINT ( 'NONE',  ( 105.3748507632057283, -38.35594986074055157, 120.2417250538963884 ) ) ;
#91142 = CARTESIAN_POINT ( 'NONE',  ( 12.32648393225135486, 22.38102541151338087, -6.322412828060416601 ) ) ;
#91143 = CARTESIAN_POINT ( 'NONE',  ( 85.09281517647455928, -52.71298583903853796, 20.05580076196299899 ) ) ;
#91144 = CARTESIAN_POINT ( 'NONE',  ( -31.03561048997209681, 439.3357289228141553, 22.68171793430912686 ) ) ;
#91146 = STYLED_ITEM ( 'NONE', ( #20740 ), #12512 ) ;
#91145 = CARTESIAN_POINT ( 'NONE',  ( 4.651132217449188921, -5.000000000000000000, -15.66661053588737751 ) ) ;
#91147 = CARTESIAN_POINT ( 'NONE',  ( -33.13240178283476212, 323.0802024858354002, -5.539852619051230498 ) ) ;
#91148 = SURFACE_SIDE_STYLE ('',( #58772 ) ) ;
#91149 = CARTESIAN_POINT ( 'NONE',  ( 74.36297015317659032, -59.99999999999999289, 175.8144878597308889 ) ) ;
#91150 = ADVANCED_FACE ( 'NONE', ( #77372 ), #5223, .T. ) ;
#91151 =( BOUNDED_SURFACE ( )  B_SPLINE_SURFACE ( 3, 2, ( 
 ( #101474, #3306, #101994 ),
 ( #66989, #32847, #66247 ),
 ( #82436, #57604, #99129 ),
 ( #75400, #41970, #32314 ) ),
 .UNSPECIFIED., .F., .F., .F. ) 
 B_SPLINE_SURFACE_WITH_KNOTS ( ( 4, 4 ),
 ( 3, 3 ),
 ( 1.474514954580286030E-17, 0.001313222278771296152 ),
 ( 0.000000000000000000, 1.000000000000000000 ),
 .UNSPECIFIED. ) 
 GEOMETRIC_REPRESENTATION_ITEM ( )  RATIONAL_B_SPLINE_SURFACE ( (
 ( 1.000000000000000000, 0.8270258197359552366, 1.000000000000000000),
 ( 1.000000000000000000, 0.8180084242886545010, 1.000000000000000000),
 ( 1.000000000000000000, 0.8088315090908722027, 1.000000000000000000),
 ( 1.000000000000000000, 0.7996726260853299628, 1.000000000000000000) ) ) 
 REPRESENTATION_ITEM ( '' )  SURFACE ( )  );
#91152 = CARTESIAN_POINT ( 'NONE',  ( 17.61582496125343411, 45.00000000000001421, 63.05442575584599751 ) ) ;
#91153 = EDGE_LOOP ( 'NONE', ( #84369, #92420, #8040, #46245, #50307, #73818, #66645 ) ) ;
#91154 = CARTESIAN_POINT ( 'NONE',  ( 61.58695439658515625, -56.86329823613085210, 85.14614063634395791 ) ) ;
#91155 = EDGE_CURVE ( 'NONE', #93202, #35657, #19045, .T. ) ;
#91156 = CARTESIAN_POINT ( 'NONE',  ( -23.10650858598700452, 303.3356527799805917, -9.896241053147848632 ) ) ;
#91157 = CARTESIAN_POINT ( 'NONE',  ( 9.226722513859208163, -53.47035606567975918, 23.14374324513729064 ) ) ;
#91158 = CARTESIAN_POINT ( 'NONE',  ( 14.85284876471456350, 1.482358050883964840E-15, 0.000000000000000000 ) ) ;
#91160 = CARTESIAN_POINT ( 'NONE',  ( -38.81358894279936322, 485.1131561813189705, -4.191378885295510948 ) ) ;
#91159 = CARTESIAN_POINT ( 'NONE',  ( -84.69403854917420915, -38.35848897778367217, -23.12898730350110554 ) ) ;
#91161 = EDGE_CURVE ( 'NONE', #22579, #54135, #37972, .T. ) ;
#91162 = CARTESIAN_POINT ( 'NONE',  ( -40.95806866577292027, 396.9764538775766596, 27.65151128674859393 ) ) ;
#91163 = CARTESIAN_POINT ( 'NONE',  ( -37.72544201219972848, 25.42175550654698313, -13.45617127781035016 ) ) ;
#91164 = CARTESIAN_POINT ( 'NONE',  ( 7.999999999999998224, -23.09374999999999645, 3.313708498984766049 ) ) ;
#91165 = CARTESIAN_POINT ( 'NONE',  ( -8.000000000000000000, -26.84374999999998934, -3.313708498984762496 ) ) ;
#91166 = DIRECTION ( 'NONE',  ( -1.000000000000000000, -0.000000000000000000, -0.000000000000000000 ) ) ;
#91167 = AXIS2_PLACEMENT_3D ( 'NONE', #24060, #64498, #14322 ) ;
#91168 = AXIS2_PLACEMENT_3D ( 'NONE', #10898, #76177, #44359 ) ;
#91169 = STYLED_ITEM ( 'NONE', ( #35305 ), #102736 ) ;
#91170 = DIRECTION ( 'NONE',  ( -1.000000000000000000, -1.224606353822377258E-16, -0.000000000000000000 ) ) ;
#91171 = ORIENTED_EDGE ( 'NONE', *, *, #59351, .F. ) ;
#91172 = CARTESIAN_POINT ( 'NONE',  ( 85.02604456486491813, -28.87707945974564794, 172.9526225289325509 ) ) ;
#91173 = CARTESIAN_POINT ( 'NONE',  ( 0.000000000000000000, 115.0000000000000000, 0.000000000000000000 ) ) ;
#91174 = CARTESIAN_POINT ( 'NONE',  ( 13.37207953394533355, 5.000000000000003553, 0.000000000000000000 ) ) ;
#91175 = VERTEX_POINT ( 'NONE', #13680 ) ;
#91176 = CARTESIAN_POINT ( 'NONE',  ( 0.000000000000000000, 0.000000000000000000, 0.000000000000000000 ) ) ;
#91177 = CARTESIAN_POINT ( 'NONE',  ( 35.11650669486618170, 1.474610560812782335E-15, 0.000000000000000000 ) ) ;
#91178 = CARTESIAN_POINT ( 'NONE',  ( -32.93513049338655918, 465.6726574193328929, 10.66039033145153425 ) ) ;
#91179 = FACE_OUTER_BOUND ( 'NONE', #103160, .T. ) ;
#91180 = CARTESIAN_POINT ( 'NONE',  ( -34.74080303120308599, -31.24499895687540274, -37.89147051442173364 ) ) ;
#91181 = CARTESIAN_POINT ( 'NONE',  ( -12.37144696128342147, -4.000000000000003553, 20.44658103856077602 ) ) ;
#91182 = MECHANICAL_DESIGN_GEOMETRIC_PRESENTATION_REPRESENTATION (  '', ( #72218 ), #67000 ) ;
#91183 = CARTESIAN_POINT ( 'NONE',  ( 53.65548343568850242, -60.00000000000000711, 81.46444441885545018 ) ) ;
#91184 = VECTOR ( 'NONE', #41946, 1000.000000000000000 ) ;
#91185 = CARTESIAN_POINT ( 'NONE',  ( 7.213352437320215138, 107.0183647300768257, -3.463014597543483841 ) ) ;
#91186 = CARTESIAN_POINT ( 'NONE',  ( 28.19983488487488188, -20.81563479387831350, 31.87448879475714136 ) ) ;
#91188 = CARTESIAN_POINT ( 'NONE',  ( -15.54108745661637769, 22.95061784590342668, 1.145812418174521952 ) ) ;
#91187 = CARTESIAN_POINT ( 'NONE',  ( -15.78206918482793952, -23.13227408766112347, 36.04868682780729472 ) ) ;
#91189 = EDGE_CURVE ( 'NONE', #17567, #41746, #20250, .T. ) ;
#91190 = CARTESIAN_POINT ( 'NONE',  ( -2.977408999572650039, -11.18750000204838457, -7.188101187500001821 ) ) ;
#91191 = PRESENTATION_STYLE_ASSIGNMENT (( #58266 ) ) ;
#91192 = CARTESIAN_POINT ( 'NONE',  ( 13.50000000000000355, 7.794228634059978233, -1.205771365940065953 ) ) ;
#91193 = VECTOR ( 'NONE', #11900, 999.9999999999998863 ) ;
#91194 = ORIENTED_EDGE ( 'NONE', *, *, #103518, .F. ) ;
#91195 = CARTESIAN_POINT ( 'NONE',  ( -17.49999999999999289, 48.58944628575790148, 64.09148194233866036 ) ) ;
#91196 =( NAMED_UNIT ( * ) SI_UNIT ( $, .STERADIAN. ) SOLID_ANGLE_UNIT ( ) );
#91197 = SURFACE_SIDE_STYLE ('',( #25965 ) ) ;
#91198 = EDGE_CURVE ( 'NONE', #71461, #100372, #39654, .T. ) ;
#91200 = CARTESIAN_POINT ( 'NONE',  ( 56.92553280862420451, -47.40888104890370869, -28.31668682213464550 ) ) ;
#91199 = CARTESIAN_POINT ( 'NONE',  ( 8.000000000000000000, 9.797174393178825657E-16, -3.725171428571429022 ) ) ;
#91201 = VERTEX_POINT ( 'NONE', #95160 ) ;
#91202 = MECHANICAL_DESIGN_GEOMETRIC_PRESENTATION_REPRESENTATION (  '', ( #75706 ), #77407 ) ;
#91203 = CARTESIAN_POINT ( 'NONE',  ( 31.08349330513380337, 1.593028355512270567E-15, 0.000000000000000000 ) ) ;
#91204 = CARTESIAN_POINT ( 'NONE',  ( -4.044114467841184890, 52.00960197897231296, 7.152013030799439619 ) ) ;
#91205 = VERTEX_POINT ( 'NONE', #36944 ) ;
#91206 = SURFACE_STYLE_FILL_AREA ( #58279 ) ;
#91207 = CARTESIAN_POINT ( 'NONE',  ( 12.13034742782427955, 48.00000000000000000, -93.82352941176471006 ) ) ;
#91208 = AXIS2_PLACEMENT_3D ( 'NONE', #14137, #3950, #45483 ) ;
#91209 = CARTESIAN_POINT ( 'NONE',  ( -23.97981144771549467, 41.62095615380706448, -74.33343198471487767 ) ) ;
#91210 = CARTESIAN_POINT ( 'NONE',  ( -103.7767948193627490, -59.99999999999998579, 103.1325596424688058 ) ) ;
#91211 = CARTESIAN_POINT ( 'NONE',  ( 28.45521705596386397, 17.07436234393351171, -41.11936415921402954 ) ) ;
#91212 = CARTESIAN_POINT ( 'NONE',  ( -43.89279753500660064, 435.4168038201347599, 16.20034641759655258 ) ) ;
#91213 = CARTESIAN_POINT ( 'NONE',  ( 35.44563196690202744, 355.0508310518326311, 1.542887188955126110 ) ) ;
#91214 = CARTESIAN_POINT ( 'NONE',  ( 39.86761651079377344, 459.8416857619859570, 1.882458089123050904 ) ) ;
#91216 = CARTESIAN_POINT ( 'NONE',  ( -5.363597346089342466, 41.33266196706077267, -58.39526881795508473 ) ) ;
#91215 = CARTESIAN_POINT ( 'NONE',  ( -35.45036406932369033, 436.3203772529674893, 5.179456583041581297 ) ) ;
#91217 = EDGE_CURVE ( 'NONE', #50622, #20770, #103384, .T. ) ;
#91218 = AXIS2_PLACEMENT_3D ( 'NONE', #78583, #37651, #87760 ) ;
#91219 = CARTESIAN_POINT ( 'NONE',  ( -80.54720188594731667, -60.43838022186359638, 180.0448206866681176 ) ) ;
#91220 = ORIENTED_EDGE ( 'NONE', *, *, #29060, .F. ) ;
#91221 = CARTESIAN_POINT ( 'NONE',  ( -43.63899620156483650, 434.3182181978405652, 14.37213632273153330 ) ) ;
#91222 = ORIENTED_EDGE ( 'NONE', *, *, #8848, .T. ) ;
#91223 = ORIENTED_EDGE ( 'NONE', *, *, #22137, .F. ) ;
#91224 = CARTESIAN_POINT ( 'NONE',  ( 17.33349330513380693, 1.593028355512270962E-15, 0.000000000000000000 ) ) ;
#91225 = EDGE_CURVE ( 'NONE', #42316, #89611, #59920, .T. ) ;
#91226 = CARTESIAN_POINT ( 'NONE',  ( -7.000000000000000000, 8.572527594031471218E-16, -13.00000000000000000 ) ) ;
#91227 = ORIENTED_EDGE ( 'NONE', *, *, #61755, .F. ) ;
#91228 = CARTESIAN_POINT ( 'NONE',  ( -19.83463548332443338, 303.8035096162418540, 9.926734387303303819 ) ) ;
#91229 = CARTESIAN_POINT ( 'NONE',  ( -6.837824896291513355, -3.947820044545450102, -6.564402953523720718 ) ) ;
#91230 = CARTESIAN_POINT ( 'NONE',  ( -7.551892080562056186, -61.99012297460618726, 2.647003822403979356 ) ) ;
#91231 = CARTESIAN_POINT ( 'NONE',  ( 43.33854370778465182, 463.6229669622573510, 5.371557844377655933 ) ) ;
#91232 = CARTESIAN_POINT ( 'NONE',  ( 5.799999999999999822, -6.928203230275510549, -3.999999999999997335 ) ) ;
#91233 = CARTESIAN_POINT ( 'NONE',  ( -5.000000000000000000, 0.000000000000000000, -1.446714285714285841 ) ) ;
#91234 = AXIS2_PLACEMENT_3D ( 'NONE', #86151, #95816, #28455 ) ;
#91235 = CARTESIAN_POINT ( 'NONE',  ( 114.5290872765719570, -59.99999999999999289, 168.5341745518089738 ) ) ;
#91236 = CARTESIAN_POINT ( 'NONE',  ( -106.6793529335496515, -14.21045842199435860, 163.7930604915816559 ) ) ;
#91237 = CARTESIAN_POINT ( 'NONE',  ( -58.43140080053613161, -49.91469830724326329, 72.99038015592236661 ) ) ;
#91238 = EDGE_LOOP ( 'NONE', ( #15644, #75148, #5561, #22538, #42738, #10573 ) ) ;
#91239 = CARTESIAN_POINT ( 'NONE',  ( -20.09676425191630500, 38.95313086215059428, 60.48296960500260155 ) ) ;
#91240 = CARTESIAN_POINT ( 'NONE',  ( 103.8610105594060826, -59.99999999999504752, 202.9082511799323640 ) ) ;
#91241 = ORIENTED_EDGE ( 'NONE', *, *, #96371, .T. ) ;
#91242 = CARTESIAN_POINT ( 'NONE',  ( 8.168457008275577635, -39.47263446743016857, 30.46165443850678756 ) ) ;
#91244 = CARTESIAN_POINT ( 'NONE',  ( -104.0415063169905210, -60.15505986368567193, 141.9492927151964068 ) ) ;
#91243 = AXIS2_PLACEMENT_3D ( 'NONE', #85170, #59852, #1014 ) ;
#91245 = CARTESIAN_POINT ( 'NONE',  ( -1.320432766682874540E-15, -13.90625000204838457, 7.188101187500000044 ) ) ;
#91246 = CARTESIAN_POINT ( 'NONE',  ( -20.17756551592432501, 302.8253764644770172, 1.931382329378721119 ) ) ;
#91247 = DIRECTION ( 'NONE',  ( -0.000000000000000000, -0.000000000000000000, -1.000000000000000000 ) ) ;
#91248 = ORIENTED_EDGE ( 'NONE', *, *, #70494, .F. ) ;
#91249 = EDGE_CURVE ( 'NONE', #106280, #88025, #106753, .T. ) ;
#91250 = CARTESIAN_POINT ( 'NONE',  ( -34.12482747856847709, -60.00000000000001421, 45.63882276711500907 ) ) ;
#91251 = CARTESIAN_POINT ( 'NONE',  ( 2.977408999572650927, -17.75000000204838457, -7.188101187500001821 ) ) ;
#91252 = FACE_OUTER_BOUND ( 'NONE', #2035, .T. ) ;
#91253 = DIRECTION ( 'NONE',  ( 0.000000000000000000, -1.000000000000000000, 0.000000000000000000 ) ) ;
#91254 = CARTESIAN_POINT ( 'NONE',  ( 4.418206560264961169, 0.000000000000000000, -16.46930219881951629 ) ) ;
#91255 = DIRECTION ( 'NONE',  ( -1.000000000000000000, -0.000000000000000000, -0.000000000000000000 ) ) ;
#91256 = DIRECTION ( 'NONE',  ( -0.000000000000000000, -1.000000000000000000, -0.000000000000000000 ) ) ;
#91257 = CARTESIAN_POINT ( 'NONE',  ( 5.369276582105083406, -15.91634619257528627, 14.07054258737598573 ) ) ;
#91258 = CARTESIAN_POINT ( 'NONE',  ( -1.000000000000000000, -69.59657292933731298, 12.76848391598547394 ) ) ;
#91259 = CARTESIAN_POINT ( 'NONE',  ( 106.4812587873048386, -60.00000000000000711, 170.6759392298722844 ) ) ;
#91260 = CARTESIAN_POINT ( 'NONE',  ( -32.30208268559946561, -18.68134237623966243, 30.13613988364853569 ) ) ;
#91261 = CARTESIAN_POINT ( 'NONE',  ( 43.31019682569796458, -49.88810819673993535, 44.39210588798376023 ) ) ;
#91262 = CYLINDRICAL_SURFACE ( 'NONE', #59286, 4.000000000000000888 ) ;
#91263 = EDGE_LOOP ( 'NONE', ( #52888, #49279, #31469, #99588 ) ) ;
#91264 = CARTESIAN_POINT ( 'NONE',  ( 43.72886361455203996, 434.3043191536616519, 13.94145212282615631 ) ) ;
#91265 = AXIS2_PLACEMENT_3D ( 'NONE', #3092, #78046, #59752 ) ;
#91266 = CARTESIAN_POINT ( 'NONE',  ( -78.45100946094439109, -38.62822479361768302, 189.5449468668735449 ) ) ;
#91267 = ORIENTED_EDGE ( 'NONE', *, *, #9971, .T. ) ;
#91269 = CARTESIAN_POINT ( 'NONE',  ( 27.18908553330205180, 296.5274986157688772, 10.30015177545897842 ) ) ;
#91268 = CARTESIAN_POINT ( 'NONE',  ( 42.33349330513380693, 4.000000000000002665, 0.000000000000000000 ) ) ;
#91270 = CARTESIAN_POINT ( 'NONE',  ( 41.33432493934709129, -60.00000000000001421, 44.56932545367675402 ) ) ;
#91271 = DIRECTION ( 'NONE',  ( -0.000000000000000000, -0.000000000000000000, -1.000000000000000000 ) ) ;
#91272 = CARTESIAN_POINT ( 'NONE',  ( -43.03894652950290123, 464.9992092536287487, 11.55502599541316044 ) ) ;
#91273 = DIRECTION ( 'NONE',  ( -1.000000000000000000, -1.224606353822377258E-16, -0.000000000000000000 ) ) ;
#91274 = CARTESIAN_POINT ( 'NONE',  ( 0.000000000000000000, 0.000000000000000000, 0.000000000000000000 ) ) ;
#91275 = CARTESIAN_POINT ( 'NONE',  ( -30.96044075740587331, 348.7637019778929357, 19.04753708084649233 ) ) ;
#91276 =( GEOMETRIC_REPRESENTATION_CONTEXT ( 3 ) GLOBAL_UNCERTAINTY_ASSIGNED_CONTEXT ( ( #22429 ) ) GLOBAL_UNIT_ASSIGNED_CONTEXT ( ( #52356, #21625, #46404 ) ) REPRESENTATION_CONTEXT ( 'NONE', 'WORKASPACE' ) );
#91277 = CARTESIAN_POINT ( 'NONE',  ( 108.6217454145117074, -59.99999999999999289, 133.3216537659859000 ) ) ;
#91278 = CARTESIAN_POINT ( 'NONE',  ( -1.725809793176851681, -53.91240363267208124, 40.89521640499670241 ) ) ;
#91279 = EDGE_CURVE ( 'NONE', #22572, #54691, #102308, .T. ) ;
#91280 = SURFACE_STYLE_FILL_AREA ( #18461 ) ;
#91281 = CIRCLE ( 'NONE', #58549, 5.000000000000002665 ) ;
#91282 = VERTEX_POINT ( 'NONE', #80009 ) ;
#91283 = EDGE_CURVE ( 'NONE', #17325, #50186, #55081, .T. ) ;
#91284 = CARTESIAN_POINT ( 'NONE',  ( -97.66629619665867779, -29.99999999999996447, 190.7960662493706536 ) ) ;
#91285 = ORIENTED_EDGE ( 'NONE', *, *, #88792, .F. ) ;
#91286 = DIRECTION ( 'NONE',  ( 0.000000000000000000, 1.000000000000000000, 0.000000000000000000 ) ) ;
#91287 = CARTESIAN_POINT ( 'NONE',  ( 28.53554096041415988, 313.9464476106043662, 12.39025823560460537 ) ) ;
#91288 = CARTESIAN_POINT ( 'NONE',  ( 9.948513602187993854, 26.13022056656141245, 1.045942665286129003 ) ) ;
#91289 = CARTESIAN_POINT ( 'NONE',  ( 7.188101187500000044, -21.03125000204838813, 0.000000000000000000 ) ) ;
#91290 = EDGE_CURVE ( 'NONE', #9148, #38226, #60295, .T. ) ;
#91291 = CARTESIAN_POINT ( 'NONE',  ( 7.319240905726694280, 40.56016492320068068, -70.61401732095062300 ) ) ;
#91292 = AXIS2_PLACEMENT_3D ( 'NONE', #61544, #29207, #36759 ) ;
#91293 = VERTEX_POINT ( 'NONE', #49227 ) ;
#91294 = CARTESIAN_POINT ( 'NONE',  ( 81.74723224102429242, -42.96870066486594908, 163.6216033774333880 ) ) ;
#91295 = CIRCLE ( 'NONE', #24180, 3.309500000000007880 ) ;
#91296 = FACE_OUTER_BOUND ( 'NONE', #21031, .T. ) ;
#91297 = FILL_AREA_STYLE ('',( #50797 ) ) ;
#91298 = ORIENTED_EDGE ( 'NONE', *, *, #58100, .F. ) ;
#91299 = DIRECTION ( 'NONE',  ( -1.000000000000000000, -1.224606353822377258E-16, -0.000000000000000000 ) ) ;
#91300 = CARTESIAN_POINT ( 'NONE',  ( -0.5272038479004254041, 18.60450536692893664, -49.36031152383475273 ) ) ;
#91301 = CARTESIAN_POINT ( 'NONE',  ( -3.594033448928638741, -9.156975712238445197, 6.225088131883843801 ) ) ;
#91302 = CARTESIAN_POINT ( 'NONE',  ( 0.000000000000000000, 0.000000000000000000, -13.00000000000000000 ) ) ;
#91303 = CARTESIAN_POINT ( 'NONE',  ( -5.094000037296072314, 252.4463412377122609, -3.174960020027671970 ) ) ;
#91304 = CARTESIAN_POINT ( 'NONE',  ( -32.97750030479636507, 361.8904936952960725, 22.71549378251080853 ) ) ;
#91305 = CARTESIAN_POINT ( 'NONE',  ( -32.81992448453860334, 465.7192846569213884, 11.17271167765305862 ) ) ;
#91306 = ORIENTED_EDGE ( 'NONE', *, *, #51329, .F. ) ;
#91307 =( NAMED_UNIT ( * ) PLANE_ANGLE_UNIT ( ) SI_UNIT ( $, .RADIAN. ) );
#91308 = CARTESIAN_POINT ( 'NONE',  ( -6.499999999999999112, -3.752776749732595452, -0.7999999999999977129 ) ) ;
#91309 = SURFACE_SIDE_STYLE ('',( #60543 ) ) ;
#91310 = CARTESIAN_POINT ( 'NONE',  ( 86.99289245865087139, -28.01648969556236679, 186.8500900893037340 ) ) ;
#91311 = CARTESIAN_POINT ( 'NONE',  ( 19.00000000000001066, -4.000000000000000000, -1.500000000000001332 ) ) ;
#91312 = EDGE_CURVE ( 'NONE', #86629, #8148, #22424, .T. ) ;
#91313 = CARTESIAN_POINT ( 'NONE',  ( 5.082755093536325930, -30.96875000204838813, -5.082755093536325042 ) ) ;
#91314 = CARTESIAN_POINT ( 'NONE',  ( 16.51330895492884210, 294.5655680487705013, -2.060813375747557075 ) ) ;
#91315 = CARTESIAN_POINT ( 'NONE',  ( 0.000000000000000000, 38.19193163660327173, 0.000000000000000000 ) ) ;
#91316 = ADVANCED_FACE ( 'NONE', ( #6656 ), #57319, .T. ) ;
#91317 = CARTESIAN_POINT ( 'NONE',  ( 65.52222222222222570, 6.915964383211875250E-15, 0.000000000000000000 ) ) ;
#91318 = ITEM_DEFINED_TRANSFORMATION ( 'NONE', 'NONE', #74787,  #10728 ) ;
#91319 = LINE ( 'NONE', #40100, #33295 ) ;
#91320 = VERTEX_POINT ( 'NONE', #82132 ) ;
#91321 = CARTESIAN_POINT ( 'NONE',  ( 1.012463078293192487, 43.34708279331648839, 18.25106663962358411 ) ) ;
#91322 = DIRECTION ( 'NONE',  ( 1.000000000000000000, 0.000000000000000000, 0.000000000000000000 ) ) ;
#91323 = CARTESIAN_POINT ( 'NONE',  ( -5.892146328597755556, 4.649454379198777687, -5.000000000000000000 ) ) ;
#91324 = EDGE_CURVE ( 'NONE', #59127, #27380, #10977, .T. ) ;
#91325 = CARTESIAN_POINT ( 'NONE',  ( 73.33904886068935980, 6.975173280561618775E-15, 0.000000000000000000 ) ) ;
#91326 = AXIS2_PLACEMENT_3D ( 'NONE', #62454, #47307, #38713 ) ;
#91327 = ORIENTED_EDGE ( 'NONE', *, *, #102621, .F. ) ;
#91328 = DIRECTION ( 'NONE',  ( -1.000000000000000000, -0.000000000000000000, -0.000000000000000000 ) ) ;
#91329 = FILL_AREA_STYLE ('',( #34169 ) ) ;
#91330 = CARTESIAN_POINT ( 'NONE',  ( -4.852941176470593199, 9.833333333333344584, -70.80672828634229177 ) ) ;
#91331 = CARTESIAN_POINT ( 'NONE',  ( 112.4379523079562375, -57.67145323133323132, 146.7647033902477745 ) ) ;
#91332 = AXIS2_PLACEMENT_3D ( 'NONE', #30579, #72593, #6256 ) ;
#91333 = CARTESIAN_POINT ( 'NONE',  ( 5.299999999999999822, 7.505553499465139389, 0.000000000000000000 ) ) ;
#91334 = FACE_BOUND ( 'NONE', #54211, .T. ) ;
#91335 = FILL_AREA_STYLE ('',( #42763 ) ) ;
#91336 = CARTESIAN_POINT ( 'NONE',  ( -76.22964667330261079, -60.00000000000000000, 187.8941157857488520 ) ) ;
#91337 = PLANE ( 'NONE',  #105462 ) ;
#91338 = CARTESIAN_POINT ( 'NONE',  ( 19.70764564238371719, 304.7954121406193622, 9.925013215726785631 ) ) ;
#91339 = CARTESIAN_POINT ( 'NONE',  ( -37.51854390953261742, 313.5286481325095451, 14.45587837336505999 ) ) ;
#91340 = CARTESIAN_POINT ( 'NONE',  ( -85.56701186126900893, -28.63696673469639364, 178.3758072176077860 ) ) ;
#91341 = EDGE_LOOP ( 'NONE', ( #19878, #19953, #58710, #6874 ) ) ;
#91342 = CARTESIAN_POINT ( 'NONE',  ( 25.61872641138599604, 306.5028686783192029, -9.638171963028243638 ) ) ;
#91343 = AXIS2_PLACEMENT_3D ( 'NONE', #90937, #49925, #808 ) ;
#91344 = CIRCLE ( 'NONE', #60411, 10.00000000000000178 ) ;
#91345 = ORIENTED_EDGE ( 'NONE', *, *, #5015, .T. ) ;
#91346 = DIRECTION ( 'NONE',  ( -0.000000000000000000, 1.000000000000000000, -0.000000000000000000 ) ) ;
#91347 = ADVANCED_FACE ( 'NONE', ( #63857 ), #96747, .F. ) ;
#91348 = CARTESIAN_POINT ( 'NONE',  ( -5.232798140227934880, -1.976627073750570673, 104.1190344879413914 ) ) ;
#91349 = CARTESIAN_POINT ( 'NONE',  ( -83.25979992438379895, -37.78815355357362193, -6.773437407079532235 ) ) ;
#91350 = CARTESIAN_POINT ( 'NONE',  ( -15.57484877165060944, 43.91708715447281008, 6.061292577738371712 ) ) ;
#91351 = CARTESIAN_POINT ( 'NONE',  ( 6.125000000000000888, -80.00000000000000000, 14.41094225130411033 ) ) ;
#91352 = CARTESIAN_POINT ( 'NONE',  ( 6.683837171061803417, 3.955946848495959234, -6.851900933636991375 ) ) ;
#91353 = CARTESIAN_POINT ( 'NONE',  ( -29.83308852634790043, 42.00000000000000000, -51.76085035113232635 ) ) ;
#91354 = EDGE_CURVE ( 'NONE', #23483, #90700, #14797, .T. ) ;
#91355 = CARTESIAN_POINT ( 'NONE',  ( -22.00868112945024535, 27.89883671455867287, 32.31191507115328676 ) ) ;
#91356 = AXIS2_PLACEMENT_3D ( 'NONE', #97868, #24024, #17506 ) ;
#91357 = CARTESIAN_POINT ( 'NONE',  ( 34.13661050418165388, -59.99999999999998579, -42.84071489294807122 ) ) ;
#91358 = CARTESIAN_POINT ( 'NONE',  ( -79.51372813587923361, -25.61810700385877126, 129.8594159933582830 ) ) ;
#91359 = ORIENTED_EDGE ( 'NONE', *, *, #78238, .T. ) ;
#91360 = CARTESIAN_POINT ( 'NONE',  ( 58.28796150060976089, -14.21045842199433729, 78.47796032183087789 ) ) ;
#91361 = FACE_OUTER_BOUND ( 'NONE', #15820, .T. ) ;
#91362 = CARTESIAN_POINT ( 'NONE',  ( 113.6418193360469928, -57.67116734740694994, 183.3658933255892123 ) ) ;
#91363 = ORIENTED_EDGE ( 'NONE', *, *, #94348, .F. ) ;
#91364 = CARTESIAN_POINT ( 'NONE',  ( 15.86067392853018632, -3.472586522186453806, 14.59605311390719784 ) ) ;
#91365 = STYLED_ITEM ( 'NONE', ( #27870 ), #70975 ) ;
#91366 = DIRECTION ( 'NONE',  ( 0.000000000000000000, -1.000000000000000000, 0.000000000000000000 ) ) ;
#91367 = ORIENTED_EDGE ( 'NONE', *, *, #30428, .F. ) ;
#91368 = DIRECTION ( 'NONE',  ( 0.000000000000000000, 0.000000000000000000, -1.000000000000000000 ) ) ;
#91369 = EDGE_CURVE ( 'NONE', #51789, #58408, #82668, .T. ) ;
#91370 = CARTESIAN_POINT ( 'NONE',  ( 4.472135954999579610, 249.9999999999999716, -4.000000000000002665 ) ) ;
#91371 = CARTESIAN_POINT ( 'NONE',  ( -2.977408999572650039, -14.18750000204838280, -7.188101187500001821 ) ) ;
#91372 = FACE_OUTER_BOUND ( 'NONE', #68069, .T. ) ;
#91373 = CARTESIAN_POINT ( 'NONE',  ( 1.898590314185344186, -0.1325191295835281280, 102.2339902357106780 ) ) ;
#91374 = FACE_OUTER_BOUND ( 'NONE', #49432, .T. ) ;
#91375 = CARTESIAN_POINT ( 'NONE',  ( -12.47767672221401725, -3.661475206072811517, -13.56848805978015804 ) ) ;
#91376 = CARTESIAN_POINT ( 'NONE',  ( 5.756917790976764593, 48.00000000000000711, -98.90122916984913104 ) ) ;
#91377 = EDGE_LOOP ( 'NONE', ( #15046, #63542 ) ) ;
#91378 = CARTESIAN_POINT ( 'NONE',  ( -7.274973724374026673, 40.00000000004767742, -70.77553044199200372 ) ) ;
#91380 = CARTESIAN_POINT ( 'NONE',  ( 31.80301772498203405, -25.61137255198223883, 31.25798125024838114 ) ) ;
#91379 = CARTESIAN_POINT ( 'NONE',  ( -3.438773559904606980, -49.17061000814768335, 103.7823003339747601 ) ) ;
#91381 = CIRCLE ( 'NONE', #70734, 4.000000000000001776 ) ;
#91382 = CARTESIAN_POINT ( 'NONE',  ( 26.02261751055236516, 306.8105359686700808, -8.568281061380174535 ) ) ;
#91383 = ORIENTED_EDGE ( 'NONE', *, *, #59880, .F. ) ;
#91384 = CARTESIAN_POINT ( 'NONE',  ( -1.159861628855096694, 17.01140986925715026, 50.01797968613450251 ) ) ;
#91385 = AXIS2_PLACEMENT_3D ( 'NONE', #105579, #32245, #80768 ) ;
#91386 = ORIENTED_EDGE ( 'NONE', *, *, #28814, .F. ) ;
#91388 = CARTESIAN_POINT ( 'NONE',  ( 3.280815508853482942, 7.221948645665444921, -7.591546097228403234 ) ) ;
#91387 = CARTESIAN_POINT ( 'NONE',  ( 86.75754961941542831, 1.030564683017419500E-14, 0.000000000000000000 ) ) ;
#91389 = CARTESIAN_POINT ( 'NONE',  ( 6.026974479199131350E-05, -59.99999999999998579, 33.88964995960238014 ) ) ;
#91390 = CARTESIAN_POINT ( 'NONE',  ( -9.970195021759465703, 302.6460196488380348, -10.04373974541435466 ) ) ;
#91391 = APPLICATION_CONTEXT ( 'automotive_design' ) ;
#91392 = FILL_AREA_STYLE_COLOUR ( '', #106584 ) ;
#91393 = CARTESIAN_POINT ( 'NONE',  ( 21.08349330513380693, -4.000000000000000000, 4.898587196589415787E-16 ) ) ;
#91394 = CARTESIAN_POINT ( 'NONE',  ( 0.9986626498655565287, 14.07191026904348874, -51.25503100627838649 ) ) ;
#91395 = ORIENTED_EDGE ( 'NONE', *, *, #81040, .F. ) ;
#91396 = CARTESIAN_POINT ( 'NONE',  ( 92.74004866154591298, -60.00000000000000711, -6.457183730990628590 ) ) ;
#91397 = CARTESIAN_POINT ( 'NONE',  ( 32.22120753352737665, 464.6691781026588046, 10.60621122532779026 ) ) ;
#91398 = PRESENTATION_STYLE_ASSIGNMENT (( #58494 ) ) ;
#91399 = CARTESIAN_POINT ( 'NONE',  ( 40.96815392870802697, 488.3809129049201374, 10.59964723858293745 ) ) ;
#91400 = CARTESIAN_POINT ( 'NONE',  ( -47.07350275986928523, 18.64911821952795279, -14.79681583022523128 ) ) ;
#91401 = ORIENTED_EDGE ( 'NONE', *, *, #21945, .T. ) ;
#91402 = EDGE_CURVE ( 'NONE', #19034, #1527, #74572, .T. ) ;
#91403 = VECTOR ( 'NONE', #51292, 1000.000000000000000 ) ;
#91404 = CARTESIAN_POINT ( 'NONE',  ( 0.000000000000000000, 45.89575828009193259, -11.27631144943088337 ) ) ;
#91405 = ORIENTED_EDGE ( 'NONE', *, *, #97164, .F. ) ;
#91406 = ORIENTED_EDGE ( 'NONE', *, *, #41679, .T. ) ;
#91407 = CARTESIAN_POINT ( 'NONE',  ( 7.744991119775238353, 81.53561214574871485, -2.016316005557097668 ) ) ;
#91408 = FILL_AREA_STYLE ('',( #101076 ) ) ;
#91409 = DIRECTION ( 'NONE',  ( 0.9984555975339683975, -0.000000000000000000, -0.05555555555555529573 ) ) ;
#91410 =( LENGTH_UNIT ( ) NAMED_UNIT ( * ) SI_UNIT ( .MILLI., .METRE. ) );
#91411 = CARTESIAN_POINT ( 'NONE',  ( 85.67969062639832600, -52.73321948659197034, -3.978974129479640354 ) ) ;
#91412 = CARTESIAN_POINT ( 'NONE',  ( -32.43729139937729400, 312.3396530769931019, -7.763169779620859856 ) ) ;
#91413 = CARTESIAN_POINT ( 'NONE',  ( 7.188101187500001821, -34.43750000204838813, -2.977408999572650483 ) ) ;
#91415 = EDGE_CURVE ( 'NONE', #3555, #44907, #49772, .T. ) ;
#91414 = CARTESIAN_POINT ( 'NONE',  ( 12.50000000000000533, 39.74580781711993183, -64.99248152779956911 ) ) ;
#91416 = ORIENTED_EDGE ( 'NONE', *, *, #34942, .F. ) ;
#91417 = CARTESIAN_POINT ( 'NONE',  ( 6.499999999999999112, 0.6470732608156867238, -0.01945970098672831355 ) ) ;
#91418 = ORIENTED_EDGE ( 'NONE', *, *, #67, .F. ) ;
#91419 = CARTESIAN_POINT ( 'NONE',  ( -7.500000000000006217, 40.00000000007573675, -70.73267643392316018 ) ) ;
#91420 = CARTESIAN_POINT ( 'NONE',  ( 4.051286199644065888, -48.60127012969240212, 103.8758286790405378 ) ) ;
#91421 = AXIS2_PLACEMENT_3D ( 'NONE', #27564, #11850, #99803 ) ;
#91423 = VERTEX_POINT ( 'NONE', #51889 ) ;
#91422 = CARTESIAN_POINT ( 'NONE',  ( 67.48317336153286305, 4.898587196589294500E-16, -4.000000000000007105 ) ) ;
#91424 = CARTESIAN_POINT ( 'NONE',  ( 76.02982832201053043, -49.90348184441494084, 133.3415602174417529 ) ) ;
#91425 = B_SPLINE_CURVE_WITH_KNOTS ( 'NONE', 3,
 ( #85353, #2283, #77262, #35232 ),
 .UNSPECIFIED., .F., .F.,
 ( 4, 4 ),
 ( 0.000000000000000000, 0.0002604505668081740334 ),
 .UNSPECIFIED. ) ;
#91426 = EDGE_LOOP ( 'NONE', ( #66490, #72718, #12207, #69484, #66233 ) ) ;
#91427 = CIRCLE ( 'NONE', #89641, 1.999999999999998224 ) ;
#91428 = FILL_AREA_STYLE ('',( #58523 ) ) ;
#91429 = CARTESIAN_POINT ( 'NONE',  ( 7.188101187499999156, -22.25000000204839523, 2.977408999572654924 ) ) ;
#91430 = AXIS2_PLACEMENT_3D ( 'NONE', #4654, #101743, #45125 ) ;
#91431 = CARTESIAN_POINT ( 'NONE',  ( -114.1029252960232725, -57.67113437255621022, 166.8310794691209367 ) ) ;
#91432 = EDGE_CURVE ( 'NONE', #70286, #27681, #18499, .T. ) ;
#91433 = ORIENTED_EDGE ( 'NONE', *, *, #91607, .T. ) ;
#91434 = CARTESIAN_POINT ( 'NONE',  ( 6.162888688655350222, -7.505553499465148271, 0.000000000000000000 ) ) ;
#91435 = CARTESIAN_POINT ( 'NONE',  ( 103.8300117340547644, -45.28274633995925313, 179.3923655754059610 ) ) ;
#91436 = CARTESIAN_POINT ( 'NONE',  ( -34.79468063549888512, 490.6633164237441633, 11.75004032470205395 ) ) ;
#91437 = CIRCLE ( 'NONE', #105209, 5.000000000000011546 ) ;
#91438 = CARTESIAN_POINT ( 'NONE',  ( 30.00000000000000000, 3.157894736842105754, 14.66382285868951030 ) ) ;
#91439 = CARTESIAN_POINT ( 'NONE',  ( -5.656854249492381470, -22.25000000409676915, 5.656854249492379694 ) ) ;
#91440 = CARTESIAN_POINT ( 'NONE',  ( -89.99999999999997158, 500000.0000000000582, 196.0238439516549818 ) ) ;
#91441 = CARTESIAN_POINT ( 'NONE',  ( 9.334514330295450080, 248.2137726231820523, -3.588704711590614771 ) ) ;
#91442 =( NAMED_UNIT ( * ) PLANE_ANGLE_UNIT ( ) SI_UNIT ( $, .RADIAN. ) );
#91443 = CARTESIAN_POINT ( 'NONE',  ( 9.918325909156573417, 33.79235231707431808, 1.298699613733151681 ) ) ;
#91444 = CARTESIAN_POINT ( 'NONE',  ( 7.150053860865849487, -8.217345460860238759, 3.590189269391289351 ) ) ;
#91445 = DIRECTION ( 'NONE',  ( -1.894296555319077948E-20, 0.4412131870756560437, 0.8974023197822382780 ) ) ;
#91446 = VERTEX_POINT ( 'NONE', #75639 ) ;
#91447 = CARTESIAN_POINT ( 'NONE',  ( 3.750000000000000888, -6.495190528383301576, -6.991905250253759085 ) ) ;
#91448 = CARTESIAN_POINT ( 'NONE',  ( 12.86962311105386370, -60.00000000000000711, 39.71074230895528245 ) ) ;
#91449 = CARTESIAN_POINT ( 'NONE',  ( -91.56480674067756809, -29.99999999999999645, 190.7188212141660699 ) ) ;
#91450 = EDGE_CURVE ( 'NONE', #63378, #18205, #58566, .T. ) ;
#91451 = AXIS2_PLACEMENT_3D ( 'NONE', #10908, #59499, #2288 ) ;
#91452 = ORIENTED_EDGE ( 'NONE', *, *, #81171, .T. ) ;
#91453 = ORIENTED_EDGE ( 'NONE', *, *, #54026, .F. ) ;
#91454 = DIRECTION ( 'NONE',  ( 0.5735764363510491570, -0.8191520442889895781, 1.003171929053522035E-16 ) ) ;
#91455 = CARTESIAN_POINT ( 'NONE',  ( 69.37660719181492652, -57.68221287598195346, 149.8084875684434110 ) ) ;
#91456 = LINE ( 'NONE', #50432, #94803 ) ;
#91457 = CARTESIAN_POINT ( 'NONE',  ( 21.80423302458568102, -26.50636464758302324, -38.45223598383380192 ) ) ;
#91458 = AXIS2_PLACEMENT_3D ( 'NONE', #59713, #25233, #18194 ) ;
#91459 = CARTESIAN_POINT ( 'NONE',  ( -0.1690119616668960822, 43.17849121649364719, 18.74136049120801673 ) ) ;
#91460 = SURFACE_STYLE_USAGE ( .BOTH. , #25145 ) ;
#91461 = CARTESIAN_POINT ( 'NONE',  ( -38.99971751517416152, -60.00000000000000000, 50.74464281562639911 ) ) ;
#91462 = CARTESIAN_POINT ( 'NONE',  ( 0.000000000000000000, 16.00000000000000000, 0.000000000000000000 ) ) ;
#91463 = CARTESIAN_POINT ( 'NONE',  ( 0.7832924031922618990, 46.11172308909048922, -16.51234007558469230 ) ) ;
#91464 = CARTESIAN_POINT ( 'NONE',  ( -85.18066487451336855, -53.84498426936280424, 190.9692991790889778 ) ) ;
#91465 = ORIENTED_EDGE ( 'NONE', *, *, #77238, .F. ) ;
#91466 = CARTESIAN_POINT ( 'NONE',  ( 12.24503781984882167, -5.251331492636921894, 20.21097953542564696 ) ) ;
#91467 = CARTESIAN_POINT ( 'NONE',  ( -6.184616894767937190, -53.40250187758704925, 32.78001493188074988 ) ) ;
#91468 = CARTESIAN_POINT ( 'NONE',  ( -5.425084051525484341, 41.91238126712414669, -59.10640584780988149 ) ) ;
#91469 = CARTESIAN_POINT ( 'NONE',  ( 84.44642999311443532, -56.38380764954431612, 190.8905981808263448 ) ) ;
#91470 =( BOUNDED_SURFACE ( )  B_SPLINE_SURFACE ( 3, 2, ( 
 ( #102762, #69349, #45603 ),
 ( #2456, #28377, #61253 ),
 ( #44537, #27860, #85527 ),
 ( #60728, #61800, #53672 ) ),
 .UNSPECIFIED., .F., .F., .F. ) 
 B_SPLINE_SURFACE_WITH_KNOTS ( ( 4, 4 ),
 ( 3, 3 ),
 ( 0.05627786335318932243, 0.08234838753898729435 ),
 ( 0.000000000000000000, 0.6299190952401180210 ),
 .UNSPECIFIED. ) 
 GEOMETRIC_REPRESENTATION_ITEM ( )  RATIONAL_B_SPLINE_SURFACE ( (
 ( 1.000000000000000000, 0.8155006124047963212, 0.8634405994222458247),
 ( 1.000000000000000000, 0.8155002931124427645, 0.8634403630942395491),
 ( 1.000000000000000000, 0.8155003711612234252, 0.8634404208629662403),
 ( 1.000000000000000000, 0.8155006853121260502, 0.8634406533854668275) ) ) 
 REPRESENTATION_ITEM ( '' )  SURFACE ( )  );
#91472 = CARTESIAN_POINT ( 'NONE',  ( 4.752062635003135860, -66.34841433710333547, 13.81155678746845794 ) ) ;
#91471 = CARTESIAN_POINT ( 'NONE',  ( 93.39999999999999147, 1.023464760207051730E-14, 0.000000000000000000 ) ) ;
#91473 = EDGE_CURVE ( 'NONE', #72947, #6171, #90777, .T. ) ;
#91474 = VERTEX_POINT ( 'NONE', #16892 ) ;
#91475 = CARTESIAN_POINT ( 'NONE',  ( 26.12439441013744101, 34.87005242119162318, 9.598401274034952024 ) ) ;
#91476 = CARTESIAN_POINT ( 'NONE',  ( -8.480229304264785384, -5.000000000000526690, -16.24557161192316102 ) ) ;
#91477 = CARTESIAN_POINT ( 'NONE',  ( 15.64300095959876202, 35.03905011530154212, 22.45650292849707341 ) ) ;
#91478 = CARTESIAN_POINT ( 'NONE',  ( 26.93224738266096097, 304.9750774871889689, -9.533213446127941637 ) ) ;
#91479 = DIRECTION ( 'NONE',  ( -1.000000000000000000, -0.000000000000000000, -0.000000000000000000 ) ) ;
#91480 = EDGE_CURVE ( 'NONE', #35363, #29175, #77862, .T. ) ;
#91481 = CARTESIAN_POINT ( 'NONE',  ( 38.86650669486618881, 1.474610560812782335E-15, 0.000000000000000000 ) ) ;
#91482 = CARTESIAN_POINT ( 'NONE',  ( -43.27530345108696963, 461.7562057072040034, 3.870800370039641169 ) ) ;
#91483 = CARTESIAN_POINT ( 'NONE',  ( 106.4854190881680154, -14.21045842199434439, 182.1792229330528983 ) ) ;
#91484 = CARTESIAN_POINT ( 'NONE',  ( -85.11433041153968304, -18.62775704286118739, 156.3534888976464572 ) ) ;
#91485 = ORIENTED_EDGE ( 'NONE', *, *, #69631, .T. ) ;
#91486 = DIRECTION ( 'NONE',  ( -1.000000000000000000, -1.224606353822377258E-16, -0.000000000000000000 ) ) ;
#91487 = CARTESIAN_POINT ( 'NONE',  ( -9.989690267985819716, 253.9744441659491088, -0.5238310916885637880 ) ) ;
#91488 = SURFACE_SIDE_STYLE ('',( #25174 ) ) ;
#91489 = CARTESIAN_POINT ( 'NONE',  ( 34.35000000000000142, 1.533819458162526451E-15, 0.000000000000000000 ) ) ;
#91490 = CARTESIAN_POINT ( 'NONE',  ( 45.49126702261580135, 409.1826088023510124, 8.336894800179337039 ) ) ;
#91491 = CARTESIAN_POINT ( 'NONE',  ( 70.89460441624491693, 6.975173280561618775E-15, 0.000000000000000000 ) ) ;
#91492 = VERTEX_POINT ( 'NONE', #124 ) ;
#91493 = UNCERTAINTY_MEASURE_WITH_UNIT (LENGTH_MEASURE( 1.000000000000000082E-05 ), #99651, 'distance_accuracy_value', 'NONE');
#91494 = PRESENTATION_LAYER_ASSIGNMENT (  '', '', ( #51818 ) ) ;
#91496 = EDGE_CURVE ( 'NONE', #95805, #88641, #79194, .T. ) ;
#91495 = CIRCLE ( 'NONE', #103496, 4.000000000000001776 ) ;
#91497 = CARTESIAN_POINT ( 'NONE',  ( 45.11650669486618881, -3.851859888774471706E-31, 4.000000000000000888 ) ) ;
#91498 = ORIENTED_EDGE ( 'NONE', *, *, #11221, .F. ) ;
#91499 = CARTESIAN_POINT ( 'NONE',  ( 19.00000000000001421, -3.999999999999999112, -1.500000000000000000 ) ) ;
#91500 = CARTESIAN_POINT ( 'NONE',  ( 4.210530276627960866, 14.99999999999998934, 10.00000000000003908 ) ) ;
#91501 = CARTESIAN_POINT ( 'NONE',  ( 5.959251246171458405, -13.44866041637670939, 13.58291813670162362 ) ) ;
#91502 = AXIS2_PLACEMENT_3D ( 'NONE', #402, #48451, #7456 ) ;
#91503 = CARTESIAN_POINT ( 'NONE',  ( 43.65107446674234382, 435.6495114220916207, 9.088599805106140295 ) ) ;
#91504 = EDGE_LOOP ( 'NONE', ( #63237, #50508, #17776, #1658, #73164, #44987 ) ) ;
#91505 = CARTESIAN_POINT ( 'NONE',  ( 92.16359607964912470, -59.99999999999998579, 3.391195432473796068 ) ) ;
#91507 = CARTESIAN_POINT ( 'NONE',  ( 15.54306593367750722, -32.51112372676959694, 29.48007834858285037 ) ) ;
#91506 = CARTESIAN_POINT ( 'NONE',  ( -72.11328378729270128, -60.00000000000007816, 177.1367255069332316 ) ) ;
#91508 = FILL_AREA_STYLE_COLOUR ( '', #69677 ) ;
#91509 = DIRECTION ( 'NONE',  ( 0.000000000000000000, 0.000000000000000000, -1.000000000000000000 ) ) ;
#91510 = CARTESIAN_POINT ( 'NONE',  ( -39.97149089181551318, -56.80599509476397202, 42.45399057685605015 ) ) ;
#91511 = VECTOR ( 'NONE', #2533, 1000.000000000000000 ) ;
#91512 = CARTESIAN_POINT ( 'NONE',  ( 51.01037695545453232, 500.0000000000002274, -5.000000000000001776 ) ) ;
#91513 = VERTEX_POINT ( 'NONE', #26609 ) ;
#91514 = SURFACE_SIDE_STYLE ('',( #76366 ) ) ;
#91515 = CARTESIAN_POINT ( 'NONE',  ( 7.312892434773027972, 54.25556936841643818, 2.973951097466557059 ) ) ;
#91516 = CARTESIAN_POINT ( 'NONE',  ( 26.54817876223620488, 310.6276912632132507, 11.31208242866018132 ) ) ;
#91517 = SURFACE_SIDE_STYLE ('',( #58616 ) ) ;
#91518 = CARTESIAN_POINT ( 'NONE',  ( 6.683837171061802529, 3.955946848495962787, 6.851900933636986935 ) ) ;
#91519 = CARTESIAN_POINT ( 'NONE',  ( -32.04667661469866147, 487.4982811826213833, 8.072210805887316099 ) ) ;
#91520 = VERTEX_POINT ( 'NONE', #76167 ) ;
#91521 = DIRECTION ( 'NONE',  ( -8.673617379884035472E-17, 0.000000000000000000, -1.000000000000000000 ) ) ;
#91522 = VERTEX_POINT ( 'NONE', #98838 ) ;
#91523 = CARTESIAN_POINT ( 'NONE',  ( 81.11895617840627892, -30.00000000000015987, -11.48067823770064244 ) ) ;
#91524 = CARTESIAN_POINT ( 'NONE',  ( -43.00000000000000000, 438.3878896346931242, 16.22878885428556472 ) ) ;
#91525 = UNCERTAINTY_MEASURE_WITH_UNIT (LENGTH_MEASURE( 1.000000000000000082E-05 ), #60614, 'distance_accuracy_value', 'NONE');
#91526 = CARTESIAN_POINT ( 'NONE',  ( 23.84269658596081243, 25.80551286858905868, -30.86189937676715545 ) ) ;
#91527 = DIRECTION ( 'NONE',  ( 0.000000000000000000, 0.000000000000000000, 1.000000000000000000 ) ) ;
#91528 = CARTESIAN_POINT ( 'NONE',  ( 86.67015649070671657, -30.00000000000000355, 68.44422152834891904 ) ) ;
#91529 = CARTESIAN_POINT ( 'NONE',  ( -31.92839208162568454, 356.8913991353554138, 21.71261904506107143 ) ) ;
#91530 = ORIENTED_EDGE ( 'NONE', *, *, #106561, .T. ) ;
#91531 = EDGE_CURVE ( 'NONE', #68832, #87776, #65504, .T. ) ;
#91532 = AXIS2_PLACEMENT_3D ( 'NONE', #48858, #66122, #106575 ) ;
#91533 = ORIENTED_EDGE ( 'NONE', *, *, #35936, .T. ) ;
#91534 = ORIENTED_EDGE ( 'NONE', *, *, #85442, .F. ) ;
#91535 = CARTESIAN_POINT ( 'NONE',  ( -47.24099558602559057, 11.75653836616713299, -16.58383527959137638 ) ) ;
#91536 = FACE_OUTER_BOUND ( 'NONE', #69891, .T. ) ;
#91537 = COLOUR_RGB ( '', 0.72549020, 0.75294118, 0.79215686) ;
#91538 = CARTESIAN_POINT ( 'NONE',  ( 4.567209634097052273, -10.93599786085512804, -3.891254717191802381 ) ) ;
#91539 = ADVANCED_FACE ( 'NONE', ( #57849 ), #87844, .T. ) ;
#91540 = CARTESIAN_POINT ( 'NONE',  ( 6.445370176741902490, 4.584736124523943523, -5.738941594274561631 ) ) ;
#91542 = EDGE_CURVE ( 'NONE', #15534, #74862, #10361, .T. ) ;
#91541 = FACE_OUTER_BOUND ( 'NONE', #71152, .T. ) ;
#91543 = EDGE_LOOP ( 'NONE', ( #80573, #56299, #11515, #18223 ) ) ;
#91544 = FACE_OUTER_BOUND ( 'NONE', #46702, .T. ) ;
#91545 = VECTOR ( 'NONE', #106512, 1000.000000000000000 ) ;
#91546 = ORIENTED_EDGE ( 'NONE', *, *, #66887, .T. ) ;
#91547 = DIRECTION ( 'NONE',  ( 0.000000000000000000, -1.000000000000000000, 0.000000000000000000 ) ) ;
#91548 = CARTESIAN_POINT ( 'NONE',  ( 75.52049878556597662, -38.35346467193087250, 174.3913471852752082 ) ) ;
#91549 = CARTESIAN_POINT ( 'NONE',  ( 12.33349330513380337, 1.593028355512270567E-15, 0.000000000000000000 ) ) ;
#91550 = CARTESIAN_POINT ( 'NONE',  ( 26.71565930479108530, 306.5341601446122581, 10.78094868360216196 ) ) ;
#91551 = CARTESIAN_POINT ( 'NONE',  ( -4.813555570991618460, 248.2052620348266601, -3.584128953194777534 ) ) ;
#91552 = ORIENTED_EDGE ( 'NONE', *, *, #58467, .T. ) ;
#91553 = CARTESIAN_POINT ( 'NONE',  ( -40.18832759596268289, 460.7626523741620872, 2.139563623142588966 ) ) ;
#91554 = CARTESIAN_POINT ( 'NONE',  ( 30.33571977314562673, 298.1669207346403709, 2.668496471951124160 ) ) ;
#91555 = LINE ( 'NONE', #33866, #99678 ) ;
#91556 = EDGE_CURVE ( 'NONE', #44531, #88114, #24193, .T. ) ;
#91557 = CIRCLE ( 'NONE', #55335, 4.172000000000009479 ) ;
#91558 = CARTESIAN_POINT ( 'NONE',  ( 14.97535898699462997, 1.269652431126665260, -0.8876819510628390919 ) ) ;
#91559 = ORIENTED_EDGE ( 'NONE', *, *, #76804, .T. ) ;
#91560 = CARTESIAN_POINT ( 'NONE',  ( -28.51914334966707543, 297.3191045173070393, 10.47832804806128060 ) ) ;
#91561 = CARTESIAN_POINT ( 'NONE',  ( 30.56153846153846132, 1.411358822780289120E-15, 0.000000000000000000 ) ) ;
#91562 = UNCERTAINTY_MEASURE_WITH_UNIT (LENGTH_MEASURE( 1.000000000000000082E-05 ), #103295, 'distance_accuracy_value', 'NONE');
#91563 = CARTESIAN_POINT ( 'NONE',  ( 56.48317336153285595, -4.000000000000000000, 0.000000000000000000 ) ) ;
#91564 = CARTESIAN_POINT ( 'NONE',  ( 89.93133926947346879, -2.002967142162725287E-29, 5.000000000000011546 ) ) ;
#91565 = DIRECTION ( 'NONE',  ( 0.000000000000000000, 0.000000000000000000, 1.000000000000000000 ) ) ;
#91566 = ADVANCED_FACE ( 'NONE', ( #77780 ), #44352, .T. ) ;
#91567 = CARTESIAN_POINT ( 'NONE',  ( 8.730595983954971828, 295.2524660276815780, 4.886029594169265522 ) ) ;
#91568 = CARTESIAN_POINT ( 'NONE',  ( 10.41054107240687188, 3.851859888774471706E-31, 5.000000000000001776 ) ) ;
#91569 = CARTESIAN_POINT ( 'NONE',  ( 83.83731836935660908, -61.02556977702034402, 192.0768483181223019 ) ) ;
#91570 = CARTESIAN_POINT ( 'NONE',  ( 0.000000000000000000, 15.00000000000000000, -10.00000000000000000 ) ) ;
#91571 = FILL_AREA_STYLE_COLOUR ( '', #7334 ) ;
#91572 = ORIENTED_EDGE ( 'NONE', *, *, #27802, .T. ) ;
#91573 = CARTESIAN_POINT ( 'NONE',  ( 83.90317718560991977, -57.67099787064372407, -27.79890540918554365 ) ) ;
#91574 = CARTESIAN_POINT ( 'NONE',  ( -71.61946902996672293, -38.00000000000000711, -21.68294473311254578 ) ) ;
#91575 = CARTESIAN_POINT ( 'NONE',  ( 86.75754961941542831, 1.030564683017419500E-14, 0.000000000000000000 ) ) ;
#91576 = CARTESIAN_POINT ( 'NONE',  ( -16.75187969033532553, -1.200000000000000030E-05, 23.05698433968612093 ) ) ;
#91577 =( GEOMETRIC_REPRESENTATION_CONTEXT ( 3 ) GLOBAL_UNCERTAINTY_ASSIGNED_CONTEXT ( ( #104534 ) ) GLOBAL_UNIT_ASSIGNED_CONTEXT ( ( #26585, #2783, #76140 ) ) REPRESENTATION_CONTEXT ( 'NONE', 'WORKASPACE' ) );
#91578 = CARTESIAN_POINT ( 'NONE',  ( -80.78937829594153186, -29.99999999999999645, 9.273401272670504625 ) ) ;
#91579 = MECHANICAL_DESIGN_GEOMETRIC_PRESENTATION_REPRESENTATION (  '', ( #72551 ), #45091 ) ;
#91580 = CARTESIAN_POINT ( 'NONE',  ( 23.21751746555220564, 28.11705169068991950, -30.70617127781077116 ) ) ;
#91581 = CARTESIAN_POINT ( 'NONE',  ( -5.088535779736856668, 5.722386535631781790, -7.491772860716145566 ) ) ;
#91583 = CARTESIAN_POINT ( 'NONE',  ( 7.500000000000000888, -4.999999999999997335, -14.04024970282782547 ) ) ;
#91582 = DIRECTION ( 'NONE',  ( 0.000000000000000000, 0.000000000000000000, 1.000000000000000000 ) ) ;
#91584 = CIRCLE ( 'NONE', #45096, 4.172000000000001485 ) ;
#91585 = CARTESIAN_POINT ( 'NONE',  ( -17.49999999999997513, 49.09249047134142785, 64.04102639539493680 ) ) ;
#91586 = CARTESIAN_POINT ( 'NONE',  ( -29.59455828143376266, 18.41848238274119609, 39.60535821593508388 ) ) ;
#91587 = CARTESIAN_POINT ( 'NONE',  ( -36.14965894305860417, 491.8061723310894990, 12.56429772144753443 ) ) ;
#91588 = CARTESIAN_POINT ( 'NONE',  ( 4.656749229489884456, -83.68239591873569339, -3.785628640239149689 ) ) ;
#91589 = DIRECTION ( 'NONE',  ( -0.3845251595719093585, 0.02506431005095593675, 0.9227741771516296820 ) ) ;
#91590 = CARTESIAN_POINT ( 'NONE',  ( 20.77592568779148863, 1.482358050883964840E-15, 0.000000000000000000 ) ) ;
#91591 = CARTESIAN_POINT ( 'NONE',  ( 68.29510937182399744, -29.93295853997381073, -21.58228327437667460 ) ) ;
#91592 = ORIENTED_EDGE ( 'NONE', *, *, #76989, .F. ) ;
#91593 = DIRECTION ( 'NONE',  ( -0.000000000000000000, -0.000000000000000000, -1.000000000000000000 ) ) ;
#91594 = DIRECTION ( 'NONE',  ( -1.000000000000000000, -0.000000000000000000, -0.000000000000000000 ) ) ;
#91595 = DIRECTION ( 'NONE',  ( -1.000000000000000000, -0.000000000000000000, -0.000000000000000000 ) ) ;
#91596 = CARTESIAN_POINT ( 'NONE',  ( -38.83077474420895214, -24.51455171004923983, -30.53465071944147979 ) ) ;
#91598 = CARTESIAN_POINT ( 'NONE',  ( 37.54559764570182523, 464.1143081516207189, 19.43664670202678835 ) ) ;
#91597 = CARTESIAN_POINT ( 'NONE',  ( 37.33349330513379982, 1.593028355512270962E-15, 0.000000000000000000 ) ) ;
#91599 = EDGE_CURVE ( 'NONE', #67261, #41862, #84444, .T. ) ;
#91600 = ORIENTED_EDGE ( 'NONE', *, *, #54863, .F. ) ;
#91601 = AXIS2_PLACEMENT_3D ( 'NONE', #52337, #2724, #42656 ) ;
#91602 = ADVANCED_FACE ( 'NONE', ( #29789, #93968, #69170, #54007, #95551 ), #75809, .F. ) ;
#91603 = CARTESIAN_POINT ( 'NONE',  ( 6.167866516170612989, -1.339763354879983215, -6.499999999999395150 ) ) ;
#91604 = ORIENTED_EDGE ( 'NONE', *, *, #6916, .T. ) ;
#91605 = DIRECTION ( 'NONE',  ( 0.5735764363510490460, 0.8191520442889896891, 0.000000000000000000 ) ) ;
#91606 = EDGE_CURVE ( 'NONE', #7244, #53673, #25149, .T. ) ;
#91607 = EDGE_CURVE ( 'NONE', #3985, #8366, #62068, .T. ) ;
#91608 = AXIS2_PLACEMENT_3D ( 'NONE', #103908, #96377, #103390 ) ;
#91609 = CARTESIAN_POINT ( 'NONE',  ( -66.17813322318392011, -60.00000000000000000, -33.83408426857283757 ) ) ;
#91610 = ORIENTED_EDGE ( 'NONE', *, *, #57027, .T. ) ;
#91611 = FILL_AREA_STYLE ('',( #34465 ) ) ;
#91612 = CARTESIAN_POINT ( 'NONE',  ( -8.559508646656370345, 53.68473964988125857, -4.031152949374577688 ) ) ;
#91613 = CARTESIAN_POINT ( 'NONE',  ( 98.44230880729132593, -37.77081898374070335, 192.2818622570195259 ) ) ;
#91615 = CARTESIAN_POINT ( 'NONE',  ( -17.84510959215117509, 45.37789619860912893, 5.053583809357591328 ) ) ;
#91614 = CARTESIAN_POINT ( 'NONE',  ( 0.000000000000000000, 294.8518027762758038, -10.00000000000000178 ) ) ;
#91616 = ORIENTED_EDGE ( 'NONE', *, *, #3822, .F. ) ;
#91617 = EDGE_CURVE ( 'NONE', #45028, #23591, #89597, .T. ) ;
#91618 = ORIENTED_EDGE ( 'NONE', *, *, #5674, .F. ) ;
#91619 = ORIENTED_EDGE ( 'NONE', *, *, #88246, .T. ) ;
#91620 = CARTESIAN_POINT ( 'NONE',  ( 30.19392226039637350, 332.6110142126161691, 15.69272685516405907 ) ) ;
#91621 = CARTESIAN_POINT ( 'NONE',  ( 4.898587196589412829E-16, -28.62499999999999289, -8.000000000000000000 ) ) ;
#91622 = CARTESIAN_POINT ( 'NONE',  ( 15.43372845131084858, 46.13227632078331197, 5.762758105581649026 ) ) ;
#91623 = VERTEX_POINT ( 'NONE', #70743 ) ;
#91624 = DIRECTION ( 'NONE',  ( 0.000000000000000000, -1.000000000000000000, 0.000000000000000000 ) ) ;
#91625 = CARTESIAN_POINT ( 'NONE',  ( 6.562974947121713143, 7.579827465851455948, 0.5629870116737627495 ) ) ;
#91626 = DIRECTION ( 'NONE',  ( -0.000000000000000000, 0.5000000000000018874, 0.8660254037844375974 ) ) ;
#91627 = CARTESIAN_POINT ( 'NONE',  ( -19.49904798085934843, -57.67182591607114261, 42.12704350231687300 ) ) ;
#91628 = CARTESIAN_POINT ( 'NONE',  ( 7.188101187500000044, -32.65625000204838813, 0.000000000000000000 ) ) ;
#91629 = CARTESIAN_POINT ( 'NONE',  ( -44.11327388758650159, 464.4313852428384735, 9.822198357558047377 ) ) ;
#91630 = CARTESIAN_POINT ( 'NONE',  ( -31.02212611900126760, 360.5725590293961318, 22.12937154125974715 ) ) ;
#91631 = CARTESIAN_POINT ( 'NONE',  ( -7.006861776756331039, 41.19339244735165551, -58.48462588885441704 ) ) ;
#91632 = CARTESIAN_POINT ( 'NONE',  ( -94.98233504546384154, -60.00000000000004263, -11.07720828487985720 ) ) ;
#91633 = FILL_AREA_STYLE_COLOUR ( '', #103337 ) ;
#91634 = CARTESIAN_POINT ( 'NONE',  ( -49.26216918836951209, -42.98127006318125609, 50.67504490609899648 ) ) ;
#91635 = CARTESIAN_POINT ( 'NONE',  ( 5.656854249492380582, -27.31249999999999645, -5.656854249492379694 ) ) ;
#91636 = ORIENTED_EDGE ( 'NONE', *, *, #74814, .T. ) ;
#91637 = CARTESIAN_POINT ( 'NONE',  ( 0.000000000000000000, 0.000000000000000000, 0.000000000000000000 ) ) ;
#91638 = CARTESIAN_POINT ( 'NONE',  ( -6.145867760194407836, 301.8770827788611086, -10.02048593162379042 ) ) ;
#91639 = CARTESIAN_POINT ( 'NONE',  ( 45.36923076923077502, -4.171999999999999709, 5.616230220889763424E-16 ) ) ;
#91640 = VERTEX_POINT ( 'NONE', #103637 ) ;
#91641 = CARTESIAN_POINT ( 'NONE',  ( -17.51143763087804572, 34.75099232332586041, -22.05163403062407923 ) ) ;
#91642 = CARTESIAN_POINT ( 'NONE',  ( 106.1546576866561225, -38.37411319834205869, 196.1368700578019002 ) ) ;
#91643 = FILL_AREA_STYLE ('',( #67368 ) ) ;
#91644 = LINE ( 'NONE', #49028, #12919 ) ;
#91645 = PRESENTATION_LAYER_ASSIGNMENT (  '', '', ( #31380 ) ) ;
#91646 = CARTESIAN_POINT ( 'NONE',  ( -19.22284019411856804, 302.7169880953082952, 9.908343670167209183 ) ) ;
#91647 = CARTESIAN_POINT ( 'NONE',  ( 92.29684323675850521, -29.99999999999999645, 190.9540310920743309 ) ) ;
#91648 = AXIS2_PLACEMENT_3D ( 'NONE', #31494, #32010, #36549 ) ;
#91649 = CARTESIAN_POINT ( 'NONE',  ( 43.69697758767897966, 434.4335448986662982, 11.30914782516539674 ) ) ;
#91650 = SURFACE_SIDE_STYLE ('',( #58755 ) ) ;
#91651 = EDGE_CURVE ( 'NONE', #79598, #29102, #94855, .T. ) ;
#91652 = ORIENTED_EDGE ( 'NONE', *, *, #71134, .T. ) ;
#91653 = VERTEX_POINT ( 'NONE', #44896 ) ;
#91654 = CARTESIAN_POINT ( 'NONE',  ( 52.28277805137703638, -42.97149545941184812, 56.06074786058347570 ) ) ;
#91655 = CARTESIAN_POINT ( 'NONE',  ( 6.586014638021513434, 41.68775674026067435, -58.88021276518479397 ) ) ;
#91656 = CARTESIAN_POINT ( 'NONE',  ( 9.685714585015881894, 51.27227691868331760, 3.330047012961471431 ) ) ;
#91657 = EDGE_CURVE ( 'NONE', #60305, #11929, #27677, .T. ) ;
#91658 = CONICAL_SURFACE ( 'NONE', #86533, 5.000000000000001776, 0.9599310885968803664 ) ;
#91659 = EDGE_CURVE ( 'NONE', #45575, #56185, #91381, .T. ) ;
#91660 = ORIENTED_EDGE ( 'NONE', *, *, #86935, .F. ) ;
#91661 = CARTESIAN_POINT ( 'NONE',  ( -90.67172824033494294, -38.34345381613530179, 8.532772670937511350 ) ) ;
#91662 = EDGE_LOOP ( 'NONE', ( #106276, #37521, #61154, #40793 ) ) ;
#91663 = CARTESIAN_POINT ( 'NONE',  ( 16.05785784214672773, 4.775831776474229073, 3.710403933782411734 ) ) ;
#91664 = CARTESIAN_POINT ( 'NONE',  ( 110.2491435845926588, -38.35601175776276506, 184.3373205914413120 ) ) ;
#91665 = CARTESIAN_POINT ( 'NONE',  ( 15.53945107738913300, 22.94853113541235601, -1.161811152313551920 ) ) ;
#91666 = CARTESIAN_POINT ( 'NONE',  ( 85.41402076159042167, -45.28278736550084460, 38.51236139168902639 ) ) ;
#91667 = CARTESIAN_POINT ( 'NONE',  ( -17.77056504783044844, 43.17862847894689793, -5.954854177184050634 ) ) ;
#91668 = CARTESIAN_POINT ( 'NONE',  ( 34.87165355513719334, 435.0272833139666773, 7.833813470889964492 ) ) ;
#91669 = CARTESIAN_POINT ( 'NONE',  ( 2.232946119676683772, -69.45268377165729135, 12.90885355194285999 ) ) ;
#91670 = CARTESIAN_POINT ( 'NONE',  ( 74.84030112959139558, -60.00000000000000711, 180.0309485043998450 ) ) ;
#91671 = CARTESIAN_POINT ( 'NONE',  ( -34.13897275411324017, 489.1603865320491309, 11.37941925714664926 ) ) ;
#91672 = CARTESIAN_POINT ( 'NONE',  ( 18.22717058311603466, 45.00000000000000711, 62.43928791138841916 ) ) ;
#91673 = VERTEX_POINT ( 'NONE', #52422 ) ;
#91674 = CARTESIAN_POINT ( 'NONE',  ( 60.17165906010207976, -32.54078018923782167, 69.39975707695209906 ) ) ;
#91675 = CARTESIAN_POINT ( 'NONE',  ( -27.31158286324798468, 296.2711421484885363, -9.693697505745531018 ) ) ;
#91676 = CARTESIAN_POINT ( 'NONE',  ( 65.52222222222222570, 6.915964383211875250E-15, 0.000000000000000000 ) ) ;
#91677 = AXIS2_PLACEMENT_3D ( 'NONE', #71574, #81254, #97984 ) ;
#91678 = CARTESIAN_POINT ( 'NONE',  ( -9.189739293810873733, -4.999999999999998224, -17.80227345177911502 ) ) ;
#91679 = CARTESIAN_POINT ( 'NONE',  ( -36.02691569689581286, 484.4775272227933556, -2.201217060995769526 ) ) ;
#91680 = CARTESIAN_POINT ( 'NONE',  ( -42.78195672996899646, 397.2058786343547467, 19.86382575910961990 ) ) ;
#91681 = CARTESIAN_POINT ( 'NONE',  ( -37.88755491168825529, 25.36998983636258131, -13.42507852288176728 ) ) ;
#91682 = DIRECTION ( 'NONE',  ( 0.000000000000000000, 0.000000000000000000, 1.000000000000000000 ) ) ;
#91683 = CARTESIAN_POINT ( 'NONE',  ( -3.313708498984765161, -27.96874999999999289, 7.999999999999998224 ) ) ;
#91684 = CIRCLE ( 'NONE', #95151, 8.500000000000000000 ) ;
#91685 = CARTESIAN_POINT ( 'NONE',  ( -24.73976553408828138, -19.17417380900784352, 31.50158786446911208 ) ) ;
#91686 = CIRCLE ( 'NONE', #86550, 4.000000000000007105 ) ;
#91687 = CARTESIAN_POINT ( 'NONE',  ( 37.48925363931293475, 48.00000000000000000, 53.34938573421631247 ) ) ;
#91688 = PRESENTATION_LAYER_ASSIGNMENT (  '', '', ( #64141 ) ) ;
#91689 = ORIENTED_EDGE ( 'NONE', *, *, #75590, .F. ) ;
#91690 = CARTESIAN_POINT ( 'NONE',  ( 82.97048537381988353, -53.65713580650503189, 186.0269519114637831 ) ) ;
#91691 = EDGE_CURVE ( 'NONE', #101661, #1636, #61618, .T. ) ;
#91692 = CARTESIAN_POINT ( 'NONE',  ( 99.75754961941544252, 6.123233995736568081E-16, -5.000000000000011546 ) ) ;
#91693 = LINE ( 'NONE', #91174, #69579 ) ;
#91694 = VERTEX_POINT ( 'NONE', #37352 ) ;
#91695 = CARTESIAN_POINT ( 'NONE',  ( -5.656854249492379694, -33.12500000409677625, -5.656854249492380582 ) ) ;
#91696 = CARTESIAN_POINT ( 'NONE',  ( 4.898587196589412829E-16, -27.31250000409677270, -8.000000000000000000 ) ) ;
#91697 = CARTESIAN_POINT ( 'NONE',  ( -32.93681933015854213, 464.9081438945292462, 10.83352224627681970 ) ) ;
#91698 =( NAMED_UNIT ( * ) SI_UNIT ( $, .STERADIAN. ) SOLID_ANGLE_UNIT ( ) );
#91699 = CARTESIAN_POINT ( 'NONE',  ( 5.293743209220361123, -3.000000000000003109, -99.09939186120909937 ) ) ;
#91700 = CARTESIAN_POINT ( 'NONE',  ( -38.75976230197111505, -32.56425988891942325, -37.56949155413147423 ) ) ;
#91701 = CARTESIAN_POINT ( 'NONE',  ( -5.385673916453011856, 0.000000000000000000, 18.57417562100670949 ) ) ;
#91702 = CARTESIAN_POINT ( 'NONE',  ( 56.51238540776725472, -60.00000000000000000, 89.69717995302688962 ) ) ;
#91703 = DIRECTION ( 'NONE',  ( -1.000000000000000000, -0.000000000000000000, 0.000000000000000000 ) ) ;
#91704 = CARTESIAN_POINT ( 'NONE',  ( 4.445870512337758207, -12.80577256473136671, 32.12328779665543266 ) ) ;
#91706 = CARTESIAN_POINT ( 'NONE',  ( -12.34875849493573519, 20.40955147515336421, -6.752960215329498972 ) ) ;
#91705 = CARTESIAN_POINT ( 'NONE',  ( -16.06393304193705873, -23.29483378636053814, 36.09226395465890391 ) ) ;
#91707 = CARTESIAN_POINT ( 'NONE',  ( 46.00000000000000000, 500.0000000000002274, 5.000000000000001776 ) ) ;
#91708 = CARTESIAN_POINT ( 'NONE',  ( -2.977408999572654480, -12.12500000204838990, 7.188101187499999156 ) ) ;
#91709 = DIRECTION ( 'NONE',  ( -1.000000000000000000, -0.000000000000000000, -0.000000000000000000 ) ) ;
#91710 = CARTESIAN_POINT ( 'NONE',  ( 9.349999999999997868, 3.309500000000003439, 4.052968581778167743E-16 ) ) ;
#91711 = ORIENTED_EDGE ( 'NONE', *, *, #67541, .F. ) ;
#91712 = CARTESIAN_POINT ( 'NONE',  ( -74.38258808346769513, -38.35603007024654687, -29.43386503283010214 ) ) ;
#91713 = CARTESIAN_POINT ( 'NONE',  ( -17.50000000000292744, 50.00000000000124345, 59.64162155654736353 ) ) ;
#91714 = UNCERTAINTY_MEASURE_WITH_UNIT (LENGTH_MEASURE( 1.000000000000000082E-05 ), #85601, 'distance_accuracy_value', 'NONE');
#91715 = FACE_OUTER_BOUND ( 'NONE', #28918, .T. ) ;
#91716 = VECTOR ( 'NONE', #15022, 1000.000000000000000 ) ;
#91718 = CARTESIAN_POINT ( 'NONE',  ( 19.42798308777478056, -60.22819309317802805, -36.14118300158362018 ) ) ;
#91717 = CARTESIAN_POINT ( 'NONE',  ( 4.206664005177994881, 53.86290224764378820, 7.924430552076916712 ) ) ;
#91719 = EDGE_CURVE ( 'NONE', #62139, #15446, #77595, .T. ) ;
#91720 = ORIENTED_EDGE ( 'NONE', *, *, #67464, .T. ) ;
#91721 = CARTESIAN_POINT ( 'NONE',  ( 13.46465456495261215, 20.01166497731195903, -7.140621403355150498 ) ) ;
#91723 = VERTEX_POINT ( 'NONE', #103118 ) ;
#91722 = AXIS2_PLACEMENT_3D ( 'NONE', #80617, #64979, #6738 ) ;
#91724 = EDGE_CURVE ( 'NONE', #60190, #44416, #87998, .T. ) ;
#91725 = FACE_OUTER_BOUND ( 'NONE', #91068, .T. ) ;
#91726 = B_SPLINE_CURVE_WITH_KNOTS ( 'NONE', 3,
 ( #24919, #26013, #97706, #50740, #23871, #33538, #83646, #574 ),
 .UNSPECIFIED., .F., .F.,
 ( 4, 2, 2, 4 ),
 ( 0.000000000000000000, 0.002020203531082300028, 0.003030305296623449392, 0.004040407062164599189 ),
 .UNSPECIFIED. ) ;
#91727 = EDGE_CURVE ( 'NONE', #40703, #51662, #32875, .T. ) ;
#91728 = CARTESIAN_POINT ( 'NONE',  ( 30.93381850223209639, 8.838939540955992769, -40.91347331214265637 ) ) ;
#91729 = CARTESIAN_POINT ( 'NONE',  ( -33.12584033004571893, 40.69330525349585059, -62.10061223356491666 ) ) ;
#91730 = CARTESIAN_POINT ( 'NONE',  ( -100.8717445597720399, -60.00000000000000000, 86.14780900159736632 ) ) ;
#91731 = CARTESIAN_POINT ( 'NONE',  ( -13.48662581987258946, 304.5494697335691967, -9.064266068579863500 ) ) ;
#91732 = CARTESIAN_POINT ( 'NONE',  ( 22.18906107735381283, 305.1406206946286943, -9.938500898754245583 ) ) ;
#91733 = CARTESIAN_POINT ( 'NONE',  ( -3.964299495114179450, -48.70984094615566562, 103.9028936078247085 ) ) ;
#91735 = CARTESIAN_POINT ( 'NONE',  ( 29.99999999996260058, 488.4118811724847546, 8.310946025480145494 ) ) ;
#91734 = CARTESIAN_POINT ( 'NONE',  ( -9.739726766103894207, -3.000000000000002665, -82.38252115500876016 ) ) ;
#91736 = CARTESIAN_POINT ( 'NONE',  ( -82.63399304676930512, -46.48556652261747502, 177.1140125195145743 ) ) ;
#91737 = VERTEX_POINT ( 'NONE', #23818 ) ;
#91738 = CARTESIAN_POINT ( 'NONE',  ( 54.52222222222221859, 3.309500000000014541, 0.000000000000000000 ) ) ;
#91739 = EDGE_CURVE ( 'NONE', #57829, #86235, #99618, .T. ) ;
#91740 = ORIENTED_EDGE ( 'NONE', *, *, #48782, .T. ) ;
#91741 = VERTEX_POINT ( 'NONE', #96086 ) ;
#91742 = DIRECTION ( 'NONE',  ( -0.000000000000000000, -1.000000000000000000, -0.000000000000000000 ) ) ;
#91743 = AXIS2_PLACEMENT_3D ( 'NONE', #65686, #66756, #24198 ) ;
#91744 = ORIENTED_EDGE ( 'NONE', *, *, #2015, .T. ) ;
#91745 = DIRECTION ( 'NONE',  ( -1.000000000000000000, -1.224606353822377258E-16, -0.000000000000000000 ) ) ;
#91746 = CARTESIAN_POINT ( 'NONE',  ( -51.62523913740291448, -57.67116585372185966, -39.59675499642695939 ) ) ;
#91747 = CARTESIAN_POINT ( 'NONE',  ( 6.936184427528457874, 0.000000000000000000, 0.000000000000000000 ) ) ;
#91748 = FACE_OUTER_BOUND ( 'NONE', #15347, .T. ) ;
#91749 = AXIS2_PLACEMENT_3D ( 'NONE', #84239, #10333, #2774 ) ;
#91750 = CARTESIAN_POINT ( 'NONE',  ( 43.55305824496269906, 463.9995833982595741, 6.100617664814004470 ) ) ;
#91751 = DIRECTION ( 'NONE',  ( 0.000000000000000000, 1.000000000000000000, 0.000000000000000000 ) ) ;
#91752 = DIRECTION ( 'NONE',  ( 0.000000000000000000, 0.000000000000000000, 1.000000000000000000 ) ) ;
#91753 = CARTESIAN_POINT ( 'NONE',  ( 102.6948251682922404, -14.21045842199434084, 129.2649694714442035 ) ) ;
#91754 = CARTESIAN_POINT ( 'NONE',  ( -106.6847104835838564, -14.21045842199429288, 180.1424598013736329 ) ) ;
#91755 = CARTESIAN_POINT ( 'NONE',  ( -61.52905154805608134, -22.11594851545532237, 67.98467379429274615 ) ) ;
#91756 = ORIENTED_EDGE ( 'NONE', *, *, #20418, .T. ) ;
#91757 = CARTESIAN_POINT ( 'NONE',  ( 5.887945094627411002, 14.31209784358735249, 3.787642776067695394 ) ) ;
#91758 = CARTESIAN_POINT ( 'NONE',  ( 15.62220340632255500, -60.00000000000000000, 39.81715212526117398 ) ) ;
#91759 = ORIENTED_EDGE ( 'NONE', *, *, #5809, .T. ) ;
#91760 = CARTESIAN_POINT ( 'NONE',  ( 6.184718825718106494, -53.39673701277134654, 32.77909904936606011 ) ) ;
#91761 = CARTESIAN_POINT ( 'NONE',  ( -103.7347427267881699, -52.71028617885053080, 187.7480353013368699 ) ) ;
#91762 = CARTESIAN_POINT ( 'NONE',  ( -7.188101187500002709, -9.687500002048384573, 2.977408999572647819 ) ) ;
#91763 = DIRECTION ( 'NONE',  ( 0.000000000000000000, -0.5000000000000009992, -0.8660254037844380415 ) ) ;
#91764 = SURFACE_STYLE_FILL_AREA ( #51278 ) ;
#91765 = VERTEX_POINT ( 'NONE', #80943 ) ;
#91766 = DIRECTION ( 'NONE',  ( 0.000000000000000000, -1.000000000000000000, 0.000000000000000000 ) ) ;
#91767 = CARTESIAN_POINT ( 'NONE',  ( -74.64324676806940317, -60.00000000000002132, 178.4426176709596632 ) ) ;
#91768 = CARTESIAN_POINT ( 'NONE',  ( -1.450088712723273554, -0.02381973979900874755, 101.4852321302689688 ) ) ;
#91769 = CARTESIAN_POINT ( 'NONE',  ( -2.977408999572654480, -21.50000000204839168, 7.188101187499999156 ) ) ;
#91770 = DIRECTION ( 'NONE',  ( 0.000000000000000000, 0.000000000000000000, 1.000000000000000000 ) ) ;
#91771 = DIRECTION ( 'NONE',  ( 0.000000000000000000, 0.000000000000000000, 1.000000000000000000 ) ) ;
#91772 =( BOUNDED_SURFACE ( )  B_SPLINE_SURFACE ( 2, 3, ( 
 ( #68095, #91843, #99378, #50309, #17971, #66500 ),
 ( #139, #58417, #16355, #50828, #9845, #26620 ),
 ( #49240, #91330, #75649, #1201, #43294, #84284 ) ),
 .UNSPECIFIED., .F., .F., .F. ) 
 B_SPLINE_SURFACE_WITH_KNOTS ( ( 3, 3 ),
 ( 4, 2, 4 ),
 ( 0.000000000000000000, 1.000000000000000000 ),
 ( 0.07468083296558609974, 0.1199308329655860983, 0.1241808329655861021 ),
 .UNSPECIFIED. ) 
 GEOMETRIC_REPRESENTATION_ITEM ( )  RATIONAL_B_SPLINE_SURFACE ( (
 ( 1.000000000000000000, 1.000000000000000000, 1.000000000000000000, 1.000000000000000000, 1.000000000000000000, 1.000000000000000000),
 ( 1.857142857142858317, 1.857142857142858317, 1.857142857142858317, 1.857142857142858317, 1.857142857142858317, 1.857142857142858317),
 ( 1.000000000000000000, 1.000000000000000000, 1.000000000000000000, 1.000000000000000000, 1.000000000000000000, 1.000000000000000000) ) ) 
 REPRESENTATION_ITEM ( '' )  SURFACE ( )  );
#91773 = CARTESIAN_POINT ( 'NONE',  ( -0.2701328141633552726, 21.85270131633358304, -7.000000000000010658 ) ) ;
#91774 = CARTESIAN_POINT ( 'NONE',  ( -21.25502769577498796, 305.0480251235313176, 9.978840188629131802 ) ) ;
#91775 = CYLINDRICAL_SURFACE ( 'NONE', #105354, 5.000000000000000888 ) ;
#91776 = CARTESIAN_POINT ( 'NONE',  ( 4.470309410577035791, -8.781697353302565290, 13.55535895067712815 ) ) ;
#91777 = CARTESIAN_POINT ( 'NONE',  ( 33.52307692307692122, -4.171999999999999709, 0.000000000000000000 ) ) ;
#91778 = DIRECTION ( 'NONE',  ( 0.000000000000000000, -0.5626279437298172814, -0.8267102254928009319 ) ) ;
#91779 = CARTESIAN_POINT ( 'NONE',  ( -30.72484781686770816, -22.13132935070668950, 30.23765891460996968 ) ) ;
#91780 = B_SPLINE_CURVE_WITH_KNOTS ( 'NONE', 3,
 ( #158, #33124, #65993, #23986 ),
 .UNSPECIFIED., .F., .F.,
 ( 4, 4 ),
 ( 0.000000000000000000, 1.000000000000000000 ),
 .UNSPECIFIED. ) ;
#91781 = CARTESIAN_POINT ( 'NONE',  ( 0.000000000000000000, 0.000000000000000000, 0.000000000000000000 ) ) ;
#91782 = CARTESIAN_POINT ( 'NONE',  ( 42.93374039441252421, -36.07034193160639290, 40.55194211749969924 ) ) ;
#91783 = DIRECTION ( 'NONE',  ( 1.000000000000000000, 1.224606353822377258E-16, 0.000000000000000000 ) ) ;
#91784 = ORIENTED_EDGE ( 'NONE', *, *, #26371, .F. ) ;
#91785 = CARTESIAN_POINT ( 'NONE',  ( 43.81062608880509401, 434.3289934330969686, 12.63519120572941823 ) ) ;
#91786 = EDGE_CURVE ( 'NONE', #56342, #27639, #79882, .T. ) ;
#91787 = CARTESIAN_POINT ( 'NONE',  ( -80.66978632760687162, -38.82151610998087676, 194.1105594702565611 ) ) ;
#91788 = ORIENTED_EDGE ( 'NONE', *, *, #5946, .F. ) ;
#91789 = CARTESIAN_POINT ( 'NONE',  ( 0.000000000000000000, -78.00000000000000000, 27.00000000000000000 ) ) ;
#91790 = CARTESIAN_POINT ( 'NONE',  ( 66.68617954663659475, -59.99999999999999289, 102.5125723375521716 ) ) ;
#91791 = DIRECTION ( 'NONE',  ( -1.000000000000000000, -0.000000000000000000, -0.000000000000000000 ) ) ;
#91792 = CARTESIAN_POINT ( 'NONE',  ( -7.413000813362873309, 41.14546169070921877, -59.83891281791527916 ) ) ;
#91793 = CARTESIAN_POINT ( 'NONE',  ( 35.00384615384614762, 1.411358822780289120E-15, 0.000000000000000000 ) ) ;
#91794 = DIRECTION ( 'NONE',  ( 0.000000000000000000, 0.000000000000000000, 1.000000000000000000 ) ) ;
#91796 = CARTESIAN_POINT ( 'NONE',  ( 42.99999999999999289, 464.8825480873695710, 15.07585856869433272 ) ) ;
#91795 = VECTOR ( 'NONE', #100766, 1000.000000000000000 ) ;
#91797 = CARTESIAN_POINT ( 'NONE',  ( 17.85737165039480701, 45.30383319674706399, 5.717692534355065526 ) ) ;
#91798 = CARTESIAN_POINT ( 'NONE',  ( 108.8962094583731215, -60.00000000000000711, 135.2403837889553415 ) ) ;
#91799 = CARTESIAN_POINT ( 'NONE',  ( 29.34999999999999787, -3.309499999999999886, 0.000000000000000000 ) ) ;
#91800 = COLOUR_RGB ( '', 0.72549020, 0.75294118, 0.79215686) ;
#91801 =( NAMED_UNIT ( * ) PLANE_ANGLE_UNIT ( ) SI_UNIT ( $, .RADIAN. ) );
#91802 = EDGE_CURVE ( 'NONE', #39269, #76220, #62142, .T. ) ;
#91803 = ORIENTED_EDGE ( 'NONE', *, *, #45660, .T. ) ;
#91804 = CARTESIAN_POINT ( 'NONE',  ( -97.11318458300092971, -29.99999999999995026, 191.0494389299799991 ) ) ;
#91805 = EDGE_LOOP ( 'NONE', ( #51702, #11651 ) ) ;
#91806 = CARTESIAN_POINT ( 'NONE',  ( 26.78640155871314832, 36.71834478141271774, -10.02603228771729427 ) ) ;
#91807 = CARTESIAN_POINT ( 'NONE',  ( 42.79891897446039906, 462.9518546951013604, 4.196605471998886117 ) ) ;
#91808 = CARTESIAN_POINT ( 'NONE',  ( 23.38792459703088156, 304.7436589798348905, 10.13094752528676068 ) ) ;
#91809 = DIRECTION ( 'NONE',  ( -1.000000000000000000, -1.224606353822377258E-16, -0.000000000000000000 ) ) ;
#91810 = CIRCLE ( 'NONE', #76237, 4.000000000000001776 ) ;
#91811 = CARTESIAN_POINT ( 'NONE',  ( -7.188101187500001821, -21.87500000204838813, -2.977408999572651371 ) ) ;
#91812 = FACE_OUTER_BOUND ( 'NONE', #56162, .T. ) ;
#91813 = CARTESIAN_POINT ( 'NONE',  ( -8.000000000000001776, -11.84375000409677092, 3.313708498984759387 ) ) ;
#91814 = EDGE_CURVE ( 'NONE', #39760, #79581, #73369, .T. ) ;
#91816 = ORIENTED_EDGE ( 'NONE', *, *, #20482, .F. ) ;
#91815 = SURFACE_STYLE_FILL_AREA ( #60004 ) ;
#91817 = CARTESIAN_POINT ( 'NONE',  ( 83.63424747110293822, -25.60960768623118256, 154.1967841724264190 ) ) ;
#91818 = EDGE_CURVE ( 'NONE', #6036, #21078, #31378, .T. ) ;
#91819 = FILL_AREA_STYLE_COLOUR ( '', #89348 ) ;
#91820 = FACE_BOUND ( 'NONE', #46355, .T. ) ;
#91821 = ORIENTED_EDGE ( 'NONE', *, *, #9154, .T. ) ;
#91822 = CARTESIAN_POINT ( 'NONE',  ( -32.87491876135755575, 485.1684955303235824, 5.618973769089859793 ) ) ;
#91823 = CARTESIAN_POINT ( 'NONE',  ( 0.000000000000000000, 0.000000000000000000, 0.000000000000000000 ) ) ;
#91824 = CARTESIAN_POINT ( 'NONE',  ( -7.188101187500000933, -9.500000002048388126, -2.977408999572651371 ) ) ;
#91825 = CARTESIAN_POINT ( 'NONE',  ( -15.90614609307868399, -3.157894736842107530, 14.66382285868950675 ) ) ;
#91826 =( NAMED_UNIT ( * ) PLANE_ANGLE_UNIT ( ) SI_UNIT ( $, .RADIAN. ) );
#91828 = CARTESIAN_POINT ( 'NONE',  ( -22.86828579430564545, 303.4455862872093235, 10.06510526139748585 ) ) ;
#91827 = VECTOR ( 'NONE', #8867, 1000.000000000000000 ) ;
#91829 = VERTEX_POINT ( 'NONE', #104696 ) ;
#91830 = DIRECTION ( 'NONE',  ( 0.000000000000000000, -1.000000000000000000, 0.000000000000000000 ) ) ;
#91831 = CARTESIAN_POINT ( 'NONE',  ( 87.38076970993836312, -46.41592001660386302, 191.3361042550797890 ) ) ;
#91832 = CARTESIAN_POINT ( 'NONE',  ( -2.500000000000000000, 7.216878364870323637, -7.063244554130002406 ) ) ;
#91833 = CARTESIAN_POINT ( 'NONE',  ( 2.977408999572650927, -30.87500000204838813, -7.188101187500001821 ) ) ;
#91834 = CARTESIAN_POINT ( 'NONE',  ( -41.14856704871675674, 488.9704688040295650, 10.18682326004923056 ) ) ;
#91835 = CARTESIAN_POINT ( 'NONE',  ( 8.559508646656398767, 51.83514083332404709, 1.531152949374243510 ) ) ;
#91836 = CARTESIAN_POINT ( 'NONE',  ( 40.91005831554789296, 436.7586844285373218, 21.64591360582873492 ) ) ;
#91837 = CONTEXT_DEPENDENT_SHAPE_REPRESENTATION ( #3182, #77655 ) ;
#91838 = EDGE_LOOP ( 'NONE', ( #28571, #64987, #37474, #36621 ) ) ;
#91839 = DIRECTION ( 'NONE',  ( -1.000000000000000000, 0.000000000000000000, 0.000000000000000000 ) ) ;
#91840 = CARTESIAN_POINT ( 'NONE',  ( 30.59999999999999787, 3.309500000000003439, 4.052968581778167743E-16 ) ) ;
#91841 = CARTESIAN_POINT ( 'NONE',  ( -5.903805371513020539, 4.632738215795892955, -4.999999999999999112 ) ) ;
#91842 = ORIENTED_EDGE ( 'NONE', *, *, #84567, .F. ) ;
#91843 = CARTESIAN_POINT ( 'NONE',  ( -7.500000000000005329, 9.833333333333344584, -68.91429205785459544 ) ) ;
#91844 = CARTESIAN_POINT ( 'NONE',  ( 106.1565704622439483, -57.67112875917140968, 105.3532823125157591 ) ) ;
#91845 = ORIENTED_EDGE ( 'NONE', *, *, #3865, .T. ) ;
#91846 = CARTESIAN_POINT ( 'NONE',  ( 70.41111111111112564, -3.309500000000000774, 0.000000000000000000 ) ) ;
#91847 = SURFACE_STYLE_FILL_AREA ( #59495 ) ;
#91848 = CARTESIAN_POINT ( 'NONE',  ( 99.75754961941544252, 1.030564683017419500E-14, 0.000000000000000000 ) ) ;
#91849 = CARTESIAN_POINT ( 'NONE',  ( 18.39953584734496062, 302.6496520256866916, 9.894388632544812268 ) ) ;
#91850 = CARTESIAN_POINT ( 'NONE',  ( -76.29703970935240420, -59.99999999999999289, 188.1515592608628253 ) ) ;
#91851 = CIRCLE ( 'NONE', #88400, 8.900000000000000355 ) ;
#91852 = DIRECTION ( 'NONE',  ( 0.000000000000000000, 0.000000000000000000, -1.000000000000000000 ) ) ;
#91853 = DIRECTION ( 'NONE',  ( 1.000000000000000000, 1.224606353822377258E-16, 0.000000000000000000 ) ) ;
#91854 = CARTESIAN_POINT ( 'NONE',  ( 34.83349330513380693, -3.851859888774471706E-31, 4.000000000000001776 ) ) ;
#91855 = CARTESIAN_POINT ( 'NONE',  ( -86.40763381868782744, -17.66018640161714615, 176.8075989531612322 ) ) ;
#91856 = AXIS2_PLACEMENT_3D ( 'NONE', #49114, #78986, #38041 ) ;
#91857 = ORIENTED_EDGE ( 'NONE', *, *, #99905, .F. ) ;
#91858 = ADVANCED_FACE ( 'NONE', ( #71784 ), #15152, .F. ) ;
#91859 = CONICAL_SURFACE ( 'NONE', #74679, 3.400000000000000355, 0.9599310885968748153 ) ;
#91860 = ORIENTED_EDGE ( 'NONE', *, *, #94957, .F. ) ;
#91861 = DIRECTION ( 'NONE',  ( 0.000000000000000000, -1.000000000000000000, 0.000000000000000000 ) ) ;
#91862 = EDGE_CURVE ( 'NONE', #36519, #40430, #7572, .T. ) ;
#91863 = CARTESIAN_POINT ( 'NONE',  ( 3.352941176471718077, -1.200583151107622815, 104.5794940929782797 ) ) ;
#91864 = CARTESIAN_POINT ( 'NONE',  ( -83.22986503187559038, -37.77933018691697953, -8.240303472404791663 ) ) ;
#91865 = CARTESIAN_POINT ( 'NONE',  ( -4.312270534944379285, -9.512596744310554797, -11.64851190995530139 ) ) ;
#91866 = CARTESIAN_POINT ( 'NONE',  ( -16.64348903516517098, 43.75610143575153899, 4.157797401561652784 ) ) ;
#91867 = AXIS2_PLACEMENT_3D ( 'NONE', #35324, #74801, #82375 ) ;
#91868 = CARTESIAN_POINT ( 'NONE',  ( 23.21947149027727875, 295.1914306511582708, 2.010027678589071165 ) ) ;
#91869 = CARTESIAN_POINT ( 'NONE',  ( 0.000000000000000000, 0.000000000000000000, 4.000000000000000000 ) ) ;
#91870 = CARTESIAN_POINT ( 'NONE',  ( -22.43826451848009995, 28.20713089197012735, 30.97515248374616448 ) ) ;
#91871 = CARTESIAN_POINT ( 'NONE',  ( 1.384974311275041225, -30.00000000000000000, 37.00000000000000711 ) ) ;
#91872 = CYLINDRICAL_SURFACE ( 'NONE', #44584, 1.250000000000001110 ) ;
#91873 = CARTESIAN_POINT ( 'NONE',  ( -33.15890210479862787, -30.00000000000000711, -37.92163678030271967 ) ) ;
#91874 = CARTESIAN_POINT ( 'NONE',  ( -71.46856667809383623, -32.54058556944256253, 102.5544078860655333 ) ) ;
#91875 = ORIENTED_EDGE ( 'NONE', *, *, #53800, .F. ) ;
#91876 = CARTESIAN_POINT ( 'NONE',  ( 78.68869634200761709, -14.21045842199439591, 170.0117969751115652 ) ) ;
#91877 = CARTESIAN_POINT ( 'NONE',  ( 52.56483885390524335, 40.83906611471594061, -38.23529411764712194 ) ) ;
#91878 = CARTESIAN_POINT ( 'NONE',  ( 113.4549893713481055, -57.67117437226071530, 184.8066837110240783 ) ) ;
#91879 = ORIENTED_EDGE ( 'NONE', *, *, #53663, .F. ) ;
#91880 = CARTESIAN_POINT ( 'NONE',  ( 14.07141389085968974, 41.78883774888220870, -79.52223927790954860 ) ) ;
#91881 = DIRECTION ( 'NONE',  ( -0.000000000000000000, 1.000000000000000000, 1.877893248421449036E-16 ) ) ;
#91882 = EDGE_LOOP ( 'NONE', ( #86612, #73890, #25349, #12573, #76345, #24897 ) ) ;
#91883 =( GEOMETRIC_REPRESENTATION_CONTEXT ( 3 ) GLOBAL_UNCERTAINTY_ASSIGNED_CONTEXT ( ( #66709 ) ) GLOBAL_UNIT_ASSIGNED_CONTEXT ( ( #67286, #59196, #78024 ) ) REPRESENTATION_CONTEXT ( 'NONE', 'WORKASPACE' ) );
#91884 = DIRECTION ( 'NONE',  ( -0.2908996821262230803, -0.5336441332596660869, -0.7941040951766978884 ) ) ;
#91885 = CARTESIAN_POINT ( 'NONE',  ( 7.000000000000000000, 0.000000000000000000, -0.7256075382097185722 ) ) ;
#91886 = CARTESIAN_POINT ( 'NONE',  ( 4.401442555609581635E-16, -14.28125000204838457, -7.188101187500000044 ) ) ;
#91887 = CARTESIAN_POINT ( 'NONE',  ( -10.00000000000000000, 15.00000000000000000, 10.00000000000000000 ) ) ;
#91888 = CIRCLE ( 'NONE', #105653, 7.000000000000000000 ) ;
#91889 = CARTESIAN_POINT ( 'NONE',  ( 0.000000000000000000, -5.629165124598843661, 3.250000000000012879 ) ) ;
#91890 = FILL_AREA_STYLE ('',( #59002 ) ) ;
#91891 = CARTESIAN_POINT ( 'NONE',  ( 6.293430271071538407, -5.026740376715103764, -0.4524126574264524248 ) ) ;
#91892 = DIRECTION ( 'NONE',  ( -1.000000000000000000, 1.776356839400250465E-15, 0.000000000000000000 ) ) ;
#91893 = UNCERTAINTY_MEASURE_WITH_UNIT (LENGTH_MEASURE( 1.000000000000000082E-05 ), #93905, 'distance_accuracy_value', 'NONE');
#91894 = COLOUR_RGB ( '', 0.31764706, 0.68627451, 0.89019608) ;
#91895 = CIRCLE ( 'NONE', #4051, 4.172000000000001485 ) ;
#91896 = ORIENTED_EDGE ( 'NONE', *, *, #53461, .T. ) ;
#91897 = CARTESIAN_POINT ( 'NONE',  ( -6.856834871365124151, 41.38254192121598862, -70.56142688853883271 ) ) ;
#91899 = CARTESIAN_POINT ( 'NONE',  ( 33.23707082931593249, -46.42958337853537643, 35.74295623557356549 ) ) ;
#91898 = CARTESIAN_POINT ( 'NONE',  ( -3.369683342533021708, -49.08678202233276977, 104.1613013819151519 ) ) ;
#91900 = CARTESIAN_POINT ( 'NONE',  ( 23.77225596033269284, 305.6233131784293846, -8.833847462781667659 ) ) ;
#91901 = ORIENTED_EDGE ( 'NONE', *, *, #57683, .F. ) ;
#91902 = CARTESIAN_POINT ( 'NONE',  ( -1.250906133227802419, 15.60029824371900276, 50.60801902191838053 ) ) ;
#91903 = ADVANCED_FACE ( 'NONE', ( #24346 ), #19122, .F. ) ;
#91904 = EDGE_LOOP ( 'NONE', ( #28416, #90954, #1500, #29687 ) ) ;
#91906 = CARTESIAN_POINT ( 'NONE',  ( -5.062272329161832118, -5.000000000000001776, -8.716576110314617765 ) ) ;
#91905 = CARTESIAN_POINT ( 'NONE',  ( 0.2573354458087849794, -6.889406814520515177, 1.067197363239225538 ) ) ;
#91907 = CARTESIAN_POINT ( 'NONE',  ( 4.854898838401722649, 40.57569111244889370, -70.80100276615310406 ) ) ;
#91908 = LINE ( 'NONE', #105952, #8645 ) ;
#91909 = CARTESIAN_POINT ( 'NONE',  ( -89.99999999999997158, -38.00000000001091394, 196.0238439516549818 ) ) ;
#91910 = CARTESIAN_POINT ( 'NONE',  ( -36.69951191943324176, 463.3005535825507764, 20.13750663043760625 ) ) ;
#91911 = ORIENTED_EDGE ( 'NONE', *, *, #81811, .F. ) ;
#91912 = CARTESIAN_POINT ( 'NONE',  ( 81.11655526126887139, -60.00000000000000000, -27.26544461796351371 ) ) ;
#91913 = CARTESIAN_POINT ( 'NONE',  ( -10.28624191511820207, 45.38549880562041494, 15.40779740156164124 ) ) ;
#91914 = CARTESIAN_POINT ( 'NONE',  ( 32.14710229350392012, 464.7836479068001267, 11.45504703818881609 ) ) ;
#91915 = CARTESIAN_POINT ( 'NONE',  ( 41.58908019493944863, 487.6887286007225271, 9.912025820237996498 ) ) ;
#91916 = CARTESIAN_POINT ( 'NONE',  ( 0.000000000000000000, 0.000000000000000000, -0.4455245229258316120 ) ) ;
#91917 = EDGE_CURVE ( 'NONE', #51593, #4237, #96534, .T. ) ;
#91918 = ORIENTED_EDGE ( 'NONE', *, *, #12154, .T. ) ;
#91919 = ADVANCED_FACE ( 'NONE', ( #63732 ), #90639, .T. ) ;
#91920 = LINE ( 'NONE', #92435, #12579 ) ;
#91921 = VERTEX_POINT ( 'NONE', #25959 ) ;
#91922 = EDGE_LOOP ( 'NONE', ( #19236, #56540, #62115, #10891, #69510 ) ) ;
#91923 = DIRECTION ( 'NONE',  ( 0.000000000000000000, 0.000000000000000000, 1.000000000000000000 ) ) ;
#91924 = PRESENTATION_STYLE_ASSIGNMENT (( #58503 ) ) ;
#91925 = CARTESIAN_POINT ( 'NONE',  ( 57.45015997180046696, 6.975173280561618775E-15, 0.000000000000000000 ) ) ;
#91926 = CARTESIAN_POINT ( 'NONE',  ( 28.58349330513380337, 4.000000000000002665, 0.000000000000000000 ) ) ;
#91927 = CARTESIAN_POINT ( 'NONE',  ( 83.52925484045992732, -45.27642508538186661, -13.37253514952393552 ) ) ;
#91928 = CARTESIAN_POINT ( 'NONE',  ( -37.17110534794960586, 304.2510796055892115, -7.844238214609251969 ) ) ;
#91929 = CARTESIAN_POINT ( 'NONE',  ( -6.779925268006731898, 303.7378072031825127, -10.02423307061381230 ) ) ;
#91930 = ORIENTED_EDGE ( 'NONE', *, *, #39752, .F. ) ;
#91931 = CARTESIAN_POINT ( 'NONE',  ( -43.74985542820359541, 435.5770091380368854, 16.96136490515567985 ) ) ;
#91932 = ORIENTED_EDGE ( 'NONE', *, *, #36831, .F. ) ;
#91933 = CARTESIAN_POINT ( 'NONE',  ( 9.324240130834043683, 51.33788018723820556, -3.783820555081815140 ) ) ;
#91934 = CIRCLE ( 'NONE', #50560, 0.5999999999999980904 ) ;
#91936 = VERTEX_POINT ( 'NONE', #91192 ) ;
#91935 = DIRECTION ( 'NONE',  ( -1.000000000000000000, -0.000000000000000000, -0.000000000000000000 ) ) ;
#91937 = CARTESIAN_POINT ( 'NONE',  ( 75.71757240347274376, -53.37388941686415222, 134.6993321033900486 ) ) ;
#91938 = EDGE_CURVE ( 'NONE', #99464, #45751, #50173, .T. ) ;
#91939 = CIRCLE ( 'NONE', #76445, 4.999999999999999112 ) ;
#91940 = ORIENTED_EDGE ( 'NONE', *, *, #40871, .T. ) ;
#91941 = CARTESIAN_POINT ( 'NONE',  ( 6.999999999999997335, -46.00000000000000000, 39.12435565298214613 ) ) ;
#91942 = PRESENTATION_LAYER_ASSIGNMENT (  '', '', ( #100560 ) ) ;
#91943 = CARTESIAN_POINT ( 'NONE',  ( -5.082755093536326818, -25.71875000204838813, 5.082755093536325042 ) ) ;
#91944 = CARTESIAN_POINT ( 'NONE',  ( -109.3314759607053759, -57.67120315069445269, 124.6891463060778165 ) ) ;
#91945 = EDGE_CURVE ( 'NONE', #99731, #47025, #100314, .T. ) ;
#91946 = ORIENTED_EDGE ( 'NONE', *, *, #23416, .T. ) ;
#91947 = DIRECTION ( 'NONE',  ( 0.5735764363510491570, -0.8191520442889895781, 1.003171929053522035E-16 ) ) ;
#91948 = CARTESIAN_POINT ( 'NONE',  ( 103.5970710204898779, -45.28273151134633423, 181.5168165621360572 ) ) ;
#91949 = EDGE_CURVE ( 'NONE', #20613, #33098, #90104, .T. ) ;
#91950 = CARTESIAN_POINT ( 'NONE',  ( -36.35334569080745126, 28.20664209161598635, -11.89422708507966497 ) ) ;
#91951 = DIRECTION ( 'NONE',  ( 0.000000000000000000, 0.000000000000000000, 1.000000000000000000 ) ) ;
#91952 = CARTESIAN_POINT ( 'NONE',  ( 3.313708498984762496, -23.46875000409677270, 7.999999999999998224 ) ) ;
#91953 = EDGE_CURVE ( 'NONE', #46925, #94099, #89686, .T. ) ;
#91954 = DIRECTION ( 'NONE',  ( -0.000000000000000000, 1.000000000000000000, -0.000000000000000000 ) ) ;
#91955 = DIRECTION ( 'NONE',  ( -1.000000000000000000, -1.224606353822377258E-16, -0.000000000000000000 ) ) ;
#91956 = SURFACE_STYLE_FILL_AREA ( #42874 ) ;
#91957 = DIRECTION ( 'NONE',  ( 0.000000000000000000, 0.000000000000000000, -1.000000000000000000 ) ) ;
#91959 = AXIS2_PLACEMENT_3D ( 'NONE', #73082, #9411, #84396 ) ;
#91958 = DIRECTION ( 'NONE',  ( 1.000000000000000000, 0.000000000000000000, 0.000000000000000000 ) ) ;
#91960 = DIRECTION ( 'NONE',  ( -1.000000000000000000, -1.224606353822377258E-16, -0.000000000000000000 ) ) ;
#91961 = ORIENTED_EDGE ( 'NONE', *, *, #45015, .F. ) ;
#91962 = CARTESIAN_POINT ( 'NONE',  ( 6.874999999999996447, -4.690970937165717558, -7.298562697733106397 ) ) ;
#91963 =( LENGTH_UNIT ( ) NAMED_UNIT ( * ) SI_UNIT ( .MILLI., .METRE. ) );
#91964 = CARTESIAN_POINT ( 'NONE',  ( 1.167959526168962814, 9.592220699621755386, 50.96201451364633783 ) ) ;
#91965 = CONICAL_SURFACE ( 'NONE', #14414, 13.50000000000000178, 1.047197551196596077 ) ;
#91966 = CARTESIAN_POINT ( 'NONE',  ( -84.91616747946434884, -29.99999999999999289, 169.5307764630179008 ) ) ;
#91967 = MECHANICAL_DESIGN_GEOMETRIC_PRESENTATION_REPRESENTATION (  '', ( #50592 ), #4139 ) ;
#91968 = EDGE_LOOP ( 'NONE', ( #73483, #10272, #47997, #40967 ) ) ;
#91969 = DIRECTION ( 'NONE',  ( -0.000000000000000000, 0.000000000000000000, 1.000000000000000000 ) ) ;
#91970 = CARTESIAN_POINT ( 'NONE',  ( 73.61960571407516341, -57.62828218540514769, 185.1312174396749413 ) ) ;
#91972 = CARTESIAN_POINT ( 'NONE',  ( 10.28624191511840458, -1.200000000000000030E-05, 15.40779740156149202 ) ) ;
#91971 = FILL_AREA_STYLE_COLOUR ( '', #36332 ) ;
#91973 = CARTESIAN_POINT ( 'NONE',  ( 28.41704268849491299, -28.98892241734421660, -38.24770077405835877 ) ) ;
#91974 = FILL_AREA_STYLE ('',( #262 ) ) ;
#91975 = CARTESIAN_POINT ( 'NONE',  ( -41.38414514539831401, -60.00000000000000000, 54.16917059837041393 ) ) ;
#91976 = DIRECTION ( 'NONE',  ( 1.224646799147353207E-16, 0.000000000000000000, -1.000000000000000000 ) ) ;
#91977 = CARTESIAN_POINT ( 'NONE',  ( -85.53935049295719750, -53.83736247170576661, 191.4365733638258291 ) ) ;
#91978 = EDGE_LOOP ( 'NONE', ( #50653, #40342, #67278, #72446 ) ) ;
#91979 = DIRECTION ( 'NONE',  ( 0.5735764363510491570, -0.8191520442889895781, 1.003171929053522035E-16 ) ) ;
#91980 = CARTESIAN_POINT ( 'NONE',  ( -6.121071711750540878, -42.95758222298059081, 31.03938273056196806 ) ) ;
#91981 = CYLINDRICAL_SURFACE ( 'NONE', #29186, 1.250000000000001110 ) ;
#91982 = CARTESIAN_POINT ( 'NONE',  ( -1.226484165780726832, -49.99515885551645766, 101.2642634682685951 ) ) ;
#91983 = B_SPLINE_SURFACE_WITH_KNOTS ( 'NONE', 3, 3, ( 
 ( #70503, #30589, #95836, #79111, #12243, #62414, #55346, #21967, #79634, #103392, #6264, #29542, #87751 ),
 ( #21440, #54275, #38160, #64015, #63480, #13297, #45175, #46224, #46743, #5750, #96378, #88276, #39202 ),
 ( #72079, #23027, #78053, #800, #58006, #32712, #74717, #90390, #23557, #15429, #56402, #66108, #33769 ),
 ( #8924, #40238, #73114, #48843, #106019, #66644, #16495, #56936, #81736, #49379, #97944, #14889, #57466 ),
 ( #32165, #81210, #65047, #98987, #24094, #99528, #89857, #41830, #33234, #25150, #25705, #15965, #7859 ),
 ( #74188, #40766, #73657, #98465, #90931, #64531, #48317, #17043, #106560, #49918, #97396, #88798, #65581 ),
 ( #24619, #47784, #82287, #89337, #266, #8399, #41301, #82825, #7326, #80687, #6807, #39725, #72602 ),
 ( #105507, #31647, #2431, #101674, #27832, #19738, #50970, #67714, #43967, #52575, #60702, #93585, #35378 ),
 ( #50440, #101139, #83352, #36454, #102197, #76856, #43439, #100599, #76318, #69318, #67190, #34844, #9449 ),
 ( #26760, #3513, #2963, #10523, #19212, #59632, #68245, #59095, #85499, #27299, #83884, #58567, #51515 ),
 ( #60182, #44508, #91977, #92506, #18661, #93050, #9998, #84433, #18115, #52044, #11581, #84958, #11045 ),
 ( #35920, #77397, #91464, #68791, #42363, #34313, #17578, #75250, #42903, #1891, #1351, #100067, #75797 ),
 ( #26233, #29931, #77932, #28899, #6146, #54690, #62817, #30464, #70899, #53127, #45574, #103788, #46100 ),
 ( #22382, #104314, #54155, #96257, #39077, #71413, #5107, #87097, #69841, #47139, #20814, #45049, #20276 ),
 ( #38038, #71958, #61772, #63358, #53648, #95187, #95710, #87624, #4040, #21849, #62296, #86044, #13173 ),
 ( #55227, #78983, #94110, #13708, #46618, #88152, #14233, #36973, #79515, #28345, #86578, #80033, #94669 ),
 ( #12119, #102738, #61225, #5627, #12642, #78453, #4574, #37511, #38548, #70374, #103269, #29419, #21318 ),
 ( #63885, #82158, #98859, #24507, #89210, #32588, #32050, #96775, #89743, #8271, #41184, #56820, #22904 ),
 ( #98352, #25022, #33117, #47667, #49255, #104861, #97282, #16919, #105388, #65984, #88675, #14765, #57877 ),
 ( #80562, #56272, #72481, #82698, #74061, #57341, #150, #40119, #8804, #15308, #6682, #90802, #81097 ),
 ( #90262, #39608, #16365, #15838, #64928, #41712, #48196, #49795, #48720, #65460, #31528, #31003, #64409 ),
 ( #81608, #55741, #72994, #7735, #23434, #7210, #40645, #105899, #97814, #23979, #73527, #106430, #60575 ),
 ( #42770, #9857, #10390, #26113, #34718, #75120, #76191, #35788, #51382, #84297, #83749, #34184, #91855 ),
 ( #67060, #101546, #58970, #17980, #67592, #50842, #52443, #2291, #75661, #100470, #35239, #1761, #671 ),
 ( #11450, #26630, #99937, #59502, #51915, #92374, #85361, #18522, #27699, #19075, #84831, #93466, #43308 ),
 ( #68105, #60054, #101004, #27162, #92910, #76720, #50320, #1215, #10911, #43830, #68667, #83226, #19614 ),
 ( #9320, #2833, #74594, #33635, #42231, #66516, #99389, #25573, #58431, #91340, #17454, #38425, #79382 ),
 ( #95580, #44374, #36848, #63219, #44919, #5501, #28223, #61095, #71289, #29813, #20143, #102607, #11989 ),
 ( #54557, #103662, #87495, #86453, #22244, #61644, #93983, #104182, #20685, #52996, #70767, #85916, #62688 ),
 ( #4435, #88021, #94535, #13576, #103143, #4979, #77804, #46492, #3916, #54028, #96110, #69714, #102065 ),
 ( #30326, #21715, #28764, #77271, #12514, #45444, #21198, #78320, #53524, #37380, #55091, #3382, #29290 ),
 ( #36325, #95063, #69194, #45970, #70241, #62173, #86971, #13039, #78848, #37907, #56688, #6015, #96638 ),
 ( #106294, #39476, #64282, #30872, #63751, #80433, #32457, #40517, #15704, #22774, #14626, #98733, #73394 ),
 ( #16234, #89610, #38939, #31404, #48592, #31917, #17, #8145, #90132, #39995, #82019, #24889, #57213 ),
 ( #72868, #55611, #32984, #6543, #88548, #71816, #104719, #97677, #57741, #47538, #49119, #72354, #80963 ),
 ( #65329, #105257, #81481, #48065, #97151, #105778, #98217, #23299, #56134, #89079, #41051, #15176, #73935 ),
 ( #7079, #64794, #23843, #14101, #7598, #24370, #65855, #47007, #79905, #16775, #59378, #27574, #42105 ),
 ( #74989, #67985, #66931, #101423, #91736, #10785, #35117, #100871, #2707, #99812, #17855, #51246, #76062 ),
 ( #50708, #100343, #92785, #66381, #17323, #27033, #83620, #51788, #99261, #43705, #9724, #25438, #34592 ),
 ( #42640, #58292, #2164, #84173, #26506, #92239, #83100, #43181, #1082, #68534, #25983, #67465, #8676 ),
 ( #18394, #59918, #18946, #84700, #9194, #58843, #76596, #35655, #90665, #49664, #10269, #82572, #41578 ),
 ( #91219, #74464, #544, #33507, #50198, #75538, #34057, #1633, #44247, #54422, #36726, #77139, #86843 ),
 ( #12917, #45316, #20565, #104057, #3790, #103538, #12388, #21075, #3256, #62558, #28098, #70110, #79258 ),
 ( #11318, #53404, #46368, #45840, #20018, #60453, #102483, #61510, #37248, #94403, #36197, #69065, #29686 ),
 ( #103019, #11862, #86322, #60973, #62050, #21590, #29174, #94939, #37783, #87367, #78712, #44792, #93328 ),
 ( #78198, #69592, #4312, #71162, #101938, #28627, #85231, #95444, #53911, #5382, #4849, #70644, #13447 ),
 ( #38302, #93859, #19482, #52319, #85789, #52861, #77681, #6954, #15043, #17599, #63630, #105133, #72230 ),
 ( #88424, #97030, #30744, #31788, #99549, #39871, #72743, #39353, #96520, #47410, #58583, #22651, #91484 ),
 ( #14497, #23170, #80302, #9468, #64671, #31274, #56014, #97544, #64158, #63085, #105647, #75271, #6414 ),
 ( #88948, #7470, #47933, #42380, #80841, #50461, #81360, #40387, #83371, #23705, #56558, #89485, #15579 ),
 ( #48470, #73269, #32327, #5885, #55487, #106167, #66664, #25725, #38815, #30198, #95985, #71681, #22111 ),
 ( #54965, #87894, #104588, #13976, #46881, #79785, #93069, #85521, #44530, #60200, #67210, #43986, #101693 ),
 ( #36472, #50989, #52594, #1369, #100617, #20298, #1911, #69341, #91997, #18133, #102220, #93609, #83903 ),
 ( #75816, #86067, #11599, #60722, #77418, #43461, #12138, #18680, #10017, #28368, #51536, #3534, #19235 ),
 ( #42924, #61246, #34864, #11062, #53149, #67733, #59117, #101158, #94130, #19760, #26780, #45067, #76337 ),
 ( #84980, #2450, #59649, #92525, #34335, #100084, #52065, #84450, #26254, #10543, #76873, #35397, #2985 ),
 ( #68265, #27320, #35940, #68811, #27853, #13727, #69862, #53665, #14787, #63377, #103293, #21337, #94687 ),
 ( #37529, #96274, #104330, #79531, #20835, #78471, #55760, #30478, #5644, #80052, #46634, #102756, #95205 ),
 ( #22400, #96791, #54174, #79006, #38568, #55244, #29952, #5126, #87644, #6163, #86599, #4595, #14252 ),
 ( #39095, #12663, #104885, #38059, #45594, #21867, #88691, #62835, #70394, #88168, #71428, #47157, #71975 ),
 ( #31024, #29439, #77949, #13190, #54707, #28917, #63905, #22923, #4064, #36992, #61793, #62312, #87116 ),
 ( #46121, #70915, #103807, #95726, #33132, #23455, #105916, #15327, #25591, #57896, #169, #90820, #89761 ),
 ( #64943, #31548, #41727, #23996, #64430, #74083, #56291, #66002, #32607, #7752, #91358, #89229, #56837 ),
 ( #16936, #15858, #99409, #98879, #106449, #8291, #48736, #57362, #48213, #49814, #65480, #73012, #47682 ),
 ( #24522, #98369, #33656, #81118, #81629, #40662, #90281, #32069, #73545, #7225, #49271, #8823, #16384 ),
 ( #82175, #40135, #97835, #74611, #41197, #691, #25039, #82719, #66535, #58449, #80580, #6701, #39629 ),
 ( #72500, #105405, #97300, #92930, #61111, #75682, #9878, #1781, #101562, #100488, #28241, #18539, #44392 ),
 ( #68681, #36342, #26645, #51404, #84845, #2849, #76208, #84315, #27177, #19630, #99959, #50861, #60593 ),
 ( #85381, #26132, #77288, #10412, #58986, #68126, #17473, #2313, #91874, #35803, #10928, #60067, #19092 ),
 ( #76739, #34738, #102079, #59520, #101023, #42248, #11465, #51933, #93481, #52463, #3400, #42789, #92391 ),
 ( #69213, #50336, #83245, #43849, #9338, #75139, #27719, #1234, #34204, #67076, #18001, #83767, #67609 ),
 ( #35259, #43327, #71306, #88040, #13591, #78336, #30887, #5517, #78867, #103159, #4994, #104737, #93998 ),
 ( #70787, #45987, #28780, #6032, #86472, #3932, #85934, #12005, #103683, #20160, #94551, #30342, #12528 ),
 ( #95595, #46505, #69731, #21732, #21212, #44938, #37925, #104199, #63236, #29827, #53010, #62704, #87511 ),
 ( #22261, #36863, #38440, #77822, #45463, #38954, #20703, #55110, #102622, #61662, #14120, #79401, #53541 ),
 ( #4453, #71831, #96128, #47021, #79923, #29304, #37397, #70258, #62194, #95080, #54041, #86988, #13055 ),
 ( #54572, #48610, #23858, #560, #7096, #35, #15725, #24392, #47553, #65874, #31420, #73412, #82589 ),
 ( #14644, #56702, #49683, #49139, #23314, #63768, #105794, #64811, #40533, #97693, #80449, #6560, #33007 ),
 ( #81495, #39493, #8694, #98753, #7615, #41602, #65345, #105274, #97167, #64295, #41070, #74485, #24907 ),
 ( #55626, #72368, #96656, #82039, #89094, #40011, #56150, #15189, #48078, #8163, #90149, #98236, #80980 ),
 ( #22791, #16254, #57231, #57761, #106309, #88563, #72883, #32474, #73954, #31933, #90687, #16796, #89625 ),
 ( #42123, #84192, #44269, #92259, #1104, #51809, #27056, #43200, #2185, #26002, #92806, #91755, #11337 ),
 ( #10288, #58312, #27593, #76085, #76615, #2727, #101440, #58865, #42659, #18965, #60475, #35678, #68554 ),
 ( #93354, #25459, #35135, #91237, #77161, #33528, #75009, #17344, #59940, #66400, #34078, #51270, #99281 ),
 ( #19506, #84722, #17875, #50219, #10807, #18413, #75559, #68005, #83120, #66951, #9743, #9215, #52340 ),
 ( #100890, #85253, #99830, #50728, #26525, #83638, #43724, #1654, #34612, #67483, #100362, #59398, #4334 ),
 ( #52884, #46388, #5401, #62071, #93879, #22131, #79279, #53931, #96006, #4868, #44812, #36748, #77699 ),
 ( #54983, #38322, #45859, #101958, #85809, #46904, #95465, #28647, #53425, #20038, #11884, #69610, #21612 ),
 ( #37805, #3811, #102504, #87913, #29708, #70667, #71184, #78733, #28118, #20586, #103558, #21097, #13995 ),
 ( #104077, #29196, #30219, #3277, #63105, #86863, #94960, #61531, #36217, #94424, #86343, #60993, #12409 ),
 ( #69085, #45340, #62582, #78218, #37268, #70132, #103038, #12938, #54442, #87392, #13467, #97565, #38836 ),
 ( #63648, #106186, #88447, #32348, #64695, #39890, #16667, #23191, #16130, #31805, #40407, #96538, #81914 ),
 ( #89503, #98635, #6433, #30762, #72764, #65754, #65220, #39371, #79807, #15066, #80860, #56580, #6972 ),
 ( #22669, #49014, #8031, #23729, #55507, #24785, #40943, #15598, #57634, #81383, #14519, #72248, #47431 ),
 ( #90559, #73835, #48488, #71699, #80321, #5906, #98113, #105150, #56036, #31293, #64179, #97049, #24262 ),
 ( #7493, #88969, #47953, #104611, #57111, #73289, #106730, #90024, #105670, #32879, #18290, #67359, #35549 ),
 ( #18838, #75432, #10684, #60344, #92682, #26404, #1524, #91110, #68422, #42002, #66277, #41471, #74359 ),
 ( #93220, #50092, #51682, #74882, #9621, #51145, #75965, #25323, #84063, #83518, #437, #34490, #26930 ),
 ( #100238, #8568, #92142, #43078, #43600, #84602, #99165, #100764, #49558, #969, #101317, #82999, #76491 ),
 ( #59270, #2598, #66820, #27467, #9094, #82467, #33951, #99709, #42530, #25879, #33408, #10164, #17747 ),
 ( #2063, #58738, #58183, #35013, #17219, #91634, #50603, #67878, #59803, #102369, #30098, #20456, #46267 ),
 ( #5279, #13341, #95347, #45218, #87263, #62984, #62455, #102907, #78093, #60866, #38202, #11750, #36091 ),
 ( #44142, #29074, #19383, #19908, #21483, #44684, #86216, #20978, #45730, #101833, #53811, #53297, #11211 ),
 ( #103434, #54318, #4211, #85126, #61941, #12815, #79152, #71063, #68962, #70546, #52214, #77571, #103954 ),
 ( #77030, #3147, #27997, #93754, #4743, #52752, #3688, #85673, #36618, #29585, #78611, #69483, #61399 ),
 ( #28516, #94291, #12288, #37141, #70006, #37683, #94833, #86742, #80734, #55906, #32758, #39249, #32214 ),
 ( #56453, #79682, #97990, #63522, #105551, #7906, #22552, #46790, #88843, #81783, #81261, #55393, #95884 ),
 ( #96932, #72651, #23068, #5793, #38714, #65094, #24144, #47830, #71579, #40812, #56986, #39775, #73706 ),
 ( #30634, #88324, #96421, #104484, #87792, #13874, #31690, #22009, #14396, #89902, #47309, #14936, #97442 ),
 ( #80203, #23604, #6852, #6308, #64577, #73162, #16011, #89385, #54864, #15477, #48368, #48890, #106608 ),
 ( #40287, #72123, #105033, #31174, #64057, #7374, #106065, #49430, #100645, #51018, #41348, #17090, #33281 ),
 ( #74239, #82339, #92024, #43486, #66152, #83398, #24662, #42952, #59676, #18159, #49967, #2475, #83932 ),
 ( #65631, #8970, #1939, #17625, #26280, #8446, #67757, #99034, #75301, #84477, #25200, #16543, #58610 ),
 ( #10045, #58056, #98514, #843, #66693, #42407, #99575, #316, #90979, #34891, #26803, #50485, #82874 ),
 ( #92556, #9495, #51561, #67238, #41875, #74764, #33817, #75844, #10569, #18706, #1397, #57515, #25751 ),
 ( #76362, #91510, #34363, #100115, #59142, #90436, #22287, #61820, #37021, #85005, #35968, #14669, #96154 ),
 ( #38983, #77975, #60227, #52621, #4092, #53177, #22817, #30912, #6057, #61271, #104762, #47578, #79947 ),
 ( #94162, #76904, #55651, #27883, #63794, #55135, #19787, #80473, #88064, #20330, #44559, #86093, #35423 ),
 ( #11629, #93095, #71858, #3560, #88589, #14144, #12164, #102784, #36498, #45095, #68838, #96679, #69889 ),
 ( #68294, #28398, #28947, #47048, #101188, #101716, #69366, #77446, #27349, #93637, #102246, #60749, #19267 ),
 ( #52095, #11089, #44014, #85548, #3015, #33554, #72909, #66425, #64840, #97718, #73442, #23884, #91260 ),
 ( #23340, #105819, #98781, #33031, #8189, #56179, #7119, #17370, #65898, #41097, #8718, #49164, #31443 ),
 ( #82070, #24417, #99309, #588, #82616, #32500, #74511, #50242, #49710, #90176, #65371, #48104, #25481 ),
 ( #89119, #105298, #64323, #16280, #6586, #40034, #41626, #31960, #106336, #73977, #24936, #15216, #60 ),
 ( #97195, #98263, #90715, #58337, #57255, #72394, #57787, #16825, #39518, #81005, #56727, #89649, #15750 ),
 ( #48634, #81518, #7643, #40559, #66976, #11362, #68577, #58888, #34638, #50754, #61017, #93376, #35702 ),
 ( #93904, #83661, #100914, #42149, #60496, #9772, #44289, #99856, #26029, #77184, #101462, #91779, #67506 ),
 ( #20059, #19527, #27613, #52363, #18439, #83145, #100387, #17902, #3295, #59421, #42687, #2749, #75583 ),
 ( #68024, #43225, #9242, #26549, #85275, #35157, #43748, #1681, #36238, #92284, #92826, #101980, #51294 ),
 ( #76108, #69107, #28140, #84214, #75033, #10309, #2208, #59963, #27080, #18987, #51831, #1131, #34104 ),
 ( #84744, #10828, #76640, #45879, #30238, #70687, #28669, #94449, #61554, #87413, #96027, #5418, #4892 ),
 ( #12430, #62088, #45360, #22152, #103577, #103060, #94980, #29727, #37290, #52908, #62601, #85830, #78241 ),
 ( #4354, #46411, #70156, #11906, #21117, #55003, #79297, #38342, #87934, #29216, #53949, #21631, #13488 ),
 ( #86884, #95486, #71203, #20606, #12957, #104098, #78758, #63127, #53444, #44835, #37825, #86365, #54462 ),
 ( #77721, #3832, #36767, #69633, #102525, #11172, #34972, #101793, #100724, #20411, #84560, #93176, #67317 ),
 ( #19344, #85631, #11706, #3643, #67836, #51642, #27960, #101276, #3103, #26364, #44643, #10126, #52173 ),
 ( #75923, #100199, #35502, #28476, #60823, #2024, #86173, #10643, #43560, #85088, #76446, #59227, #92101 ),
 ( #77527, #27427, #18244, #61357, #36579, #44099, #94250, #76987, #84020, #26887, #43035, #19868, #53255 ),
 ( #36048, #34448, #51101, #42490, #93715, #59760, #92638, #18796, #2555, #68381, #52704, #68919, #69445 ),
 ( #60304, #75386, #102327, #1484, #2559, #85637, #60827, #61901, #86177, #12249, #53775, #11175, #36052 ),
 ( #45694, #78056, #11710, #93719, #76450, #86705, #27431, #51645, #26891, #59766, #44647, #78574, #35507 ),
 ( #34976, #19872, #68386, #53259, #28480, #77531, #3648, #60308, #94254, #93182, #12776, #76994, #36582 ),
 ( #29035, #69449, #4174, #37105, #102870, #19348, #44103, #20415, #94796, #69968, #20939, #102331, #67838 ),
 ( #61361, #92642, #100729, #18800, #43564, #84566, #45179, #10647, #101280, #52708, #52177, #85091, #3106 ),
 ( #68922, #101796, #27964, #96382, #13836, #22511, #15433, #71023, #37643, #72607, #48321, #80164, #55351 ),
 ( #105510, #80691, #30594, #31651, #4709, #47787, #88280, #63483, #46227, #23562, #103914, #21444, #103395 ),
 ( #14356, #70507, #5238, #6811, #30062, #71540, #6268, #31132, #87222, #39206, #38675, #29547, #47268 ),
 ( #39729, #72082, #62418, #104990, #64021, #64535, #97400, #54279, #55865, #95312, #62944, #56406, #38164 ),
 ( #13302, #79115, #89341, #96897, #95840, #21971, #54825, #87755, #14893, #23031, #46748, #79638, #5755 ),
 ( #104443, #88804, #57471, #65052, #803, #89862, #33772, #66112, #41306, #18118, #24623, #17583, #33238 ),
 ( #97948, #83355, #48847, #90935, #100070, #7863, #32169, #74192, #67193, #66647, #40770, #81215, #16498 ),
 ( #58010, #98991, #26237, #73661, #49383, #82291, #17046, #32716, #271, #81740, #82830, #42366, #49922 ),
 ( #90394, #106565, #98470, #1354, #65585, #34316, #8403, #25154, #8929, #41833, #59099, #74720, #99531 ),
 ( #25708, #58570, #91467, #24098, #50443, #91980, #9452, #75253, #15969, #7330, #40242, #56940, #73118 ),
 ( #106023, #94672, #51518, #94113, #43443, #11048, #52578, #77400, #26763, #85502, #84962, #42906, #35923 ),
 ( #20279, #2966, #10001, #93589, #44511, #45051, #86047, #100602, #102201, #50973, #76321, #69844, #84436 ),
 ( #34848, #67717, #12122, #36457, #59634, #2434, #18664, #28902, #61228, #3516, #53130, #93053, #61775 ),
 ( #92509, #77936, #27302, #10526, #69323, #35381, #28348, #68794, #43970, #83887, #101142, #4044, #101677 ),
 ( #68248, #36976, #60185, #60705, #102741, #19216, #1894, #76859, #75800, #52047, #27835, #19741, #11584 ),
 ( #105771, #23293, #37514, #70377, #65323, #24364, #80959, #4577, #41046, #98211, #72863, #8138, #23837 ) ),
 .UNSPECIFIED., .F., .F., .F.,
 ( 4, 3, 3, 3, 3, 3, 3, 3, 3, 3, 3, 3, 3, 3, 3, 3, 3, 3, 3, 3, 3, 3, 3, 3, 3, 3, 3, 3, 3, 3, 3, 3, 3, 3, 3, 3, 3, 3, 3, 3, 3, 3, 3, 3, 3, 3, 3, 3, 3, 3, 3, 3, 3, 4 ),
 ( 4, 3, 3, 3, 4 ),
 ( 0.8179795923582280359, 0.8194016267929293829, 0.8201126440102800563, 0.8208236612276307298, 0.8236677300970334237, 0.8243787473143840971, 0.8250897645317347706, 0.8265117989664361176, 0.8279338334011374645, 0.8293558678358388114, 0.8321999367052415053, 0.8350440055746441992, 0.8364660400093455461, 0.8378880744440468931, 0.8407321433134495869, 0.8435762121828522808, 0.8464202810522549747, 0.8521084187910603625, 0.8577965565298657502, 0.8634846942686710269, 0.8691728320074763037, 0.8748609697462816914, 0.8862372452238924669, 0.9089897961791140180, 0.9203660716567247935, 0.9232101405261274873, 0.9260542093955301812, 0.9317423471343355690, 0.9374304848731409567, 0.9431186226119463445, 0.9459626914813490384, 0.9488067603507517322, 0.9516508292201544261, 0.9544948980895570090, 0.9559169325242582449, 0.9573389669589595918, 0.9601830358283622857, 0.9630271046977649796, 0.9658711735671676735, 0.9687152424365703673, 0.9715593113059730612, 0.9722703285233237347, 0.9729813457406744082, 0.9744033801753757551, 0.9758254146100771020, 0.9772474490447784490, 0.9800915179141811429, 0.9829355867835838367, 0.9857796556529865306, 0.9886237245223892245, 0.9914677933917919184, 0.9943118622611946122, 0.9971559311305973061, 1.000000000000000000 ),
 ( 0.03164164694831613639, 0.3798059082496895167, 0.7279701695510628623, 1.076134430852436319, 1.424298692153809665 ),
 .UNSPECIFIED. ) ;
#91985 = CARTESIAN_POINT ( 'NONE',  ( 5.009049782182684041, -64.84921313000529608, 13.89804781769288944 ) ) ;
#91984 = CARTESIAN_POINT ( 'NONE',  ( 33.76105693399937024, 471.3091059247025782, 5.717665057388511940 ) ) ;
#91986 = EDGE_CURVE ( 'NONE', #57238, #74417, #60441, .T. ) ;
#91987 = ORIENTED_EDGE ( 'NONE', *, *, #85967, .T. ) ;
#91989 = CARTESIAN_POINT ( 'NONE',  ( 38.54515645702225868, 5.000000000000003553, 0.000000000000000000 ) ) ;
#91988 = MECHANICAL_DESIGN_GEOMETRIC_PRESENTATION_REPRESENTATION (  '', ( #54097 ), #36981 ) ;
#91990 = CARTESIAN_POINT ( 'NONE',  ( 18.58349330513380337, 1.593028355512270567E-15, 0.000000000000000000 ) ) ;
#91991 = CARTESIAN_POINT ( 'NONE',  ( 81.98192093697382177, -38.00000000001091394, -13.86368299876859567 ) ) ;
#91992 = CARTESIAN_POINT ( 'NONE',  ( 34.45135090351298146, 300.8539718218502230, -8.652709364234928202 ) ) ;
#91993 = EDGE_CURVE ( 'NONE', #83753, #26189, #38051, .T. ) ;
#91994 = CARTESIAN_POINT ( 'NONE',  ( -13.00000000000003730, -85.00000000000000000, 0.000000000000000000 ) ) ;
#91995 = CARTESIAN_POINT ( 'NONE',  ( 32.11957450231073352, 486.1307089099603331, 5.366351229209024076 ) ) ;
#91996 = CARTESIAN_POINT ( 'NONE',  ( 114.5290872765719570, -59.99999999999999289, 168.5341745518089738 ) ) ;
#91997 = CARTESIAN_POINT ( 'NONE',  ( -82.26374899041833544, -32.56066175956263464, 153.0468411736874259 ) ) ;
#91998 = AXIS2_PLACEMENT_3D ( 'NONE', #13904, #5823, #14432 ) ;
#91999 = EDGE_LOOP ( 'NONE', ( #62362, #22599, #97759, #81158 ) ) ;
#92000 = DIRECTION ( 'NONE',  ( -1.000000000000000000, -0.000000000000000000, -0.000000000000000000 ) ) ;
#92001 = CARTESIAN_POINT ( 'NONE',  ( -9.843481099141484947, 253.5920455615338653, -1.779148000612170488 ) ) ;
#92002 = PLANE ( 'NONE',  #81670 ) ;
#92003 = CIRCLE ( 'NONE', #14526, 10.00000000000000178 ) ;
#92004 = CARTESIAN_POINT ( 'NONE',  ( -6.293430271071535742, 5.026740376715093106, -0.4524126574264451528 ) ) ;
#92005 = CARTESIAN_POINT ( 'NONE',  ( 37.63246688678780316, 374.2349153975987406, 4.690254487569156083 ) ) ;
#92006 = CARTESIAN_POINT ( 'NONE',  ( 6.562974947121711367, -4.277474787035888681, 6.282829635893496523 ) ) ;
#92007 = EDGE_LOOP ( 'NONE', ( #95423, #82766, #105360, #66935 ) ) ;
#92008 = CARTESIAN_POINT ( 'NONE',  ( -19.73463816634110302, 304.7971333121958537, 8.925379062039136002 ) ) ;
#92009 = ORIENTED_EDGE ( 'NONE', *, *, #91599, .F. ) ;
#92010 = FILL_AREA_STYLE ('',( #84462 ) ) ;
#92011 = CARTESIAN_POINT ( 'NONE',  ( 0.000000000000000000, 15.00000000000000000, 10.00000000000000000 ) ) ;
#92012 = CARTESIAN_POINT ( 'NONE',  ( 32.62137895416793043, 486.7356100975906088, 7.182248123802368767 ) ) ;
#92013 = EDGE_CURVE ( 'NONE', #81048, #78409, #84146, .T. ) ;
#92014 = CARTESIAN_POINT ( 'NONE',  ( -5.371836670387280854, 41.43594048061098079, -58.48719196077191640 ) ) ;
#92015 = CARTESIAN_POINT ( 'NONE',  ( 6.031968554556502049, -14.91855978929650561, 14.31416968664684575 ) ) ;
#92016 = CARTESIAN_POINT ( 'NONE',  ( 46.00000000005143619, 436.1645721954917576, 9.605727516982005554 ) ) ;
#92017 = EDGE_LOOP ( 'NONE', ( #2248, #89299, #102951, #95990, #74147, #15088 ) ) ;
#92018 = CARTESIAN_POINT ( 'NONE',  ( 111.9602503973177647, -59.99999999999997868, 180.3351832281744578 ) ) ;
#92020 = CARTESIAN_POINT ( 'NONE',  ( 18.63452250350944084, -22.07072144282664183, 27.94029182146244494 ) ) ;
#92019 = CARTESIAN_POINT ( 'NONE',  ( -79.87726071770381964, -29.99999999999996092, 191.0765191543576407 ) ) ;
#92022 = CARTESIAN_POINT ( 'NONE',  ( -9.993576133260312108E-16, 61.49999999999999289, 8.160374191332742555 ) ) ;
#92021 = PRODUCT_DEFINITION_CONTEXT ( 'detailed design', #91391, 'design' ) ;
#92023 = FACE_OUTER_BOUND ( 'NONE', #60328, .T. ) ;
#92024 = CARTESIAN_POINT ( 'NONE',  ( -43.39865720172556962, -53.34764174391096958, 45.35594569590636382 ) ) ;
#92025 = EDGE_CURVE ( 'NONE', #63587, #91492, #63532, .T. ) ;
#92026 = CARTESIAN_POINT ( 'NONE',  ( -22.47385306462515331, 18.64284798593318371, -31.17447444075813223 ) ) ;
#92027 = UNCERTAINTY_MEASURE_WITH_UNIT (LENGTH_MEASURE( 1.000000000000000082E-05 ), #82656, 'distance_accuracy_value', 'NONE');
#92028 = VERTEX_POINT ( 'NONE', #66905 ) ;
#92029 = FACE_OUTER_BOUND ( 'NONE', #53986, .T. ) ;
#92030 = DIRECTION ( 'NONE',  ( 0.8191520442889974607, 1.003171929053531649E-16, -0.5735764363510380548 ) ) ;
#92031 = CARTESIAN_POINT ( 'NONE',  ( 31.00389226249483698, 502.9289871839745842, 8.047326149841639520 ) ) ;
#92032 =( LENGTH_UNIT ( ) NAMED_UNIT ( * ) SI_UNIT ( .MILLI., .METRE. ) );
#92033 = CARTESIAN_POINT ( 'NONE',  ( 27.99999999999999645, 0.000000000000000000, -11.00000000000000000 ) ) ;
#92034 = CARTESIAN_POINT ( 'NONE',  ( -33.52002750074903759, 462.9426806248537218, 5.597136840648579970 ) ) ;
#92035 = EDGE_LOOP ( 'NONE', ( #105275, #21510, #99673, #59832, #8741, #2803, #88169 ) ) ;
#92036 = CARTESIAN_POINT ( 'NONE',  ( -48.35517769068118099, -38.32756362620095558, 64.77550779848442630 ) ) ;
#92037 = ORIENTED_EDGE ( 'NONE', *, *, #85918, .T. ) ;
#92038 = CARTESIAN_POINT ( 'NONE',  ( 81.53245238598010758, -30.00000000000000000, -8.829371841663466114 ) ) ;
#92039 = CARTESIAN_POINT ( 'NONE',  ( 22.63965596209432718, 41.71073122692603619, -76.14257482519676046 ) ) ;
#92040 = AXIS2_PLACEMENT_3D ( 'NONE', #52156, #26347, #60289 ) ;
#92041 = CARTESIAN_POINT ( 'NONE',  ( 8.099999999999999645, -3.752776749732574135, -6.500000000000001776 ) ) ;
#92042 = CYLINDRICAL_SURFACE ( 'NONE', #53226, 8.000000000000000000 ) ;
#92043 = CARTESIAN_POINT ( 'NONE',  ( 80.76588975746719257, -30.00000000000000355, 10.92248678019670471 ) ) ;
#92044 = CARTESIAN_POINT ( 'NONE',  ( -29.60389654270521476, 319.5417381178118603, 13.79948592438576149 ) ) ;
#92045 = EDGE_CURVE ( 'NONE', #38530, #30487, #50682, .T. ) ;
#92046 = VERTEX_POINT ( 'NONE', #67959 ) ;
#92047 = AXIS2_PLACEMENT_3D ( 'NONE', #97920, #104020, #90908 ) ;
#92048 = VERTEX_POINT ( 'NONE', #82545 ) ;
#92049 = ORIENTED_EDGE ( 'NONE', *, *, #9325, .F. ) ;
#92050 = DIRECTION ( 'NONE',  ( 0.000000000000000000, 0.000000000000000000, 1.000000000000000000 ) ) ;
#92051 = DIRECTION ( 'NONE',  ( -1.000000000000000000, 0.000000000000000000, 0.000000000000000000 ) ) ;
#92052 = CARTESIAN_POINT ( 'NONE',  ( -37.02112216959907443, 25.93502769547995257, -11.07860630295547999 ) ) ;
#92053 = CARTESIAN_POINT ( 'NONE',  ( 6.692588830498425345, 3.932766476276028822, -6.892929031562515796 ) ) ;
#92054 = DIRECTION ( 'NONE',  ( 0.000000000000000000, 1.000000000000000000, 0.000000000000000000 ) ) ;
#92055 = ORIENTED_EDGE ( 'NONE', *, *, #72468, .F. ) ;
#92056 = ORIENTED_EDGE ( 'NONE', *, *, #54602, .F. ) ;
#92057 = CARTESIAN_POINT ( 'NONE',  ( 33.04853154822865235, 439.4047662902921729, 23.83380291423624797 ) ) ;
#92058 = CARTESIAN_POINT ( 'NONE',  ( 74.29104448979910558, -38.32825804840491202, 162.8965795265015402 ) ) ;
#92059 = CARTESIAN_POINT ( 'NONE',  ( 5.691929483231185749, 1.734723475976807094E-15, 6.500000000000001776 ) ) ;
#92060 = CARTESIAN_POINT ( 'NONE',  ( 32.73569771302867792, 300.2484905015194840, 3.150108463464334818 ) ) ;
#92061 = CARTESIAN_POINT ( 'NONE',  ( -5.093234209761986264, 247.5553222653508669, 3.176141468578064675 ) ) ;
#92062 = ORIENTED_EDGE ( 'NONE', *, *, #62421, .T. ) ;
#92063 = DIRECTION ( 'NONE',  ( 1.000000000000000000, 0.000000000000000000, 0.000000000000000000 ) ) ;
#92064 = CARTESIAN_POINT ( 'NONE',  ( 35.90484354297773706, 1.340359594676612611E-15, 0.000000000000000000 ) ) ;
#92065 = DIRECTION ( 'NONE',  ( 0.000000000000000000, 0.000000000000000000, 1.000000000000000000 ) ) ;
#92066 = ADVANCED_FACE ( 'NONE', ( #49639 ), #35089, .F. ) ;
#92067 = B_SPLINE_CURVE_WITH_KNOTS ( 'NONE', 3,
 ( #70199, #20651, #100967, #44337, #92872, #37341, #36288, #68631, #43794, #85880, #103106, #11950, #21167, #29256, #61060, #53994, #10876, #84795 ),
 .UNSPECIFIED., .F., .F.,
 ( 4, 2, 2, 2, 2, 2, 2, 2, 4 ),
 ( 0.003784215161170911314, 0.004287519624513744590, 0.004790824087856576999, 0.005042476319527991468, 0.005294128551199405938, 0.005797433014542233143, 0.006300737477885061215, 0.006804041941227888420, 0.007810650867913536757 ),
 .UNSPECIFIED. ) ;
#92068 = CARTESIAN_POINT ( 'NONE',  ( 15.50569080111995568, 2.636008032211578200, 0.8338155181783696301 ) ) ;
#92069 = ORIENTED_EDGE ( 'NONE', *, *, #22285, .F. ) ;
#92070 = CARTESIAN_POINT ( 'NONE',  ( -28.98553719038945431, 297.3123734288306537, 2.475459991885067712 ) ) ;
#92071 = CARTESIAN_POINT ( 'NONE',  ( 30.00000000000000000, 450.0000000000002274, 13.20242257375370976 ) ) ;
#92072 = FACE_OUTER_BOUND ( 'NONE', #79778, .T. ) ;
#92073 = EDGE_CURVE ( 'NONE', #4416, #76808, #102453, .T. ) ;
#92074 = DIRECTION ( 'NONE',  ( -0.000000000000000000, -1.000000000000000000, -0.000000000000000000 ) ) ;
#92075 = AXIS2_PLACEMENT_3D ( 'NONE', #67136, #25653, #100020 ) ;
#92076 = CYLINDRICAL_SURFACE ( 'NONE', #96653, 4.000000000000000000 ) ;
#92077 = AXIS2_PLACEMENT_3D ( 'NONE', #39614, #72487, #63363 ) ;
#92078 = CARTESIAN_POINT ( 'NONE',  ( 86.31765247549246567, -21.06018481759237559, 180.2375958646254901 ) ) ;
#92079 = COLOUR_RGB ( '', 0.09019608, 0.27058824, 0.51372549) ;
#92080 = FILL_AREA_STYLE ('',( #42465 ) ) ;
#92081 = CARTESIAN_POINT ( 'NONE',  ( -8.474746145506617978, 26.96279221873722776, 0.000000000000000000 ) ) ;
#92082 = VERTEX_POINT ( 'NONE', #85204 ) ;
#92083 = CARTESIAN_POINT ( 'NONE',  ( 90.46448577880153152, -57.66543568833093758, -21.68132792077462057 ) ) ;
#92084 = EDGE_CURVE ( 'NONE', #11414, #64162, #101686, .T. ) ;
#92085 = LINE ( 'NONE', #66215, #40052 ) ;
#92086 = CARTESIAN_POINT ( 'NONE',  ( 15.90780724146583580, 35.07994696358735354, -22.13120237605230045 ) ) ;
#92087 = CARTESIAN_POINT ( 'NONE',  ( 3.352941176470599860, -1.200583151104954061, 104.5794940929807524 ) ) ;
#92088 =( BOUNDED_SURFACE ( )  B_SPLINE_SURFACE ( 3, 2, ( 
 ( #583, #33548, #41091 ),
 ( #75029, #98777, #66419 ),
 ( #34100, #58883, #7637 ),
 ( #73973, #99304, #106331 ) ),
 .UNSPECIFIED., .F., .F., .F. ) 
 B_SPLINE_SURFACE_WITH_KNOTS ( ( 4, 4 ),
 ( 3, 3 ),
 ( 0.01401837328402458401, 0.01447126798403815945 ),
 ( 0.000000000000000000, 0.8297957905794470790 ),
 .UNSPECIFIED. ) 
 GEOMETRIC_REPRESENTATION_ITEM ( )  RATIONAL_B_SPLINE_SURFACE ( (
 ( 1.000000000000000000, 0.7688303398187896764, 0.9213079014936784716),
 ( 1.000000000000000000, 0.7649186838476292882, 0.9199763408694854316),
 ( 1.000000000000000000, 0.7609618042714275665, 0.9186293857494058912),
 ( 1.000000000000000000, 0.7569584399386413143, 0.9172666068268371387) ) ) 
 REPRESENTATION_ITEM ( '' )  SURFACE ( )  );
#92089 = CARTESIAN_POINT ( 'NONE',  ( -94.06182321730192086, -30.00000000000000000, 112.3371401795816240 ) ) ;
#92090 = CARTESIAN_POINT ( 'NONE',  ( 22.37422507490784795, 28.20471669103548606, -31.02961587878864336 ) ) ;
#92091 = PLANE ( 'NONE',  #106633 ) ;
#92093 = CARTESIAN_POINT ( 'NONE',  ( 7.000000000000000000, 0.000000000000000000, -1.175078176076019387 ) ) ;
#92092 = CARTESIAN_POINT ( 'NONE',  ( 34.99305553442271588, 490.1715275948229191, 12.08183789492280091 ) ) ;
#92094 = CARTESIAN_POINT ( 'NONE',  ( -39.23172258004870372, 39.86656256230372719, -53.99799038518022343 ) ) ;
#92095 = CARTESIAN_POINT ( 'NONE',  ( -29.35793203618277047, 13.99620286145419179, 42.06478814971824676 ) ) ;
#92096 = CARTESIAN_POINT ( 'NONE',  ( 42.42823000592811411, 488.6172904996860211, 9.782215989753083818 ) ) ;
#92097 = DIRECTION ( 'NONE',  ( 0.000000000000000000, 1.000000000000000000, 0.000000000000000000 ) ) ;
#92098 = CARTESIAN_POINT ( 'NONE',  ( -65.54168109996004432, -37.85200263902478923, -24.10684023409089605 ) ) ;
#92099 = DIRECTION ( 'NONE',  ( -0.000000000000000000, -0.000000000000000000, -1.000000000000000000 ) ) ;
#92100 = CARTESIAN_POINT ( 'NONE',  ( 56.97675734779401324, -28.82016638348090609, -25.97335252889095258 ) ) ;
#92101 = CARTESIAN_POINT ( 'NONE',  ( -24.15655977932474485, -18.60408373216753475, 28.02082033799254646 ) ) ;
#92102 = ORIENTED_EDGE ( 'NONE', *, *, #76810, .T. ) ;
#92103 = CARTESIAN_POINT ( 'NONE',  ( 6.012758288945200924, 11.20935548165501316, 3.586184577130256734 ) ) ;
#92104 =( LENGTH_UNIT ( ) NAMED_UNIT ( * ) SI_UNIT ( .MILLI., .METRE. ) );
#92105 = CARTESIAN_POINT ( 'NONE',  ( -7.934203308536660337, 81.13299659982199330, 1.057099537198550321 ) ) ;
#92106 = CARTESIAN_POINT ( 'NONE',  ( -67.63677907206896123, -29.90539320196331374, -21.89490774697042497 ) ) ;
#92107 = CIRCLE ( 'NONE', #52536, 4.000000000000000888 ) ;
#92108 = DIRECTION ( 'NONE',  ( -1.000000000000000000, -1.224606353822377258E-16, -0.000000000000000000 ) ) ;
#92109 = EDGE_CURVE ( 'NONE', #105782, #47418, #74104, .T. ) ;
#92110 = ORIENTED_EDGE ( 'NONE', *, *, #12136, .F. ) ;
#92111 = ORIENTED_EDGE ( 'NONE', *, *, #64252, .T. ) ;
#92112 = CARTESIAN_POINT ( 'NONE',  ( -36.64823341582351901, 437.5392299810053487, 4.281405873620232505 ) ) ;
#92113 = ORIENTED_EDGE ( 'NONE', *, *, #44345, .T. ) ;
#92114 = DIRECTION ( 'NONE',  ( 0.000000000000000000, 0.000000000000000000, -1.000000000000000000 ) ) ;
#92115 = EDGE_CURVE ( 'NONE', #27940, #72021, #92760, .T. ) ;
#92116 = CARTESIAN_POINT ( 'NONE',  ( 33.97359119245064818, 434.1099241184709285, 11.80501937577160732 ) ) ;
#92117 = CARTESIAN_POINT ( 'NONE',  ( -87.95683113949989718, -59.99999999999999289, -21.63131309512601419 ) ) ;
#92118 = ORIENTED_EDGE ( 'NONE', *, *, #23714, .T. ) ;
#92119 = SURFACE_STYLE_USAGE ( .BOTH. , #10661 ) ;
#92120 = CARTESIAN_POINT ( 'NONE',  ( -0.5741732275940398811, 294.8518027760915743, -9.999999999999998224 ) ) ;
#92121 = CARTESIAN_POINT ( 'NONE',  ( 100.7680253952265019, -52.74798219828765866, 193.5988501864534328 ) ) ;
#92123 = CARTESIAN_POINT ( 'NONE',  ( -7.413471587080150194, -7.356478408316738715, -3.013058070223549656 ) ) ;
#92122 = CARTESIAN_POINT ( 'NONE',  ( 68.70539558375507738, 6.856755485862130937E-15, 0.000000000000000000 ) ) ;
#92124 = EDGE_LOOP ( 'NONE', ( #25062, #49239, #62708, #88070 ) ) ;
#92125 = EDGE_LOOP ( 'NONE', ( #83810, #40178, #75339, #105889 ) ) ;
#92126 = EDGE_LOOP ( 'NONE', ( #44728, #9399, #67134, #11113 ) ) ;
#92127 = CARTESIAN_POINT ( 'NONE',  ( 32.14107381401169050, 425.0973432859777859, 24.99338633512491370 ) ) ;
#92128 = LINE ( 'NONE', #82983, #44053 ) ;
#92129 = DIRECTION ( 'NONE',  ( -1.000000000000000000, -0.000000000000000000, -0.000000000000000000 ) ) ;
#92130 = ORIENTED_EDGE ( 'NONE', *, *, #37586, .T. ) ;
#92131 = EDGE_CURVE ( 'NONE', #83331, #59135, #86294, .T. ) ;
#92132 = AXIS2_PLACEMENT_3D ( 'NONE', #78244, #86889, #62092 ) ;
#92133 = FACE_OUTER_BOUND ( 'NONE', #1411, .T. ) ;
#92134 = DIRECTION ( 'NONE',  ( 0.000000000000000000, -1.000000000000000000, 0.000000000000000000 ) ) ;
#92135 = CARTESIAN_POINT ( 'NONE',  ( -72.53004918620850106, -57.66488672193313647, 177.2532351053191348 ) ) ;
#92136 = DIRECTION ( 'NONE',  ( 0.000000000000000000, -1.000000000000000000, 0.000000000000000000 ) ) ;
#92137 = CARTESIAN_POINT ( 'NONE',  ( -31.21759734847655210, 387.2566916973277671, 24.99345285570965913 ) ) ;
#92138 = CARTESIAN_POINT ( 'NONE',  ( 38.83523057582821281, 469.0589752947456077, 0.4593318232150862546 ) ) ;
#92139 = VECTOR ( 'NONE', #20884, 1000.000000000000000 ) ;
#92140 = CARTESIAN_POINT ( 'NONE',  ( -87.68152309050471160, -14.21045842199426801, 32.26861779447729361 ) ) ;
#92141 = DIRECTION ( 'NONE',  ( 0.000000000000000000, -0.000000000000000000, 1.000000000000000000 ) ) ;
#92142 = CARTESIAN_POINT ( 'NONE',  ( -49.90681345140622938, -53.37058229338229154, 55.25435010867053620 ) ) ;
#92143 = DIRECTION ( 'NONE',  ( -1.000000000000000000, 0.000000000000000000, 0.000000000000000000 ) ) ;
#92144 = ORIENTED_EDGE ( 'NONE', *, *, #11892, .F. ) ;
#92145 = AXIS2_PLACEMENT_3D ( 'NONE', #56326, #39659, #56865 ) ;
#92146 = CARTESIAN_POINT ( 'NONE',  ( -95.20579108050159789, -45.25313649919430503, 194.1753725634821990 ) ) ;
#92147 = PRESENTATION_LAYER_ASSIGNMENT (  '', '', ( #21585 ) ) ;
#92148 = MECHANICAL_DESIGN_GEOMETRIC_PRESENTATION_REPRESENTATION (  '', ( #61222 ), #2604 ) ;
#92149 = DIRECTION ( 'NONE',  ( -0.5735764363510512664, 0.8191520442889881348, 1.003171929053520309E-16 ) ) ;
#92150 = CARTESIAN_POINT ( 'NONE',  ( 9.397785531853783070, -3.220433213403954831, 14.78444596218915130 ) ) ;
#92151 = ORIENTED_EDGE ( 'NONE', *, *, #5206, .T. ) ;
#92152 = CARTESIAN_POINT ( 'NONE',  ( 4.472135954999579610, 249.9999999999999716, -4.000000000000002665 ) ) ;
#92153 = CARTESIAN_POINT ( 'NONE',  ( 81.99224433430156012, -38.84286317575919867, 195.8945477241109927 ) ) ;
#92154 = DIRECTION ( 'NONE',  ( 0.000000000000000000, -1.000000000000000000, 0.000000000000000000 ) ) ;
#92155 = CARTESIAN_POINT ( 'NONE',  ( -6.400715382019204647, 51.30587535467638816, -7.878101082919672926 ) ) ;
#92156 = DIRECTION ( 'NONE',  ( 0.5735764363510491570, -0.8191520442889895781, 1.003171929053522035E-16 ) ) ;
#92157 = DIRECTION ( 'NONE',  ( -0.000000000000000000, 1.000000000000000000, -0.000000000000000000 ) ) ;
#92158 = CARTESIAN_POINT ( 'NONE',  ( 94.36600822773108632, -30.00000000000000711, 191.3092720282738242 ) ) ;
#92159 = CARTESIAN_POINT ( 'NONE',  ( -14.33580413386536812, 42.00000000000000000, -89.41414995615788541 ) ) ;
#92160 =( NAMED_UNIT ( * ) PLANE_ANGLE_UNIT ( ) SI_UNIT ( $, .RADIAN. ) );
#92161 = CARTESIAN_POINT ( 'NONE',  ( -0.1682998283258651528, 37.21016666119768246, 27.25000000000001421 ) ) ;
#92162 = EDGE_LOOP ( 'NONE', ( #8000, #100786 ) ) ;
#92163 = ORIENTED_EDGE ( 'NONE', *, *, #79519, .F. ) ;
#92164 = CARTESIAN_POINT ( 'NONE',  ( 53.40199480540213983, -39.50120367549543943, 56.96464640269142166 ) ) ;
#92165 = CARTESIAN_POINT ( 'NONE',  ( -46.00000000000000711, 435.9790741282528188, 14.35705232862668623 ) ) ;
#92166 = CARTESIAN_POINT ( 'NONE',  ( -7.500000000000007105, 40.00000000000000000, -58.69229087761261354 ) ) ;
#92167 = ORIENTED_EDGE ( 'NONE', *, *, #100922, .T. ) ;
#92168 = CARTESIAN_POINT ( 'NONE',  ( -88.09014624656468584, -38.37178535084554198, -19.45122215882188854 ) ) ;
#92169 = EDGE_LOOP ( 'NONE', ( #9944, #57989, #16810, #9132 ) ) ;
#92170 = CARTESIAN_POINT ( 'NONE',  ( 108.2573416289480406, -38.35772023760677740, 192.2552001511533888 ) ) ;
#92171 = CARTESIAN_POINT ( 'NONE',  ( 12.03416627641659353, 21.77447360072266846, -6.997134457414010633 ) ) ;
#92172 = CARTESIAN_POINT ( 'NONE',  ( 84.65144155607768539, -45.28281508045545678, 31.07819321620053188 ) ) ;
#92173 = CARTESIAN_POINT ( 'NONE',  ( 32.70807617001185008, 465.7746982375700782, 13.85399747858312836 ) ) ;
#92174 = CARTESIAN_POINT ( 'NONE',  ( -25.02938502635939244, 306.2014514788868382, -8.705669254435044024 ) ) ;
#92175 = CARTESIAN_POINT ( 'NONE',  ( 97.15356149169568312, -2.002967142162725287E-29, 5.000000000000011546 ) ) ;
#92176 = CARTESIAN_POINT ( 'NONE',  ( -24.20451479021888730, 25.63535626674006451, -31.17289312728862782 ) ) ;
#92177 = CIRCLE ( 'NONE', #81850, 1.000000000000000222 ) ;
#92178 = CARTESIAN_POINT ( 'NONE',  ( 70.41111111111112564, -3.309500000000000774, 4.475777889183797681E-16 ) ) ;
#92179 = ORIENTED_EDGE ( 'NONE', *, *, #11163, .F. ) ;
#92180 = CARTESIAN_POINT ( 'NONE',  ( 59.39647789081419660, -32.54350338366015194, 67.45545659301726005 ) ) ;
#92181 = DIRECTION ( 'NONE',  ( -1.000000000000000000, -1.224606353822377258E-16, -0.000000000000000000 ) ) ;
#92182 = EDGE_CURVE ( 'NONE', #40203, #60770, #12365, .T. ) ;
#92183 = CARTESIAN_POINT ( 'NONE',  ( 89.99999999999997158, -52.00000000000000000, 198.0238439516549818 ) ) ;
#92184 = ORIENTED_EDGE ( 'NONE', *, *, #66248, .F. ) ;
#92185 = CARTESIAN_POINT ( 'NONE',  ( -34.22920647855479359, 485.0586030974572509, -1.445294392290342733 ) ) ;
#92186 = CARTESIAN_POINT ( 'NONE',  ( -33.08708714024299979, 372.5548079963469377, 24.04571688234041815 ) ) ;
#92187 = FACE_OUTER_BOUND ( 'NONE', #21767, .T. ) ;
#92188 = CARTESIAN_POINT ( 'NONE',  ( 5.656854249492378806, -27.68749999999999645, 5.656854249492381470 ) ) ;
#92189 = CARTESIAN_POINT ( 'NONE',  ( -41.85571157551820676, -27.12375206088530533, 37.13791425116489364 ) ) ;
#92190 = ADVANCED_FACE ( 'NONE', ( #19988 ), #81037, .T. ) ;
#92191 = CARTESIAN_POINT ( 'NONE',  ( 65.03872891708842019, 6.856755485862130937E-15, 0.000000000000000000 ) ) ;
#92192 = ORIENTED_EDGE ( 'NONE', *, *, #65258, .T. ) ;
#92193 = CARTESIAN_POINT ( 'NONE',  ( 81.59403609548893144, -60.63023761752385354, 186.3572134667889770 ) ) ;
#92194 = CARTESIAN_POINT ( 'NONE',  ( 7.500000000000001776, 0.000000000000000000, 0.000000000000000000 ) ) ;
#92195 = AXIS2_PLACEMENT_3D ( 'NONE', #90368, #41282, #16481 ) ;
#92196 = CYLINDRICAL_SURFACE ( 'NONE', #86614, 4.000000000000000888 ) ;
#92197 = VERTEX_POINT ( 'NONE', #2679 ) ;
#92198 = CARTESIAN_POINT ( 'NONE',  ( 1.288479777019286136E-15, 37.86482112153537116, 10.52123582012687919 ) ) ;
#92199 = EDGE_CURVE ( 'NONE', #3128, #65549, #20827, .T. ) ;
#92200 = CARTESIAN_POINT ( 'NONE',  ( 43.26971690803010517, 435.9072580013536822, 8.039630127099059109 ) ) ;
#92201 = CARTESIAN_POINT ( 'NONE',  ( 1.347801180098172180, -3.000000000000003109, -100.0000000000007105 ) ) ;
#92202 = CARTESIAN_POINT ( 'NONE',  ( -18.51720514346013502, -25.29809392112008481, -38.50248889867572899 ) ) ;
#92203 = MECHANICAL_DESIGN_GEOMETRIC_PRESENTATION_REPRESENTATION (  '', ( #9518 ), #50848 ) ;
#92204 = CARTESIAN_POINT ( 'NONE',  ( 47.62749844892509543, -59.99999999999999289, 66.18161539844986407 ) ) ;
#92205 = CARTESIAN_POINT ( 'NONE',  ( 6.928203230275505220, 105.2688332450899935, -4.000000000000002665 ) ) ;
#92207 = CARTESIAN_POINT ( 'NONE',  ( -13.14907386255262445, 23.97079872446213855, 3.796718886851553343 ) ) ;
#92206 = CARTESIAN_POINT ( 'NONE',  ( -27.49835752312068848, -30.75254570659940256, 39.28988535020603479 ) ) ;
#92208 =( GEOMETRIC_REPRESENTATION_CONTEXT ( 3 ) GLOBAL_UNCERTAINTY_ASSIGNED_CONTEXT ( ( #76767 ) ) GLOBAL_UNIT_ASSIGNED_CONTEXT ( ( #12915, #53401, #37780 ) ) REPRESENTATION_CONTEXT ( 'NONE', 'WORKASPACE' ) );
#92209 = DIRECTION ( 'NONE',  ( 0.5735764363510462704, 0.8191520442889915765, 0.000000000000000000 ) ) ;
#92210 = FACE_OUTER_BOUND ( 'NONE', #4120, .T. ) ;
#92211 = AXIS2_PLACEMENT_3D ( 'NONE', #49844, #82750, #8852 ) ;
#92212 = CONICAL_SURFACE ( 'NONE', #23356, 3.309500000000001663, 0.9599310885968770357 ) ;
#92213 = CARTESIAN_POINT ( 'NONE',  ( 4.551587301587304957, -1.200583151104947843, 104.4018401814738155 ) ) ;
#92214 = AXIS2_PLACEMENT_3D ( 'NONE', #13579, #79911, #6547 ) ;
#92215 = ORIENTED_EDGE ( 'NONE', *, *, #70856, .T. ) ;
#92216 = CARTESIAN_POINT ( 'NONE',  ( -8.559508646656370345, -1.200000000000000030E-05, 1.531152949374564365 ) ) ;
#92217 = CONICAL_SURFACE ( 'NONE', #105999, 3.309500000000001663, 0.9599310885968770357 ) ;
#92218 = CARTESIAN_POINT ( 'NONE',  ( -17.49999999999995737, 51.99999999999994316, 59.82664205501144039 ) ) ;
#92219 = AXIS2_PLACEMENT_3D ( 'NONE', #99355, #76159, #59476 ) ;
#92220 = CARTESIAN_POINT ( 'NONE',  ( -40.05599234025955013, 464.9362105862702492, 17.76115130056741265 ) ) ;
#92222 = CARTESIAN_POINT ( 'NONE',  ( 22.67313198859957168, -60.22830976074993714, -35.89781762293466016 ) ) ;
#92221 = CARTESIAN_POINT ( 'NONE',  ( 5.523799489093670250E-15, 23.58303312036771615, 45.10524579772351217 ) ) ;
#92223 = EDGE_CURVE ( 'NONE', #2515, #86973, #3228, .T. ) ;
#92224 = ORIENTED_EDGE ( 'NONE', *, *, #54946, .T. ) ;
#92225 = CARTESIAN_POINT ( 'NONE',  ( 27.71645771920791645, 36.65781692560624805, 7.705275282087030497 ) ) ;
#92226 = CARTESIAN_POINT ( 'NONE',  ( -1.000000000001115108, -69.90918681875037066, 12.94764124286841067 ) ) ;
#92227 = VERTEX_POINT ( 'NONE', #93833 ) ;
#92228 = ADVANCED_FACE ( 'NONE', ( #102987 ), #70817, .T. ) ;
#92229 = FACE_OUTER_BOUND ( 'NONE', #62964, .T. ) ;
#92230 = ADVANCED_FACE ( 'NONE', ( #52294 ), #45346, .F. ) ;
#92231 = DIRECTION ( 'NONE',  ( -1.000000000000000000, -1.224606353822377258E-16, -0.000000000000000000 ) ) ;
#92232 = CARTESIAN_POINT ( 'NONE',  ( -104.6395680266647332, -59.99999999999999289, 108.2291619832981695 ) ) ;
#92233 = CARTESIAN_POINT ( 'NONE',  ( -1.469576158976823947E-15, -24.87499999999999289, 8.000000000000000000 ) ) ;
#92234 = CARTESIAN_POINT ( 'NONE',  ( 0.000000000000000000, 0.000000000000000000, 0.000000000000000000 ) ) ;
#92235 = CARTESIAN_POINT ( 'NONE',  ( 31.21933008645656926, 405.2090764464551853, 25.56980379099173817 ) ) ;
#92236 = CARTESIAN_POINT ( 'NONE',  ( 40.42601080768203303, 460.8348341399792503, 2.184598410783125111 ) ) ;
#92238 = CARTESIAN_POINT ( 'NONE',  ( -15.05785784214673129, 3.824195276770050445, -4.604276673498571171 ) ) ;
#92237 = CARTESIAN_POINT ( 'NONE',  ( 5.036189802310915731, -3.000000000000002665, -93.73786388412167980 ) ) ;
#92239 = CARTESIAN_POINT ( 'NONE',  ( -82.93997213326217377, -42.97867824148965354, 174.7049767036717185 ) ) ;
#92240 = ORIENTED_EDGE ( 'NONE', *, *, #44725, .T. ) ;
#92241 = ORIENTED_EDGE ( 'NONE', *, *, #81449, .F. ) ;
#92242 = MECHANICAL_DESIGN_GEOMETRIC_PRESENTATION_REPRESENTATION (  '', ( #81927 ), #80239 ) ;
#92243 = ORIENTED_EDGE ( 'NONE', *, *, #12978, .F. ) ;
#92245 = ADVANCED_FACE ( 'NONE', ( #33850 ), #15701, .T. ) ;
#92244 = DIRECTION ( 'NONE',  ( -1.000000000000000000, -1.224606353822377258E-16, -0.000000000000000000 ) ) ;
#92246 = CARTESIAN_POINT ( 'NONE',  ( 0.4037800551813745531, 7.199367570657607018, 0.5303295852573142177 ) ) ;
#92247 = ORIENTED_EDGE ( 'NONE', *, *, #91283, .F. ) ;
#92248 = EDGE_CURVE ( 'NONE', #42289, #84434, #34341, .T. ) ;
#92249 = CARTESIAN_POINT ( 'NONE',  ( 0.000000000000000000, 0.000000000000000000, 0.000000000000000000 ) ) ;
#92250 = CARTESIAN_POINT ( 'NONE',  ( 13.37207953394533355, 1.482358050883964840E-15, 0.000000000000000000 ) ) ;
#92251 = CARTESIAN_POINT ( 'NONE',  ( -6.818272094961328023, -1.321852500971161248, -6.208027553811809263 ) ) ;
#92252 = CARTESIAN_POINT ( 'NONE',  ( -7.413471587080153746, -62.35647840831676092, -3.013058070223552765 ) ) ;
#92253 = CARTESIAN_POINT ( 'NONE',  ( -0.1694193870205596697, 54.30391592751540486, 7.758667673557112288 ) ) ;
#92254 = CARTESIAN_POINT ( 'NONE',  ( 0.000000000000000000, 43.34115912517999902, 0.000000000000000000 ) ) ;
#92255 = CARTESIAN_POINT ( 'NONE',  ( -5.000000000000000000, -13.99331560178746869, 11.59713945945469504 ) ) ;
#92256 = CARTESIAN_POINT ( 'NONE',  ( 89.21217950020245269, -30.00000000000004974, 13.74488734703711934 ) ) ;
#92257 = EDGE_CURVE ( 'NONE', #35979, #54576, #40796, .T. ) ;
#92258 = CARTESIAN_POINT ( 'NONE',  ( -73.20331151331558317, -59.99999999999998579, 185.6225630369678470 ) ) ;
#92259 = CARTESIAN_POINT ( 'NONE',  ( -59.90188342519598308, -49.91569465878361456, 76.94345777252618745 ) ) ;
#92260 = VERTEX_POINT ( 'NONE', #91497 ) ;
#92261 = CARTESIAN_POINT ( 'NONE',  ( 6.770001855160700188, 16.58332918785157872, 1.796682604554741935 ) ) ;
#92262 = CARTESIAN_POINT ( 'NONE',  ( 87.20415626912121354, -59.99999999999998579, -25.76356015432472901 ) ) ;
#92263 = ORIENTED_EDGE ( 'NONE', *, *, #65093, .T. ) ;
#92264 = CARTESIAN_POINT ( 'NONE',  ( 7.005973654531714168, -22.06726470602710677, 27.55784255609015077 ) ) ;
#92265 = CARTESIAN_POINT ( 'NONE',  ( -101.5318813598352676, -45.26482616480781473, 190.2983095272828962 ) ) ;
#92266 = DIRECTION ( 'NONE',  ( -1.000000000000000000, -0.000000000000000000, -0.000000000000000000 ) ) ;
#92267 = ADVANCED_FACE ( 'NONE', ( #98494 ), #1881, .F. ) ;
#92268 = CYLINDRICAL_SURFACE ( 'NONE', #77008, 10.00000000000000178 ) ;
#92269 = CARTESIAN_POINT ( 'NONE',  ( -16.14595037822616419, 20.23371447306202597, -4.922994507635920947 ) ) ;
#92270 = ORIENTED_EDGE ( 'NONE', *, *, #74158, .T. ) ;
#92271 = CARTESIAN_POINT ( 'NONE',  ( 19.47704209976909695, 49.99346651654762042, 60.32563227602115319 ) ) ;
#92272 = CIRCLE ( 'NONE', #52703, 4.000000000000001776 ) ;
#92273 = CARTESIAN_POINT ( 'NONE',  ( -80.72759035304791553, -59.99999999999998579, 196.8484650859923875 ) ) ;
#92274 = CARTESIAN_POINT ( 'NONE',  ( 36.94571008616465235, 25.95814344041297517, -11.10931082871520026 ) ) ;
#92275 = CARTESIAN_POINT ( 'NONE',  ( 5.082755093536325930, -20.84375000204838813, -5.082755093536325042 ) ) ;
#92276 = CARTESIAN_POINT ( 'NONE',  ( -1.218835986930302706, 36.86216219021419960, -28.17983935174571641 ) ) ;
#92277 = CARTESIAN_POINT ( 'NONE',  ( 11.24494283604391498, -0.000000000000000000, -12.81923949848203570 ) ) ;
#92278 = CARTESIAN_POINT ( 'NONE',  ( -24.93816302196866275, 307.4233949143036284, 10.52291764336465008 ) ) ;
#92279 = CARTESIAN_POINT ( 'NONE',  ( 6.227327457448970094, -7.358135131406661422, 13.83618408075120776 ) ) ;
#92280 = FACE_OUTER_BOUND ( 'NONE', #21968, .T. ) ;
#92281 = AXIS2_PLACEMENT_3D ( 'NONE', #82377, #8485, #33323 ) ;
#92282 = CARTESIAN_POINT ( 'NONE',  ( -7.500000000000002665, 9.462792962020666110, -29.31754814678773968 ) ) ;
#92283 = UNCERTAINTY_MEASURE_WITH_UNIT (LENGTH_MEASURE( 1.000000000000000082E-05 ), #148, 'distance_accuracy_value', 'NONE');
#92284 = CARTESIAN_POINT ( 'NONE',  ( -29.88958479793361889, -29.06775393404062058, 31.22462154783213961 ) ) ;
#92285 = CARTESIAN_POINT ( 'NONE',  ( 4.000000000000001776, 18.12398157863135850, 5.744562646538044604 ) ) ;
#92286 = CARTESIAN_POINT ( 'NONE',  ( 42.62262948205808044, -25.70207388102151569, 37.69155540254526215 ) ) ;
#92287 = PRESENTATION_LAYER_ASSIGNMENT (  '', '', ( #35449 ) ) ;
#92288 = CARTESIAN_POINT ( 'NONE',  ( 3.313708498984685225, -13.71874999999998934, -8.000000000000076383 ) ) ;
#92289 = ORIENTED_EDGE ( 'NONE', *, *, #13613, .T. ) ;
#92290 = CARTESIAN_POINT ( 'NONE',  ( -0.8415904055670518913, 45.41420510540432787, 18.42786602808935470 ) ) ;
#92291 = CARTESIAN_POINT ( 'NONE',  ( -80.10895284081995271, -38.78997264253702326, 193.1831740812525595 ) ) ;
#92292 = ORIENTED_EDGE ( 'NONE', *, *, #53875, .T. ) ;
#92294 = FACE_OUTER_BOUND ( 'NONE', #106620, .T. ) ;
#92293 = CARTESIAN_POINT ( 'NONE',  ( -16.11155731265022339, 21.67754735132975696, -1.749455090966761439 ) ) ;
#92295 = CARTESIAN_POINT ( 'NONE',  ( 49.17729069842651768, -59.99999999999997868, 56.10385161243137020 ) ) ;
#92296 = DIRECTION ( 'NONE',  ( -1.000000000000000000, 0.000000000000000000, 0.000000000000000000 ) ) ;
#92297 = CARTESIAN_POINT ( 'NONE',  ( -7.268970507964822581, 41.22981623788603400, -58.87267832762033493 ) ) ;
#92298 = CIRCLE ( 'NONE', #66511, 4.250000000000000000 ) ;
#92299 = AXIS2_PLACEMENT_3D ( 'NONE', #48352, #65078, #97976 ) ;
#92300 = CARTESIAN_POINT ( 'NONE',  ( 9.607634652977997902, 15.83450757143046950, -2.797224791467303628 ) ) ;
#92301 = DIRECTION ( 'NONE',  ( 1.000000000000000000, 1.224606353822377258E-16, 0.000000000000000000 ) ) ;
#92302 = CONICAL_SURFACE ( 'NONE', #88927, 4.172000000000001485, 0.9599310885968750373 ) ;
#92303 = FACE_OUTER_BOUND ( 'NONE', #78850, .T. ) ;
#92304 = DIRECTION ( 'NONE',  ( -1.000000000000000000, -1.224606353822377258E-16, -0.000000000000000000 ) ) ;
#92305 = CARTESIAN_POINT ( 'NONE',  ( 102.1815710810213318, -60.00000000000000000, 93.80444312277987251 ) ) ;
#92306 = CARTESIAN_POINT ( 'NONE',  ( 6.445370176742116541, -4.584736124524379619, 5.738941594274989733 ) ) ;
#92307 = CONICAL_SURFACE ( 'NONE', #44128, 4.000000000000001776, 0.9599310885968808105 ) ;
#92308 = B_SPLINE_CURVE_WITH_KNOTS ( 'NONE', 3,
 ( #18851, #1538, #59281, #98647 ),
 .UNSPECIFIED., .F., .F.,
 ( 4, 4 ),
 ( 0.000000000000000000, 1.000000000000000000 ),
 .UNSPECIFIED. ) ;
#92309 = CARTESIAN_POINT ( 'NONE',  ( 14.83349330513380693, 1.593028355512270962E-15, 0.000000000000000000 ) ) ;
#92310 = VERTEX_POINT ( 'NONE', #8954 ) ;
#92311 = CARTESIAN_POINT ( 'NONE',  ( 34.62919541716566840, 437.4394979580218319, 4.999019296794181777 ) ) ;
#92312 = EDGE_CURVE ( 'NONE', #79135, #55161, #15670, .T. ) ;
#92313 = CARTESIAN_POINT ( 'NONE',  ( -96.54523544995177531, -29.99999999999999645, 127.4433644037409294 ) ) ;
#92314 = ORIENTED_EDGE ( 'NONE', *, *, #77802, .T. ) ;
#92315 = CARTESIAN_POINT ( 'NONE',  ( 0.000000000000000000, 6.123233995736770227E-16, -5.000000000000002665 ) ) ;
#92316 =( LENGTH_UNIT ( ) NAMED_UNIT ( * ) SI_UNIT ( .MILLI., .METRE. ) );
#92317 = CARTESIAN_POINT ( 'NONE',  ( 28.84740160328638225, 315.3509136110029658, 12.74594617175954703 ) ) ;
#92318 = AXIS2_PLACEMENT_3D ( 'NONE', #60914, #36138, #77078 ) ;
#92319 = CARTESIAN_POINT ( 'NONE',  ( 0.000000000000000000, -30.00000000000000000, 8.000000000000000000 ) ) ;
#92320 = CARTESIAN_POINT ( 'NONE',  ( -2.977408999572650039, -17.56250000204838813, -7.188101187500001821 ) ) ;
#92321 = CARTESIAN_POINT ( 'NONE',  ( 30.00000000000000000, 461.8802764867031669, 14.89328939272360053 ) ) ;
#92322 = ADVANCED_FACE ( 'NONE', ( #828, #33797, #102231, #26790, #19774 ), #10514, .F. ) ;
#92323 = ADVANCED_FACE ( 'NONE', ( #43470 ), #24336, .T. ) ;
#92324 = B_SPLINE_CURVE_WITH_KNOTS ( 'NONE', 3,
 ( #390, #59217, #18236, #92095, #40896, #99658, #65708, #25272, #17695, #74314, #82417, #81332, #82949, #73780, #66225, #106681, #24213, #40358, #17168, #33897, #90507, #65167, #66770, #81859, #32828, #9044, #33357, #98062, #91586, #1477 ),
 .UNSPECIFIED., .F., .F.,
 ( 4, 2, 2, 2, 2, 2, 2, 2, 2, 2, 2, 2, 2, 2, 4 ),
 ( 0.0006904739626665865699, 0.001153765004792748619, 0.001617056046918910776, 0.002543638131171222297, 0.003470220215423534468, 0.004396802299675845772, 0.005323384383928157944, 0.005786675426054318366, 0.006249966468180478789, 0.006713257510306639211, 0.006944903031369712050, 0.007176548552432786623, 0.007408194073495859462, 0.007639839594558934036, 0.008103130636685088387 ),
 .UNSPECIFIED. ) ;
#92325 = CARTESIAN_POINT ( 'NONE',  ( 30.82780881727078182, 15.25261229662383933, -40.33825946679404240 ) ) ;
#92327 = ORIENTED_EDGE ( 'NONE', *, *, #19855, .T. ) ;
#92326 = FILL_AREA_STYLE_COLOUR ( '', #34033 ) ;
#92328 = CARTESIAN_POINT ( 'NONE',  ( 83.21183222637840515, -29.08118594051771311, 155.6702613005863611 ) ) ;
#92329 = ADVANCED_FACE ( 'NONE', ( #36484 ), #48772, .F. ) ;
#92330 = LINE ( 'NONE', #19566, #42838 ) ;
#92331 = VERTEX_POINT ( 'NONE', #84990 ) ;
#92332 = CARTESIAN_POINT ( 'NONE',  ( 82.70911704725124025, 6.123233995736582872E-16, -5.000000000000011546 ) ) ;
#92333 = ADVANCED_FACE ( 'NONE', ( #11073 ), #27866, .T. ) ;
#92335 = ADVANCED_FACE ( 'NONE', ( #1923 ), #85533, .T. ) ;
#92334 = DIRECTION ( 'NONE',  ( 0.2271661929662003865, 0.3956501727921482581, 0.8898631701238041147 ) ) ;
#92336 = CARTESIAN_POINT ( 'NONE',  ( 4.678819457397437986, 8.078722181090837395, 0.000000000000000000 ) ) ;
#92337 = CARTESIAN_POINT ( 'NONE',  ( 5.947762761376480078, -6.880090707843049991, -1.083333333333332593 ) ) ;
#92338 = CIRCLE ( 'NONE', #47598, 10.00000000000000000 ) ;
#92339 = CARTESIAN_POINT ( 'NONE',  ( -31.33955551928141503, 325.4742652106692731, 15.49549166411432921 ) ) ;
#92340 = CARTESIAN_POINT ( 'NONE',  ( 9.045527390509329635, -0.3367924543029778839, 19.71820488350171274 ) ) ;
#92341 = ORIENTED_EDGE ( 'NONE', *, *, #4977, .T. ) ;
#92342 = CARTESIAN_POINT ( 'NONE',  ( -6.499999999999999112, -1.280811194704867262, -0.07768058122908140517 ) ) ;
#92343 = CARTESIAN_POINT ( 'NONE',  ( 86.71928054816494580, -53.76640798283146694, 192.6448558597238048 ) ) ;
#92344 = DIRECTION ( 'NONE',  ( -1.000000000000000000, -0.000000000000000000, -0.000000000000000000 ) ) ;
#92345 = CARTESIAN_POINT ( 'NONE',  ( -2.977408999572650039, -23.18750000204838813, -7.188101187500001821 ) ) ;
#92346 = CYLINDRICAL_SURFACE ( 'NONE', #44002, 3.400000000000000355 ) ;
#92347 = CARTESIAN_POINT ( 'NONE',  ( 2.690931834596300476, -5.951943280390056934, -1.764030815951805255E-14 ) ) ;
#92348 = CARTESIAN_POINT ( 'NONE',  ( -7.808218555862453059, -4.508077085119343685, -7.999534413642745534 ) ) ;
#92349 = VECTOR ( 'NONE', #79072, 1000.000000000000114 ) ;
#92350 = ORIENTED_EDGE ( 'NONE', *, *, #68390, .T. ) ;
#92351 = CARTESIAN_POINT ( 'NONE',  ( 1.250539423207229994, 43.55815149200913083, 17.65460189445720474 ) ) ;
#92352 = CARTESIAN_POINT ( 'NONE',  ( -10.00000000000000355, 30.00000000000000000, -4.000000000000000000 ) ) ;
#92353 = CARTESIAN_POINT ( 'NONE',  ( -5.912155184616126213, 4.620813446856026019, -4.999999999999999112 ) ) ;
#92354 = DIRECTION ( 'NONE',  ( -1.000000000000000000, -1.224606353822377258E-16, -0.000000000000000000 ) ) ;
#92355 = CONICAL_SURFACE ( 'NONE', #61364, 4.000000000000001776, 0.9599310885968808105 ) ;
#92356 = ADVANCED_BREP_SHAPE_REPRESENTATION ( '', ( #17340, #10728 ), #3983 ) ;
#92357 = ORIENTED_EDGE ( 'NONE', *, *, #4714, .T. ) ;
#92358 = CARTESIAN_POINT ( 'NONE',  ( -32.02667885475513998, 464.8582969030198910, 12.88960884979827348 ) ) ;
#92359 = CARTESIAN_POINT ( 'NONE',  ( -43.10371592039376054, 462.6168321841617512, 4.970041475410676313 ) ) ;
#92360 = CIRCLE ( 'NONE', #83990, 5.000000000000010658 ) ;
#92361 = EDGE_LOOP ( 'NONE', ( #36466, #70953, #39096, #80625 ) ) ;
#92362 = ADVANCED_FACE ( 'NONE', ( #104341 ), #87655, .F. ) ;
#92363 = CARTESIAN_POINT ( 'NONE',  ( 31.73464696827581122, 436.7284713362857360, 21.10242107247917787 ) ) ;
#92364 = PRESENTATION_STYLE_ASSIGNMENT (( #9848 ) ) ;
#92365 = CARTESIAN_POINT ( 'NONE',  ( 24.83349330513380337, -4.000000000000000000, 4.898587196589415787E-16 ) ) ;
#92366 = CIRCLE ( 'NONE', #66508, 46.61112130868859538 ) ;
#92367 = CARTESIAN_POINT ( 'NONE',  ( 13.50000000000000355, 7.794228634059934713, -13.00000000000000000 ) ) ;
#92368 = CARTESIAN_POINT ( 'NONE',  ( -89.32677887001227646, -60.00000000000000000, 201.7918933705177551 ) ) ;
#92369 = CIRCLE ( 'NONE', #80279, 13.27631144943088515 ) ;
#92370 = CIRCLE ( 'NONE', #25277, 15.00000000000000178 ) ;
#92371 = AXIS2_PLACEMENT_3D ( 'NONE', #58307, #57226, #82035 ) ;
#92372 = CARTESIAN_POINT ( 'NONE',  ( 9.176927881262047393, 44.04115577556814287, -13.55866590325632970 ) ) ;
#92373 = DIRECTION ( 'NONE',  ( 0.000000000000000000, 0.000000000000000000, 1.000000000000000000 ) ) ;
#92374 = CARTESIAN_POINT ( 'NONE',  ( -84.53343285826699116, -42.97347055893645518, 184.1442894847539264 ) ) ;
#92375 = CYLINDRICAL_SURFACE ( 'NONE', #50424, 1.250000000000001110 ) ;
#92376 = AXIS2_PLACEMENT_3D ( 'NONE', #3885, #97642, #72324 ) ;
#92377 =( BOUNDED_SURFACE ( )  B_SPLINE_SURFACE ( 3, 2, ( 
 ( #93052, #92508, #18663 ),
 ( #52046, #47669, #88154 ),
 ( #71960, #102740, #70901 ),
 ( #70376, #22384, #28901 ),
 ( #39079, #38040, #69843 ),
 ( #36975, #55744, #96259 ),
 ( #6148, #63887, #54692 ),
 ( #104863, #20816, #87626 ),
 ( #29421, #103791, #47142 ),
 ( #104316, #103271, #61774 ),
 ( #21321, #5109, #53650 ),
 ( #31005, #86581, #4576 ),
 ( #45576, #13175, #12645 ),
 ( #30466, #55229, #96777 ),
 ( #22907, #29934, #14236 ),
 ( #80035, #37513, #88678 ),
 ( #14767, #80564, #94671 ),
 ( #78455, #62298, #63360 ),
 ( #95190, #13710, #62819 ),
 ( #54157, #95712, #87099 ),
 ( #21851, #46102, #78985 ),
 ( #46620, #79517, #5630 ),
 ( #38551, #71415, #89212 ),
 ( #15310, #48198, #98354 ),
 ( #97284, #33638, #23981 ),
 ( #40121, #7212, #64412 ),
 ( #81611, #48722, #49257 ),
 ( #73529, #72997, #8273 ),
 ( #57879, #90804, #25575 ),
 ( #7737, #105390, #24509 ),
 ( #81099, #98862, #105901 ),
 ( #49797, #89745, #72483 ),
 ( #41186, #106432, #152 ),
 ( #90265, #40647, #32590 ),
 ( #64931, #65462, #32052 ),
 ( #74597, #16921, #82701 ),
 ( #58433, #91342, #97816 ),
 ( #33119, #57344, #17457 ),
 ( #674, #8806, #41714 ),
 ( #50322, #66518, #16367 ),
 ( #6684, #99391, #39610 ),
 ( #56822, #31531, #82160 ),
 ( #15840, #74063, #23437 ),
 ( #56274, #65987, #25024 ) ),
 .UNSPECIFIED., .F., .F., .T. ) 
 B_SPLINE_SURFACE_WITH_KNOTS ( ( 4, 2, 2, 2, 2, 2, 2, 2, 2, 2, 2, 2, 2, 2, 2, 2, 2, 2, 2, 2, 2, 4 ),
 ( 3, 3 ),
 ( 0.05246299049208403426, 0.07033874506154716433, 0.08821449963101030134, 0.1060902542004734384, 0.1150281314852049930, 0.1239660087699365615, 0.1418417633393996846, 0.1597175179088628216, 0.1686553951935944040, 0.1731243338359601813, 0.1753588031571430839, 0.1775932724783259586, 0.1820622111206917360, 0.1831794457812832011, 0.1842966804418746385, 0.1865311497630575133, 0.1876483844236489507, 0.1887656190842404158, 0.1898828537448318809, 0.1910000884054233183, 0.1932345577266061931, 0.1954690270477890957 ),
 ( 0.000000000000000000, 1.000000000000000000 ),
 .UNSPECIFIED. ) 
 GEOMETRIC_REPRESENTATION_ITEM ( )  RATIONAL_B_SPLINE_SURFACE ( (
 ( 1.000000000000000000, 0.7071066982776790244, 1.000000000000000000),
 ( 1.000000000000000000, 0.7071066246860953086, 1.000000000000000000),
 ( 1.000000000000000000, 0.7071067817483319695, 1.000000000000000000),
 ( 1.000000000000000000, 0.7071067817483319695, 1.000000000000000000),
 ( 1.000000000000000000, 0.7071067820003403837, 1.000000000000000000),
 ( 1.000000000000000000, 0.7071067820003403837, 1.000000000000000000),
 ( 1.000000000000000000, 0.7071085911072407804, 1.000000000000000000),
 ( 1.000000000000000000, 0.7071090165955132845, 1.000000000000000000),
 ( 1.000000000000000000, 0.7071082982937503258, 1.000000000000000000),
 ( 1.000000000000000000, 0.7071068030320751818, 1.000000000000000000),
 ( 1.000000000000000000, 0.7071066538725350181, 1.000000000000000000),
 ( 1.000000000000000000, 0.7071092477002908216, 1.000000000000000000),
 ( 1.000000000000000000, 0.7071091921374882405, 1.000000000000000000),
 ( 1.000000000000000000, 0.7071056146855209112, 1.000000000000000000),
 ( 1.000000000000000000, 0.7070854685221523717, 1.000000000000000000),
 ( 1.000000000000000000, 0.7071229475123441688, 1.000000000000000000),
 ( 1.000000000000000000, 0.7071321772062534317, 1.000000000000000000),
 ( 1.000000000000000000, 0.7071076013889080469, 1.000000000000000000),
 ( 1.000000000000000000, 0.7071078047556201840, 1.000000000000000000),
 ( 1.000000000000000000, 0.7071116805962889273, 1.000000000000000000),
 ( 1.000000000000000000, 0.7071114737089826408, 1.000000000000000000),
 ( 1.000000000000000000, 0.7071088341742440830, 1.000000000000000000),
 ( 1.000000000000000000, 0.7071030604351956628, 1.000000000000000000),
 ( 1.000000000000000000, 0.7071149245157897223, 1.000000000000000000),
 ( 1.000000000000000000, 0.7072266118915774280, 1.000000000000000000),
 ( 1.000000000000000000, 0.7071506248185068788, 1.000000000000000000),
 ( 1.000000000000000000, 0.7071307950262011310, 1.000000000000000000),
 ( 1.000000000000000000, 0.7071052445289376376, 1.000000000000000000),
 ( 1.000000000000000000, 0.7071065825907152380, 1.000000000000000000),
 ( 1.000000000000000000, 0.7071121758606627727, 1.000000000000000000),
 ( 1.000000000000000000, 0.7071099217218235200, 1.000000000000000000),
 ( 1.000000000000000000, 0.7071058422322067383, 1.000000000000000000),
 ( 1.000000000000000000, 0.7071037979643884919, 1.000000000000000000),
 ( 1.000000000000000000, 0.7070993061526186230, 1.000000000000000000),
 ( 1.000000000000000000, 0.7070996420988305831, 1.000000000000000000),
 ( 1.000000000000000000, 0.7071045601661539726, 1.000000000000000000),
 ( 1.000000000000000000, 0.7071036778919828070, 1.000000000000000000),
 ( 1.000000000000000000, 0.7071145233811817477, 1.000000000000000000),
 ( 1.000000000000000000, 0.7071234056344251062, 1.000000000000000000),
 ( 1.000000000000000000, 0.7071224454176588958, 1.000000000000000000),
 ( 1.000000000000000000, 0.7071033992339055274, 1.000000000000000000),
 ( 1.000000000000000000, 0.7071405256055924848, 1.000000000000000000),
 ( 1.000000000000000000, 0.7071192080192385543, 1.000000000000000000),
 ( 1.000000000000000000, 0.7071067811865661135, 1.000000000000000000) ) ) 
 REPRESENTATION_ITEM ( '' )  SURFACE ( )  );
#92378 = ORIENTED_EDGE ( 'NONE', *, *, #48546, .F. ) ;
#92380 = ADVANCED_FACE ( 'NONE', ( #21879 ), #82816, .T. ) ;
#92379 = CARTESIAN_POINT ( 'NONE',  ( 0.000000000000000000, 0.000000000000000000, 5.000000000000002665 ) ) ;
#92381 = CARTESIAN_POINT ( 'NONE',  ( 4.284822031654965002, -1.092833614412281884, 104.4267991316945086 ) ) ;
#92382 = CARTESIAN_POINT ( 'NONE',  ( -86.34385121660355367, -60.13442145805939987, 4.656109867693190907 ) ) ;
#92383 = VECTOR ( 'NONE', #33578, 1000.000000000000000 ) ;
#92384 = CARTESIAN_POINT ( 'NONE',  ( 85.59800593614014019, 1.016364837396684119E-14, 0.000000000000000000 ) ) ;
#92385 = DIRECTION ( 'NONE',  ( 0.000000000000000000, 0.000000000000000000, -1.000000000000000000 ) ) ;
#92386 = DIRECTION ( 'NONE',  ( 0.000000000000000000, 0.000000000000000000, 1.000000000000000000 ) ) ;
#92387 = CARTESIAN_POINT ( 'NONE',  ( -2.912673042965788187E-14, 42.00000000000000000, -90.56128410203886858 ) ) ;
#92388 = CARTESIAN_POINT ( 'NONE',  ( 3.352941176470599860, -1.200583151104954061, 104.5794940929807524 ) ) ;
#92389 = CARTESIAN_POINT ( 'NONE',  ( 71.37437158690347871, -14.21045842199427156, 121.5198118854055451 ) ) ;
#92390 = CARTESIAN_POINT ( 'NONE',  ( -90.08857655234534434, -29.99999999999997158, -9.079940112750868764 ) ) ;
#92391 = CARTESIAN_POINT ( 'NONE',  ( -69.94854193131207865, -18.63627970369213216, 89.84632296843932409 ) ) ;
#92392 = VERTEX_POINT ( 'NONE', #95216 ) ;
#92393 = CARTESIAN_POINT ( 'NONE',  ( 60.31460910868286618, -60.00000000000004263, 109.8329304423809702 ) ) ;
#92394 = CARTESIAN_POINT ( 'NONE',  ( -56.56225795719330307, 40.83885343800341161, 32.16455131414174673 ) ) ;
#92395 = CARTESIAN_POINT ( 'NONE',  ( 71.84765068926689935, -57.67113087382353598, -33.99244728326649323 ) ) ;
#92396 = EDGE_LOOP ( 'NONE', ( #22448, #46284, #27233, #9307 ) ) ;
#92397 = CARTESIAN_POINT ( 'NONE',  ( 7.595889545591794523, -12.40783199751988697, 8.429977207772983760 ) ) ;
#92398 = CARTESIAN_POINT ( 'NONE',  ( -7.188101187500002709, -24.68750000204838813, 2.977408999572647819 ) ) ;
#92399 = ADVANCED_FACE ( 'NONE', ( #13737 ), #38136, .F. ) ;
#92400 = PLANE ( 'NONE',  #85591 ) ;
#92401 = ORIENTED_EDGE ( 'NONE', *, *, #65298, .F. ) ;
#92402 = AXIS2_PLACEMENT_3D ( 'NONE', #58034, #825, #49945 ) ;
#92403 = CARTESIAN_POINT ( 'NONE',  ( 5.007715329123895321E-16, -7.505553499465175804, -8.000000000000000000 ) ) ;
#92404 = DIRECTION ( 'NONE',  ( 0.000000000000000000, 1.000000000000000000, -0.000000000000000000 ) ) ;
#92405 = CARTESIAN_POINT ( 'NONE',  ( 47.01788285976068238, 17.61616053603655629, -16.34433538609931347 ) ) ;
#92406 = CARTESIAN_POINT ( 'NONE',  ( -11.12940285222375891, 43.17715607477184392, 15.08446948163250845 ) ) ;
#92407 = CARTESIAN_POINT ( 'NONE',  ( 2.977408999572650927, -15.87500000204838635, -7.188101187500001821 ) ) ;
#92408 = DIRECTION ( 'NONE',  ( 0.000000000000000000, -1.000000000000000000, 0.000000000000000000 ) ) ;
#92409 = COLOUR_RGB ( '', 0.72549020, 0.75294118, 0.79215686) ;
#92410 = CARTESIAN_POINT ( 'NONE',  ( 0.000000000000000000, 0.000000000000000000, -0.01269999999999830292 ) ) ;
#92411 = CARTESIAN_POINT ( 'NONE',  ( -9.999999999999989342, 49.99999999999999289, -86.30899693748770574 ) ) ;
#92412 = DIRECTION ( 'NONE',  ( -1.000000000000000000, -1.224606353822377258E-16, -0.000000000000000000 ) ) ;
#92413 = CARTESIAN_POINT ( 'NONE',  ( 10.63258248847111709, 47.99999999999999289, -95.64586607611548175 ) ) ;
#92414 = ORIENTED_EDGE ( 'NONE', *, *, #44045, .T. ) ;
#92415 = CARTESIAN_POINT ( 'NONE',  ( 5.803898591548207087, -3.468598768277492805, 103.8893302396401026 ) ) ;
#92416 = CARTESIAN_POINT ( 'NONE',  ( 32.74417656138047761, -42.96070844271284273, 34.86843745313173315 ) ) ;
#92417 = ORIENTED_EDGE ( 'NONE', *, *, #64245, .T. ) ;
#92418 = UNCERTAINTY_MEASURE_WITH_UNIT (LENGTH_MEASURE( 1.000000000000000082E-05 ), #46940, 'distance_accuracy_value', 'NONE');
#92419 = PRODUCT_RELATED_PRODUCT_CATEGORY ( 'part', '', ( #75968 ) ) ;
#92420 = ORIENTED_EDGE ( 'NONE', *, *, #17963, .T. ) ;
#92422 = CARTESIAN_POINT ( 'NONE',  ( -1.308371270545584553, -5.000000000000000000, -10.00012749751951624 ) ) ;
#92421 = CARTESIAN_POINT ( 'NONE',  ( -26.48777125522224551, 34.95844695497470411, -7.716963249296902028 ) ) ;
#92423 = CARTESIAN_POINT ( 'NONE',  ( 16.12042885873492892, 302.5603998061997686, -10.06194182264846049 ) ) ;
#92424 = CARTESIAN_POINT ( 'NONE',  ( -19.59509420870743668, 302.7300561768714147, -10.02587803886942197 ) ) ;
#92425 = DIRECTION ( 'NONE',  ( -1.000000000000000000, -1.224606353822377258E-16, -0.000000000000000000 ) ) ;
#92426 = CARTESIAN_POINT ( 'NONE',  ( 0.000000000000000000, 0.000000000000000000, -6.275264681066861527 ) ) ;
#92427 = CARTESIAN_POINT ( 'NONE',  ( -37.31409640255164106, 464.0485063763171638, 19.52659819501306160 ) ) ;
#92428 = ORIENTED_EDGE ( 'NONE', *, *, #56018, .T. ) ;
#92429 = CARTESIAN_POINT ( 'NONE',  ( 89.81584424423061819, -59.99999999999999289, -19.13689436224120044 ) ) ;
#92430 = CIRCLE ( 'NONE', #101065, 6.000000000000000888 ) ;
#92431 = CARTESIAN_POINT ( 'NONE',  ( 23.09999999999999432, 1.533819458162526451E-15, 0.000000000000000000 ) ) ;
#92432 = DIRECTION ( 'NONE',  ( 0.000000000000000000, 1.000000000000000000, 0.000000000000000000 ) ) ;
#92433 = CARTESIAN_POINT ( 'NONE',  ( 33.09999999999999432, 1.533819458162526451E-15, 0.000000000000000000 ) ) ;
#92434 = ORIENTED_EDGE ( 'NONE', *, *, #3504, .T. ) ;
#92435 = CARTESIAN_POINT ( 'NONE',  ( 0.000000000000000000, 55.00000000000000000, 0.000000000000000000 ) ) ;
#92436 = ORIENTED_EDGE ( 'NONE', *, *, #95268, .T. ) ;
#92437 = EDGE_LOOP ( 'NONE', ( #57138, #102494, #6109, #52846, #38256 ) ) ;
#92438 = CARTESIAN_POINT ( 'NONE',  ( 6.943926999490792618, 84.46699007373855750, -3.973092371898546027 ) ) ;
#92439 = CARTESIAN_POINT ( 'NONE',  ( 6.222742520105476238, -7.673830019007169767, 0.2914634815676377388 ) ) ;
#92440 = DIRECTION ( 'NONE',  ( 0.000000000000000000, -1.000000000000000000, 0.000000000000000000 ) ) ;
#92441 = CARTESIAN_POINT ( 'NONE',  ( 31.84999999999999787, 1.533819458162526451E-15, 0.000000000000000000 ) ) ;
#92443 = CARTESIAN_POINT ( 'NONE',  ( 85.70736671412652186, -60.21256416796455824, -14.76746838438766574 ) ) ;
#92442 = AXIS2_PLACEMENT_3D ( 'NONE', #72858, #97143, #55085 ) ;
#92444 = CIRCLE ( 'NONE', #40778, 8.000000000000000000 ) ;
#92445 = CARTESIAN_POINT ( 'NONE',  ( -39.80034396060564461, 313.8274241824321962, 2.558633328708789012 ) ) ;
#92446 = CARTESIAN_POINT ( 'NONE',  ( 66.74444444444444002, 6.915964383211875250E-15, 0.000000000000000000 ) ) ;
#92447 = CARTESIAN_POINT ( 'NONE',  ( -17.31689591039211251, 34.17651138339384431, 24.17515860248506598 ) ) ;
#92448 = ORIENTED_EDGE ( 'NONE', *, *, #34650, .T. ) ;
#92449 = FACE_OUTER_BOUND ( 'NONE', #18006, .T. ) ;
#92450 = EDGE_CURVE ( 'NONE', #97405, #36785, #13964, .T. ) ;
#92451 = ORIENTED_EDGE ( 'NONE', *, *, #51467, .F. ) ;
#92452 = CARTESIAN_POINT ( 'NONE',  ( -29.68315524076956891, -1.200000000000000030E-05, 39.60535821593508388 ) ) ;
#92453 = DIRECTION ( 'NONE',  ( -0.000000000000000000, 1.000000000000000000, -1.224646799147353207E-16 ) ) ;
#92454 =( GEOMETRIC_REPRESENTATION_CONTEXT ( 3 ) GLOBAL_UNCERTAINTY_ASSIGNED_CONTEXT ( ( #3018 ) ) GLOBAL_UNIT_ASSIGNED_CONTEXT ( ( #42303, #54622, #21788 ) ) REPRESENTATION_CONTEXT ( 'NONE', 'WORKASPACE' ) );
#92455 = CONICAL_SURFACE ( 'NONE', #42563, 5.000000000000010658, 0.9599310885968697082 ) ;
#92456 = CIRCLE ( 'NONE', #104462, 2.000000000000000000 ) ;
#92457 = VECTOR ( 'NONE', #99975, 1000.000000000000114 ) ;
#92459 = EDGE_LOOP ( 'NONE', ( #93722, #16238, #96579, #93716, #52954 ) ) ;
#92458 = DIRECTION ( 'NONE',  ( -0.000000000000000000, -0.000000000000000000, 1.000000000000000000 ) ) ;
#92460 = CARTESIAN_POINT ( 'NONE',  ( 76.96578608493661022, -39.49246347046180006, 129.2675137813639878 ) ) ;
#92461 = CIRCLE ( 'NONE', #97606, 2.000000000000000000 ) ;
#92462 = ORIENTED_EDGE ( 'NONE', *, *, #67408, .F. ) ;
#92463 = CARTESIAN_POINT ( 'NONE',  ( 0.9999999999999940048, -50.00000000000000000, 44.97220075561143204 ) ) ;
#92465 = DIRECTION ( 'NONE',  ( 0.000000000000000000, 0.000000000000000000, -1.000000000000000000 ) ) ;
#92464 = AXIS2_PLACEMENT_3D ( 'NONE', #37904, #54554, #87493 ) ;
#92466 = EDGE_CURVE ( 'NONE', #43607, #72268, #26061, .T. ) ;
#92467 = CARTESIAN_POINT ( 'NONE',  ( -7.188101187500002709, -25.81250000204838457, 2.977408999572647819 ) ) ;
#92468 = EDGE_CURVE ( 'NONE', #27527, #75440, #80067, .T. ) ;
#92469 = CARTESIAN_POINT ( 'NONE',  ( -93.88160267686131988, -57.67344353738141649, 16.36278552810739839 ) ) ;
#92470 = ORIENTED_EDGE ( 'NONE', *, *, #19874, .F. ) ;
#92471 = SHAPE_REPRESENTATION_RELATIONSHIP ( 'NONE' , 'NONE' ,  #84690, #101356 ) ;
#92472 = FACE_OUTER_BOUND ( 'NONE', #100767, .T. ) ;
#92473 = CARTESIAN_POINT ( 'NONE',  ( 105.2955105692893767, -60.15122319160084885, 186.5850414784887903 ) ) ;
#92474 = CARTESIAN_POINT ( 'NONE',  ( 5.455839282392823009, 51.31686971843895861, -8.522937042329454371 ) ) ;
#92475 = LINE ( 'NONE', #84401, #56670 ) ;
#92476 = CARTESIAN_POINT ( 'NONE',  ( 5.656854249492378806, -24.87500000409677270, 5.656854249492381470 ) ) ;
#92477 = LINE ( 'NONE', #17554, #62339 ) ;
#92478 = CARTESIAN_POINT ( 'NONE',  ( 9.918512371096317892, 246.2071700772944780, -1.297150762882707031 ) ) ;
#92479 = EDGE_CURVE ( 'NONE', #104058, #89914, #66193, .T. ) ;
#92480 =( NAMED_UNIT ( * ) SI_UNIT ( $, .STERADIAN. ) SOLID_ANGLE_UNIT ( ) );
#92481 = CIRCLE ( 'NONE', #23612, 9.000000000000000000 ) ;
#92482 = CARTESIAN_POINT ( 'NONE',  ( -37.71459991402551282, 437.7716825518406836, 4.505118785440030749 ) ) ;
#92483 = CARTESIAN_POINT ( 'NONE',  ( 31.46253585067004721, 1.340359594676612611E-15, 0.000000000000000000 ) ) ;
#92484 = CARTESIAN_POINT ( 'NONE',  ( 51.88291765283191381, 572.1183258647163257, 155.1969486012868913 ) ) ;
#92485 = CARTESIAN_POINT ( 'NONE',  ( 3.736676496572839845, -30.00000000000000000, -6.612488830499654746 ) ) ;
#92486 = ORIENTED_EDGE ( 'NONE', *, *, #45470, .T. ) ;
#92487 = CARTESIAN_POINT ( 'NONE',  ( 32.94331731755185189, 463.6330061646623335, 6.942105804440950045 ) ) ;
#92488 = CIRCLE ( 'NONE', #46005, 5.000000000000000000 ) ;
#92489 = CARTESIAN_POINT ( 'NONE',  ( 1.115771448223378925, 9.312113948361041338, 51.08078732034569924 ) ) ;
#92490 = CARTESIAN_POINT ( 'NONE',  ( -85.61137192986321054, -30.00000000000000000, 175.7392374104872772 ) ) ;
#92491 = B_SPLINE_CURVE_WITH_KNOTS ( 'NONE', 3,
 ( #41676, #74566, #639, #66479, #25538, #42203, #75086, #28196, #93430, #19583, #28722, #44886, #61065, #54520, #102032, #38392, #69162, #12480, #85330, #93959, #13008, #85884, #87464, #13543, #46461, #70205, #86938, #21170, #45934, #94501 ),
 .UNSPECIFIED., .F., .F.,
 ( 4, 2, 2, 2, 2, 2, 2, 2, 2, 2, 2, 2, 2, 2, 4 ),
 ( 0.000000000000000000, 0.0004909127471943187113, 0.0009818254943886374226, 0.001963650988777274845, 0.002945476483165912918, 0.003927301977554550558, 0.005890952966331935124, 0.007854603955109319691, 0.008836429449498011540, 0.009818254943886705124, 0.01178190593266408882, 0.01276373142705274771, 0.01374555692144140487, 0.01472738241583006549, 0.01570920791021872265 ),
 .UNSPECIFIED. ) ;
#92492 = ORIENTED_EDGE ( 'NONE', *, *, #102819, .T. ) ;
#92493 = CARTESIAN_POINT ( 'NONE',  ( 4.999999999999996447, -46.28647768034126386, 42.58845726811991739 ) ) ;
#92494 = CARTESIAN_POINT ( 'NONE',  ( 72.49335252660162610, -57.66551810483609586, 176.8856597097985457 ) ) ;
#92496 = CARTESIAN_POINT ( 'NONE',  ( -7.000000000000000000, -60.71953810597521795, 12.61250543006203273 ) ) ;
#92495 = CARTESIAN_POINT ( 'NONE',  ( -14.38793715987803878, 1.958934843038082851, -4.277839136690804622 ) ) ;
#92497 = ADVANCED_FACE ( 'NONE', ( #88707 ), #104897, .T. ) ;
#92498 = CARTESIAN_POINT ( 'NONE',  ( 37.56709637062468232, -32.17750619218406882, -37.66840575663092494 ) ) ;
#92499 = CARTESIAN_POINT ( 'NONE',  ( -14.66255430293768569, 22.40929092343608175, -3.546301636274618030 ) ) ;
#92500 = B_SPLINE_CURVE_WITH_KNOTS ( 'NONE', 3,
 ( #61552, #70154, #94446, #20604, #60494, #35154 ),
 .UNSPECIFIED., .F., .F.,
 ( 4, 2, 4 ),
 ( 0.01390592816464533178, 0.01784842065628997748, 0.02179091314793462492 ),
 .UNSPECIFIED. ) ;
#92501 = CARTESIAN_POINT ( 'NONE',  ( -44.03654441204246694, 435.3114017552750852, 15.42721916006553684 ) ) ;
#92502 = CARTESIAN_POINT ( 'NONE',  ( -29.01163664099933825, -59.99999999999997868, 42.57063036807574719 ) ) ;
#92503 = PRESENTATION_STYLE_ASSIGNMENT (( #26757 ) ) ;
#92504 = CARTESIAN_POINT ( 'NONE',  ( -11.91432047182415133, 48.00000000000000000, 64.17585289259233150 ) ) ;
#92505 = AXIS2_PLACEMENT_3D ( 'NONE', #64363, #81044, #89157 ) ;
#92506 = CARTESIAN_POINT ( 'NONE',  ( -85.76695094951085707, -50.18274658732842397, 190.4785943899394738 ) ) ;
#92507 = ORIENTED_EDGE ( 'NONE', *, *, #76700, .F. ) ;
#92508 = CARTESIAN_POINT ( 'NONE',  ( 35.67188573693742626, 438.4052817328919787, 3.942852940163526831 ) ) ;
#92509 = CARTESIAN_POINT ( 'NONE',  ( -2.053642860964516981, -60.36585557917648970, 33.94789663158027793 ) ) ;
#92510 = CYLINDRICAL_SURFACE ( 'NONE', #23940, 4.000000000000000000 ) ;
#92511 = CARTESIAN_POINT ( 'NONE',  ( 32.42646496125431099, 485.5066083816492437, 3.829258843081624786 ) ) ;
#92514 = EDGE_CURVE ( 'NONE', #78362, #37165, #54508, .T. ) ;
#92513 = CARTESIAN_POINT ( 'NONE',  ( -7.797782256654760324, 54.21795136539236637, 1.776235144415082567 ) ) ;
#92512 = CARTESIAN_POINT ( 'NONE',  ( -36.34772026823453928, 305.6056078828891032, 4.444403256936394264 ) ) ;
#92515 = ORIENTED_EDGE ( 'NONE', *, *, #39415, .T. ) ;
#92516 = CARTESIAN_POINT ( 'NONE',  ( -8.000000000000000000, 0.000000000000000000, -11.12471428571428689 ) ) ;
#92517 = FACE_OUTER_BOUND ( 'NONE', #56551, .T. ) ;
#92518 = AXIS2_PLACEMENT_3D ( 'NONE', #66793, #48985, #72735 ) ;
#92519 = AXIS2_PLACEMENT_3D ( 'NONE', #86461, #13048, #61104 ) ;
#92520 = CARTESIAN_POINT ( 'NONE',  ( 17.52467020414865218, 50.00000000000000000, 63.14993973816012129 ) ) ;
#92521 = CARTESIAN_POINT ( 'NONE',  ( 45.49982102694234953, 388.3127959276886827, 7.886590035822850453 ) ) ;
#92522 = CARTESIAN_POINT ( 'NONE',  ( 0.000000000000000000, 0.000000000000000000, 0.000000000000000000 ) ) ;
#92523 = DIRECTION ( 'NONE',  ( 0.000000000000000000, 0.000000000000000000, 1.000000000000000000 ) ) ;
#92524 = CARTESIAN_POINT ( 'NONE',  ( 110.2448519957423940, -60.00000000000004974, 128.1456905595833575 ) ) ;
#92525 = CARTESIAN_POINT ( 'NONE',  ( -79.44753746119148730, -49.90808891599596819, 154.1174546483202903 ) ) ;
#92526 = ORIENTED_EDGE ( 'NONE', *, *, #64566, .T. ) ;
#92527 = DIRECTION ( 'NONE',  ( -0.5735764363510459374, -0.8191520442889919096, 0.000000000000000000 ) ) ;
#92528 = CARTESIAN_POINT ( 'NONE',  ( 5.725004243152318928, 253.5751914825536346, -1.812899781754669259 ) ) ;
#92529 = AXIS2_PLACEMENT_3D ( 'NONE', #88108, #87579, #52140 ) ;
#92530 = CARTESIAN_POINT ( 'NONE',  ( 22.32272541537730604, -57.67282817906140480, 42.57846511115439370 ) ) ;
#92531 = AXIS2_PLACEMENT_3D ( 'NONE', #49913, #18108, #74713 ) ;
#92532 = VECTOR ( 'NONE', #4046, 1000.000000000000000 ) ;
#92533 = AXIS2_PLACEMENT_3D ( 'NONE', #15211, #74505, #58331 ) ;
#92534 = FACE_OUTER_BOUND ( 'NONE', #18446, .T. ) ;
#92535 = CARTESIAN_POINT ( 'NONE',  ( -42.61140200160144786, 465.9030374194822457, 13.21253569360411895 ) ) ;
#92536 = ADVANCED_FACE ( 'NONE', ( #29963 ), #95738, .F. ) ;
#92537 = CARTESIAN_POINT ( 'NONE',  ( 43.03357534759653902, 463.2291678140142608, 4.675918524165878054 ) ) ;
#92538 = ORIENTED_EDGE ( 'NONE', *, *, #100251, .T. ) ;
#92539 = DIRECTION ( 'NONE',  ( 0.000000000000000000, 0.000000000000000000, -1.000000000000000000 ) ) ;
#92540 = ORIENTED_EDGE ( 'NONE', *, *, #43505, .F. ) ;
#92541 =( NAMED_UNIT ( * ) SI_UNIT ( $, .STERADIAN. ) SOLID_ANGLE_UNIT ( ) );
#92542 = AXIS2_PLACEMENT_3D ( 'NONE', #61404, #79155, #70549 ) ;
#92544 = EDGE_CURVE ( 'NONE', #46516, #46768, #8301, .T. ) ;
#92543 = CARTESIAN_POINT ( 'NONE',  ( -9.035703905990965623, 10.37169118567825343, -12.88508357975252316 ) ) ;
#92545 = CARTESIAN_POINT ( 'NONE',  ( 32.68130198256140062, 486.6487900980583845, 8.407187415474162151 ) ) ;
#92546 = CARTESIAN_POINT ( 'NONE',  ( 11.91432047181420195, 49.99999999997997691, 64.17585289263315929 ) ) ;
#92547 = CARTESIAN_POINT ( 'NONE',  ( 4.999999999999920064, -15.02849299145039552, 13.75080192255986766 ) ) ;
#92548 = B_SPLINE_CURVE_WITH_KNOTS ( 'NONE', 3,
 ( #93862, #94941, #12390, #21593, #5887, #45318, #54967, #87896, #69067, #78200, #103021, #29176 ),
 .UNSPECIFIED., .F., .F.,
 ( 4, 2, 2, 2, 2, 4 ),
 ( 5.851754814686364485E-16, 0.001874863313077309570, 0.003749726626154033671, 0.004687158282692394096, 0.005624589939230754954, 0.007499453252307401209 ),
 .UNSPECIFIED. ) ;
#92549 = DIRECTION ( 'NONE',  ( 0.000000000000000000, 0.000000000000000000, 1.000000000000000000 ) ) ;
#92550 = ORIENTED_EDGE ( 'NONE', *, *, #105893, .T. ) ;
#92551 = CARTESIAN_POINT ( 'NONE',  ( 100.7596044958396106, -60.00000000000001421, 201.6406045078230136 ) ) ;
#92553 = CARTESIAN_POINT ( 'NONE',  ( 21.78139057835771553, -56.87475540586999756, 34.12209627113270471 ) ) ;
#92552 = CARTESIAN_POINT ( 'NONE',  ( -81.10703223160209063, -14.21045842199456288, 192.6080781080067652 ) ) ;
#92554 = CARTESIAN_POINT ( 'NONE',  ( 83.10779110695617078, -38.00000000000002842, -10.21842127791309274 ) ) ;
#92555 = CARTESIAN_POINT ( 'NONE',  ( 37.61445974613948806, 372.0213524726607943, 4.443563355633848744 ) ) ;
#92556 = CARTESIAN_POINT ( 'NONE',  ( -41.03595122651036320, -60.25878796785968206, 44.31288513920497252 ) ) ;
#92557 = CIRCLE ( 'NONE', #42585, 5.000000000000000888 ) ;
#92558 = DIRECTION ( 'NONE',  ( 0.000000000000000000, 0.000000000000000000, -1.000000000000000000 ) ) ;
#92559 = VERTEX_POINT ( 'NONE', #49826 ) ;
#92560 = DIRECTION ( 'NONE',  ( 0.000000000000000000, 0.000000000000000000, 1.000000000000000000 ) ) ;
#92561 = CARTESIAN_POINT ( 'NONE',  ( 7.370192266679785220, 54.30878245688016648, 2.387241612175243333 ) ) ;
#92562 = CARTESIAN_POINT ( 'NONE',  ( -43.71999369285486381, 463.9422086738335338, 7.488562083380655210 ) ) ;
#92563 = FACE_OUTER_BOUND ( 'NONE', #3817, .T. ) ;
#92564 = DIRECTION ( 'NONE',  ( 0.000000000000000000, 0.000000000000000000, 1.000000000000000000 ) ) ;
#92565 = CARTESIAN_POINT ( 'NONE',  ( -30.00000000000000355, 489.0575207958488591, 4.971052219119334481 ) ) ;
#92567 = EDGE_LOOP ( 'NONE', ( #14087, #25490, #11728, #92247, #13617, #103294 ) ) ;
#92566 = VECTOR ( 'NONE', #15074, 1000.000000000000000 ) ;
#92568 = SURFACE_STYLE_FILL_AREA ( #99586 ) ;
#92569 = EDGE_LOOP ( 'NONE', ( #2645, #69795, #63438 ) ) ;
#92570 = CARTESIAN_POINT ( 'NONE',  ( 97.20601475542966341, -29.99999999999981171, 191.0240291480905910 ) ) ;
#92571 = CARTESIAN_POINT ( 'NONE',  ( 40.55775739592876050, 39.72826581815989044, -52.22352489735080638 ) ) ;
#92572 = ADVANCED_FACE ( 'NONE', ( #82731 ), #12215, .F. ) ;
#92573 = CARTESIAN_POINT ( 'NONE',  ( -5.191472769733078252, -82.35908423281054525, -3.014900733016756540 ) ) ;
#92574 = CARTESIAN_POINT ( 'NONE',  ( 86.61511892060461548, -30.00000000000000355, 68.09894758470834120 ) ) ;
#92575 = CARTESIAN_POINT ( 'NONE',  ( -25.97927592289829946, 307.2264714490293613, 10.71202005274685298 ) ) ;
#92576 = EDGE_LOOP ( 'NONE', ( #57772, #56310, #72998, #79883, #53426 ) ) ;
#92577 = VERTEX_POINT ( 'NONE', #91370 ) ;
#92578 = EDGE_LOOP ( 'NONE', ( #89823, #100003 ) ) ;
#92580 = ORIENTED_EDGE ( 'NONE', *, *, #69607, .T. ) ;
#92579 = CARTESIAN_POINT ( 'NONE',  ( -47.55322331356164511, 10.90908589463665734, -16.76771630193830376 ) ) ;
#92581 = CARTESIAN_POINT ( 'NONE',  ( 29.34999999999999787, 1.533819458162526451E-15, 0.000000000000000000 ) ) ;
#92582 = CARTESIAN_POINT ( 'NONE',  ( -37.56673239365863282, 25.75719283951018568, -10.95617127781023648 ) ) ;
#92583 = CARTESIAN_POINT ( 'NONE',  ( 5.981691436642411652, -13.97269099194115860, -0.5384679144502718673 ) ) ;
#92584 = CARTESIAN_POINT ( 'NONE',  ( -31.39564607133891982, 425.0048870508487084, 23.79503637330282828 ) ) ;
#92585 = VECTOR ( 'NONE', #86086, 999.9999999999998863 ) ;
#92586 = VERTEX_POINT ( 'NONE', #48747 ) ;
#92587 = CARTESIAN_POINT ( 'NONE',  ( 5.036189802310016006, 50.00000000000001421, -93.73786388411662074 ) ) ;
#92588 = ORIENTED_EDGE ( 'NONE', *, *, #56990, .T. ) ;
#92589 = FACE_BOUND ( 'NONE', #18041, .T. ) ;
#92590 = CARTESIAN_POINT ( 'NONE',  ( 75.54928104856406890, -38.35460038409268435, 174.6471884719728394 ) ) ;
#92591 = DIRECTION ( 'NONE',  ( 0.000000000000000000, 1.000000000000000000, 0.000000000000000000 ) ) ;
#92592 = CARTESIAN_POINT ( 'NONE',  ( 32.36394494278211198, 300.7469127741676971, 11.27404243930863714 ) ) ;
#92593 = CARTESIAN_POINT ( 'NONE',  ( 0.000000000000000000, 0.000000000000000000, 0.000000000000000000 ) ) ;
#92594 = CIRCLE ( 'NONE', #30644, 8.331345277524542681 ) ;
#92595 = ORIENTED_EDGE ( 'NONE', *, *, #21344, .T. ) ;
#92596 = CARTESIAN_POINT ( 'NONE',  ( 28.61418328824293766, 13.49088233573899487, -40.19504096224954992 ) ) ;
#92597 = DIRECTION ( 'NONE',  ( 0.000000000000000000, 1.000000000000000000, 0.000000000000000000 ) ) ;
#92598 = CARTESIAN_POINT ( 'NONE',  ( 26.55368054879998141, 296.1687614156957693, 2.221803138960261492 ) ) ;
#92599 = ADVANCED_FACE ( 'NONE', ( #99971 ), #64954, .T. ) ;
#92600 = DIRECTION ( 'NONE',  ( -1.000000000000000000, -0.000000000000000000, -0.000000000000000000 ) ) ;
#92601 = CARTESIAN_POINT ( 'NONE',  ( 14.27029591641831274, 3.391655494167682861, 4.551126452496778718 ) ) ;
#92602 = ORIENTED_EDGE ( 'NONE', *, *, #51641, .T. ) ;
#92603 = CARTESIAN_POINT ( 'NONE',  ( 7.344133061198927948, -87.44494392680577732, 3.176267128233875248 ) ) ;
#92604 = CARTESIAN_POINT ( 'NONE',  ( -3.857142857142850989, -1.200583151104938517, 103.1763305333244318 ) ) ;
#92605 = CARTESIAN_POINT ( 'NONE',  ( 33.52307692307692122, 1.411358822780289120E-15, 0.000000000000000000 ) ) ;
#92606 = CARTESIAN_POINT ( 'NONE',  ( -3.295171437451867469, -7.213553046160193993, -7.590212325761443779 ) ) ;
#92607 = CARTESIAN_POINT ( 'NONE',  ( 106.4000000000000057, 0.000000000000000000, 0.000000000000000000 ) ) ;
#92608 = ADVANCED_FACE ( 'NONE', ( #32619, #67088, #7237, #40145 ), #7768, .F. ) ;
#92609 = VECTOR ( 'NONE', #53910, 1000.000000000000114 ) ;
#92610 = LINE ( 'NONE', #91041, #63964 ) ;
#92611 = AXIS2_PLACEMENT_3D ( 'NONE', #77066, #3180, #68995 ) ;
#92612 = CARTESIAN_POINT ( 'NONE',  ( 86.06184277206247657, -28.35162415433135763, 182.3406178006961227 ) ) ;
#92613 = CARTESIAN_POINT ( 'NONE',  ( 0.3539438260514400914, 15.11738935797732530, -9.999999999999998224 ) ) ;
#92614 = CARTESIAN_POINT ( 'NONE',  ( -8.309329435564448474, 32.78459446882924766, 0.000000000000000000 ) ) ;
#92615 = ORIENTED_EDGE ( 'NONE', *, *, #35616, .T. ) ;
#92616 = CARTESIAN_POINT ( 'NONE',  ( -4.555432764205793461, 5.242992371775925697, -6.208169345099787684 ) ) ;
#92617 = DIRECTION ( 'NONE',  ( -1.000000000000000000, -1.224606353822377258E-16, -0.000000000000000000 ) ) ;
#92618 = LINE ( 'NONE', #3084, #66166 ) ;
#92619 = LINE ( 'NONE', #59209, #20056 ) ;
#92620 = CIRCLE ( 'NONE', #68538, 66.50000000000000000 ) ;
#92621 = CARTESIAN_POINT ( 'NONE',  ( -90.12656837431330814, -29.99999999999999645, 89.23295766621065184 ) ) ;
#92622 = ADVANCED_FACE ( 'NONE', ( #702 ), #72493, .T. ) ;
#92623 = CONICAL_SURFACE ( 'NONE', #97774, 3.309500000000001663, 0.9599310885968770357 ) ;
#92624 = FACE_OUTER_BOUND ( 'NONE', #35416, .T. ) ;
#92625 = DIRECTION ( 'NONE',  ( -1.000000000000000000, -0.000000000000000000, -0.000000000000000000 ) ) ;
#92626 = CARTESIAN_POINT ( 'NONE',  ( -5.276498195232381505, 6.073236878018020590, -7.633618187056802284 ) ) ;
#92627 = CARTESIAN_POINT ( 'NONE',  ( -7.907996613752301229, -3.055722423191993276, -7.792112796859424151 ) ) ;
#92628 = ADVANCED_FACE ( 'NONE', ( #33673 ), #33145, .F. ) ;
#92629 = VECTOR ( 'NONE', #50354, 1000.000000000000000 ) ;
#92630 = CARTESIAN_POINT ( 'NONE',  ( 3.833393730521447829, -52.97426161280114343, 40.46628978130268450 ) ) ;
#92631 = CARTESIAN_POINT ( 'NONE',  ( 9.797174393178839462E-16, 80.00000000000000000, 8.000000000000010658 ) ) ;
#92632 = CARTESIAN_POINT ( 'NONE',  ( -19.50010530980351220, 50.00000000000000000, 59.90637122617393828 ) ) ;
#92633 = DIRECTION ( 'NONE',  ( 2.742080092235280244E-17, 0.000000000000000000, -1.000000000000000000 ) ) ;
#92634 = CARTESIAN_POINT ( 'NONE',  ( 72.11682663846713126, 4.000000000000013323, 0.000000000000000000 ) ) ;
#92635 = CARTESIAN_POINT ( 'NONE',  ( 64.05557409813005165, -29.67380080880776561, -23.45134551522981425 ) ) ;
#92636 = STYLED_ITEM ( 'NONE', ( #719 ), #30042 ) ;
#92637 = EDGE_CURVE ( 'NONE', #93970, #103206, #66014, .T. ) ;
#92638 = CARTESIAN_POINT ( 'NONE',  ( -22.50258514725704373, -39.47840698168496942, 31.31635883088512884 ) ) ;
#92639 = ORIENTED_EDGE ( 'NONE', *, *, #91531, .F. ) ;
#92640 = CARTESIAN_POINT ( 'NONE',  ( 6.481088301903606741, 9.994875444612373983, -2.652222390170977384 ) ) ;
#92641 = CARTESIAN_POINT ( 'NONE',  ( -9.537909130738276176, 107.6461483096339435, -3.010726932293859903 ) ) ;
#92642 = CARTESIAN_POINT ( 'NONE',  ( -17.08789101759687767, -56.88345495196291779, 33.63599213401663945 ) ) ;
#92643 = CARTESIAN_POINT ( 'NONE',  ( -38.36866069078110542, -24.37386123566381713, -30.62827207695247012 ) ) ;
#92646 = EDGE_CURVE ( 'NONE', #11977, #103417, #86310, .T. ) ;
#92645 = DIRECTION ( 'NONE',  ( 1.000000000000000000, 0.000000000000000000, 0.000000000000000000 ) ) ;
#92644 = CARTESIAN_POINT ( 'NONE',  ( 43.75401118688382951, 486.3173572309547694, 5.908089951475070656 ) ) ;
#92647 = ORIENTED_EDGE ( 'NONE', *, *, #98287, .F. ) ;
#92648 = AXIS2_PLACEMENT_3D ( 'NONE', #56262, #56807, #97273 ) ;
#92649 = CARTESIAN_POINT ( 'NONE',  ( 6.222802839579463452, -4.089658325571342345, -6.499999999999999112 ) ) ;
#92650 = ORIENTED_EDGE ( 'NONE', *, *, #75812, .F. ) ;
#92651 = DIRECTION ( 'NONE',  ( -0.5735764363510512664, 0.8191520442889881348, 1.003171929053520309E-16 ) ) ;
#92652 = CARTESIAN_POINT ( 'NONE',  ( 0.000000000000000000, 0.000000000000000000, 0.000000000000000000 ) ) ;
#92653 = CARTESIAN_POINT ( 'NONE',  ( -13.21548557454697281, -60.00000000000000000, -42.26782324170446259 ) ) ;
#92654 = ORIENTED_EDGE ( 'NONE', *, *, #70852, .T. ) ;
#92655 = CARTESIAN_POINT ( 'NONE',  ( -5.855865337385174563, 294.7602933681740183, -8.111083302970204301 ) ) ;
#92656 = CARTESIAN_POINT ( 'NONE',  ( 101.3229910990397968, -52.73391794366923335, 193.0151051031019449 ) ) ;
#92657 = PRESENTATION_LAYER_ASSIGNMENT (  '', '', ( #28986 ) ) ;
#92659 = CARTESIAN_POINT ( 'NONE',  ( -8.000113193197769590, -5.999773613541393047, -0.2613481123984661703 ) ) ;
#92658 = CARTESIAN_POINT ( 'NONE',  ( 7.676252702269514394, -19.86679654487617341, 27.19205508634107460 ) ) ;
#92660 = EDGE_CURVE ( 'NONE', #44939, #48427, #34216, .T. ) ;
#92661 = CIRCLE ( 'NONE', #35893, 5.000000000000002665 ) ;
#92662 = VERTEX_POINT ( 'NONE', #91885 ) ;
#92663 = ORIENTED_EDGE ( 'NONE', *, *, #28315, .F. ) ;
#92664 = ORIENTED_EDGE ( 'NONE', *, *, #79657, .T. ) ;
#92665 = CARTESIAN_POINT ( 'NONE',  ( 25.56551311124981751, 308.5030443763377548, 10.78605441908344531 ) ) ;
#92666 = EDGE_CURVE ( 'NONE', #75037, #48423, #27749, .T. ) ;
#92667 = FACE_OUTER_BOUND ( 'NONE', #37703, .T. ) ;
#92668 = CARTESIAN_POINT ( 'NONE',  ( 16.64348903516523848, 45.88445698070336221, 4.157797401561420081 ) ) ;
#92669 = VERTEX_POINT ( 'NONE', #49283 ) ;
#92670 = FACE_OUTER_BOUND ( 'NONE', #102049, .T. ) ;
#92671 = DIRECTION ( 'NONE',  ( 0.000000000000000000, 0.000000000000000000, 1.000000000000000000 ) ) ;
#92672 = CARTESIAN_POINT ( 'NONE',  ( 31.43619199075894244, 438.9212978929645033, 23.14895173483415292 ) ) ;
#92673 = CARTESIAN_POINT ( 'NONE',  ( -93.13590452085961147, -60.00000000000967049, -17.97697602678234574 ) ) ;
#92674 = DIRECTION ( 'NONE',  ( -1.000000000000000000, -0.000000000000000000, -0.000000000000000000 ) ) ;
#92675 = AXIS2_PLACEMENT_3D ( 'NONE', #60335, #93208, #19373 ) ;
#92676 = CARTESIAN_POINT ( 'NONE',  ( -23.96375140441108442, 306.3052962357393199, 10.25885168886986243 ) ) ;
#92677 = VECTOR ( 'NONE', #64953, 999.9999999999998863 ) ;
#92678 = DIRECTION ( 'NONE',  ( -1.000000000000000000, -1.224606353822377258E-16, -0.000000000000000000 ) ) ;
#92679 = CARTESIAN_POINT ( 'NONE',  ( -82.45890327043613865, -29.99999999999992184, -23.17447414549992146 ) ) ;
#92680 = EDGE_CURVE ( 'NONE', #6033, #44023, #32951, .T. ) ;
#92681 = PRESENTATION_STYLE_ASSIGNMENT (( #43599 ) ) ;
#92682 = CARTESIAN_POINT ( 'NONE',  ( -51.13654845188015230, -46.44342577944571104, 55.14519627722154382 ) ) ;
#92683 = VERTEX_POINT ( 'NONE', #57375 ) ;
#92684 = CARTESIAN_POINT ( 'NONE',  ( 0.000000000000000000, 45.00000000000000711, 0.000000000000000000 ) ) ;
#92686 = ORIENTED_EDGE ( 'NONE', *, *, #71346, .F. ) ;
#92685 = CIRCLE ( 'NONE', #25420, 4.172000000000009479 ) ;
#92687 = DIRECTION ( 'NONE',  ( 0.000000000000000000, 0.000000000000000000, -1.000000000000000000 ) ) ;
#92688 = VECTOR ( 'NONE', #59055, 1000.000000000000000 ) ;
#92689 = CARTESIAN_POINT ( 'NONE',  ( -4.250000000000000000, 5.204748896376250699E-16, -8.028130060628445364 ) ) ;
#92690 = CARTESIAN_POINT ( 'NONE',  ( 15.90614609307868399, -3.157894736842107086, 14.66382285868950852 ) ) ;
#92691 = ORIENTED_EDGE ( 'NONE', *, *, #101780, .T. ) ;
#92692 = CARTESIAN_POINT ( 'NONE',  ( 84.40671846796894329, -38.73973353392212005, 198.0806718234546508 ) ) ;
#92693 = EDGE_CURVE ( 'NONE', #13812, #44516, #87989, .T. ) ;
#92694 = LINE ( 'NONE', #43613, #3116 ) ;
#92695 = CARTESIAN_POINT ( 'NONE',  ( 87.41401970320464443, -30.00000000000000000, 185.1823391226513422 ) ) ;
#92696 = LINE ( 'NONE', #85141, #75111 ) ;
#92697 = DIRECTION ( 'NONE',  ( 0.000000000000000000, -1.000000000000000000, 0.000000000000000000 ) ) ;
#92698 = MECHANICAL_DESIGN_GEOMETRIC_PRESENTATION_REPRESENTATION (  '', ( #4860 ), #80602 ) ;
#92699 = ORIENTED_EDGE ( 'NONE', *, *, #19266, .F. ) ;
#92700 = ORIENTED_EDGE ( 'NONE', *, *, #90048, .T. ) ;
#92701 = CARTESIAN_POINT ( 'NONE',  ( 52.14939519039409532, -60.30582305101183493, 62.32281964044140921 ) ) ;
#92702 = CARTESIAN_POINT ( 'NONE',  ( -46.00000000000000000, 437.8919113138612147, 12.69150955565185335 ) ) ;
#92703 = CARTESIAN_POINT ( 'NONE',  ( -43.00000000000000000, 485.2629658518202405, -2.796394914059407100 ) ) ;
#92704 = ORIENTED_EDGE ( 'NONE', *, *, #7213, .F. ) ;
#92705 = CARTESIAN_POINT ( 'NONE',  ( -85.43458966979623881, -38.35985982854320042, -22.44720385632372128 ) ) ;
#92706 =( GEOMETRIC_REPRESENTATION_CONTEXT ( 3 ) GLOBAL_UNCERTAINTY_ASSIGNED_CONTEXT ( ( #75349 ) ) GLOBAL_UNIT_ASSIGNED_CONTEXT ( ( #4103, #92160, #86105 ) ) REPRESENTATION_CONTEXT ( 'NONE', 'WORKASPACE' ) );
#92707 = ORIENTED_EDGE ( 'NONE', *, *, #65588, .F. ) ;
#92708 = CARTESIAN_POINT ( 'NONE',  ( -1.469576158976823947E-15, -29.56250000409677270, 8.000000000000000000 ) ) ;
#92709 = CARTESIAN_POINT ( 'NONE',  ( 106.8991994874582190, -38.36537085630794053, 195.0165758976116308 ) ) ;
#92710 = CARTESIAN_POINT ( 'NONE',  ( 15.20001342229217123, 22.50991373429433295, -3.104903353136252431 ) ) ;
#92711 = CARTESIAN_POINT ( 'NONE',  ( 84.42372515681569212, -45.28278671564551416, 28.58935177623963853 ) ) ;
#92712 = CARTESIAN_POINT ( 'NONE',  ( -1.249368327036161963, 45.80196013925338860, -17.33667219389016978 ) ) ;
#92713 = CARTESIAN_POINT ( 'NONE',  ( -23.13382475031087537, 305.4031188766097671, -9.881612764625065992 ) ) ;
#92714 = SURFACE_SIDE_STYLE ('',( #59843 ) ) ;
#92715 = AXIS2_PLACEMENT_3D ( 'NONE', #69509, #102395, #28545 ) ;
#92716 = FACE_OUTER_BOUND ( 'NONE', #44695, .T. ) ;
#92717 = CARTESIAN_POINT ( 'NONE',  ( -43.63899620156475834, 434.3182181978404515, 14.37213632273176600 ) ) ;
#92718 = CARTESIAN_POINT ( 'NONE',  ( 2.869468778192031166, 64.67094895189187298, 5.000000000000000000 ) ) ;
#92720 = VERTEX_POINT ( 'NONE', #61126 ) ;
#92719 =( BOUNDED_SURFACE ( )  B_SPLINE_SURFACE ( 3, 2, ( 
 ( #70431, #60236, #61278 ),
 ( #76915, #103327, #3025 ),
 ( #29473, #95240, #36506 ),
 ( #21372, #54210, #46155 ),
 ( #5163, #93104, #19276 ),
 ( #27891, #60758, #93646 ) ),
 .UNSPECIFIED., .F., .F., .F. ) 
 B_SPLINE_SURFACE_WITH_KNOTS ( ( 4, 2, 4 ),
 ( 3, 3 ),
 ( -2.180330568868349417E-15, 0.001801542390186249357, 0.003603084780374679261 ),
 ( 0.000000000000000000, 1.000000000000000000 ),
 .UNSPECIFIED. ) 
 GEOMETRIC_REPRESENTATION_ITEM ( )  RATIONAL_B_SPLINE_SURFACE ( (
 ( 1.000000000000000000, 0.8291561975892046688, 1.000000000000000000),
 ( 1.000000000000000000, 0.8506934603553527596, 1.000000000000000000),
 ( 1.000000000000000000, 0.8671388017650453195, 1.000000000000000000),
 ( 1.000000000000000000, 0.8933560653587880873, 1.000000000000000000),
 ( 1.000000000000000000, 0.9032011672209129260, 1.000000000000000000),
 ( 1.000000000000000000, 0.9115707425103370953, 1.000000000000000000) ) ) 
 REPRESENTATION_ITEM ( '' )  SURFACE ( )  );
#92721 = ADVANCED_FACE ( 'NONE', ( #10944 ), #55237, .T. ) ;
#92722 = CARTESIAN_POINT ( 'NONE',  ( 28.17977184163764193, 1.482358050883964840E-15, 0.000000000000000000 ) ) ;
#92723 = CARTESIAN_POINT ( 'NONE',  ( 0.000000000000000000, 0.000000000000000000, 5.000000000000002665 ) ) ;
#92724 = EDGE_LOOP ( 'NONE', ( #16575, #58278, #52705, #70668 ) ) ;
#92725 = CARTESIAN_POINT ( 'NONE',  ( -4.297323614437654093, 53.80478256577427487, 8.057193928358454826 ) ) ;
#92726 = AXIS2_PLACEMENT_3D ( 'NONE', #95433, #39730, #4832 ) ;
#92727 = CARTESIAN_POINT ( 'NONE',  ( -31.09395556286335704, 323.2306627077637700, 14.95105751057811538 ) ) ;
#92728 = CARTESIAN_POINT ( 'NONE',  ( -7.500000000000000000, -4.330127018922201643, -7.422398894150036064 ) ) ;
#92729 = FACE_OUTER_BOUND ( 'NONE', #16529, .T. ) ;
#92730 = CARTESIAN_POINT ( 'NONE',  ( 3.313708498984762052, -24.21874999999999289, -8.000000000000000000 ) ) ;
#92731 = CARTESIAN_POINT ( 'NONE',  ( 28.90468586868453471, -21.14203283741673545, 31.90548891044728919 ) ) ;
#92732 = ADVANCED_FACE ( 'NONE', ( #43865, #69228, #53027, #28256, #36359 ), #96608, .T. ) ;
#92733 = MECHANICAL_DESIGN_GEOMETRIC_PRESENTATION_REPRESENTATION (  '', ( #68655 ), #94454 ) ;
#92734 = CARTESIAN_POINT ( 'NONE',  ( 9.833493305133805151, 4.000000000000003553, 0.000000000000000000 ) ) ;
#92735 = AXIS2_PLACEMENT_3D ( 'NONE', #42943, #101181, #18697 ) ;
#92736 = EDGE_CURVE ( 'NONE', #47738, #105869, #3615, .T. ) ;
#92737 = EDGE_LOOP ( 'NONE', ( #5370, #39961 ) ) ;
#92738 = CARTESIAN_POINT ( 'NONE',  ( 83.57408830821859169, -42.98028180361450978, 179.4502539513921988 ) ) ;
#92739 = FACE_OUTER_BOUND ( 'NONE', #57607, .T. ) ;
#92740 = AXIS2_PLACEMENT_3D ( 'NONE', #93973, #19596, #68649 ) ;
#92741 = CARTESIAN_POINT ( 'NONE',  ( 10.28624191511773844, 43.25714326066793092, -15.40779740156427202 ) ) ;
#92742 = EDGE_LOOP ( 'NONE', ( #11945, #99344, #104788, #69222 ) ) ;
#92743 = CARTESIAN_POINT ( 'NONE',  ( -94.80169991939609986, -37.82085344593683374, 106.6770961138861367 ) ) ;
#92744 = CARTESIAN_POINT ( 'NONE',  ( -32.17646412119415800, 464.6980787822275261, 10.84896803612779514 ) ) ;
#92745 = DIRECTION ( 'NONE',  ( -1.000000000000000000, -1.224606353822377258E-16, -0.000000000000000000 ) ) ;
#92746 = CARTESIAN_POINT ( 'NONE',  ( -13.83769416168977173, -3.000000000000002665, -79.05569278143936174 ) ) ;
#92747 = CARTESIAN_POINT ( 'NONE',  ( -23.24548731573063165, -27.04727666617280235, -38.41943903429619667 ) ) ;
#92748 = EDGE_CURVE ( 'NONE', #96544, #74990, #84862, .T. ) ;
#92749 = CARTESIAN_POINT ( 'NONE',  ( 42.15184130795574902, -60.00000000000000000, 55.41083953232990211 ) ) ;
#92750 = CARTESIAN_POINT ( 'NONE',  ( 27.02674341509898781, -30.42927322169125404, 39.08002995295369431 ) ) ;
#92751 = MECHANICAL_DESIGN_GEOMETRIC_PRESENTATION_REPRESENTATION (  '', ( #106527 ), #3219 ) ;
#92752 = CARTESIAN_POINT ( 'NONE',  ( 6.849999999999999645, 0.000000000000000000, 0.000000000000000000 ) ) ;
#92753 = CARTESIAN_POINT ( 'NONE',  ( 20.00000000000000000, 12.99999999999999289, 0.000000000000000000 ) ) ;
#92754 = AXIS2_PLACEMENT_3D ( 'NONE', #32798, #24184, #73210 ) ;
#92756 = CARTESIAN_POINT ( 'NONE',  ( -13.46110359768981368, 24.53700931164864230, -2.095215872004557944 ) ) ;
#92755 = CARTESIAN_POINT ( 'NONE',  ( -28.18961936475973573, -31.22569484158471909, 39.61244384221697601 ) ) ;
#92757 = CARTESIAN_POINT ( 'NONE',  ( 0.1244054282680990831, 295.1039052012444586, -9.999999999994756195 ) ) ;
#92758 = CARTESIAN_POINT ( 'NONE',  ( 34.95237279327285762, 304.8277712208536627, 12.26231981495593537 ) ) ;
#92759 = CONICAL_SURFACE ( 'NONE', #46271, 4.000000000000001776, 0.9599310885968808105 ) ;
#92760 = LINE ( 'NONE', #28071, #41400 ) ;
#92761 = ORIENTED_EDGE ( 'NONE', *, *, #20083, .T. ) ;
#92762 = CARTESIAN_POINT ( 'NONE',  ( 4.639619758717001829, -4.826867782832391818, -0.1499059597315433867 ) ) ;
#92763 = LINE ( 'NONE', #3231, #88901 ) ;
#92764 = FACE_OUTER_BOUND ( 'NONE', #13783, .T. ) ;
#92765 = DIRECTION ( 'NONE',  ( 0.000000000000000000, -1.000000000000000000, 0.000000000000000000 ) ) ;
#92768 = EDGE_CURVE ( 'NONE', #45425, #347, #19827, .T. ) ;
#92767 = CARTESIAN_POINT ( 'NONE',  ( 57.64153548184016529, -60.22831400432175286, -30.33932336446891753 ) ) ;
#92766 = CARTESIAN_POINT ( 'NONE',  ( 9.843039827103257977, 253.5908350250832939, -1.781495459429556893 ) ) ;
#92769 = ORIENTED_EDGE ( 'NONE', *, *, #62163, .F. ) ;
#92770 = CARTESIAN_POINT ( 'NONE',  ( -44.29577627588397348, 464.1408972797700585, 8.778647706801374184 ) ) ;
#92771 = DIRECTION ( 'NONE',  ( -1.000000000000000000, -1.224606353822377258E-16, -0.000000000000000000 ) ) ;
#92772 = CIRCLE ( 'NONE', #63545, 4.000000000000007105 ) ;
#92773 = VERTEX_POINT ( 'NONE', #51418 ) ;
#92774 = FACE_BOUND ( 'NONE', #6771, .T. ) ;
#92775 = VECTOR ( 'NONE', #23209, 1000.000000000000000 ) ;
#92776 = CARTESIAN_POINT ( 'NONE',  ( 34.35000000000000142, 3.309500000000003439, 4.052968581778167743E-16 ) ) ;
#92777 = DIRECTION ( 'NONE',  ( 1.000000000000000000, 0.000000000000000000, 0.000000000000000000 ) ) ;
#92778 = CARTESIAN_POINT ( 'NONE',  ( -92.23564407392396447, -60.00000000000000000, 2.399895685214207930 ) ) ;
#92779 = CARTESIAN_POINT ( 'NONE',  ( 67.96666666666666856, 6.915964383211875250E-15, 0.000000000000000000 ) ) ;
#92780 = CARTESIAN_POINT ( 'NONE',  ( 38.55382211449396834, 464.3891087764564531, 18.94281067283265330 ) ) ;
#92782 = CARTESIAN_POINT ( 'NONE',  ( 39.83854393463795418, 460.2189570659127753, 2.210463671043265244 ) ) ;
#92781 =( REPRESENTATION_RELATIONSHIP ('NONE','NONE', #69581, #533 ) REPRESENTATION_RELATIONSHIP_WITH_TRANSFORMATION ( #69694 )SHAPE_REPRESENTATION_RELATIONSHIP( ) );
#92783 = CARTESIAN_POINT ( 'NONE',  ( -2.617478844990583031, -3.000000000000002665, -94.73972676610416954 ) ) ;
#92784 = MECHANICAL_DESIGN_GEOMETRIC_PRESENTATION_REPRESENTATION (  '', ( #101422 ), #104805 ) ;
#92785 = CARTESIAN_POINT ( 'NONE',  ( -81.72239385450473037, -53.48791114501855049, 179.5194371415524870 ) ) ;
#92786 = ORIENTED_EDGE ( 'NONE', *, *, #21429, .F. ) ;
#92787 = CARTESIAN_POINT ( 'NONE',  ( -44.49963734947764493, 484.8409368627554272, 4.258617019824068706 ) ) ;
#92788 = ORIENTED_EDGE ( 'NONE', *, *, #69682, .F. ) ;
#92789 = ORIENTED_EDGE ( 'NONE', *, *, #41690, .T. ) ;
#92790 = FACE_OUTER_BOUND ( 'NONE', #43096, .T. ) ;
#92791 = CARTESIAN_POINT ( 'NONE',  ( 15.51786670351831354, -4.332661967059896035, 9.509450810727432923 ) ) ;
#92792 = EDGE_CURVE ( 'NONE', #43338, #88345, #19646, .T. ) ;
#92793 = CARTESIAN_POINT ( 'NONE',  ( 33.74271564777244237, 484.1802673187708592, 2.058285076122321922 ) ) ;
#92794 = ORIENTED_EDGE ( 'NONE', *, *, #82546, .T. ) ;
#92795 = CARTESIAN_POINT ( 'NONE',  ( -72.50181434431193850, -38.00000000001091394, -21.26203725901419261 ) ) ;
#92796 = CARTESIAN_POINT ( 'NONE',  ( 66.74444444444444002, 6.915964383211875250E-15, 0.000000000000000000 ) ) ;
#92797 = CARTESIAN_POINT ( 'NONE',  ( 7.744329845603314944, -13.46288230153455778, -2.018701143083234673 ) ) ;
#92798 = DIRECTION ( 'NONE',  ( 0.000000000000000000, -1.000000000000000000, 0.000000000000000000 ) ) ;
#92799 = FACE_OUTER_BOUND ( 'NONE', #12056, .T. ) ;
#92800 = PRESENTATION_STYLE_ASSIGNMENT (( #9738 ) ) ;
#92801 = CARTESIAN_POINT ( 'NONE',  ( -5.000000000000000000, -13.79686997522500036, 10.70729389128589659 ) ) ;
#92802 = CLOSED_SHELL ( 'NONE', ( #39739, #67399, #87719, #79664, #81102, #20850, #91919, #17828 ) ) ;
#92803 = CARTESIAN_POINT ( 'NONE',  ( 105.2982900294548614, -30.00000000000001066, 128.8790101386541096 ) ) ;
#92804 = EDGE_CURVE ( 'NONE', #91205, #26711, #13449, .T. ) ;
#92805 = CARTESIAN_POINT ( 'NONE',  ( -71.69513722905418263, -59.99999999999990763, 172.8795092261717912 ) ) ;
#92806 = CARTESIAN_POINT ( 'NONE',  ( -61.32617096396685952, -25.59081373081079747, 69.10494924817277251 ) ) ;
#92807 = VERTEX_POINT ( 'NONE', #13073 ) ;
#92808 = LINE ( 'NONE', #52342, #65915 ) ;
#92809 = ORIENTED_EDGE ( 'NONE', *, *, #25381, .T. ) ;
#92810 = CARTESIAN_POINT ( 'NONE',  ( -102.7692820952204045, -45.26544015360205009, 186.5759103958386333 ) ) ;
#92811 = PRESENTATION_STYLE_ASSIGNMENT (( #84727 ) ) ;
#92812 = CARTESIAN_POINT ( 'NONE',  ( -6.518108746679445176, 51.36497237057859166, 7.568279843509460925 ) ) ;
#92814 = CARTESIAN_POINT ( 'NONE',  ( 17.81438722625302518, 1.482358050883964840E-15, 0.000000000000000000 ) ) ;
#92813 = AXIS2_PLACEMENT_3D ( 'NONE', #91325, #106413, #16900 ) ;
#92815 = VERTEX_POINT ( 'NONE', #29318 ) ;
#92816 = CARTESIAN_POINT ( 'NONE',  ( 4.852941176470594975, -4.999999999999998224, -70.80672828634229177 ) ) ;
#92817 = CARTESIAN_POINT ( 'NONE',  ( -76.66120007774280509, -59.99999999999997868, 189.5221980919927489 ) ) ;
#92818 = CARTESIAN_POINT ( 'NONE',  ( -1.888159750444540430, -0.09357170100955422565, 101.9303315792851947 ) ) ;
#92819 = CARTESIAN_POINT ( 'NONE',  ( -1.320432766682874540E-15, -19.90625000204838457, 7.188101187500000044 ) ) ;
#92820 = EDGE_CURVE ( 'NONE', #5324, #41809, #67431, .T. ) ;
#92821 = CARTESIAN_POINT ( 'NONE',  ( -1.220317183347022771, 36.63139401606524359, -28.81440893545308768 ) ) ;
#92822 = DIRECTION ( 'NONE',  ( 0.000000000000000000, 1.000000000000000000, 0.000000000000000000 ) ) ;
#92823 = CARTESIAN_POINT ( 'NONE',  ( 6.928203230275508773, -84.73069070304464390, -4.000000000000001776 ) ) ;
#92824 = DIRECTION ( 'NONE',  ( -0.000000000000000000, 1.000000000000000000, -0.000000000000000000 ) ) ;
#92825 = CARTESIAN_POINT ( 'NONE',  ( -9.215420734788356327, -54.00000000000001421, 23.11721482942554928 ) ) ;
#92826 = CARTESIAN_POINT ( 'NONE',  ( -29.71626147859926448, -25.59364090554883120, 30.54361049305994058 ) ) ;
#92827 = LINE ( 'NONE', #75584, #100702 ) ;
#92828 = CARTESIAN_POINT ( 'NONE',  ( 45.67906931825459793, -56.80297510144281858, 49.30526560711538053 ) ) ;
#92829 = CARTESIAN_POINT ( 'NONE',  ( -31.96724538747962896, 486.9512181893487082, 7.078368790597582283 ) ) ;
#92830 =( GEOMETRIC_REPRESENTATION_CONTEXT ( 3 ) GLOBAL_UNCERTAINTY_ASSIGNED_CONTEXT ( ( #46405 ) ) GLOBAL_UNIT_ASSIGNED_CONTEXT ( ( #3078, #9557, #68355 ) ) REPRESENTATION_CONTEXT ( 'NONE', 'WORKASPACE' ) );
#92831 = CARTESIAN_POINT ( 'NONE',  ( -6.943482370013980720, 85.52848370260727506, 3.973876482044367275 ) ) ;
#92832 = CARTESIAN_POINT ( 'NONE',  ( -95.43172166446088056, -38.48744210534112398, 201.2268467534914862 ) ) ;
#92833 = ORIENTED_EDGE ( 'NONE', *, *, #106174, .T. ) ;
#92835 = CARTESIAN_POINT ( 'NONE',  ( 0.000000000000000000, 0.000000000000000000, 0.000000000000000000 ) ) ;
#92834 = DIRECTION ( 'NONE',  ( -1.000000000000000000, -1.224606353822377258E-16, -0.000000000000000000 ) ) ;
#92836 = CARTESIAN_POINT ( 'NONE',  ( 62.91912717164011326, -60.00000000000000000, 90.67547237248358272 ) ) ;
#92837 = CARTESIAN_POINT ( 'NONE',  ( -48.90253429252444306, 9.379793601652298918, -14.70143532337769088 ) ) ;
#92838 = CARTESIAN_POINT ( 'NONE',  ( -7.493767324785338246, 40.39058438512729055, -59.41312847858032598 ) ) ;
#92839 = COLOUR_RGB ( '', 0.40784314, 0.44705882, 0.49803922) ;
#92840 = CARTESIAN_POINT ( 'NONE',  ( 9.999999999999998224, 15.11603512202947108, -0.3498606326598576177 ) ) ;
#92841 = CARTESIAN_POINT ( 'NONE',  ( 44.83349330513380693, 1.593028355512270567E-15, 0.000000000000000000 ) ) ;
#92842 = LINE ( 'NONE', #60510, #20796 ) ;
#92843 = CARTESIAN_POINT ( 'NONE',  ( 0.000000000000000000, 4.898587196589413815E-16, -4.000000000000000888 ) ) ;
#92844 = CARTESIAN_POINT ( 'NONE',  ( 112.0489445181305683, -60.00000000000000000, 179.0880007768037103 ) ) ;
#92845 = CARTESIAN_POINT ( 'NONE',  ( 6.333820801331439654, -6.982605850969140882, 0.9057718968901056211 ) ) ;
#92846 = CARTESIAN_POINT ( 'NONE',  ( 6.400000000000000355, 4.618802153517005848, 7.999999999999996447 ) ) ;
#92847 = EDGE_LOOP ( 'NONE', ( #73019, #25258, #83945, #29567, #100669 ) ) ;
#92848 = EDGE_CURVE ( 'NONE', #38206, #42880, #34730, .T. ) ;
#92849 = AXIS2_PLACEMENT_3D ( 'NONE', #104583, #4306, #62553 ) ;
#92850 = CARTESIAN_POINT ( 'NONE',  ( -81.23169817918467572, -30.00000000000000000, 0.5271219704189816779 ) ) ;
#92851 = VERTEX_POINT ( 'NONE', #6576 ) ;
#92853 = CARTESIAN_POINT ( 'NONE',  ( 0.000000000000000000, 0.000000000000000000, 5.000000000000000888 ) ) ;
#92852 = CARTESIAN_POINT ( 'NONE',  ( -77.60330327168814790, -38.52455064180648492, 186.9244840374806813 ) ) ;
#92854 = DIRECTION ( 'NONE',  ( -1.000000000000000000, -1.224606353822377258E-16, -0.000000000000000000 ) ) ;
#92855 = CARTESIAN_POINT ( 'NONE',  ( 7.188101187500001821, -20.93750000204838457, -2.977408999572650483 ) ) ;
#92856 = LINE ( 'NONE', #101495, #43372 ) ;
#92857 = EDGE_CURVE ( 'NONE', #44273, #17408, #87978, .T. ) ;
#92858 = CIRCLE ( 'NONE', #75614, 4.000000000000000888 ) ;
#92859 = CARTESIAN_POINT ( 'NONE',  ( 30.90663305326217980, 14.69720259819713171, -40.57123681776414514 ) ) ;
#92860 = AXIS2_PLACEMENT_3D ( 'NONE', #46136, #96290, #22415 ) ;
#92862 = ORIENTED_EDGE ( 'NONE', *, *, #96316, .F. ) ;
#92861 = DIRECTION ( 'NONE',  ( 0.000000000000000000, 0.000000000000000000, 1.000000000000000000 ) ) ;
#92863 = CARTESIAN_POINT ( 'NONE',  ( 80.46043862466507335, -53.38907585616056650, 168.0494285789779383 ) ) ;
#92864 = DIRECTION ( 'NONE',  ( -0.5735764363510510444, -0.8191520442889883569, 0.000000000000000000 ) ) ;
#92865 = CARTESIAN_POINT ( 'NONE',  ( 6.270061300899935297, -4.268872906156522262, -6.443866470201764507 ) ) ;
#92866 = ORIENTED_EDGE ( 'NONE', *, *, #104539, .F. ) ;
#92867 = CARTESIAN_POINT ( 'NONE',  ( -32.86259851300448531, 485.9239370913668381, 5.440925357813682695 ) ) ;
#92868 = CARTESIAN_POINT ( 'NONE',  ( -31.86888217434299264, 485.1577972469723363, 5.527887721100189999 ) ) ;
#92869 = CARTESIAN_POINT ( 'NONE',  ( 38.54613318107097797, 27.49665781920858265, -11.41323020553166856 ) ) ;
#92870 = DIRECTION ( 'NONE',  ( -1.000000000000000000, -1.224606353822377258E-16, -0.000000000000000000 ) ) ;
#92871 = CARTESIAN_POINT ( 'NONE',  ( -5.725989721596485005, 253.5767711125646713, 1.809923354557167352 ) ) ;
#92872 = CARTESIAN_POINT ( 'NONE',  ( 17.40520516324947309, 43.24891479535327932, 6.413032873378024412 ) ) ;
#92873 = B_SPLINE_SURFACE_WITH_KNOTS ( 'NONE', 3, 3, ( 
 ( #96217, #61738, #39038, #37477, #87590, #103761, #70869, #71922 ),
 ( #95153, #62269, #13675, #4534, #87064, #20780, #46584, #88120 ),
 ( #29898, #29383, #86549, #70341, #30969, #103237, #63848, #79482 ),
 ( #21286, #94634, #53614, #5594, #46066, #78950, #30427, #71380 ),
 ( #104281, #22346, #55191, #14200, #117, #74037, #72965, #640 ),
 ( #16885, #41154, #33088, #8774, #105872, #97777, #57312, #82124 ),
 ( #24989, #90231, #23397, #89174, #7174, #40088, #89708, #88639 ),
 ( #15806, #56238, #105356, #40612, #33607, #48688, #16336, #24476 ) ),
 .UNSPECIFIED., .F., .F., .F.,
 ( 4, 2, 2, 4 ),
 ( 4, 2, 2, 4 ),
 ( 0.000000000000000000, 0.2500000000000000000, 0.5000000000000000000, 1.000000000000000000 ),
 ( 0.000000000000000000, 0.2500000000000000000, 0.5000000000000000000, 1.000000000000000000 ),
 .UNSPECIFIED. ) ;
#92874 = CARTESIAN_POINT ( 'NONE',  ( -27.99999999999999645, 1.836970198721029589E-15, -15.00000000000000000 ) ) ;
#92875 = EDGE_CURVE ( 'NONE', #70548, #77685, #29580, .T. ) ;
#92876 = ORIENTED_EDGE ( 'NONE', *, *, #89960, .T. ) ;
#92877 = CIRCLE ( 'NONE', #20653, 4.172000000000001485 ) ;
#92878 = CARTESIAN_POINT ( 'NONE',  ( 16.84999999999999787, -3.309499999999999886, 0.000000000000000000 ) ) ;
#92880 = PRESENTATION_STYLE_ASSIGNMENT (( #84266 ) ) ;
#92879 =( BOUNDED_CURVE ( )  B_SPLINE_CURVE ( 2, ( #13002, #44334, #95025, #78807, #102570, #69155, #45928, #85877, #77228 ),
 .UNSPECIFIED., .F., .F. ) 
 B_SPLINE_CURVE_WITH_KNOTS ( ( 3, 2, 2, 2, 3 ),
 ( 0.2205882352941176960, 0.2279411764705882859, 0.2352941176470588758, 0.2426470588235294656, 0.2500000000000000555 ),
 .UNSPECIFIED. ) 
 CURVE ( )  GEOMETRIC_REPRESENTATION_ITEM ( )  RATIONAL_B_SPLINE_CURVE ( ( 0.9999999999999994449, 0.9238795325112872936, 1.000000000000000000, 0.9238795325112867385, 1.000000000000000000, 0.9238795325112867385, 1.000000000000000000, 0.9238795325112861834, 1.000000000000000666 ) ) 
 REPRESENTATION_ITEM ( '' )  );
#92882 = ADVANCED_FACE ( 'NONE', ( #78882 ), #26124, .T. ) ;
#92881 = CARTESIAN_POINT ( 'NONE',  ( 14.86288555396978062, 23.03472989906422086, 1.260572299733986101 ) ) ;
#92883 = LINE ( 'NONE', #19047, #24229 ) ;
#92884 = TOROIDAL_SURFACE ( 'NONE', #13658, 2.000000000000011102, 5.000000000000000000 ) ;
#92885 = CARTESIAN_POINT ( 'NONE',  ( -1.320432766682874540E-15, -27.03125000204838813, 7.188101187500000044 ) ) ;
#92886 = DIRECTION ( 'NONE',  ( -0.5000000000000011102, -0.8660254037844380415, 0.000000000000000000 ) ) ;
#92887 = CARTESIAN_POINT ( 'NONE',  ( 9.797174393178825657E-16, -30.00000000000000000, -8.000000000000000000 ) ) ;
#92888 = CIRCLE ( 'NONE', #6740, 5.000000000000010658 ) ;
#92889 = CARTESIAN_POINT ( 'NONE',  ( 14.84266821126072777, 4.606643506668125276, 5.685020543978089869 ) ) ;
#92890 = CONTEXT_DEPENDENT_SHAPE_REPRESENTATION ( #19768, #13067 ) ;
#92891 = ORIENTED_EDGE ( 'NONE', *, *, #9553, .F. ) ;
#92892 = LINE ( 'NONE', #43285, #52633 ) ;
#92893 =( LENGTH_UNIT ( ) NAMED_UNIT ( * ) SI_UNIT ( .MILLI., .METRE. ) );
#92894 = CARTESIAN_POINT ( 'NONE',  ( -9.999565592957996074, 7.500620397551100105, -4.999999999999999112 ) ) ;
#92895 = CARTESIAN_POINT ( 'NONE',  ( 56.22793774957824553, -4.000000000000000888, 4.898587196589422689E-16 ) ) ;
#92896 = ORIENTED_EDGE ( 'NONE', *, *, #29334, .F. ) ;
#92897 = CARTESIAN_POINT ( 'NONE',  ( -7.576492623273555438, 51.95166532205756482, -3.569847711208139707 ) ) ;
#92898 = CARTESIAN_POINT ( 'NONE',  ( -4.707696486720360340, 49.99999999999999289, -99.43546650844932344 ) ) ;
#92899 = CIRCLE ( 'NONE', #22345, 4.172000000000009479 ) ;
#92900 = CARTESIAN_POINT ( 'NONE',  ( 32.37381880833165582, 435.2096513840866692, 18.54399430281184635 ) ) ;
#92901 = CARTESIAN_POINT ( 'NONE',  ( -1.115712391155330829, 9.312447554110960368, -51.08064749475159516 ) ) ;
#92902 = CARTESIAN_POINT ( 'NONE',  ( 0.000000000000000000, -14.49999999999999822, -8.500000000000000000 ) ) ;
#92903 = CARTESIAN_POINT ( 'NONE',  ( 36.35697729507720766, 25.99969806902772262, 12.56106323611688502 ) ) ;
#92904 = CARTESIAN_POINT ( 'NONE',  ( -108.2689893803878363, -60.00000000000000000, 195.1503591843108723 ) ) ;
#92905 = AXIS2_PLACEMENT_3D ( 'NONE', #91203, #33491, #65316 ) ;
#92906 = CARTESIAN_POINT ( 'NONE',  ( 19.13866731016917910, 49.71730248559679666, 61.67331676224903703 ) ) ;
#92907 = CARTESIAN_POINT ( 'NONE',  ( -45.29905483860081716, 480.9466865490944656, -2.171671249451534003 ) ) ;
#92908 =( LENGTH_UNIT ( ) NAMED_UNIT ( * ) SI_UNIT ( .MILLI., .METRE. ) );
#92909 = FILL_AREA_STYLE_COLOUR ( '', #47341 ) ;
#92910 = CARTESIAN_POINT ( 'NONE',  ( -84.10481117900889103, -46.56341232157270582, 184.9836422536479006 ) ) ;
#92911 = FILL_AREA_STYLE_COLOUR ( '', #33301 ) ;
#92912 = ORIENTED_EDGE ( 'NONE', *, *, #72195, .F. ) ;
#92913 = CARTESIAN_POINT ( 'NONE',  ( 8.000000000000000000, -25.99999999999999645, 0.000000000000000000 ) ) ;
#92914 = ADVANCED_FACE ( 'NONE', ( #71846 ), #70801, .T. ) ;
#92915 = CARTESIAN_POINT ( 'NONE',  ( 4.245164436742090430, -1.071807799196438316, 104.4592797835113061 ) ) ;
#92916 = CARTESIAN_POINT ( 'NONE',  ( -82.45168481354632206, -37.83267541790726796, 9.374888728109986857 ) ) ;
#92917 = AXIS2_PLACEMENT_3D ( 'NONE', #20837, #103809, #61795 ) ;
#92918 = DIRECTION ( 'NONE',  ( -1.000000000000000000, -0.000000000000000000, -0.000000000000000000 ) ) ;
#92919 = EDGE_CURVE ( 'NONE', #22823, #19286, #104752, .T. ) ;
#92920 = EDGE_LOOP ( 'NONE', ( #86241, #104875, #45207, #84158, #43754 ) ) ;
#92921 = CARTESIAN_POINT ( 'NONE',  ( -6.999999999999975131, -12.54465221550630183, 8.223849511754991681 ) ) ;
#92922 = DIRECTION ( 'NONE',  ( 0.000000000000000000, 0.000000000000000000, -1.000000000000000000 ) ) ;
#92923 = CARTESIAN_POINT ( 'NONE',  ( 72.41885610122542971, 42.00000000000000000, -55.65414010180089832 ) ) ;
#92924 = EDGE_CURVE ( 'NONE', #54950, #106205, #30360, .T. ) ;
#92925 = CARTESIAN_POINT ( 'NONE',  ( 66.35352848486118660, -59.99999999999995737, 134.7740243497364645 ) ) ;
#92926 = PRESENTATION_LAYER_ASSIGNMENT (  '', '', ( #20636 ) ) ;
#92927 =( LENGTH_UNIT ( ) NAMED_UNIT ( * ) SI_UNIT ( .MILLI., .METRE. ) );
#92928 = EDGE_CURVE ( 'NONE', #29837, #97818, #39076, .T. ) ;
#92929 = CARTESIAN_POINT ( 'NONE',  ( -87.61621634008581339, -14.21045842199436571, -10.69165924380367372 ) ) ;
#92930 = CARTESIAN_POINT ( 'NONE',  ( -74.24509999404291705, -49.90998642872604307, 125.1187655734622126 ) ) ;
#92931 = ORIENTED_EDGE ( 'NONE', *, *, #82009, .F. ) ;
#92932 = CARTESIAN_POINT ( 'NONE',  ( 74.93436731647082638, -29.99999999999996803, 156.1785850212263824 ) ) ;
#92933 = CARTESIAN_POINT ( 'NONE',  ( 64.91136071154012654, 40.83917339310983863, 6.834607325964931590 ) ) ;
#92934 = CARTESIAN_POINT ( 'NONE',  ( 84.62951063988832345, -57.67093676639928645, -27.31841214351725355 ) ) ;
#92935 = ORIENTED_EDGE ( 'NONE', *, *, #65982, .F. ) ;
#92936 = CARTESIAN_POINT ( 'NONE',  ( 7.806021097029844036, 51.84152802710514862, -3.791216216185762988 ) ) ;
#92937 = CARTESIAN_POINT ( 'NONE',  ( -2.977408999572654480, -24.50000000204839168, 7.188101187499999156 ) ) ;
#92938 = STYLED_ITEM ( 'NONE', ( #86490 ), #32241 ) ;
#92939 = EDGE_CURVE ( 'NONE', #86174, #103837, #31461, .T. ) ;
#92940 = CARTESIAN_POINT ( 'NONE',  ( -5.191472769733075587, -7.359084232810527482, -3.014900733016758760 ) ) ;
#92941 = EDGE_LOOP ( 'NONE', ( #1286, #6955 ) ) ;
#92942 = DIRECTION ( 'NONE',  ( 0.000000000000000000, 0.000000000000000000, -1.000000000000000000 ) ) ;
#92943 = ORIENTED_EDGE ( 'NONE', *, *, #863, .T. ) ;
#92944 = CARTESIAN_POINT ( 'NONE',  ( -1.735558044533041189, 41.99999999999999289, -69.74083754112251654 ) ) ;
#92945 = DIRECTION ( 'NONE',  ( 0.000000000000000000, 0.8299985787540355986, -0.5577655056260480970 ) ) ;
#92946 = CARTESIAN_POINT ( 'NONE',  ( -53.16843670460360016, -59.99999999999020872, 87.15546671691542713 ) ) ;
#92947 = CARTESIAN_POINT ( 'NONE',  ( -11.39536947849075688, 43.21380559344856920, 14.75801218667085912 ) ) ;
#92948 = CARTESIAN_POINT ( 'NONE',  ( -7.188101187500001821, -14.00000000204838457, -2.977408999572651371 ) ) ;
#92949 = ADVANCED_FACE ( 'NONE', ( #49153 ), #26786, .F. ) ;
#92950 = EDGE_CURVE ( 'NONE', #62030, #63004, #69140, .T. ) ;
#92951 = DIRECTION ( 'NONE',  ( 1.000000000000000000, 0.000000000000000000, 0.000000000000000000 ) ) ;
#92952 = DIRECTION ( 'NONE',  ( -1.000000000000000000, -0.000000000000000000, -0.000000000000000000 ) ) ;
#92953 = CARTESIAN_POINT ( 'NONE',  ( 37.96538461538461462, 1.411358822780289120E-15, 0.000000000000000000 ) ) ;
#92954 = CARTESIAN_POINT ( 'NONE',  ( 9.596002107493083244, 50.00000000000000000, -92.37456064097861486 ) ) ;
#92955 = CARTESIAN_POINT ( 'NONE',  ( -12.48764691435734875, -3.515361478854691857, -13.73627036880986019 ) ) ;
#92956 =( NAMED_UNIT ( * ) PLANE_ANGLE_UNIT ( ) SI_UNIT ( $, .RADIAN. ) );
#92957 = UNCERTAINTY_MEASURE_WITH_UNIT (LENGTH_MEASURE( 1.000000000000000082E-05 ), #44299, 'distance_accuracy_value', 'NONE');
#92958 = VECTOR ( 'NONE', #55192, 1000.000000000000114 ) ;
#92959 = ORIENTED_EDGE ( 'NONE', *, *, #68620, .T. ) ;
#92961 = CARTESIAN_POINT ( 'NONE',  ( 32.12746647248193455, -42.96020264381913734, 34.58970033397424260 ) ) ;
#92960 = CARTESIAN_POINT ( 'NONE',  ( -3.384215095276469132, -49.13301901873835220, 104.0501775326191876 ) ) ;
#92962 = CARTESIAN_POINT ( 'NONE',  ( -5.820808985964939453, -8.673617379884035472E-16, 21.65942590380532451 ) ) ;
#92963 = VERTEX_POINT ( 'NONE', #77174 ) ;
#92964 = CARTESIAN_POINT ( 'NONE',  ( 6.123233995736763324E-16, 48.00000000000000000, -95.00000000000000000 ) ) ;
#92965 = AXIS2_PLACEMENT_3D ( 'NONE', #57931, #41756, #33693 ) ;
#92966 = ORIENTED_EDGE ( 'NONE', *, *, #3037, .F. ) ;
#92967 = PRESENTATION_STYLE_ASSIGNMENT (( #8851 ) ) ;
#92968 = DIRECTION ( 'NONE',  ( 0.000000000000000000, 0.000000000000000000, -1.000000000000000000 ) ) ;
#92969 = CARTESIAN_POINT ( 'NONE',  ( 0.9999999999999956701, -4.000000000000000000, 42.58845726811989607 ) ) ;
#92970 = B_SPLINE_CURVE_WITH_KNOTS ( 'NONE', 3,
 ( #3374, #10382, #77796, #3907, #36839, #101537, #11438, #52435, #77261, #19068, #51909, #92901, #1754, #100996, #76183, #43299, #50834, #84822, #10902, #34711, #43821, #75652, #2282, #26623, #36317, #93456, #69706, #2824 ),
 .UNSPECIFIED., .F., .F.,
 ( 4, 2, 2, 2, 2, 2, 2, 2, 2, 2, 2, 2, 2, 4 ),
 ( 0.01419955293336414015, 0.01443026280088062670, 0.01466097266839711498, 0.01512239240343009848, 0.01558381213846308198, 0.01604523187349606722, 0.01696807134356204116, 0.01789091081362801858, 0.01881375028369399252, 0.01973658975375996993, 0.02019800948879296038, 0.02065942922382595082, 0.02112084895885894473, 0.02158226869389193517 ),
 .UNSPECIFIED. ) ;
#92971 = CARTESIAN_POINT ( 'NONE',  ( 0.000000000000000000, 115.0000000000000000, -10.00000000000000000 ) ) ;
#92972 = CARTESIAN_POINT ( 'NONE',  ( 57.45015997180046696, -4.000000000000000888, 4.898587196589422689E-16 ) ) ;
#92973 = ORIENTED_EDGE ( 'NONE', *, *, #23528, .F. ) ;
#92974 = VECTOR ( 'NONE', #80171, 1000.000000000000000 ) ;
#92975 = CARTESIAN_POINT ( 'NONE',  ( 92.55954463226689199, -60.00000000000000000, -10.73077478005948926 ) ) ;
#92976 = FACE_OUTER_BOUND ( 'NONE', #55477, .T. ) ;
#92977 = DIRECTION ( 'NONE',  ( 0.000000000000000000, 0.000000000000000000, 1.000000000000000000 ) ) ;
#92978 = CARTESIAN_POINT ( 'NONE',  ( 37.50059943756144776, 490.7879993827856993, 12.38039871356534505 ) ) ;
#92979 = CARTESIAN_POINT ( 'NONE',  ( -6.238184438393528986, 40.55825027053369070, -71.19044207184282413 ) ) ;
#92980 = CARTESIAN_POINT ( 'NONE',  ( 10.59999999999999609, 1.533819458162526451E-15, 0.000000000000000000 ) ) ;
#92981 = ORIENTED_EDGE ( 'NONE', *, *, #73938, .F. ) ;
#92982 = B_SPLINE_CURVE_WITH_KNOTS ( 'NONE', 3,
 ( #52074, #37004, #84989, #28380, #87125, #2459, #13202, #68822, #20844, #93619, #53159, #45606, #61255, #94141, #35950, #12673, #60211, #43996, #20311, #4607 ),
 .UNSPECIFIED., .F., .F.,
 ( 4, 2, 2, 2, 2, 2, 2, 2, 2, 4 ),
 ( 0.007651485924207266677, 0.008155685132977938748, 0.008659884341748609951, 0.009164083550519281154, 0.009668282759289954092, 0.01017248196806062877, 0.01067668117683130344, 0.01092878078121663904, 0.01118088038560197638, 0.01168507959437264758 ),
 .UNSPECIFIED. ) ;
#92983 = CARTESIAN_POINT ( 'NONE',  ( -105.2209555712209976, -30.00000000000275691, 195.0728638946999638 ) ) ;
#92984 = ORIENTED_EDGE ( 'NONE', *, *, #61426, .T. ) ;
#92985 = ORIENTED_EDGE ( 'NONE', *, *, #55610, .F. ) ;
#92986 = CARTESIAN_POINT ( 'NONE',  ( 30.00000000000000000, 0.000000000000000000, 0.000000000000000000 ) ) ;
#92987 = CARTESIAN_POINT ( 'NONE',  ( 6.333820801330213968, -6.982605850969823891, -0.9057718968899813872 ) ) ;
#92988 = CARTESIAN_POINT ( 'NONE',  ( 7.914973979435151463, 3.817460047930442357, -7.907502498112419786 ) ) ;
#92989 = CARTESIAN_POINT ( 'NONE',  ( 84.67034172243197077, -52.74716631599819294, -13.90098049673125047 ) ) ;
#92990 = CARTESIAN_POINT ( 'NONE',  ( -32.71417592245104800, 313.0749680721571622, -7.579415757426488653 ) ) ;
#92991 = CARTESIAN_POINT ( 'NONE',  ( 16.64348903516512834, 45.88445698070336931, -4.157797401561768247 ) ) ;
#92992 = AXIS2_PLACEMENT_3D ( 'NONE', #23403, #90238, #56247 ) ;
#92993 = CARTESIAN_POINT ( 'NONE',  ( -17.91081636847285807, 45.00000000000001421, 62.63222563193455983 ) ) ;
#92994 = DIRECTION ( 'NONE',  ( -1.000000000000000000, -1.224606353822377258E-16, -0.000000000000000000 ) ) ;
#92995 = EDGE_LOOP ( 'NONE', ( #91298, #45253, #80015, #63965, #15637, #30590 ) ) ;
#92997 = EDGE_CURVE ( 'NONE', #62818, #47025, #90446, .T. ) ;
#92996 = CARTESIAN_POINT ( 'NONE',  ( -6.826296012759263121, -2.664253980648909614, -6.325071479459888124 ) ) ;
#92998 = ORIENTED_EDGE ( 'NONE', *, *, #94779, .F. ) ;
#92999 = SURFACE_STYLE_USAGE ( .BOTH. , #27249 ) ;
#93000 = DIRECTION ( 'NONE',  ( 0.000000000000000000, -0.9584033143583334802, 0.2854173908978941965 ) ) ;
#93001 = EDGE_CURVE ( 'NONE', #49207, #98370, #83648, .T. ) ;
#93003 = VERTEX_POINT ( 'NONE', #27604 ) ;
#93002 = CARTESIAN_POINT ( 'NONE',  ( 12.50000000000000000, -2.999999999999996891, -14.34180675897363955 ) ) ;
#93004 = CARTESIAN_POINT ( 'NONE',  ( 71.58615475096345904, -60.32492746567568531, 120.7698757878210500 ) ) ;
#93005 = ORIENTED_EDGE ( 'NONE', *, *, #91953, .T. ) ;
#93006 = CARTESIAN_POINT ( 'NONE',  ( 3.733302338951465682, -48.92326939679833231, 43.79944126545571237 ) ) ;
#93007 = DIRECTION ( 'NONE',  ( 0.000000000000000000, 0.8660254037844381525, -0.5000000000000009992 ) ) ;
#93008 = CARTESIAN_POINT ( 'NONE',  ( -5.082755093536325042, -24.59375000204838813, -5.082755093536325930 ) ) ;
#93009 = CARTESIAN_POINT ( 'NONE',  ( -94.01586347659660703, -57.67588051021766660, 5.310313041227479935 ) ) ;
#93010 = VERTEX_POINT ( 'NONE', #18975 ) ;
#93011 = SURFACE_SIDE_STYLE ('',( #68205 ) ) ;
#93012 = DIRECTION ( 'NONE',  ( -1.000000000000000000, 0.000000000000000000, 0.000000000000000000 ) ) ;
#93013 = CONICAL_SURFACE ( 'NONE', #37917, 3.309500000000001663, 0.9599310885968770357 ) ;
#93014 = CARTESIAN_POINT ( 'NONE',  ( 101.7586560006743213, -37.84847941927726822, 185.3643445841708797 ) ) ;
#93015 = CARTESIAN_POINT ( 'NONE',  ( -29.68315524077005207, 13.47185074185902209, -42.10535821593474282 ) ) ;
#93016 = EDGE_CURVE ( 'NONE', #20894, #34743, #85292, .T. ) ;
#93017 = CARTESIAN_POINT ( 'NONE',  ( 48.69302668856813909, 13.59112006857157162, -16.66703530934498900 ) ) ;
#93018 = CARTESIAN_POINT ( 'NONE',  ( 4.898587196589412829E-16, -16.81250000409677270, -8.000000000000000000 ) ) ;
#93019 = CARTESIAN_POINT ( 'NONE',  ( -51.68662921661150023, -29.93083927907686004, 49.51763535396641913 ) ) ;
#93020 = CARTESIAN_POINT ( 'NONE',  ( 9.646083234704185827, 246.9870939097651785, -2.643797197754298889 ) ) ;
#93021 = EDGE_CURVE ( 'NONE', #18245, #14702, #12419, .T. ) ;
#93022 = CARTESIAN_POINT ( 'NONE',  ( -36.74148664940358344, 437.9559008978174575, 4.252305828303493129 ) ) ;
#93023 = CARTESIAN_POINT ( 'NONE',  ( 10.50000000000000178, -5.000000000000000000, -12.52300748975612166 ) ) ;
#93024 = DIRECTION ( 'NONE',  ( -1.000000000000000000, -4.493451613004637105E-20, 9.836563810793380808E-22 ) ) ;
#93025 = CARTESIAN_POINT ( 'NONE',  ( 33.78656477175017869, 463.8460037827032352, 7.347243016399514381 ) ) ;
#93026 = ORIENTED_EDGE ( 'NONE', *, *, #17401, .F. ) ;
#93027 = CARTESIAN_POINT ( 'NONE',  ( 43.63899620156485781, 434.3182181978398830, 14.37213632273147290 ) ) ;
#93028 = CONICAL_SURFACE ( 'NONE', #49981, 4.000000000000001776, 0.9599310885968808105 ) ;
#93029 = FILL_AREA_STYLE ('',( #3495 ) ) ;
#93031 = CARTESIAN_POINT ( 'NONE',  ( 1.248957290998449210, 10.99524951701871878, 50.37123180686704416 ) ) ;
#93030 =( BOUNDED_SURFACE ( )  B_SPLINE_SURFACE ( 3, 2, ( 
 ( #66774, #25834, #75382 ),
 ( #2553, #85084, #100196 ),
 ( #17699, #51639, #10122 ),
 ( #68916, #27958, #60821 ) ),
 .UNSPECIFIED., .F., .F., .F. ) 
 B_SPLINE_SURFACE_WITH_KNOTS ( ( 4, 4 ),
 ( 3, 3 ),
 ( 0.05672608053137292994, 0.08145892399347254287 ),
 ( 0.3700819440699701923, 1.000000000000000000 ),
 .UNSPECIFIED. ) 
 GEOMETRIC_REPRESENTATION_ITEM ( )  RATIONAL_B_SPLINE_SURFACE ( (
 ( 0.8634409826472493332, 0.8155016482958543644, 1.000000000000000000),
 ( 0.8634411984245984328, 0.8155019398223021243, 1.000000000000000000),
 ( 0.8634411456911572635, 0.8155018685766739495, 1.000000000000000000),
 ( 0.8634409290728097819, 0.8155015759139936371, 1.000000000000000000) ) ) 
 REPRESENTATION_ITEM ( '' )  SURFACE ( )  );
#93032 = STYLED_ITEM ( 'NONE', ( #95762 ), #49080 ) ;
#93033 = CARTESIAN_POINT ( 'NONE',  ( -89.02983586496698365, -30.00000000000000355, 188.7461324850866902 ) ) ;
#93034 = B_SPLINE_CURVE_WITH_KNOTS ( 'NONE', 3,
 ( #88713, #72516, #22416, #39112, #79550, #14805, #96291, #5662, #13742, #21355 ),
 .UNSPECIFIED., .F., .F.,
 ( 4, 2, 2, 2, 4 ),
 ( 0.000000000000000000, 0.5000000000000000000, 0.7500000000000000000, 0.8750000000000000000, 1.000000000000000000 ),
 .UNSPECIFIED. ) ;
#93035 = VERTEX_POINT ( 'NONE', #54452 ) ;
#93036 = VECTOR ( 'NONE', #45806, 1000.000000000000000 ) ;
#93037 = CARTESIAN_POINT ( 'NONE',  ( 38.17883673876440298, 25.52816737538899261, -11.10479361635789175 ) ) ;
#93038 = CARTESIAN_POINT ( 'NONE',  ( 86.13252104161762190, -57.57606074614650993, 202.7608471217752140 ) ) ;
#93040 = DIRECTION ( 'NONE',  ( 0.000000000000000000, -1.000000000000000000, 0.000000000000000000 ) ) ;
#93039 =( NAMED_UNIT ( * ) SI_UNIT ( $, .STERADIAN. ) SOLID_ANGLE_UNIT ( ) );
#93042 = CARTESIAN_POINT ( 'NONE',  ( 38.01963658391477452, -32.32223440244047197, -37.62936076183553524 ) ) ;
#93041 = CONICAL_SURFACE ( 'NONE', #72403, 5.000000000000001776, 0.9599310885968803664 ) ;
#93043 = CARTESIAN_POINT ( 'NONE',  ( 9.500000000000007105, -5.000000000000000000, -52.94236561372729000 ) ) ;
#93044 = LINE ( 'NONE', #86039, #73577 ) ;
#93045 = CARTESIAN_POINT ( 'NONE',  ( -35.97666713092540647, -60.00000000000000711, 47.32977935146745097 ) ) ;
#93046 = AXIS2_PLACEMENT_3D ( 'NONE', #92969, #67109, #101059 ) ;
#93047 = FILL_AREA_STYLE ('',( #18658 ) ) ;
#93048 = CIRCLE ( 'NONE', #25886, 4.172000000000001485 ) ;
#93049 = CARTESIAN_POINT ( 'NONE',  ( -28.89099332390824770, 48.00000000000000000, 58.53034795347328867 ) ) ;
#93050 = CARTESIAN_POINT ( 'NONE',  ( -86.18659369993858377, -42.85476313570202933, 188.6125987248406659 ) ) ;
#93051 = ORIENTED_EDGE ( 'NONE', *, *, #74780, .T. ) ;
#93052 = CARTESIAN_POINT ( 'NONE',  ( 36.64546344323804306, 438.4369965796255997, 4.168996892756918093 ) ) ;
#93053 = CARTESIAN_POINT ( 'NONE',  ( -2.979541785652459751, -22.06772564117152058, 27.56319171407887936 ) ) ;
#93054 = CARTESIAN_POINT ( 'NONE',  ( -41.57463013743633695, 490.5138136697628397, 10.95472345905721312 ) ) ;
#93056 = CARTESIAN_POINT ( 'NONE',  ( -46.00000000000000000, 500.0000000000002274, 0.000000000000000000 ) ) ;
#93055 = CARTESIAN_POINT ( 'NONE',  ( -40.35833863900601415, 321.1205797084799656, 8.337674143375151559 ) ) ;
#93057 = EDGE_LOOP ( 'NONE', ( #35856, #99893, #22795, #19890, #11837, #86763, #106649, #82348, #60977, #7385 ) ) ;
#93058 = CARTESIAN_POINT ( 'NONE',  ( 2.979761111870779223E-15, 34.19642918197134662, 12.16579798332631412 ) ) ;
#93059 = CARTESIAN_POINT ( 'NONE',  ( 39.41037217365025214, 489.7138547546053928, 11.67903818732042431 ) ) ;
#93060 = ADVANCED_FACE ( 'NONE', ( #79288 ), #98440, .T. ) ;
#93061 = DIRECTION ( 'NONE',  ( -0.2230022920435996703, -0.09894799074349024115, 0.9697831060969909212 ) ) ;
#93062 = CIRCLE ( 'NONE', #67204, 33.82893434829264123 ) ;
#93063 = CARTESIAN_POINT ( 'NONE',  ( 17.58776036026792156, 49.99999999999999289, 62.73861743982075723 ) ) ;
#93064 = CARTESIAN_POINT ( 'NONE',  ( 44.66387834505498944, 341.6072687625629101, 1.189588019127773677 ) ) ;
#93065 = EDGE_CURVE ( 'NONE', #66369, #66199, #40196, .T. ) ;
#93066 = CARTESIAN_POINT ( 'NONE',  ( 9.365057959178315627, 53.65588038361938317, -1.821971454984222083 ) ) ;
#93067 = EDGE_CURVE ( 'NONE', #87322, #54320, #33035, .T. ) ;
#93068 = CARTESIAN_POINT ( 'NONE',  ( 104.6654747121523030, -30.00000000000000000, 124.7724495044359116 ) ) ;
#93069 = CARTESIAN_POINT ( 'NONE',  ( -81.69435353299347469, -39.50040572665027128, 158.0323826615473592 ) ) ;
#93070 = EDGE_LOOP ( 'NONE', ( #86236, #24566, #4646, #5094, #29151 ) ) ;
#93071 = CARTESIAN_POINT ( 'NONE',  ( 5.749654562269868196E-15, 24.35682532067546902, 46.94949242731048145 ) ) ;
#93072 = CARTESIAN_POINT ( 'NONE',  ( 5.192560085536420900, 252.6430544263124034, 3.013051918867540202 ) ) ;
#93073 = DIRECTION ( 'NONE',  ( -1.000000000000000000, -1.224606353822377258E-16, -0.000000000000000000 ) ) ;
#93074 = CARTESIAN_POINT ( 'NONE',  ( 34.04963612134775985, 317.5215674871631109, -6.459372692351979417 ) ) ;
#93075 = CARTESIAN_POINT ( 'NONE',  ( 44.22225178598134931, 464.2590902508150066, 9.202154635662399329 ) ) ;
#93076 = ORIENTED_EDGE ( 'NONE', *, *, #19700, .F. ) ;
#93077 = CARTESIAN_POINT ( 'NONE',  ( -32.70432414512315233, 489.1110749878013735, 10.33859015772251055 ) ) ;
#93078 = CARTESIAN_POINT ( 'NONE',  ( 31.83648269796258390, 439.0038992192014575, 23.56519623501327132 ) ) ;
#93079 = ADVANCED_FACE ( 'NONE', ( #94969, #20596, #13477 ), #45350, .F. ) ;
#93080 = VERTEX_POINT ( 'NONE', #88456 ) ;
#93081 = CARTESIAN_POINT ( 'NONE',  ( 2.701558353794677014, 15.00000000000000000, 9.999999999999998224 ) ) ;
#93082 = CARTESIAN_POINT ( 'NONE',  ( 6.965116047733301841, 41.61856606189723351, -70.00485699918135651 ) ) ;
#93083 = CARTESIAN_POINT ( 'NONE',  ( -52.56483885390515098, 49.99999999999999289, -38.23529411764716457 ) ) ;
#93084 = CARTESIAN_POINT ( 'NONE',  ( 3.653337153954944405, -8.634979741397113884, -12.30782724873841083 ) ) ;
#93085 = AXIS2_PLACEMENT_3D ( 'NONE', #55002, #79822, #29215 ) ;
#93086 = B_SPLINE_CURVE_WITH_KNOTS ( 'NONE', 3,
 ( #67808, #85059, #78023, #93685, #102296, #76414, #37068, #2525, #44609, #86672, #27397, #92604 ),
 .UNSPECIFIED., .F., .F.,
 ( 4, 2, 2, 2, 2, 4 ),
 ( 0.000000000000000000, 0.0008247946606697857024, 0.001649589321339571405, 0.002061986651674464419, 0.002474383982009356782, 0.003299178642679125896 ),
 .UNSPECIFIED. ) ;
#93087 = FILL_AREA_STYLE_COLOUR ( '', #44566 ) ;
#93088 = ORIENTED_EDGE ( 'NONE', *, *, #102621, .T. ) ;
#93089 = CARTESIAN_POINT ( 'NONE',  ( 5.600000207755288173, 12.35529564071043040, -13.00000000000000888 ) ) ;
#93091 = CARTESIAN_POINT ( 'NONE',  ( 21.87256311572295076, -60.35484851998849365, 34.71956232952695842 ) ) ;
#93090 = CARTESIAN_POINT ( 'NONE',  ( -94.89844962927027439, -60.00000000000001421, 205.0338773334991060 ) ) ;
#93093 = CARTESIAN_POINT ( 'NONE',  ( -7.420756919583588009E-15, 4.501353321498349658, 60.59507871780017751 ) ) ;
#93092 = PRODUCT_DEFINITION_CONTEXT ( 'detailed design', #52789, 'design' ) ;
#93094 = DIRECTION ( 'NONE',  ( 0.000000000000000000, 1.000000000000000000, 0.000000000000000000 ) ) ;
#93095 = CARTESIAN_POINT ( 'NONE',  ( -36.77948966406264475, -56.82339243700149467, 39.80873089715750268 ) ) ;
#93096 = UNCERTAINTY_MEASURE_WITH_UNIT (LENGTH_MEASURE( 1.000000000000000082E-05 ), #4142, 'distance_accuracy_value', 'NONE');
#93097 = EDGE_LOOP ( 'NONE', ( #67472, #79539, #38261, #63368, #5613 ) ) ;
#93098 = CONICAL_SURFACE ( 'NONE', #91421, 13.50000000000000178, 1.047197551196596077 ) ;
#93099 = FACE_OUTER_BOUND ( 'NONE', #95119, .T. ) ;
#93100 = DIRECTION ( 'NONE',  ( 0.000000000000000000, 0.000000000000000000, -1.000000000000000000 ) ) ;
#93101 = CARTESIAN_POINT ( 'NONE',  ( -13.56225034990342948, -55.77878166967040130, 23.52491571494838851 ) ) ;
#93102 = CARTESIAN_POINT ( 'NONE',  ( 37.56673239365841255, -1.200000000000000030E-05, -10.95617127781092037 ) ) ;
#93103 = CARTESIAN_POINT ( 'NONE',  ( 7.744991119775239241, -61.53561214574870775, -2.016316005557097668 ) ) ;
#93104 = CARTESIAN_POINT ( 'NONE',  ( -15.82318872385067543, 4.444012391166255682, 4.874853782845832484 ) ) ;
#93105 = EDGE_LOOP ( 'NONE', ( #92009, #32608, #11198, #23761 ) ) ;
#93106 = ORIENTED_EDGE ( 'NONE', *, *, #27307, .T. ) ;
#93107 = CARTESIAN_POINT ( 'NONE',  ( 97.69330145236169471, -30.00000000000014921, 190.7792052488607908 ) ) ;
#93108 = CARTESIAN_POINT ( 'NONE',  ( 34.83748305993398731, 40.47757374547448705, -59.82462169405419417 ) ) ;
#93110 = CARTESIAN_POINT ( 'NONE',  ( -4.814352310392316703, -83.20321405896427791, -3.583053941560736089 ) ) ;
#93109 = AXIS2_PLACEMENT_3D ( 'NONE', #101078, #60649, #9936 ) ;
#93111 = CARTESIAN_POINT ( 'NONE',  ( 84.99074402005219042, -30.00000000000000711, 57.64709464612924705 ) ) ;
#93112 = AXIS2_PLACEMENT_3D ( 'NONE', #46026, #12571, #38999 ) ;
#93113 = CARTESIAN_POINT ( 'NONE',  ( -25.12075135752968436, 306.0640628473120159, 10.43383969269943279 ) ) ;
#93114 = VERTEX_POINT ( 'NONE', #38845 ) ;
#93115 = AXIS2_PLACEMENT_3D ( 'NONE', #98198, #40501, #73378 ) ;
#93116 = ORIENTED_EDGE ( 'NONE', *, *, #37501, .T. ) ;
#93117 = ORIENTED_EDGE ( 'NONE', *, *, #54459, .F. ) ;
#93118 = CARTESIAN_POINT ( 'NONE',  ( -32.75517716563597048, 465.7432004789473012, 11.49884209862459095 ) ) ;
#93119 = CARTESIAN_POINT ( 'NONE',  ( 64.78349330513380266, 4.000000000000013323, 0.000000000000000000 ) ) ;
#93120 = CARTESIAN_POINT ( 'NONE',  ( 0.000000000000000000, 0.000000000000000000, 0.000000000000000000 ) ) ;
#93121 = CARTESIAN_POINT ( 'NONE',  ( 5.382954851612913316, -12.99987491489446434, -2.657971597726729307 ) ) ;
#93122 = DIRECTION ( 'NONE',  ( 0.000000000000000000, 0.000000000000000000, 1.000000000000000000 ) ) ;
#93123 = DIRECTION ( 'NONE',  ( 1.734723475976807094E-16, 0.000000000000000000, 1.000000000000000000 ) ) ;
#93124 = VERTEX_POINT ( 'NONE', #21620 ) ;
#93126 = EDGE_CURVE ( 'NONE', #44793, #86259, #3683, .T. ) ;
#93125 = CARTESIAN_POINT ( 'NONE',  ( 7.996668422916345165, 49.99999999999455014, -91.14546720080639375 ) ) ;
#93127 = CIRCLE ( 'NONE', #43232, 5.000000000000010658 ) ;
#93128 = ORIENTED_EDGE ( 'NONE', *, *, #83066, .F. ) ;
#93129 = CARTESIAN_POINT ( 'NONE',  ( -4.472135954999578722, -65.00000000000000000, -4.000000000000002665 ) ) ;
#93130 = CARTESIAN_POINT ( 'NONE',  ( 71.86920016943035705, -38.32705086600410027, 145.1004257776124291 ) ) ;
#93131 = CARTESIAN_POINT ( 'NONE',  ( 18.91791044776121211, 45.00000000000000711, 62.18611311450882795 ) ) ;
#93132 = B_SPLINE_CURVE_WITH_KNOTS ( 'NONE', 3,
 ( #28802, #94573, #20722, #83786, #9898, #68703 ),
 .UNSPECIFIED., .F., .F.,
 ( 4, 2, 4 ),
 ( 0.000000000000000000, 0.0003916983043530463489, 0.0007833966087060926977 ),
 .UNSPECIFIED. ) ;
#93133 = CARTESIAN_POINT ( 'NONE',  ( 24.17442261560467287, 295.4908974038082761, 10.07402396700452663 ) ) ;
#93134 = VECTOR ( 'NONE', #48349, 1000.000000000000000 ) ;
#93135 = CARTESIAN_POINT ( 'NONE',  ( -5.093082057083965886, 247.5555379357842298, -3.176439207277718779 ) ) ;
#93136 = ORIENTED_EDGE ( 'NONE', *, *, #13466, .F. ) ;
#93137 = CARTESIAN_POINT ( 'NONE',  ( -5.036189803708991164, -3.000000000000003109, -93.73786388354257326 ) ) ;
#93138 = CARTESIAN_POINT ( 'NONE',  ( 17.71915776462823189, 45.45154592806376570, -4.750161495150260649 ) ) ;
#93139 = CARTESIAN_POINT ( 'NONE',  ( 31.26787864934703265, 298.8785962927613014, 2.831404287848908297 ) ) ;
#93140 = ADVANCED_FACE ( 'NONE', ( #63659 ), #95012, .T. ) ;
#93141 = DIRECTION ( 'NONE',  ( 1.000000000000000000, 0.000000000000000000, 0.000000000000000000 ) ) ;
#93142 = CARTESIAN_POINT ( 'NONE',  ( 15.47565679866152699, 2.746345986933767858, 1.655435732256164139 ) ) ;
#93143 = ORIENTED_EDGE ( 'NONE', *, *, #73491, .F. ) ;
#93145 = CARTESIAN_POINT ( 'NONE',  ( 7.934203308536662114, -88.86700340017800670, 1.057099537198545214 ) ) ;
#93144 = SURFACE_STYLE_FILL_AREA ( #85057 ) ;
#93146 = CARTESIAN_POINT ( 'NONE',  ( 0.000000000000000000, 0.000000000000000000, 0.000000000000000000 ) ) ;
#93147 = LINE ( 'NONE', #75350, #38484 ) ;
#93148 = DIRECTION ( 'NONE',  ( 0.000000000000000000, -1.000000000000000000, 0.000000000000000000 ) ) ;
#93149 = CARTESIAN_POINT ( 'NONE',  ( -32.87547266101557852, 465.6993878536674742, 10.91512469976539279 ) ) ;
#93150 =( GEOMETRIC_REPRESENTATION_CONTEXT ( 3 ) GLOBAL_UNCERTAINTY_ASSIGNED_CONTEXT ( ( #40961 ) ) GLOBAL_UNIT_ASSIGNED_CONTEXT ( ( #24862, #41553, #43678 ) ) REPRESENTATION_CONTEXT ( 'NONE', 'WORKASPACE' ) );
#93151 = DIRECTION ( 'NONE',  ( -0.5735764363510494901, -0.8191520442889894671, 0.000000000000000000 ) ) ;
#93152 = CARTESIAN_POINT ( 'NONE',  ( 45.99999999998675548, 464.1057728262775868, 11.12967041734905393 ) ) ;
#93153 = CARTESIAN_POINT ( 'NONE',  ( 86.60070351626397667, -39.13477975523821328, 188.3070256512509104 ) ) ;
#93154 = ADVANCED_FACE ( 'NONE', ( #86873 ), #5451, .T. ) ;
#93155 = CARTESIAN_POINT ( 'NONE',  ( 3.006829104376305816E-15, 43.19193163660326462, 24.55262289886175964 ) ) ;
#93156 = ADVANCED_FACE ( 'NONE', ( #47440, #86354, #70145, #103050 ), #62079, .T. ) ;
#93157 = CARTESIAN_POINT ( 'NONE',  ( -7.860264365984205526, 85.36576122646903286, 0.000000000000000000 ) ) ;
#93158 = VERTEX_POINT ( 'NONE', #7501 ) ;
#93159 = SURFACE_STYLE_USAGE ( .BOTH. , #27411 ) ;
#93160 = CARTESIAN_POINT ( 'NONE',  ( -8.559508646656389885, -1.200000000000000030E-05, -2.781152949374503081 ) ) ;
#93161 = CARTESIAN_POINT ( 'NONE',  ( 20.00000000000000000, 12.99999999999999467, 6.999999999999999112 ) ) ;
#93162 = SURFACE_SIDE_STYLE ('',( #10108 ) ) ;
#93163 = EDGE_CURVE ( 'NONE', #66061, #36374, #48458, .T. ) ;
#93164 = CARTESIAN_POINT ( 'NONE',  ( -81.86398423121568158, -29.99999999999999645, 32.54976024431884696 ) ) ;
#93165 = TOROIDAL_SURFACE ( 'NONE', #50112, 8.000000000000000000, 1.000000000000000000 ) ;
#93166 = AXIS2_PLACEMENT_3D ( 'NONE', #37563, #86634, #61276 ) ;
#93167 = SURFACE_STYLE_FILL_AREA ( #52163 ) ;
#93168 = CARTESIAN_POINT ( 'NONE',  ( 32.58266151836870250, -57.69062872889872295, 46.99190750165519859 ) ) ;
#93170 = FACE_OUTER_BOUND ( 'NONE', #83149, .T. ) ;
#93169 = CARTESIAN_POINT ( 'NONE',  ( -9.644834624769993425, 246.9910949979422128, 2.648308524638419925 ) ) ;
#93171 = CARTESIAN_POINT ( 'NONE',  ( -43.37300451664871304, -36.38839727959540937, 41.06639963762513190 ) ) ;
#93172 = CARTESIAN_POINT ( 'NONE',  ( 42.74220749418567777, 488.2672406020900553, 9.363116084196963840 ) ) ;
#93173 = CARTESIAN_POINT ( 'NONE',  ( 7.499940182179008374, -3.043015538677189546, -20.22995127276277927 ) ) ;
#93174 = DIRECTION ( 'NONE',  ( 0.5735764363510466035, -0.8191520442889914655, 1.003171929053524500E-16 ) ) ;
#93175 = CARTESIAN_POINT ( 'NONE',  ( 48.74245842222025260, -27.20503387118322181, -28.29543663440009738 ) ) ;
#93176 = CARTESIAN_POINT ( 'NONE',  ( -26.01996383795994205, -22.09242311380402057, 28.98075328728764788 ) ) ;
#93177 = COLOUR_RGB ( '', 0.40784314, 0.44705882, 0.49803922) ;
#93178 = AXIS2_PLACEMENT_3D ( 'NONE', #19432, #61990, #44192 ) ;
#93179 = ORIENTED_EDGE ( 'NONE', *, *, #25665, .T. ) ;
#93180 = CARTESIAN_POINT ( 'NONE',  ( 5.744562646538029504, 12.72897026649593855, -4.000000000000000888 ) ) ;
#93181 = SURFACE_SIDE_STYLE ('',( #60307 ) ) ;
#93182 = CARTESIAN_POINT ( 'NONE',  ( -18.79090678414550908, -29.03354218681774412, 29.12109915567513596 ) ) ;
#93183 = AXIS2_PLACEMENT_3D ( 'NONE', #70451, #86122, #37048 ) ;
#93185 = CARTESIAN_POINT ( 'NONE',  ( 1.005921156701460539, 36.47725511815836796, -29.24640024088538581 ) ) ;
#93184 = CARTESIAN_POINT ( 'NONE',  ( -14.90155531858861870, 42.58002643027919731, -90.01374843399875658 ) ) ;
#93186 = VERTEX_POINT ( 'NONE', #40419 ) ;
#93187 = PRESENTATION_LAYER_ASSIGNMENT (  '', '', ( #15715 ) ) ;
#93188 = FACE_OUTER_BOUND ( 'NONE', #12292, .T. ) ;
#93189 = ORIENTED_EDGE ( 'NONE', *, *, #4137, .F. ) ;
#93190 = CYLINDRICAL_SURFACE ( 'NONE', #39562, 8.000000000000000000 ) ;
#93191 = AXIS2_PLACEMENT_3D ( 'NONE', #77148, #3264, #36205 ) ;
#93192 = VECTOR ( 'NONE', #71633, 1000.000000000000000 ) ;
#93193 = CARTESIAN_POINT ( 'NONE',  ( 40.59999999999999432, -3.309499999999999886, 4.475777889183790779E-16 ) ) ;
#93194 = CARTESIAN_POINT ( 'NONE',  ( 1.405425595346621037E-06, -60.00000000000000000, -42.63907915653317104 ) ) ;
#93195 = EDGE_LOOP ( 'NONE', ( #100293, #1818, #57201, #91530, #97906 ) ) ;
#93196 = CARTESIAN_POINT ( 'NONE',  ( 99.03177814179444738, -37.80525585742561390, 191.8580698190465625 ) ) ;
#93198 = CARTESIAN_POINT ( 'NONE',  ( 63.81650669486618455, 6.856755485862130937E-15, 0.000000000000000000 ) ) ;
#93197 = LINE ( 'NONE', #100743, #37213 ) ;
#93199 = EDGE_LOOP ( 'NONE', ( #89930, #67198, #64061, #60891, #31648, #49999 ) ) ;
#93200 = ORIENTED_EDGE ( 'NONE', *, *, #74556, .F. ) ;
#93201 = EDGE_CURVE ( 'NONE', #69907, #40083, #106195, .T. ) ;
#93202 = VERTEX_POINT ( 'NONE', #90568 ) ;
#93203 = CARTESIAN_POINT ( 'NONE',  ( 24.50496542748491891, 306.8888831740973160, 10.39605820579407158 ) ) ;
#93204 = EDGE_CURVE ( 'NONE', #93532, #71278, #39381, .T. ) ;
#93205 = CARTESIAN_POINT ( 'NONE',  ( -13.49999999999999645, 0.000000000000000000, -13.00000000000000000 ) ) ;
#93206 = SURFACE_STYLE_FILL_AREA ( #45206 ) ;
#93207 = ORIENTED_EDGE ( 'NONE', *, *, #11170, .T. ) ;
#93208 = DIRECTION ( 'NONE',  ( 1.000000000000000000, -0.000000000000000000, 1.224646799147353207E-16 ) ) ;
#93209 = DIRECTION ( 'NONE',  ( -1.000000000000000000, -0.000000000000000000, -0.000000000000000000 ) ) ;
#93210 =( NAMED_UNIT ( * ) SI_UNIT ( $, .STERADIAN. ) SOLID_ANGLE_UNIT ( ) );
#93212 = CARTESIAN_POINT ( 'NONE',  ( -85.79013029828182368, -59.99999999998781419, -26.89979960300323469 ) ) ;
#93211 = AXIS2_PLACEMENT_3D ( 'NONE', #83366, #42376, #105520 ) ;
#93213 = CARTESIAN_POINT ( 'NONE',  ( 7.744168461338431619, -68.46254061715158912, 2.019395720771554270 ) ) ;
#93214 = FACE_BOUND ( 'NONE', #79604, .T. ) ;
#93215 = CARTESIAN_POINT ( 'NONE',  ( -6.635365861734280557, 41.60399665121233426, -58.75656553345891098 ) ) ;
#93216 = AXIS2_PLACEMENT_3D ( 'NONE', #106461, #65492, #98379 ) ;
#93217 = EDGE_CURVE ( 'NONE', #4337, #85522, #23740, .T. ) ;
#93218 = CARTESIAN_POINT ( 'NONE',  ( -86.58264346576902426, -59.99999999999995737, -26.28034805200384838 ) ) ;
#93219 = CARTESIAN_POINT ( 'NONE',  ( 16.08349330513380337, -4.000000000000000888, 4.898587196589416773E-16 ) ) ;
#93220 = CARTESIAN_POINT ( 'NONE',  ( -50.24583591853911457, -60.30222183590655050, 58.32363953540177448 ) ) ;
#93221 = AXIS2_PLACEMENT_3D ( 'NONE', #22980, #47215, #104945 ) ;
#93222 = ORIENTED_EDGE ( 'NONE', *, *, #45792, .F. ) ;
#93223 = DIRECTION ( 'NONE',  ( 1.000000000000000000, 1.224606353822377258E-16, 0.000000000000000000 ) ) ;
#93224 = ORIENTED_EDGE ( 'NONE', *, *, #50779, .F. ) ;
#93225 = CARTESIAN_POINT ( 'NONE',  ( -5.656854249492381470, -13.06249999999999467, 5.656854249492379694 ) ) ;
#93226 = CARTESIAN_POINT ( 'NONE',  ( -9.738398295829064466, 294.6500605438453704, -2.277702036900738136 ) ) ;
#93227 = CARTESIAN_POINT ( 'NONE',  ( 4.656749229489888897, -8.682395918735693385, -3.785628640239143472 ) ) ;
#93228 = VERTEX_POINT ( 'NONE', #81924 ) ;
#93229 = CARTESIAN_POINT ( 'NONE',  ( 5.382954851612907987, 247.0001250851054522, -2.657971597726739965 ) ) ;
#93230 = CARTESIAN_POINT ( 'NONE',  ( 75.51533756583152979, -30.00000000000000000, -27.33238513093788669 ) ) ;
#93231 = SURFACE_STYLE_FILL_AREA ( #91643 ) ;
#93232 = CARTESIAN_POINT ( 'NONE',  ( 3.685905252136403742, -48.95891067205271696, 104.2837900504726036 ) ) ;
#93233 = CARTESIAN_POINT ( 'NONE',  ( 6.982951203957191488, 41.78396383201351938, -59.69785475688320275 ) ) ;
#93234 = CARTESIAN_POINT ( 'NONE',  ( -5.022013495303277786, 18.64316884711714550, 38.36535705883633085 ) ) ;
#93235 = CARTESIAN_POINT ( 'NONE',  ( 90.25683128961706814, -29.99999999999999645, 190.0668461241068030 ) ) ;
#93236 = CARTESIAN_POINT ( 'NONE',  ( 43.78304604341470707, 434.3019790015191575, 13.50139152689089883 ) ) ;
#93237 = DIRECTION ( 'NONE',  ( -1.000000000000000000, -1.224606353822377258E-16, -0.000000000000000000 ) ) ;
#93238 = VECTOR ( 'NONE', #79575, 1000.000000000000000 ) ;
#93239 = ORIENTED_EDGE ( 'NONE', *, *, #55341, .F. ) ;
#93240 = VERTEX_POINT ( 'NONE', #105160 ) ;
#93241 = CARTESIAN_POINT ( 'NONE',  ( 54.51536369449565456, -46.43638089579248174, 62.03764367210229835 ) ) ;
#93242 = CARTESIAN_POINT ( 'NONE',  ( 5.903046305060341226, 41.64520863941469031, -58.65814346794659428 ) ) ;
#93243 = CARTESIAN_POINT ( 'NONE',  ( -7.500000000000008882, 42.00000000000000711, -65.90297133633691828 ) ) ;
#93244 = ORIENTED_EDGE ( 'NONE', *, *, #11335, .T. ) ;
#93246 = EDGE_CURVE ( 'NONE', #30956, #33490, #10594, .T. ) ;
#93245 = CARTESIAN_POINT ( 'NONE',  ( -86.94600573690735246, -38.36377377443699288, -20.89387357848544369 ) ) ;
#93247 = ORIENTED_EDGE ( 'NONE', *, *, #910, .T. ) ;
#93248 = LINE ( 'NONE', #4771, #58666 ) ;
#93249 = CARTESIAN_POINT ( 'NONE',  ( 110.3745256113219284, -38.35605052074757282, 158.9612946903319823 ) ) ;
#93250 = CARTESIAN_POINT ( 'NONE',  ( 12.78945977464362116, 21.25429375852011660, 5.669412170850756105 ) ) ;
#93251 = CARTESIAN_POINT ( 'NONE',  ( 86.42351163725670915, -60.14453129240431650, 21.61429144264777946 ) ) ;
#93252 = CARTESIAN_POINT ( 'NONE',  ( 32.70943946516541700, 465.7622690753372581, 11.83845320050794925 ) ) ;
#93253 = CARTESIAN_POINT ( 'NONE',  ( -24.16082351539475326, 304.6853429583268280, -9.820488471465781188 ) ) ;
#93254 = CARTESIAN_POINT ( 'NONE',  ( 6.999999995588868984, -13.84708942052852798, -5.798489586937981777 ) ) ;
#93255 = CARTESIAN_POINT ( 'NONE',  ( -24.23034962376434365, 25.18874428018206046, -32.69349392899435713 ) ) ;
#93256 = CONICAL_SURFACE ( 'NONE', #53675, 4.172000000000001485, 0.9599310885968750373 ) ;
#93257 = CARTESIAN_POINT ( 'NONE',  ( -44.34415387544927256, 435.2422591719043226, 12.20585227837768016 ) ) ;
#93258 = AXIS2_PLACEMENT_3D ( 'NONE', #40066, #50785, #16863 ) ;
#93259 = CARTESIAN_POINT ( 'NONE',  ( 8.361479372611764660, 121.1764542251195280, 5.000000000001228351 ) ) ;
#93260 = ORIENTED_EDGE ( 'NONE', *, *, #42170, .T. ) ;
#93261 = EDGE_CURVE ( 'NONE', #11951, #15047, #97058, .T. ) ;
#93262 = EDGE_CURVE ( 'NONE', #76235, #26529, #22272, .T. ) ;
#93263 = CARTESIAN_POINT ( 'NONE',  ( 0.4142141812692001213, 37.18443326924929693, 27.31766813022851181 ) ) ;
#93264 = CARTESIAN_POINT ( 'NONE',  ( 15.76193534935208262, 36.72733462479577327, -23.83658602074658717 ) ) ;
#93265 = DIRECTION ( 'NONE',  ( 0.000000000000000000, 0.000000000000000000, -1.000000000000000000 ) ) ;
#93266 = CIRCLE ( 'NONE', #14016, 4.000000000000000888 ) ;
#93267 = ORIENTED_EDGE ( 'NONE', *, *, #53498, .F. ) ;
#93268 = DIRECTION ( 'NONE',  ( 0.000000000000000000, -1.000000000000000000, 0.000000000000000000 ) ) ;
#93269 = CARTESIAN_POINT ( 'NONE',  ( -38.54376935657065673, 311.7842164531986100, 5.990876337056916690 ) ) ;
#93270 = CARTESIAN_POINT ( 'NONE',  ( 27.61650669486618881, 4.898587196589413815E-16, -4.000000000000000888 ) ) ;
#93271 = LINE ( 'NONE', #83566, #93746 ) ;
#93272 = CARTESIAN_POINT ( 'NONE',  ( 3.313708498984762052, -18.21874999999999645, -8.000000000000000000 ) ) ;
#93273 = CARTESIAN_POINT ( 'NONE',  ( -7.749805355827879438, -13.26271386457699997, 32.00645959793580886 ) ) ;
#93274 = AXIS2_PLACEMENT_3D ( 'NONE', #102895, #27453, #46252 ) ;
#93275 =( GEOMETRIC_REPRESENTATION_CONTEXT ( 3 ) GLOBAL_UNCERTAINTY_ASSIGNED_CONTEXT ( ( #74217 ) ) GLOBAL_UNIT_ASSIGNED_CONTEXT ( ( #106532, #73085, #14867 ) ) REPRESENTATION_CONTEXT ( 'NONE', 'WORKASPACE' ) );
#93276 = B_SPLINE_CURVE_WITH_KNOTS ( 'NONE', 3,
 ( #39693, #55824, #97903, #47752, #105984, #6773, #24059, #56900 ),
 .UNSPECIFIED., .F., .F.,
 ( 4, 2, 2, 4 ),
 ( 0.003797433802554431997, 0.004743183970586230085, 0.005688934138618028172, 0.007580434474681626948 ),
 .UNSPECIFIED. ) ;
#93277 = DIRECTION ( 'NONE',  ( -1.000000000000000000, -1.224606353822377258E-16, -0.000000000000000000 ) ) ;
#93278 = VERTEX_POINT ( 'NONE', #24271 ) ;
#93279 = CARTESIAN_POINT ( 'NONE',  ( 86.15856653264481224, -21.41364612637495668, 176.4187449916978210 ) ) ;
#93280 = DIRECTION ( 'NONE',  ( 0.000000000000000000, 0.000000000000000000, 1.000000000000000000 ) ) ;
#93281 = B_SPLINE_CURVE_WITH_KNOTS ( 'NONE', 3,
 ( #92964, #4491, #93515, #51963, #101596, #103191, #84878, #10964, #85414, #21244, #53572, #76775, #86502, #12564, #70294, #36376, #2877, #62226 ),
 .UNSPECIFIED., .F., .F.,
 ( 4, 2, 2, 2, 2, 2, 2, 2, 4 ),
 ( 0.5000000000000000000, 0.5625000000000000000, 0.6250000000000000000, 0.6875000000000000000, 0.7500000000000000000, 0.8125000000000000000, 0.8750000000000000000, 0.9375000000000000000, 1.000000000000000000 ),
 .UNSPECIFIED. ) ;
#93282 = EDGE_CURVE ( 'NONE', #35207, #9118, #24422, .T. ) ;
#93283 = CARTESIAN_POINT ( 'NONE',  ( -15.39205472978310141, 46.19766366449148620, 5.347876573122078980 ) ) ;
#93284 = EDGE_LOOP ( 'NONE', ( #38039, #78403, #88363, #34567 ) ) ;
#93285 = CARTESIAN_POINT ( 'NONE',  ( -98.00753366316151016, -52.71031723798989077, 110.7941533929202507 ) ) ;
#93286 = SURFACE_SIDE_STYLE ('',( #70068 ) ) ;
#93287 = CARTESIAN_POINT ( 'NONE',  ( -12.67000837003889124, -5.000000000000002665, -88.76274061127951143 ) ) ;
#93288 = CARTESIAN_POINT ( 'NONE',  ( 0.000000000000000000, 0.000000000000000000, -5.283275477074182547 ) ) ;
#93289 = CARTESIAN_POINT ( 'NONE',  ( -18.69161154690413795, -25.36093076282173087, -38.50044509632451906 ) ) ;
#93290 = EDGE_CURVE ( 'NONE', #33722, #57238, #79505, .T. ) ;
#93291 = CIRCLE ( 'NONE', #45115, 4.000000000000007105 ) ;
#93292 = CARTESIAN_POINT ( 'NONE',  ( 40.53591651757645309, -60.00000000000000000, 52.85790476262030779 ) ) ;
#93293 = AXIS2_PLACEMENT_3D ( 'NONE', #15606, #32359, #25333 ) ;
#93294 = CARTESIAN_POINT ( 'NONE',  ( 33.80992109950155111, -34.85164080663998476, 43.18581089266367457 ) ) ;
#93295 = CARTESIAN_POINT ( 'NONE',  ( 7.986468734911287726, 108.9731367972307936, 0.5341897780976140320 ) ) ;
#93296 = EDGE_CURVE ( 'NONE', #31195, #86477, #8044, .T. ) ;
#93298 = CARTESIAN_POINT ( 'NONE',  ( -13.02509636762063039, 21.68341507793183354, 4.986677504272470252 ) ) ;
#93297 = CARTESIAN_POINT ( 'NONE',  ( -37.27179927782982816, -36.61903506054549240, 46.51218512112991021 ) ) ;
#93299 = CONICAL_SURFACE ( 'NONE', #101909, 4.000000000000007105, 0.9599310885968835860 ) ;
#93300 = CARTESIAN_POINT ( 'NONE',  ( 3.396983858748188645, 299.9646488655011467, -10.00714413801396319 ) ) ;
#93301 = CARTESIAN_POINT ( 'NONE',  ( 44.66387834505498944, 341.6072687625629101, 1.189588019127773677 ) ) ;
#93302 = EDGE_CURVE ( 'NONE', #100266, #42587, #53637, .T. ) ;
#93303 = FILL_AREA_STYLE ('',( #46341 ) ) ;
#93304 = DIRECTION ( 'NONE',  ( -1.000000000000000000, 0.000000000000000000, 0.000000000000000000 ) ) ;
#93305 = VERTEX_POINT ( 'NONE', #40955 ) ;
#93306 = CARTESIAN_POINT ( 'NONE',  ( -3.364021409948656505, 294.8518027753228807, 9.936999415087239385 ) ) ;
#93307 = CARTESIAN_POINT ( 'NONE',  ( -2.090939542649697280, -60.00000000000000711, 39.63613289865730849 ) ) ;
#93308 = ORIENTED_EDGE ( 'NONE', *, *, #61163, .T. ) ;
#93309 = CARTESIAN_POINT ( 'NONE',  ( -15.90614609307868577, -3.157894736842107086, 14.66382285868950852 ) ) ;
#93310 = DIRECTION ( 'NONE',  ( -1.000000000000000000, -1.224606353822377258E-16, -0.000000000000000000 ) ) ;
#93311 = FACE_OUTER_BOUND ( 'NONE', #29053, .T. ) ;
#93312 = CARTESIAN_POINT ( 'NONE',  ( 3.211837540737783936, -60.22813567888628938, -36.90749154621568096 ) ) ;
#93313 = ORIENTED_EDGE ( 'NONE', *, *, #40221, .F. ) ;
#93314 = DIRECTION ( 'NONE',  ( 0.000000000000000000, 0.000000000000000000, 1.000000000000000000 ) ) ;
#93315 = DIRECTION ( 'NONE',  ( -1.000000000000000000, -1.224606353822377258E-16, -0.000000000000000000 ) ) ;
#93316 = ORIENTED_EDGE ( 'NONE', *, *, #49341, .T. ) ;
#93317 = CARTESIAN_POINT ( 'NONE',  ( 0.000000000000000000, 0.000000000000000000, -13.00000000000003730 ) ) ;
#93318 = CARTESIAN_POINT ( 'NONE',  ( 18.13561277374696701, 1.340359594676612611E-15, 0.000000000000000000 ) ) ;
#93319 = FILL_AREA_STYLE_COLOUR ( '', #51085 ) ;
#93320 = CARTESIAN_POINT ( 'NONE',  ( -92.28312636555040172, -59.99999999999999289, 23.72048675611388546 ) ) ;
#93321 = B_SPLINE_CURVE_WITH_KNOTS ( 'NONE', 3,
 ( #84706, #50714, #3261, #42647, #60459, #19487, #83627, #36202 ),
 .UNSPECIFIED., .F., .F.,
 ( 4, 2, 2, 4 ),
 ( 0.000000000000000000, 7.350793746624747918E-05, 0.0001470158749324949584, 0.0002940317498649912720 ),
 .UNSPECIFIED. ) ;
#93322 = CARTESIAN_POINT ( 'NONE',  ( -3.313708498984760276, -25.53124999999999645, -8.000000000000000000 ) ) ;
#93323 = FACE_OUTER_BOUND ( 'NONE', #84029, .T. ) ;
#93324 = CARTESIAN_POINT ( 'NONE',  ( 13.58349330513380515, 1.593028355512270962E-15, 0.000000000000000000 ) ) ;
#93325 = FACE_OUTER_BOUND ( 'NONE', #9624, .T. ) ;
#93327 =( NAMED_UNIT ( * ) SI_UNIT ( $, .STERADIAN. ) SOLID_ANGLE_UNIT ( ) );
#93326 = CARTESIAN_POINT ( 'NONE',  ( 9.739726766104286781, -3.000000000000002665, -87.61747884499031613 ) ) ;
#93328 = CARTESIAN_POINT ( 'NONE',  ( -85.45028039093672589, -18.58812102731535632, 159.4271763632907835 ) ) ;
#93329 = ORIENTED_EDGE ( 'NONE', *, *, #30704, .T. ) ;
#93330 = CARTESIAN_POINT ( 'NONE',  ( -43.62590748909082805, 434.3202425174551422, 14.43486319446150645 ) ) ;
#93331 = CONICAL_SURFACE ( 'NONE', #74145, 11.96035173608223090, 1.221730476396025722 ) ;
#93332 = AXIS2_PLACEMENT_3D ( 'NONE', #27663, #51875, #26596 ) ;
#93333 = VERTEX_POINT ( 'NONE', #64189 ) ;
#93334 =( BOUNDED_SURFACE ( )  B_SPLINE_SURFACE ( 2, 3, ( 
 ( #44534, #86603, #102224, #68269, #27324, #60204, #77953, #12668, #28922, #36476, #92530, #76341, #100622, #12142, #19239, #43990, #43465, #52069, #84984, #4068, #20303, #28373, #11066, #76877, #78475, #53153, #61250, #2990, #26784, #94691, #59653, #94134, #77422, #45598, #53669, #69866, #3538, #18684, #51540, #84454, #35944, #68814, #101697, #27857, #93613, #87120, #62316, #95209, #47160, #7229, #70919, #6706, #62840, #30483, #71978, #96795, #46124, #104888, #104334, #21341, #55248, #47686, #39633, #22404, #29443, #6167, #63909, #64433, #105409, #13194, #14791, #70398, #95731, #89233, #103811, #31550, #54179, #79010, #97304, #55763, #5130, #21871, #38063, #48217, #80584, #22927, #72504, #5648, #81120, #87648, #29956, #23459, #54711, #103297, #13730, #46638, #79535, #88696, #38572, #71433, #88172, #63381, #56294, #15330, #96278, #14256, #80057, #39098, #31028, #49275, #57900, #50866, #48740, #16389, #64947, #83249, #8295, #91878, #91362, #98883, #695, #41201, #49818, #40665, #42252, #90824, #65484, #40139, #33136, #16940, #25044, #26135, #73549, #74087, #82179, #82723, #98373, #173, #106453, #41731, #1238, #8827, #74615, #66006, #32611, #57366, #67080, #24526, #99963, #90285, #33660, #66539, #99413, #18005, #25595, #58453, #17477, #50339, #9342, #73016, #75143, #83771, #34208, #58990, #105921, #81633, #7757, #32073, #97839, #24000, #56840, #89765, #15862, #92934, #10932, #77292, #102084, #68686, #43853, #19634, #12009, #92395, #43331, #53014, #76743, #77826, #18544, #36867, #2853, #51408, #60597, #20707, #101566, #84320, #28245, #3404, #52467, #85385, #2318, #69217, #68131, #94556 ),
 ( #61115, #9882, #35263, #28784, #10416, #44942, #100492, #26649, #3935, #94002, #76212, #101027, #53545, #51936, #35807, #93485, #27724, #59526, #27181, #85938, #69735, #11468, #60072, #61666, #102626, #44396, #42793, #36347, #19096, #84849, #20164, #75686, #1785, #34742, #67613, #78340, #62198, #23317, #71834, #4997, #29830, #103163, #29308, #45990, #104740, #6035, #88043, #95084, #86991, #64298, #38958, #14123, #78870, #12532, #47556, #86476, #55113, #104202, #72371, #80452, #55629, #5520, #6563, #97170, #22794, #63239, #38443, #21216, #105277, #37928, #54046, #4458, #37401, #96131, #45467, #13059, #88566, #70790, #46508, #47024, #30890, #103686, #79926, #13594, #70262, #71309, #63771, #14647, #30346, #62707, #22264, #96659, #39496, #31423, #95598, #21736, #54575, #87514, #79404, #56705, #91240, #40014, #72886, #17347, #41605, #31936, #7618, #23861, #34082, #66403, #8697, #99284, #98239, #66954, #73416, #105797, #50222, #32477, #64816, #82592, #97697, #74488, #41073, #16257, #99833, #106313, #25463, #8167, #16800, #89628, #58315, #15728, #65877, #75012, #48613, #7099, #49142, #42126, #563, #81498, #40536, #56154, #83123, #33531, #9218, #24395, #89098, #65348, #57234, #1106, #90152, #82043, #15192, #73957, #48081, #38, #33010, #80983, #98756, #24910, #57764, #49686, #90690, #29577, #100364, #37134, #46259, #59401, #83641, #20447, #13333, #12809, #92262, #71056, #69477, #28509, #4205, #61393, #42663, #75562, #70537, #62449, #86210, #9746, #79145, #103428, #78086, #5271, #29065, #67485, #18416, #26528, #4736, #38196, #95340, #70000, #17877, #1657, #26005, #45723, #52744, #77565 ),
 ( #34615, #85667, #58868, #53805, #61935, #11740, #91758, #21476, #50731, #102901, #45212, #44678, #54311, #87258, #53289, #3680, #36612, #102362, #94825, #12282, #94282, #20971, #86734, #78605, #37675, #22002, #80725, #40806, #104480, #40279, #96413, #64050, #105544, #23596, #79676, #31682, #31165, #95878, #88835, #81252, #73155, #55900, #62976, #39767, #97435, #97983, #32208, #46782, #48360, #103947, #22544, #16007, #30626, #65086, #87785, #13868, #24138, #89377, #5786, #55385, #72642, #88315, #96925, #63514, #64568, #56981, #6843, #56444, #6301, #14390, #47301, #89895, #80197, #48883, #39241, #72115, #23061, #105025, #81777, #15467, #14929, #47821, #7367, #106056, #30093, #7900, #54855, #38708, #71572, #25192, #82330, #41341, #17618, #99568, #100639, #18154, #51010, #92551, #49960, #74758, #34356, #59136, #25747, #838, #83392, #75836, #49426, #310, #10038, #33810, #34884, #8440, #26799, #66687, #74233, #50480, #84469, #58602, #33277, #92018, #67231, #9489, #42400, #66147, #26273, #58050, #51555, #8964, #75296, #98507, #67752, #1389, #42945, #1933, #59669, #99029, #82868, #83927, #18699, #10564, #73700, #100108, #106602, #65625, #32752, #24657, #57509, #90432, #90972, #16535, #17083, #41870, #91505, #61266, #2469, #20857, #37551, #69883, #27878, #87139, #61815, #28393, #52616, #94155, #54200, #52088, #19783, #68287, #86622, #11624, #95228, #94708, #102241, #4087, #44554, #53171, #44010, #45618, #20326, #68833, #43479, #36494, #86088, #12160, #29463, #76897, #77441, #85543, #3556, #3011, #60743, #70419, #35963, #103315, #101712, #93632, #69362, #45090, #21360, #77969, #37015, #102777 ) ),
 .UNSPECIFIED., .F., .F., .T. ) 
 B_SPLINE_SURFACE_WITH_KNOTS ( ( 3, 3 ),
 ( 4, 2, 2, 2, 2, 2, 2, 2, 2, 2, 2, 2, 2, 2, 2, 2, 2, 2, 2, 2, 2, 2, 2, 2, 2, 2, 2, 2, 2, 2, 2, 2, 2, 2, 2, 2, 2, 2, 2, 2, 2, 2, 2, 2, 2, 2, 2, 2, 2, 2, 2, 2, 2, 2, 2, 2, 2, 2, 2, 2, 2, 2, 2, 2, 2, 2, 2, 2, 2, 2, 2, 2, 2, 2, 2, 2, 2, 2, 2, 2, 2, 2, 2, 2, 2, 2, 2, 2, 2, 2, 2, 2, 2, 2, 2, 2, 2, 2, 2, 2, 4 ),
 ( 0.000000000000000000, 1.000000000000000000 ),
 ( 0.000000000000000000, 0.008518889176590353426, 0.01277833376488552927, 0.01703777835318070685, 0.02129722294147588096, 0.02342694523562346975, 0.02555666752977105854, 0.02981611211806623613, 0.03088097326514003052, 0.03194583441221382492, 0.03407555670636141371, 0.03833500129465658435, 0.04046472358880417314, 0.04259444588295176193, 0.04685389047124693951, 0.05111333505954211709, 0.05537277964783729467, 0.05963222423613247225, 0.06389166882442764983, 0.06815111341272282741, 0.07667000258931316869, 0.08518889176590352386, 0.1022266701190842342, 0.1363022268254456548, 0.1533400051786263374, 0.1618588943552166926, 0.1703777835318070477, 0.1746372281201022392, 0.1788966727083974029, 0.1831561172966925666, 0.1874155618849877580, 0.1895452841791353538, 0.1916750064732829495, 0.1938047287674305452, 0.1948695899145043153, 0.1959344510615781132, 0.1980641733557256812, 0.2001938956498732769, 0.2012587567969470748, 0.2023236179440208726, 0.2044533402381684684, 0.2065830625323160641, 0.2087127848264636598, 0.2108425071206112555, 0.2129722294147588235, 0.2140370905618326214, 0.2151019517089063915, 0.2172316740030539872, 0.2182965351501277851, 0.2193613962972015830, 0.2214911185913491787, 0.2225559797384229765, 0.2236208408854967744, 0.2257505631796443701, 0.2278802854737919659, 0.2300100077679395338, 0.2342694523562346975, 0.2363991746503822933, 0.2385288969445298890, 0.2427883415328250805, 0.2470477861211202442, 0.2555666752977105993, 0.2598261198860057908, 0.2640855644743009822, 0.2726044536508913096, 0.2896422320040720200, 0.3066800103572526748, 0.3407555670636140954, 0.3577933454167948057, 0.3748311237699755161, 0.3918689021231562264, 0.4003877912997465538, 0.4089066804763369367, 0.4131661250646321282, 0.4174255696529273196, 0.4216850142412225111, 0.4259444588295176470, 0.4302039034178127830, 0.4344633480061079744, 0.4365930703002555702, 0.4387227925944031659, 0.4429822371826983574, 0.4440470983297721830, 0.4451119594768459531, 0.4472416817709935488, 0.4515011263592887403, 0.4557605709475839317, 0.4600200155358790677, 0.4621497378300266634, 0.4642794601241742036, 0.4685389047124693951, 0.4770577938890597780, 0.4855766830656501609, 0.4898361276539453524, 0.4940955722422404883, 0.5026144614188308157, 0.5111333505954211986, 0.5196522397720115816, 0.5281711289486019645, 0.5366900181251923474, 0.5452089073017826193 ),
 .UNSPECIFIED. ) 
 GEOMETRIC_REPRESENTATION_ITEM ( )  RATIONAL_B_SPLINE_SURFACE ( (
 ( 1.000000000000000000, 1.000000000000000000, 1.000000000000000000, 1.000000000000000000, 1.000000000000000000, 1.000000000000000000, 1.000000000000000000, 1.000000000000000000, 1.000000000000000000, 1.000000000000000000, 1.000000000000000000, 1.000000000000000000, 1.000000000000000000, 1.000000000000000000, 1.000000000000000000, 1.000000000000000000, 1.000000000000000000, 1.000000000000000000, 1.000000000000000000, 1.000000000000000000, 1.000000000000000000, 1.000000000000000000, 1.000000000000000000, 1.000000000000000000, 1.000000000000000000, 1.000000000000000000, 1.000000000000000000, 1.000000000000000000, 1.000000000000000000, 1.000000000000000000, 1.000000000000000000, 1.000000000000000000, 1.000000000000000000, 1.000000000000000000, 1.000000000000000000, 1.000000000000000000, 1.000000000000000000, 1.000000000000000000, 1.000000000000000000, 1.000000000000000000, 1.000000000000000000, 1.000000000000000000, 1.000000000000000000, 1.000000000000000000, 1.000000000000000000, 1.000000000000000000, 1.000000000000000000, 1.000000000000000000, 1.000000000000000000, 1.000000000000000000, 1.000000000000000000, 1.000000000000000000, 1.000000000000000000, 1.000000000000000000, 1.000000000000000000, 1.000000000000000000, 1.000000000000000000, 1.000000000000000000, 1.000000000000000000, 1.000000000000000000, 1.000000000000000000, 1.000000000000000000, 1.000000000000000000, 1.000000000000000000, 1.000000000000000000, 1.000000000000000000, 1.000000000000000000, 1.000000000000000000, 1.000000000000000000, 1.000000000000000000, 1.000000000000000000, 1.000000000000000000, 1.000000000000000000, 1.000000000000000000, 1.000000000000000000, 1.000000000000000000, 1.000000000000000000, 1.000000000000000000, 1.000000000000000000, 1.000000000000000000, 1.000000000000000000, 1.000000000000000000, 1.000000000000000000, 1.000000000000000000, 1.000000000000000000, 1.000000000000000000, 1.000000000000000000, 1.000000000000000000, 1.000000000000000000, 1.000000000000000000, 1.000000000000000000, 1.000000000000000000, 1.000000000000000000, 1.000000000000000000, 1.000000000000000000, 1.000000000000000000, 1.000000000000000000, 1.000000000000000000, 1.000000000000000000, 1.000000000000000000, 1.000000000000000000, 1.000000000000000000, 1.000000000000000000, 1.000000000000000000, 1.000000000000000000, 1.000000000000000000, 1.000000000000000000, 1.000000000000000000, 1.000000000000000000, 1.000000000000000000, 1.000000000000000000, 1.000000000000000000, 1.000000000000000000, 1.000000000000000000, 1.000000000000000000, 1.000000000000000000, 1.000000000000000000, 1.000000000000000000, 1.000000000000000000, 1.000000000000000000, 1.000000000000000000, 1.000000000000000000, 1.000000000000000000, 1.000000000000000000, 1.000000000000000000, 1.000000000000000000, 1.000000000000000000, 1.000000000000000000, 1.000000000000000000, 1.000000000000000000, 1.000000000000000000, 1.000000000000000000, 1.000000000000000000, 1.000000000000000000, 1.000000000000000000, 1.000000000000000000, 1.000000000000000000, 1.000000000000000000, 1.000000000000000000, 1.000000000000000000, 1.000000000000000000, 1.000000000000000000, 1.000000000000000000, 1.000000000000000000, 1.000000000000000000, 1.000000000000000000, 1.000000000000000000, 1.000000000000000000, 1.000000000000000000, 1.000000000000000000, 1.000000000000000000, 1.000000000000000000, 1.000000000000000000, 1.000000000000000000, 1.000000000000000000, 1.000000000000000000, 1.000000000000000000, 1.000000000000000000, 1.000000000000000000, 1.000000000000000000, 1.000000000000000000, 1.000000000000000000, 1.000000000000000000, 1.000000000000000000, 1.000000000000000000, 1.000000000000000000, 1.000000000000000000, 1.000000000000000000, 1.000000000000000000, 1.000000000000000000, 1.000000000000000000, 1.000000000000000000, 1.000000000000000000, 1.000000000000000000, 1.000000000000000000, 1.000000000000000000, 1.000000000000000000, 1.000000000000000000, 1.000000000000000000, 1.000000000000000000, 1.000000000000000000, 1.000000000000000000, 1.000000000000000000, 1.000000000000000000, 1.000000000000000000, 1.000000000000000000, 1.000000000000000000, 1.000000000000000000, 1.000000000000000000, 1.000000000000000000, 1.000000000000000000, 1.000000000000000000, 1.000000000000000000, 1.000000000000000000, 1.000000000000000000, 1.000000000000000000, 1.000000000000000000, 1.000000000000000000, 1.000000000000000000, 1.000000000000000000, 1.000000000000000000, 1.000000000000000000),
 ( 1.857142857142858317, 1.857142857142858317, 1.857142857142858317, 1.857142857142858317, 1.857142857142858317, 1.857142857142858317, 1.857142857142858317, 1.857142857142858317, 1.857142857142858317, 1.857142857142858317, 1.857142857142858317, 1.857142857142858317, 1.857142857142858317, 1.857142857142858317, 1.857142857142858317, 1.857142857142858317, 1.857142857142858317, 1.857142857142858317, 1.857142857142858317, 1.857142857142858317, 1.857142857142858317, 1.857142857142858317, 1.857142857142859205, 1.857142857142859205, 1.857142857142858317, 1.857142857142858317, 1.857142857142858317, 1.857142857142858317, 1.857142857142858317, 1.857142857142858317, 1.857142857142858317, 1.857142857142858317, 1.857142857142858317, 1.857142857142858317, 1.857142857142858317, 1.857142857142858317, 1.857142857142858317, 1.857142857142858317, 1.857142857142858317, 1.857142857142858317, 1.857142857142858317, 1.857142857142858317, 1.857142857142858317, 1.857142857142858317, 1.857142857142858317, 1.857142857142858317, 1.857142857142858317, 1.857142857142858317, 1.857142857142858317, 1.857142857142858317, 1.857142857142858317, 1.857142857142858317, 1.857142857142858317, 1.857142857142858317, 1.857142857142858317, 1.857142857142858317, 1.857142857142858317, 1.857142857142858317, 1.857142857142858317, 1.857142857142858317, 1.857142857142858317, 1.857142857142858317, 1.857142857142858317, 1.857142857142858317, 1.857142857142858317, 1.857142857142858317, 1.857142857142858317, 1.857142857142858317, 1.857142857142858317, 1.857142857142858317, 1.857142857142858317, 1.857142857142858317, 1.857142857142858317, 1.857142857142858317, 1.857142857142858317, 1.857142857142858317, 1.857142857142858317, 1.857142857142858317, 1.857142857142858317, 1.857142857142858317, 1.857142857142858317, 1.857142857142858317, 1.857142857142858317, 1.857142857142858317, 1.857142857142858317, 1.857142857142858317, 1.857142857142858317, 1.857142857142858317, 1.857142857142858317, 1.857142857142858317, 1.857142857142858317, 1.857142857142858317, 1.857142857142858317, 1.857142857142858317, 1.857142857142858317, 1.857142857142858317, 1.857142857142858317, 1.857142857142858317, 1.857142857142858317, 1.857142857142858317, 1.857142857142858317, 1.857142857142858317, 1.857142857142858317, 1.857142857142858317, 1.857142857142858317, 1.857142857142858317, 1.857142857142858317, 1.857142857142858317, 1.857142857142858317, 1.857142857142858317, 1.857142857142858317, 1.857142857142858317, 1.857142857142858317, 1.857142857142858317, 1.857142857142858317, 1.857142857142858317, 1.857142857142858317, 1.857142857142858317, 1.857142857142858317, 1.857142857142858317, 1.857142857142858317, 1.857142857142858317, 1.857142857142858317, 1.857142857142858317, 1.857142857142858317, 1.857142857142858317, 1.857142857142858317, 1.857142857142858317, 1.857142857142858317, 1.857142857142858317, 1.857142857142858317, 1.857142857142858317, 1.857142857142858317, 1.857142857142858317, 1.857142857142858317, 1.857142857142858317, 1.857142857142858317, 1.857142857142858317, 1.857142857142858317, 1.857142857142858317, 1.857142857142858317, 1.857142857142858317, 1.857142857142858317, 1.857142857142858317, 1.857142857142858317, 1.857142857142858317, 1.857142857142858317, 1.857142857142858317, 1.857142857142858317, 1.857142857142858317, 1.857142857142858317, 1.857142857142858317, 1.857142857142858317, 1.857142857142858317, 1.857142857142858317, 1.857142857142858317, 1.857142857142858317, 1.857142857142858317, 1.857142857142858317, 1.857142857142858317, 1.857142857142858317, 1.857142857142858317, 1.857142857142859205, 1.857142857142859205, 1.857142857142858317, 1.857142857142858317, 1.857142857142858317, 1.857142857142858317, 1.857142857142858317, 1.857142857142858317, 1.857142857142858317, 1.857142857142858317, 1.857142857142858317, 1.857142857142858317, 1.857142857142858317, 1.857142857142858317, 1.857142857142858317, 1.857142857142858317, 1.857142857142858317, 1.857142857142858317, 1.857142857142857428, 1.857142857142857428, 1.857142857142858317, 1.857142857142858317, 1.857142857142858317, 1.857142857142858317, 1.857142857142856318, 1.857142857142856318, 1.857142857142858317, 1.857142857142858317, 1.857142857142858317, 1.857142857142858317, 1.857142857142858317, 1.857142857142858317, 1.857142857142858317, 1.857142857142858317, 1.857142857142858317, 1.857142857142858317, 1.857142857142858317, 1.857142857142858317, 1.857142857142858317, 1.857142857142858317),
 ( 1.000000000000000000, 1.000000000000000000, 1.000000000000000000, 1.000000000000000000, 1.000000000000000000, 1.000000000000000000, 1.000000000000000000, 1.000000000000000000, 1.000000000000000000, 1.000000000000000000, 1.000000000000000000, 1.000000000000000000, 1.000000000000000000, 1.000000000000000000, 1.000000000000000000, 1.000000000000000000, 1.000000000000000000, 1.000000000000000000, 1.000000000000000000, 1.000000000000000000, 1.000000000000000000, 1.000000000000000000, 1.000000000000000000, 1.000000000000000000, 1.000000000000000000, 1.000000000000000000, 1.000000000000000000, 1.000000000000000000, 1.000000000000000000, 1.000000000000000000, 1.000000000000000000, 1.000000000000000000, 1.000000000000000000, 1.000000000000000000, 1.000000000000000000, 1.000000000000000000, 1.000000000000000000, 1.000000000000000000, 1.000000000000000000, 1.000000000000000000, 1.000000000000000000, 1.000000000000000000, 1.000000000000000000, 1.000000000000000000, 1.000000000000000000, 1.000000000000000000, 1.000000000000000000, 1.000000000000000000, 1.000000000000000000, 1.000000000000000000, 1.000000000000000000, 1.000000000000000000, 1.000000000000000000, 1.000000000000000000, 1.000000000000000000, 1.000000000000000000, 1.000000000000000000, 1.000000000000000000, 1.000000000000000000, 1.000000000000000000, 1.000000000000000000, 1.000000000000000000, 1.000000000000000000, 1.000000000000000000, 1.000000000000000000, 1.000000000000000000, 1.000000000000000000, 1.000000000000000000, 1.000000000000000000, 1.000000000000000000, 1.000000000000000000, 1.000000000000000000, 1.000000000000000000, 1.000000000000000000, 1.000000000000000000, 1.000000000000000000, 1.000000000000000000, 1.000000000000000000, 1.000000000000000000, 1.000000000000000000, 1.000000000000000000, 1.000000000000000000, 1.000000000000000000, 1.000000000000000000, 1.000000000000000000, 1.000000000000000000, 1.000000000000000000, 1.000000000000000000, 1.000000000000000000, 1.000000000000000000, 1.000000000000000000, 1.000000000000000000, 1.000000000000000000, 1.000000000000000000, 1.000000000000000000, 1.000000000000000000, 1.000000000000000000, 1.000000000000000000, 1.000000000000000000, 1.000000000000000000, 1.000000000000000000, 1.000000000000000000, 1.000000000000000000, 1.000000000000000000, 1.000000000000000000, 1.000000000000000000, 1.000000000000000000, 1.000000000000000000, 1.000000000000000000, 1.000000000000000000, 1.000000000000000000, 1.000000000000000000, 1.000000000000000000, 1.000000000000000000, 1.000000000000000000, 1.000000000000000000, 1.000000000000000000, 1.000000000000000000, 1.000000000000000000, 1.000000000000000000, 1.000000000000000000, 1.000000000000000000, 1.000000000000000000, 1.000000000000000000, 1.000000000000000000, 1.000000000000000000, 1.000000000000000000, 1.000000000000000000, 1.000000000000000000, 1.000000000000000000, 1.000000000000000000, 1.000000000000000000, 1.000000000000000000, 1.000000000000000000, 1.000000000000000000, 1.000000000000000000, 1.000000000000000000, 1.000000000000000000, 1.000000000000000000, 1.000000000000000000, 1.000000000000000000, 1.000000000000000000, 1.000000000000000000, 1.000000000000000000, 1.000000000000000000, 1.000000000000000000, 1.000000000000000000, 1.000000000000000000, 1.000000000000000000, 1.000000000000000000, 1.000000000000000000, 1.000000000000000000, 1.000000000000000000, 1.000000000000000000, 1.000000000000000000, 1.000000000000000000, 1.000000000000000000, 1.000000000000000000, 1.000000000000000000, 1.000000000000000000, 1.000000000000000000, 1.000000000000000000, 1.000000000000000000, 1.000000000000000000, 1.000000000000000000, 1.000000000000000000, 1.000000000000000000, 1.000000000000000000, 1.000000000000000000, 1.000000000000000000, 1.000000000000000000, 1.000000000000000000, 1.000000000000000000, 1.000000000000000000, 1.000000000000000000, 1.000000000000000000, 1.000000000000000000, 1.000000000000000000, 1.000000000000000000, 1.000000000000000000, 1.000000000000000000, 1.000000000000000000, 1.000000000000000000, 1.000000000000000000, 1.000000000000000000, 1.000000000000000000, 1.000000000000000000, 1.000000000000000000, 1.000000000000000000, 1.000000000000000000, 1.000000000000000000, 1.000000000000000000, 1.000000000000000000, 1.000000000000000000, 1.000000000000000000, 1.000000000000000000, 1.000000000000000000, 1.000000000000000000, 1.000000000000000000, 1.000000000000000000, 1.000000000000000000, 1.000000000000000000) ) ) 
 REPRESENTATION_ITEM ( '' )  SURFACE ( )  );
#93335 = STYLED_ITEM ( 'NONE', ( #9802 ), #51070 ) ;
#93336 = ORIENTED_EDGE ( 'NONE', *, *, #24958, .T. ) ;
#93337 = DIRECTION ( 'NONE',  ( 0.000000000000000000, 0.000000000000000000, -1.000000000000000000 ) ) ;
#93338 = CARTESIAN_POINT ( 'NONE',  ( -13.76503154704160714, -4.999999999998556710, -10.95334723230942942 ) ) ;
#93339 = EDGE_CURVE ( 'NONE', #45306, #2115, #46852, .T. ) ;
#93340 = CARTESIAN_POINT ( 'NONE',  ( 36.84999999999999432, 1.533819458162526451E-15, 0.000000000000000000 ) ) ;
#93341 = SURFACE_SIDE_STYLE ('',( #94410 ) ) ;
#93342 = ORIENTED_EDGE ( 'NONE', *, *, #95943, .T. ) ;
#93343 = DIRECTION ( 'NONE',  ( 0.000000000000000000, 0.000000000000000000, 1.000000000000000000 ) ) ;
#93344 = CARTESIAN_POINT ( 'NONE',  ( -83.74719587345013849, -57.67098913794580994, -27.91190304260424071 ) ) ;
#93345 = DIRECTION ( 'NONE',  ( -0.000000000000000000, 1.000000000000000000, -0.000000000000000000 ) ) ;
#93346 = DIRECTION ( 'NONE',  ( 0.000000000000000000, -1.000000000000000000, 0.000000000000000000 ) ) ;
#93347 = CARTESIAN_POINT ( 'NONE',  ( 23.38389609179547435, 28.08052868592283957, 30.70617127781017075 ) ) ;
#93348 = CARTESIAN_POINT ( 'NONE',  ( -13.53380759260212329, -51.99094200876919558, 30.58586009444553611 ) ) ;
#93349 = CARTESIAN_POINT ( 'NONE',  ( 44.46823338009918558, 5.000000000000003553, 0.000000000000000000 ) ) ;
#93350 = PRESENTATION_LAYER_ASSIGNMENT (  '', '', ( #64112 ) ) ;
#93351 = EDGE_CURVE ( 'NONE', #81772, #7556, #106740, .T. ) ;
#93352 = CARTESIAN_POINT ( 'NONE',  ( 101.2959083255158390, -29.99999999999995026, 104.2725399938968707 ) ) ;
#93353 = CARTESIAN_POINT ( 'NONE',  ( -79.87726071770381964, -29.99999999999996092, 191.0765191543576407 ) ) ;
#93354 = CARTESIAN_POINT ( 'NONE',  ( -57.84996654388071846, -60.33641506065911386, 76.30861162968490419 ) ) ;
#93355 = ORIENTED_EDGE ( 'NONE', *, *, #21549, .T. ) ;
#93356 = CARTESIAN_POINT ( 'NONE',  ( 5.744562646538031281, 13.26979259399947964, 4.000000000000000888 ) ) ;
#93357 = VERTEX_POINT ( 'NONE', #33416 ) ;
#93358 = CARTESIAN_POINT ( 'NONE',  ( -104.9459564440097381, -60.15519249609457830, 188.0231784350408475 ) ) ;
#93359 = CARTESIAN_POINT ( 'NONE',  ( 5.691929483231184861, 5.629165124598850767, -3.250000000000000444 ) ) ;
#93360 = CARTESIAN_POINT ( 'NONE',  ( -6.529218958540401907, 51.53898023814725349, 6.916366082103534652 ) ) ;
#93361 = FILL_AREA_STYLE_COLOUR ( '', #63061 ) ;
#93362 = ORIENTED_EDGE ( 'NONE', *, *, #85377, .T. ) ;
#93363 = CARTESIAN_POINT ( 'NONE',  ( 8.990409435383423187, -4.999999999999999112, -71.93151781320761984 ) ) ;
#93364 = B_SPLINE_CURVE_WITH_KNOTS ( 'NONE', 3,
 ( #32423, #64253, #31882, #64766, #97641, #65292, #23807, #56653, #24337, #89576, #68495, #76558, #51754, #1596, #43670, #93295, #2669, #100308, #10234, #35620, #59339, #84669, #99781, #74431, #101385, #34558, #42072, #91185, #26469, #19451, #67432, #83584, #92205, #66896 ),
 .UNSPECIFIED., .F., .F.,
 ( 4, 2, 2, 2, 2, 2, 2, 2, 2, 2, 2, 2, 2, 2, 2, 2, 4 ),
 ( 0.01272238763756221476, 0.01351613129786393211, 0.01430987495816564946, 0.01510361861846736681, 0.01589736227876908589, 0.01669110593907080498, 0.01748484959937252059, 0.01827859325967423967, 0.01907233691997595529, 0.01986608058027767437, 0.02065982424057938999, 0.02145356790088110907, 0.02224731156118282815, 0.02304105522148454377, 0.02383479888178626285, 0.02462854254208798194, 0.02542228620238969755 ),
 .UNSPECIFIED. ) ;
#93365 = CARTESIAN_POINT ( 'NONE',  ( -3.841398122528327352, -1.072224703192198536, 104.5835869663332574 ) ) ;
#93366 = CARTESIAN_POINT ( 'NONE',  ( -1.320432766682874540E-15, -13.90625000204838457, 7.188101187500000044 ) ) ;
#93367 = CARTESIAN_POINT ( 'NONE',  ( -0.08443874956765938522, 37.21016666119768246, -27.25000000000001066 ) ) ;
#93368 = CARTESIAN_POINT ( 'NONE',  ( 2.848917157793759055E-13, 44.08548369317517768, 16.24999999999732836 ) ) ;
#93369 = CARTESIAN_POINT ( 'NONE',  ( 11.24487389204834997, 0.000000000000000000, 12.81917055448515619 ) ) ;
#93370 = CARTESIAN_POINT ( 'NONE',  ( -11.72527720291174624, -4.890001682367673297, -12.55691480003112837 ) ) ;
#93371 = CARTESIAN_POINT ( 'NONE',  ( 20.52350613252515643, 304.8999024697870937, 9.947223320822450532 ) ) ;
#93372 =( BOUNDED_SURFACE ( )  B_SPLINE_SURFACE ( 3, 2, ( 
 ( #12128, #69851, #17188 ),
 ( #27310, #50061, #77941 ),
 ( #101683, #28907, #82970 ),
 ( #60192, #61781, #94676 ),
 ( #60713, #9064, #93059 ),
 ( #20823, #41971, #74854 ),
 ( #938, #52055, #47148 ),
 ( #31013, #88158, #62826 ),
 ( #71964, #71418, #56281 ),
 ( #30469, #63364, #96781 ),
 ( #88683, #47673, #70907 ),
 ( #31538, #104869, #14776 ) ),
 .UNSPECIFIED., .F., .F., .F. ) 
 B_SPLINE_SURFACE_WITH_KNOTS ( ( 4, 2, 2, 2, 2, 4 ),
 ( 3, 3 ),
 ( 1.348747502571967516E-16, 0.001914430196850316597, 0.002871645295275407350, 0.003828860393700498320, 0.005743290590550680259, 0.007657720787400862199 ),
 ( 0.000000000000000000, 1.000000000000000000 ),
 .UNSPECIFIED. ) 
 GEOMETRIC_REPRESENTATION_ITEM ( )  RATIONAL_B_SPLINE_SURFACE ( (
 ( 1.000000000000000000, 0.8904848454312670469, 1.000000000000000000),
 ( 1.000000000000000000, 0.8829463934862813446, 1.000000000000000000),
 ( 1.000000000000000000, 0.8737071328057678388, 1.000000000000000000),
 ( 1.000000000000000000, 0.8579777217483747220, 1.000000000000000000),
 ( 1.000000000000000000, 0.8524208109141675482, 1.000000000000000000),
 ( 1.000000000000000000, 0.8407737293550452407, 1.000000000000000000),
 ( 1.000000000000000000, 0.8346659945390565438, 1.000000000000000000),
 ( 1.000000000000000000, 0.8160698933129009180, 1.000000000000000000),
 ( 1.000000000000000000, 0.8031929192457759603, 1.000000000000000000),
 ( 1.000000000000000000, 0.7775868725374718293, 1.000000000000000000),
 ( 1.000000000000000000, 0.7647656555784809740, 1.000000000000000000),
 ( 1.000000000000000000, 0.7533433155455216967, 1.000000000000000000) ) ) 
 REPRESENTATION_ITEM ( '' )  SURFACE ( )  );
#93373 = CARTESIAN_POINT ( 'NONE',  ( -8.000000000000000000, -14.93750000409677092, -9.797174393178825657E-16 ) ) ;
#93374 = EDGE_CURVE ( 'NONE', #103131, #30746, #94270, .T. ) ;
#93375 = UNCERTAINTY_MEASURE_WITH_UNIT (LENGTH_MEASURE( 1.000000000000000082E-05 ), #93969, 'distance_accuracy_value', 'NONE');
#93376 = CARTESIAN_POINT ( 'NONE',  ( -31.02080448264273826, -22.13447804649420547, 30.33493143269389947 ) ) ;
#93377 = STYLED_ITEM ( 'NONE', ( #34937 ), #56232 ) ;
#93378 = SURFACE_STYLE_USAGE ( .BOTH. , #59965 ) ;
#93379 = CARTESIAN_POINT ( 'NONE',  ( 44.56484537913603106, -29.16031456794998888, 40.40432702718549507 ) ) ;
#93380 = AXIS2_PLACEMENT_3D ( 'NONE', #91387, #90848, #9367 ) ;
#93381 = CARTESIAN_POINT ( 'NONE',  ( -31.96903519139038963, 486.7815514870781044, 6.755070114922749447 ) ) ;
#93382 = CARTESIAN_POINT ( 'NONE',  ( -1.220105902931785113, 45.62896107045330041, 17.81534086607498324 ) ) ;
#93383 = COLOUR_RGB ( '', 0.66274510, 0.83137255, 0.94901961) ;
#93384 = B_SPLINE_CURVE_WITH_KNOTS ( 'NONE', 3,
 ( #10634, #52693, #102316, #85620, #2549, #19336, #11696, #3632, #84008, #1473, #83470, #42479, #68370, #28468, #92092, #60816 ),
 .UNSPECIFIED., .F., .F.,
 ( 4, 2, 2, 2, 2, 2, 2, 4 ),
 ( 1.398578778534940505E-17, 0.0003855832886952001220, 0.0007711665773903862578, 0.001156749866085572068, 0.001542333154780758421, 0.001927916443475944557, 0.002313499732171130259, 0.003084666309561404952 ),
 .UNSPECIFIED. ) ;
#93386 = ADVANCED_FACE ( 'NONE', ( #77042 ), #18849, .F. ) ;
#93385 = CARTESIAN_POINT ( 'NONE',  ( -89.02571210877493968, -38.53235496327626919, 200.2987166445973344 ) ) ;
#93387 = EDGE_LOOP ( 'NONE', ( #81499, #39153, #8677, #50393, #92966 ) ) ;
#93389 = CARTESIAN_POINT ( 'NONE',  ( 23.21751746555220564, -1.200000000000000030E-05, -30.70617127781077116 ) ) ;
#93388 = CARTESIAN_POINT ( 'NONE',  ( -16.10339698264861497, 21.83175592237823892, -0.8850307878645093940 ) ) ;
#93390 = CARTESIAN_POINT ( 'NONE',  ( 12.10323273576600478, 7.930126419769916168, -8.634503244510865372 ) ) ;
#93391 = CARTESIAN_POINT ( 'NONE',  ( -18.93991643217204057, 49.23433669341508789, 62.05747794209732859 ) ) ;
#93392 = CARTESIAN_POINT ( 'NONE',  ( -7.479729137166399866, 40.83274071714285469, -59.46320924800295415 ) ) ;
#93393 = CARTESIAN_POINT ( 'NONE',  ( 6.565384647267224594, 40.29402653084121511, -71.20315140851180047 ) ) ;
#93394 = DIRECTION ( 'NONE',  ( 1.000000000000000000, 0.000000000000000000, 0.000000000000000000 ) ) ;
#93395 = DIRECTION ( 'NONE',  ( 1.000000000000000000, 0.000000000000000000, 0.000000000000000000 ) ) ;
#93396 = CARTESIAN_POINT ( 'NONE',  ( 32.82168481641626556, 434.5290828238659628, 16.70238291264138653 ) ) ;
#93397 = CARTESIAN_POINT ( 'NONE',  ( 112.2015293769591580, -60.00000000000000711, 175.2242769347896569 ) ) ;
#93398 = DIRECTION ( 'NONE',  ( 0.000000000000000000, 0.000000000000000000, 1.000000000000000000 ) ) ;
#93399 = ORIENTED_EDGE ( 'NONE', *, *, #32427, .F. ) ;
#93400 = ADVANCED_FACE ( 'NONE', ( #18299 ), #88222, .T. ) ;
#93401 = CARTESIAN_POINT ( 'NONE',  ( 3.471301144393632576, -49.15628846923404183, 103.7432070447315908 ) ) ;
#93402 = CARTESIAN_POINT ( 'NONE',  ( -81.57395695671810643, -30.00000000000003908, -8.068917339165949443 ) ) ;
#93403 = ORIENTED_EDGE ( 'NONE', *, *, #27848, .T. ) ;
#93405 = DIRECTION ( 'NONE',  ( 0.000000000000000000, -1.000000000000000000, 0.000000000000000000 ) ) ;
#93404 = CARTESIAN_POINT ( 'NONE',  ( -62.80366873856288379, -38.34034637481484253, 105.3709165728642603 ) ) ;
#93406 = CARTESIAN_POINT ( 'NONE',  ( 93.39999999999999147, -4.171999999999998820, 5.616230220889773285E-16 ) ) ;
#93407 = DIRECTION ( 'NONE',  ( 0.000000000000000000, 0.000000000000000000, -1.000000000000000000 ) ) ;
#93408 = CARTESIAN_POINT ( 'NONE',  ( 7.090506028190232790, 41.24768140130692728, -58.61601156502441512 ) ) ;
#93409 = CARTESIAN_POINT ( 'NONE',  ( -5.082755093536326818, -14.09375000204838457, 5.082755093536325042 ) ) ;
#93410 = CARTESIAN_POINT ( 'NONE',  ( 7.374560640984048732, -5.000000000000002665, -75.40399789250147933 ) ) ;
#93411 = UNCERTAINTY_MEASURE_WITH_UNIT (LENGTH_MEASURE( 1.000000000000000082E-05 ), #46948, 'distance_accuracy_value', 'NONE');
#93412 = ORIENTED_EDGE ( 'NONE', *, *, #23726, .T. ) ;
#93413 = CARTESIAN_POINT ( 'NONE',  ( 79.80183204735519098, -60.35092112530382025, 173.0457402211850138 ) ) ;
#93414 = CARTESIAN_POINT ( 'NONE',  ( -3.713158817312831594, -1.053630055818222333, 103.2987150069905624 ) ) ;
#93415 = CARTESIAN_POINT ( 'NONE',  ( -6.999999999999999112, 0.000000000000000000, 0.000000000000000000 ) ) ;
#93416 = ORIENTED_EDGE ( 'NONE', *, *, #1204, .F. ) ;
#93417 = CONICAL_SURFACE ( 'NONE', #84787, 8.000000000000000000, 1.047197551196600296 ) ;
#93418 = CYLINDRICAL_SURFACE ( 'NONE', #6604, 4.000000000000000000 ) ;
#93419 = CARTESIAN_POINT ( 'NONE',  ( -46.79638705082423655, 18.85256363620330333, 15.38003188690398204 ) ) ;
#93420 = SURFACE_SIDE_STYLE ('',( #68628 ) ) ;
#93421 = DIRECTION ( 'NONE',  ( -1.000000000000000000, -0.000000000000000000, -0.000000000000000000 ) ) ;
#93422 = AXIS2_PLACEMENT_3D ( 'NONE', #11139, #3072, #91565 ) ;
#93423 = DIRECTION ( 'NONE',  ( 0.000000000000000000, 0.000000000000000000, 1.000000000000000000 ) ) ;
#93424 = CARTESIAN_POINT ( 'NONE',  ( 0.9433768135827877988, 17.83653422148033485, 49.67628854547170647 ) ) ;
#93425 = FACE_OUTER_BOUND ( 'NONE', #22024, .T. ) ;
#93426 = EDGE_CURVE ( 'NONE', #81048, #9279, #74412, .T. ) ;
#93427 = VERTEX_POINT ( 'NONE', #60356 ) ;
#93428 = SURFACE_SIDE_STYLE ('',( #78812 ) ) ;
#93430 = CARTESIAN_POINT ( 'NONE',  ( -2.587146340238325681, 300.7568995495286686, 9.662447471766515861 ) ) ;
#93429 = VECTOR ( 'NONE', #14403, 1000.000000000000000 ) ;
#93431 = CARTESIAN_POINT ( 'NONE',  ( 26.50079164159988210, 18.64284798592797188, 27.83217509638787490 ) ) ;
#93432 = LINE ( 'NONE', #58938, #30443 ) ;
#93433 = EDGE_CURVE ( 'NONE', #30487, #10075, #26112, .T. ) ;
#93435 = SURFACE_SIDE_STYLE ('',( #12486 ) ) ;
#93434 = DIRECTION ( 'NONE',  ( 0.000000000000000000, -0.3420201433256733758, -0.9396926207859066515 ) ) ;
#93436 = CARTESIAN_POINT ( 'NONE',  ( 2.977408999572651815, -28.43750000204839168, 7.188101187500000933 ) ) ;
#93437 = CARTESIAN_POINT ( 'NONE',  ( 6.683837171061806082, -3.955946848495971668, -6.851900933636991375 ) ) ;
#93438 = APPLICATION_CONTEXT ( 'automotive_design' ) ;
#93439 = DIRECTION ( 'NONE',  ( -0.000000000000000000, -1.000000000000000000, -0.000000000000000000 ) ) ;
#93440 = DIRECTION ( 'NONE',  ( -1.000000000000000000, -1.224606353822377258E-16, -0.000000000000000000 ) ) ;
#93441 = CONTEXT_DEPENDENT_SHAPE_REPRESENTATION ( #76248, #53698 ) ;
#93442 = ORIENTED_EDGE ( 'NONE', *, *, #99094, .T. ) ;
#93443 = EDGE_CURVE ( 'NONE', #22430, #6957, #60877, .T. ) ;
#93444 = DIRECTION ( 'NONE',  ( -1.000000000000000000, -1.224606353822377258E-16, -0.000000000000000000 ) ) ;
#93445 =( NAMED_UNIT ( * ) SI_UNIT ( $, .STERADIAN. ) SOLID_ANGLE_UNIT ( ) );
#93446 = AXIS2_PLACEMENT_3D ( 'NONE', #71638, #46843, #71121 ) ;
#93447 = DIRECTION ( 'NONE',  ( -0.7071067811865315855, 8.659560562355127608E-17, -0.7071067811865634489 ) ) ;
#93448 = B_SPLINE_CURVE_WITH_KNOTS ( 'NONE', 3,
 ( #98955, #75217, #49887, #83851 ),
 .UNSPECIFIED., .F., .F.,
 ( 4, 4 ),
 ( 0.0005341934512451263070, 0.02813855774923773589 ),
 .UNSPECIFIED. ) ;
#93449 =( GEOMETRIC_REPRESENTATION_CONTEXT ( 3 ) GLOBAL_UNCERTAINTY_ASSIGNED_CONTEXT ( ( #96355 ) ) GLOBAL_UNIT_ASSIGNED_CONTEXT ( ( #38133, #54245, #55317 ) ) REPRESENTATION_CONTEXT ( 'NONE', 'WORKASPACE' ) );
#93450 = VERTEX_POINT ( 'NONE', #26413 ) ;
#93451 = CARTESIAN_POINT ( 'NONE',  ( 8.000000000000000000, -16.99999999999999289, 0.000000000000000000 ) ) ;
#93452 = CARTESIAN_POINT ( 'NONE',  ( -8.904581707870004692, 48.00000000000000000, -97.29851715191085759 ) ) ;
#93453 = CIRCLE ( 'NONE', #40004, 5.000000000000011546 ) ;
#93454 = EDGE_LOOP ( 'NONE', ( #59407, #61821, #103980, #1333, #87897 ) ) ;
#93455 = CARTESIAN_POINT ( 'NONE',  ( 32.74193221581197832, 435.3845808012915768, 16.94201410894484994 ) ) ;
#93456 = CARTESIAN_POINT ( 'NONE',  ( -0.3043501477677958422, 13.62703061655916947, -49.28168406113174171 ) ) ;
#93457 = CARTESIAN_POINT ( 'NONE',  ( -33.85195725564127400, 465.2464970902067307, 17.18122764674263436 ) ) ;
#93458 = CARTESIAN_POINT ( 'NONE',  ( -17.86210361494380905, 36.33998000098822700, 23.65466217301429452 ) ) ;
#93459 = UNCERTAINTY_MEASURE_WITH_UNIT (LENGTH_MEASURE( 1.000000000000000082E-05 ), #86710, 'distance_accuracy_value', 'NONE');
#93460 = CARTESIAN_POINT ( 'NONE',  ( -101.8030891146729289, -60.00000000000000000, 201.2278047307587201 ) ) ;
#93461 = CARTESIAN_POINT ( 'NONE',  ( 19.49880643229863253, 49.99998348590667518, 59.93398820729930065 ) ) ;
#93463 = CIRCLE ( 'NONE', #46941, 4.000000000000000888 ) ;
#93462 = DIRECTION ( 'NONE',  ( 1.000000000000000000, 0.000000000000000000, 0.000000000000000000 ) ) ;
#93464 = CARTESIAN_POINT ( 'NONE',  ( 0.000000000000000000, 45.50000000000000711, 60.00000000000000000 ) ) ;
#93465 = DIRECTION ( 'NONE',  ( 0.000000000000000000, 0.000000000000000000, 1.000000000000000000 ) ) ;
#93466 = CARTESIAN_POINT ( 'NONE',  ( -86.18086450786695707, -21.36838705098882230, 176.9395935000053441 ) ) ;
#93467 = ORIENTED_EDGE ( 'NONE', *, *, #61347, .F. ) ;
#93468 = DIRECTION ( 'NONE',  ( 0.000000000000000000, 0.000000000000000000, -1.000000000000000000 ) ) ;
#93469 = EDGE_CURVE ( 'NONE', #80696, #23441, #311, .T. ) ;
#93470 = CARTESIAN_POINT ( 'NONE',  ( 1.000000000000000000, -43.18879712712265473, 0.3952393630211145092 ) ) ;
#93471 = CARTESIAN_POINT ( 'NONE',  ( -85.33252481412877444, -52.70932741134135568, 1.350972571353141971 ) ) ;
#93472 = FACE_OUTER_BOUND ( 'NONE', #8868, .T. ) ;
#93473 =( NAMED_UNIT ( * ) SI_UNIT ( $, .STERADIAN. ) SOLID_ANGLE_UNIT ( ) );
#93474 = CARTESIAN_POINT ( 'NONE',  ( 9.300358455898974697, 140.6343319111079779, 3.070077524146086535E-13 ) ) ;
#93475 = CARTESIAN_POINT ( 'NONE',  ( 26.69900261086841198, 1.482358050883964840E-15, 0.000000000000000000 ) ) ;
#93476 = CARTESIAN_POINT ( 'NONE',  ( -36.40416150969235787, 41.99999999991774757, -47.37019975554808582 ) ) ;
#93477 = EDGE_CURVE ( 'NONE', #57235, #21935, #23484, .T. ) ;
#93478 = CARTESIAN_POINT ( 'NONE',  ( 62.54367487775790124, -59.99999999999994316, 118.0935059193921575 ) ) ;
#93479 = CARTESIAN_POINT ( 'NONE',  ( -26.13315753361836613, 60.33964880548970910, 13.06657876680918307 ) ) ;
#93480 = CARTESIAN_POINT ( 'NONE',  ( -82.45890327043613865, -29.99999999999992184, -23.17447414549992146 ) ) ;
#93481 = CARTESIAN_POINT ( 'NONE',  ( -69.00208524908248364, -32.53704488351955604, 94.70596908067794573 ) ) ;
#93482 = ORIENTED_EDGE ( 'NONE', *, *, #72350, .T. ) ;
#93483 = CARTESIAN_POINT ( 'NONE',  ( 78.95048871113250755, -29.99999999999999645, 188.4614743794136871 ) ) ;
#93484 =( NAMED_UNIT ( * ) PLANE_ANGLE_UNIT ( ) SI_UNIT ( $, .RADIAN. ) );
#93485 = CARTESIAN_POINT ( 'NONE',  ( 28.72931389660035251, -59.99999999999750599, 45.02702490174896610 ) ) ;
#93486 = ORIENTED_EDGE ( 'NONE', *, *, #61492, .F. ) ;
#93487 = CARTESIAN_POINT ( 'NONE',  ( 15.38483753811592969, -5.586071175641518671, 13.93514129277331115 ) ) ;
#93488 = CARTESIAN_POINT ( 'NONE',  ( 2.977408999572652260, -24.31250000204838813, 7.188101187500000044 ) ) ;
#93489 = VECTOR ( 'NONE', #89505, 1000.000000000000000 ) ;
#93490 = ADVANCED_FACE ( 'NONE', ( #11762 ), #3702, .T. ) ;
#93491 = CARTESIAN_POINT ( 'NONE',  ( 34.83349330513380693, 1.593028355512270962E-15, 0.000000000000000000 ) ) ;
#93492 = ORIENTED_EDGE ( 'NONE', *, *, #37630, .F. ) ;
#93493 = CARTESIAN_POINT ( 'NONE',  ( -16.14595037822608603, 6.785770140112291848, -6.193810554583039973 ) ) ;
#93494 = VERTEX_POINT ( 'NONE', #31575 ) ;
#93495 = DIRECTION ( 'NONE',  ( -1.000000000000000000, -0.000000000000000000, -0.000000000000000000 ) ) ;
#93496 =( GEOMETRIC_REPRESENTATION_CONTEXT ( 3 ) GLOBAL_UNCERTAINTY_ASSIGNED_CONTEXT ( ( #84479 ) ) GLOBAL_UNIT_ASSIGNED_CONTEXT ( ( #77512, #12225, #37085 ) ) REPRESENTATION_CONTEXT ( 'NONE', 'WORKASPACE' ) );
#93497 = DIRECTION ( 'NONE',  ( 1.000000000000000000, -0.000000000000000000, -0.000000000000000000 ) ) ;
#93498 = CARTESIAN_POINT ( 'NONE',  ( -75.70276281760169468, -59.99999999999019451, 193.8926945017304888 ) ) ;
#93499 = CARTESIAN_POINT ( 'NONE',  ( -10.92659744279963441, 43.17638622626457590, 15.23462367102720805 ) ) ;
#93500 = CARTESIAN_POINT ( 'NONE',  ( 2.977408999572651815, -30.31250000204838813, 7.188101187500000933 ) ) ;
#93501 = CARTESIAN_POINT ( 'NONE',  ( -49.27914886956171614, 13.08292563505592376, 15.56788460764650317 ) ) ;
#93502 =( GEOMETRIC_REPRESENTATION_CONTEXT ( 3 ) GLOBAL_UNCERTAINTY_ASSIGNED_CONTEXT ( ( #47362 ) ) GLOBAL_UNIT_ASSIGNED_CONTEXT ( ( #81869, #74322, #42493 ) ) REPRESENTATION_CONTEXT ( 'NONE', 'WORKASPACE' ) );
#93503 = CARTESIAN_POINT ( 'NONE',  ( 11.17734400176826171, -4.285714285714296246, -22.67073868809949033 ) ) ;
#93504 = DIRECTION ( 'NONE',  ( -0.000000000000000000, 1.000000000000000000, -0.000000000000000000 ) ) ;
#93505 = CARTESIAN_POINT ( 'NONE',  ( -12.48571098547292912, -3.549409519532933377, -13.69689515574851058 ) ) ;
#93506 = CARTESIAN_POINT ( 'NONE',  ( 37.62251730745840206, 437.3427388312646826, 4.535622330043183048 ) ) ;
#93507 = EDGE_CURVE ( 'NONE', #27343, #91446, #76113, .T. ) ;
#93508 = VERTEX_POINT ( 'NONE', #56323 ) ;
#93509 = CARTESIAN_POINT ( 'NONE',  ( -7.320748600891240798, 41.41789230214724427, -68.91429205797308555 ) ) ;
#93510 = AXIS2_PLACEMENT_3D ( 'NONE', #82086, #73997, #75051 ) ;
#93512 = CARTESIAN_POINT ( 'NONE',  ( 31.39243574302858519, -29.07687128735913618, 31.74798812421044403 ) ) ;
#93511 = CARTESIAN_POINT ( 'NONE',  ( 4.958567106242401934, 52.14947999179454996, -6.064245278518590965 ) ) ;
#93513 = ORIENTED_EDGE ( 'NONE', *, *, #4941, .T. ) ;
#93514 = EDGE_CURVE ( 'NONE', #1802, #9641, #82969, .T. ) ;
#93515 = CARTESIAN_POINT ( 'NONE',  ( -2.617478843592799365, 48.00000000000000000, -94.73972676668314818 ) ) ;
#93517 = CARTESIAN_POINT ( 'NONE',  ( -28.76346532419124458, 309.5219921958590135, -8.933260212751790164 ) ) ;
#93516 = CARTESIAN_POINT ( 'NONE',  ( 33.00000000000000000, 489.5971041675262541, 10.80646835458729349 ) ) ;
#93518 = CARTESIAN_POINT ( 'NONE',  ( 0.000000000000000000, 0.000000000000000000, -25.03750572909317285 ) ) ;
#93519 = CARTESIAN_POINT ( 'NONE',  ( -33.65518112486073221, 435.5968223796347161, 8.977797139137742022 ) ) ;
#93520 = DIRECTION ( 'NONE',  ( 1.000000000000000000, 0.000000000000000000, 0.000000000000000000 ) ) ;
#93521 = CARTESIAN_POINT ( 'NONE',  ( -7.500000000000000888, -3.608439182435170700, -7.298562697733109061 ) ) ;
#93522 = EDGE_LOOP ( 'NONE', ( #76663, #48744, #43586, #100007 ) ) ;
#93523 = CARTESIAN_POINT ( 'NONE',  ( 92.01402115998416775, -60.00000000000000000, 5.925301312853033409 ) ) ;
#93524 = CARTESIAN_POINT ( 'NONE',  ( 86.17777777777776294, 4.172000000000019249, 5.109226446042768454E-16 ) ) ;
#93525 = FILL_AREA_STYLE ('',( #12051 ) ) ;
#93526 = CARTESIAN_POINT ( 'NONE',  ( -5.290067270632282437, 54.20842449845790867, 6.031152949371105798 ) ) ;
#93527 = CIRCLE ( 'NONE', #72846, 4.000000000000000888 ) ;
#93528 = CARTESIAN_POINT ( 'NONE',  ( -6.035340075855088138, 41.06696377143527599, -71.06135861415590682 ) ) ;
#93529 = CARTESIAN_POINT ( 'NONE',  ( -47.44667293595283297, 16.35698112199736443, -16.71846647949800513 ) ) ;
#93530 = VERTEX_POINT ( 'NONE', #19924 ) ;
#93531 = CARTESIAN_POINT ( 'NONE',  ( -109.1611028234465692, -29.99999999994022559, 160.9843952204544735 ) ) ;
#93532 = VERTEX_POINT ( 'NONE', #36628 ) ;
#93533 = CARTESIAN_POINT ( 'NONE',  ( 5.656854249492380582, -10.81249999999999289, -5.656854249492379694 ) ) ;
#93534 =( NAMED_UNIT ( * ) SI_UNIT ( $, .STERADIAN. ) SOLID_ANGLE_UNIT ( ) );
#93535 = FACE_OUTER_BOUND ( 'NONE', #56838, .T. ) ;
#93536 = CARTESIAN_POINT ( 'NONE',  ( 16.10103572754711720, 21.87195731844753865, -0.4457938393851405556 ) ) ;
#93537 = CARTESIAN_POINT ( 'NONE',  ( 86.24207113919420920, -60.22626128449206107, -13.36701399825027181 ) ) ;
#93538 = AXIS2_PLACEMENT_3D ( 'NONE', #37849, #71750, #95005 ) ;
#93539 = CARTESIAN_POINT ( 'NONE',  ( -36.05680654074119929, 304.0840038173946027, 0.1264612662495986917 ) ) ;
#93540 = CARTESIAN_POINT ( 'NONE',  ( 27.02022815836235026, 1.340359594676612611E-15, 0.000000000000000000 ) ) ;
#93541 = CARTESIAN_POINT ( 'NONE',  ( -17.08484820656748226, 34.19635467231778136, 24.27347930919938435 ) ) ;
#93542 = ORIENTED_EDGE ( 'NONE', *, *, #105815, .F. ) ;
#93543 =( BOUNDED_SURFACE ( )  B_SPLINE_SURFACE ( 3, 2, ( 
 ( #95549, #63191, #54526 ),
 ( #5474, #28729, #87470 ),
 ( #13551, #61616, #29267 ),
 ( #94509, #46469, #20661 ),
 ( #62149, #53500, #95039 ),
 ( #38399, #69169, #71264 ),
 ( #20117, #28203, #104158 ),
 ( #30303, #96084, #3359 ),
 ( #93966, #36303, #73908 ),
 ( #15677, #48566, #24861 ),
 ( #40489, #46983, #65300 ),
 ( #7052, #88525, #23815 ) ),
 .UNSPECIFIED., .F., .F., .F. ) 
 B_SPLINE_SURFACE_WITH_KNOTS ( ( 4, 2, 2, 2, 2, 4 ),
 ( 3, 3 ),
 ( 4.683753385137379155E-17, 0.005139846902489559645, 0.005782327765300748421, 0.006424808628111938064, 0.007709770353734315615, 0.01027969380497907245 ),
 ( 0.000000000000000000, 1.000000000000000000 ),
 .UNSPECIFIED. ) 
 GEOMETRIC_REPRESENTATION_ITEM ( )  RATIONAL_B_SPLINE_SURFACE ( (
 ( 1.000000000000000000, 0.7071066567438660799, 1.000000000000000000),
 ( 1.000000000000000000, 0.7071033644331966572, 1.000000000000000000),
 ( 1.000000000000000000, 0.7071056776559211388, 1.000000000000000000),
 ( 1.000000000000000000, 0.7071068248477218043, 1.000000000000000000),
 ( 1.000000000000000000, 0.7071068712035362136, 1.000000000000000000),
 ( 1.000000000000000000, 0.7071037121013128424, 1.000000000000000000),
 ( 1.000000000000000000, 0.7071011173528390925, 1.000000000000000000),
 ( 1.000000000000000000, 0.7070931233498599644, 1.000000000000000000),
 ( 1.000000000000000000, 0.7070878535667373121, 1.000000000000000000),
 ( 1.000000000000000000, 0.7070844239726482572, 1.000000000000000000),
 ( 1.000000000000000000, 0.7071028727339059294, 1.000000000000000000),
 ( 1.000000000000000000, 0.7071067811865477948, 1.000000000000000000) ) ) 
 REPRESENTATION_ITEM ( '' )  SURFACE ( )  );
#93544 = EDGE_CURVE ( 'NONE', #2998, #64476, #88201, .T. ) ;
#93545 = CARTESIAN_POINT ( 'NONE',  ( -6.499999999999998224, 4.012863338656268652, -6.470131626772280597 ) ) ;
#93546 = VERTEX_POINT ( 'NONE', #72006 ) ;
#93547 = DIRECTION ( 'NONE',  ( 4.547071256508659128E-15, -0.6177654251575146471, -0.7863624351912771315 ) ) ;
#93549 = VERTEX_POINT ( 'NONE', #104916 ) ;
#93548 = CARTESIAN_POINT ( 'NONE',  ( 6.388342523666968198, 51.65549266189224653, 6.605009197188880243 ) ) ;
#93550 = CARTESIAN_POINT ( 'NONE',  ( 70.97006384286886771, -39.48593960573443695, 105.0516801013103105 ) ) ;
#93551 = VERTEX_POINT ( 'NONE', #31058 ) ;
#93552 = CARTESIAN_POINT ( 'NONE',  ( 4.243523009780798994, -48.34445764549300151, 43.36978758336660178 ) ) ;
#93553 = CARTESIAN_POINT ( 'NONE',  ( 2.977408999572650927, -26.37500000204838457, -7.188101187500000933 ) ) ;
#93554 = CARTESIAN_POINT ( 'NONE',  ( -84.33710589588049800, -57.55216090540037044, 201.9444809301270141 ) ) ;
#93555 = ADVANCED_FACE ( 'NONE', ( #52766 ), #96822, .F. ) ;
#93556 = EDGE_LOOP ( 'NONE', ( #52862, #16445, #55721, #103472, #517, #105433, #83040, #38345 ) ) ;
#93557 = EDGE_CURVE ( 'NONE', #32543, #52389, #41530, .T. ) ;
#93558 = CARTESIAN_POINT ( 'NONE',  ( 103.4806006637074489, -45.28272409703987478, 182.5790420555011053 ) ) ;
#93559 = CARTESIAN_POINT ( 'NONE',  ( -36.95430024838550764, 27.83259845835024393, -13.30727799284015411 ) ) ;
#93560 = EDGE_CURVE ( 'NONE', #65774, #59097, #52013, .T. ) ;
#93561 = DIRECTION ( 'NONE',  ( -1.000000000000000000, 0.000000000000000000, 0.000000000000000000 ) ) ;
#93562 = CARTESIAN_POINT ( 'NONE',  ( 5.656854249492378806, -17.37500000409676915, 5.656854249492381470 ) ) ;
#93563 = CARTESIAN_POINT ( 'NONE',  ( -49.78251962175088607, -29.64715986801754610, 46.26550681513847252 ) ) ;
#93564 = CARTESIAN_POINT ( 'NONE',  ( 9.948688207305211861, 246.1297685050980704, -1.044946705213434690 ) ) ;
#93565 = AXIS2_PLACEMENT_3D ( 'NONE', #104486, #16544, #56988 ) ;
#93566 = CARTESIAN_POINT ( 'NONE',  ( 0.000000000000000000, 0.000000000000000000, -13.00000000000000000 ) ) ;
#93567 = CARTESIAN_POINT ( 'NONE',  ( -43.50377727019363761, 435.9167426301696651, 18.24083946424746117 ) ) ;
#93568 = CARTESIAN_POINT ( 'NONE',  ( 76.88291765283142354, 410.1183258646226477, 267.1969486013077244 ) ) ;
#93569 = CARTESIAN_POINT ( 'NONE',  ( 6.245865719273044903, -30.00000000000000000, -3.919462879779509024 ) ) ;
#93570 = ORIENTED_EDGE ( 'NONE', *, *, #11769, .F. ) ;
#93571 = CARTESIAN_POINT ( 'NONE',  ( -3.121913957742261658, -49.49713245390870497, 40.80120573642129500 ) ) ;
#93572 = EDGE_CURVE ( 'NONE', #9732, #65010, #96764, .T. ) ;
#93573 = CARTESIAN_POINT ( 'NONE',  ( 11.04959452034190903, -4.985681094987538309, -12.57702150655598849 ) ) ;
#93574 = FACE_OUTER_BOUND ( 'NONE', #27086, .T. ) ;
#93575 = CARTESIAN_POINT ( 'NONE',  ( -85.49392800990823105, -30.00000000000000355, 174.7729343606026475 ) ) ;
#93576 = ORIENTED_EDGE ( 'NONE', *, *, #39019, .F. ) ;
#93577 = LINE ( 'NONE', #54145, #4811 ) ;
#93578 =( GEOMETRIC_REPRESENTATION_CONTEXT ( 3 ) GLOBAL_UNCERTAINTY_ASSIGNED_CONTEXT ( ( #55786 ) ) GLOBAL_UNIT_ASSIGNED_CONTEXT ( ( #40850, #99074, #50007 ) ) REPRESENTATION_CONTEXT ( 'NONE', 'WORKASPACE' ) );
#93579 = CARTESIAN_POINT ( 'NONE',  ( 81.11165248383676385, -57.51401271914193813, 199.8270164379141249 ) ) ;
#93580 = CARTESIAN_POINT ( 'NONE',  ( 46.00000000000002132, 436.0213184034679443, 14.35141020368345366 ) ) ;
#93581 = CARTESIAN_POINT ( 'NONE',  ( 37.51403724872147194, -32.16046718318631292, -37.67293210278931781 ) ) ;
#93582 = CARTESIAN_POINT ( 'NONE',  ( 7.500000000000000000, -4.999999999999999112, -20.99851272547259384 ) ) ;
#93583 = CARTESIAN_POINT ( 'NONE',  ( 38.09999999999999432, -3.309499999999999886, 0.000000000000000000 ) ) ;
#93584 = CARTESIAN_POINT ( 'NONE',  ( -66.45734036689610491, -60.00000000000001421, 124.2522409290889271 ) ) ;
#93585 = CARTESIAN_POINT ( 'NONE',  ( -86.63543225537370063, -20.69559410499708818, 184.5538921392410430 ) ) ;
#93587 = ORIENTED_EDGE ( 'NONE', *, *, #29244, .T. ) ;
#93586 = AXIS2_PLACEMENT_3D ( 'NONE', #97491, #98040, #24190 ) ;
#93588 = LINE ( 'NONE', #60184, #95276 ) ;
#93589 = CARTESIAN_POINT ( 'NONE',  ( -4.087803312211714335, -49.92081496441304012, 32.20210259524810681 ) ) ;
#93590 = CARTESIAN_POINT ( 'NONE',  ( -6.771649247693060758, 41.86512631648978555, -59.59160522040796337 ) ) ;
#93591 = CARTESIAN_POINT ( 'NONE',  ( -3.096826397206294601, -49.41329697661214482, 103.2812258104289640 ) ) ;
#93592 = AXIS2_PLACEMENT_3D ( 'NONE', #91925, #76265, #67125 ) ;
#93594 = DIRECTION ( 'NONE',  ( 0.000000000000000000, 0.000000000000000000, -1.000000000000000000 ) ) ;
#93593 = CARTESIAN_POINT ( 'NONE',  ( 33.74977848768428146, 477.7786480585253912, 4.002244379145972530 ) ) ;
#93595 = ORIENTED_EDGE ( 'NONE', *, *, #51954, .F. ) ;
#93596 = ADVANCED_FACE ( 'NONE', ( #57928 ), #86463, .T. ) ;
#93597 = CARTESIAN_POINT ( 'NONE',  ( 7.500000000000007105, 11.33333333333401427, -68.91429205785459544 ) ) ;
#93598 = AXIS2_PLACEMENT_3D ( 'NONE', #43946, #42881, #34830 ) ;
#93599 = DIRECTION ( 'NONE',  ( 1.000000000000000000, 0.000000000000000000, -0.000000000000000000 ) ) ;
#93600 = CARTESIAN_POINT ( 'NONE',  ( 0.8395943188471228780, 28.08659877555713180, 38.57031298532696439 ) ) ;
#93601 = DIRECTION ( 'NONE',  ( 0.8660254037844380415, 0.5000000000000011102, 0.000000000000000000 ) ) ;
#93602 = CARTESIAN_POINT ( 'NONE',  ( 25.34756200978462815, 295.7221099550690155, -1.813076239403205836 ) ) ;
#93603 = CARTESIAN_POINT ( 'NONE',  ( 35.44563196690202744, 355.0508310518326311, 1.542887188894044526 ) ) ;
#93604 = EDGE_CURVE ( 'NONE', #41649, #65228, #32636, .T. ) ;
#93605 = EDGE_CURVE ( 'NONE', #59016, #11977, #17504, .T. ) ;
#93606 = DIRECTION ( 'NONE',  ( 1.000000000000000000, 0.000000000000000000, -0.000000000000000000 ) ) ;
#93607 = FACE_OUTER_BOUND ( 'NONE', #100751, .T. ) ;
#93608 = CARTESIAN_POINT ( 'NONE',  ( 92.59918368926680898, -29.99999999999998224, 50.96418643717338881 ) ) ;
#93609 = CARTESIAN_POINT ( 'NONE',  ( -83.49067641280694829, -22.15006867442743754, 148.6564140083872303 ) ) ;
#93610 = ORIENTED_EDGE ( 'NONE', *, *, #91949, .T. ) ;
#93611 = LINE ( 'NONE', #36474, #37848 ) ;
#93612 = DIRECTION ( 'NONE',  ( -0.000000000000000000, -1.000000000000000000, -0.000000000000000000 ) ) ;
#93613 = CARTESIAN_POINT ( 'NONE',  ( 57.99551341713360841, -57.67649500090644210, 100.6097491013691609 ) ) ;
#93614 = DIRECTION ( 'NONE',  ( 0.3048027540940115299, 0.4519649026942716974, -0.8383453988835765092 ) ) ;
#93615 = CARTESIAN_POINT ( 'NONE',  ( 40.16383914097482943, 315.4761916235045192, 2.976046483704458900 ) ) ;
#93616 = CARTESIAN_POINT ( 'NONE',  ( 0.000000000000000000, 0.000000000000000000, -7.657127082228716297 ) ) ;
#93617 = ORIENTED_EDGE ( 'NONE', *, *, #73094, .T. ) ;
#93618 = UNCERTAINTY_MEASURE_WITH_UNIT (LENGTH_MEASURE( 1.000000000000000082E-05 ), #68278, 'distance_accuracy_value', 'NONE');
#93619 = CARTESIAN_POINT ( 'NONE',  ( 4.036442205379928261, 54.13912236062702732, -7.152865674426393205 ) ) ;
#93620 = CARTESIAN_POINT ( 'NONE',  ( 31.31637074175829127, 438.7955421674503214, 22.44423981995848294 ) ) ;
#93621 = CARTESIAN_POINT ( 'NONE',  ( 4.401442555609581635E-16, -29.28125000204838813, -7.188101187500000044 ) ) ;
#93622 = EDGE_LOOP ( 'NONE', ( #97335, #17648, #23382, #97722 ) ) ;
#93623 = EDGE_CURVE ( 'NONE', #104941, #77653, #67509, .T. ) ;
#93624 = CARTESIAN_POINT ( 'NONE',  ( 3.400000000000000355, 0.000000000000000000, -6.123524522925831270 ) ) ;
#93625 = CARTESIAN_POINT ( 'NONE',  ( 6.629186139556361823, 41.56975587237539571, -70.49374931123308841 ) ) ;
#93626 = CARTESIAN_POINT ( 'NONE',  ( -61.09659575455685143, 50.00000000000000000, -16.41787579824995902 ) ) ;
#93627 = B_SPLINE_CURVE_WITH_KNOTS ( 'NONE', 3,
 ( #20958, #28493, #46242, #27977, #61377, #37658, #12267, #86719 ),
 .UNSPECIFIED., .F., .F.,
 ( 4, 2, 2, 4 ),
 ( 0.02179091314793461798, 0.02376333058066960879, 0.02573574801340459961, 0.02968058287887458471 ),
 .UNSPECIFIED. ) ;
#93628 = CARTESIAN_POINT ( 'NONE',  ( 12.50000000000000533, -3.000000000000000888, -55.91956093573309516 ) ) ;
#93629 = EDGE_CURVE ( 'NONE', #103302, #52464, #79585, .T. ) ;
#93630 = DIRECTION ( 'NONE',  ( 0.9502668926229327351, 0.000000000000000000, 0.3114367235647647614 ) ) ;
#93631 = VERTEX_POINT ( 'NONE', #82748 ) ;
#93632 = CARTESIAN_POINT ( 'NONE',  ( 22.21354712676404830, -60.00000000000001421, -41.66341169407889566 ) ) ;
#93634 = CARTESIAN_POINT ( 'NONE',  ( 23.00510670403769709, -56.87329948538524604, 34.33241275911512247 ) ) ;
#93633 = CARTESIAN_POINT ( 'NONE',  ( -43.57786082180619047, -59.99999999999987921, 62.86006299602857439 ) ) ;
#93635 = CARTESIAN_POINT ( 'NONE',  ( 55.68167212273443312, 51.11204936430952017, -27.84083606136720945 ) ) ;
#93636 = EDGE_CURVE ( 'NONE', #49140, #33725, #35069, .T. ) ;
#93637 = CARTESIAN_POINT ( 'NONE',  ( -34.08206426064871408, -29.10158233164262853, 32.84525425997023973 ) ) ;
#93638 = UNCERTAINTY_MEASURE_WITH_UNIT (LENGTH_MEASURE( 1.000000000000000082E-05 ), #32748, 'distance_accuracy_value', 'NONE');
#93639 = ORIENTED_EDGE ( 'NONE', *, *, #91283, .T. ) ;
#93640 = DIRECTION ( 'NONE',  ( 0.000000000000000000, 1.000000000000000000, -0.000000000000000000 ) ) ;
#93641 = CARTESIAN_POINT ( 'NONE',  ( -5.596957125887387363, -47.31575451833741397, 103.9718581041641698 ) ) ;
#93642 = CIRCLE ( 'NONE', #47028, 7.000000000000000000 ) ;
#93643 = CARTESIAN_POINT ( 'NONE',  ( 46.00000000000000000, 450.0000000000002274, 28.20242257375372219 ) ) ;
#93644 = EDGE_CURVE ( 'NONE', #58764, #33833, #19356, .T. ) ;
#93645 = CARTESIAN_POINT ( 'NONE',  ( 7.002619243997878939, -63.94992681986182248, -3.868708944013000917 ) ) ;
#93646 = CARTESIAN_POINT ( 'NONE',  ( -15.05785784214257284, 3.824195276785038011, 4.604276673521291663 ) ) ;
#93647 = ORIENTED_EDGE ( 'NONE', *, *, #35422, .T. ) ;
#93648 = PRESENTATION_STYLE_ASSIGNMENT (( #58620 ) ) ;
#93649 = EDGE_LOOP ( 'NONE', ( #27998, #81916, #6931, #29876 ) ) ;
#93650 = CARTESIAN_POINT ( 'NONE',  ( 98.69640391454856854, -29.99999999999997868, 189.4887148491113180 ) ) ;
#93651 = CARTESIAN_POINT ( 'NONE',  ( 42.29757377725155010, 39.52300599983767171, -49.89852198136856742 ) ) ;
#93652 = VECTOR ( 'NONE', #27441, 1000.000000000000000 ) ;
#93653 = DIRECTION ( 'NONE',  ( 0.000000000000000000, -1.000000000000000000, 0.000000000000000000 ) ) ;
#93654 = CARTESIAN_POINT ( 'NONE',  ( 81.33220965908822109, -30.00000000000000000, -0.9688136936568159108 ) ) ;
#93655 = FILL_AREA_STYLE_COLOUR ( '', #29530 ) ;
#93656 = ORIENTED_EDGE ( 'NONE', *, *, #55813, .F. ) ;
#93657 = ORIENTED_EDGE ( 'NONE', *, *, #24251, .F. ) ;
#93658 = ORIENTED_EDGE ( 'NONE', *, *, #15452, .T. ) ;
#93659 = CARTESIAN_POINT ( 'NONE',  ( -32.03420920423447882, 464.8550977446592469, 13.91744750518814655 ) ) ;
#93660 = CARTESIAN_POINT ( 'NONE',  ( 3.400000000000000355, 0.000000000000000000, -5.283275477074182547 ) ) ;
#93661 = CARTESIAN_POINT ( 'NONE',  ( 0.000000000000000000, 0.000000000000000000, -0.4621369752184079083 ) ) ;
#93662 = CARTESIAN_POINT ( 'NONE',  ( 4.472135954999581386, -10.27077220067364749, 4.000000000000000888 ) ) ;
#93663 = CARTESIAN_POINT ( 'NONE',  ( -16.95986460590401634, 43.64169184087446496, -4.188100785892593159 ) ) ;
#93664 = CARTESIAN_POINT ( 'NONE',  ( -3.400000000000000355, 4.163799117101001052E-16, -7.259124522925831435 ) ) ;
#93665 = CARTESIAN_POINT ( 'NONE',  ( 12.13034742782428133, 49.99999999999999289, -93.82352941176471006 ) ) ;
#93666 = VERTEX_POINT ( 'NONE', #106478 ) ;
#93667 = CARTESIAN_POINT ( 'NONE',  ( -3.140974613988893882, 50.00000000000000000, -96.68767211932436112 ) ) ;
#93668 = ORIENTED_EDGE ( 'NONE', *, *, #96759, .T. ) ;
#93669 = CARTESIAN_POINT ( 'NONE',  ( -4.814352310392309597, -63.20321405896424238, -3.583053941560743194 ) ) ;
#93670 = CARTESIAN_POINT ( 'NONE',  ( 75.46173676908961170, -38.35133497314376427, 173.8617030787818578 ) ) ;
#93671 = CARTESIAN_POINT ( 'NONE',  ( 30.00000000000000000, 450.0000000000002274, 13.20242257375370976 ) ) ;
#93672 = B_SPLINE_CURVE_WITH_KNOTS ( 'NONE', 3,
 ( #17434, #50303, #97794, #97267 ),
 .UNSPECIFIED., .F., .F.,
 ( 4, 4 ),
 ( 2.795030908892879291E-15, 0.0001439741052602189176 ),
 .UNSPECIFIED. ) ;
#93673 = CARTESIAN_POINT ( 'NONE',  ( 25.11507076259356097, 295.6895725033105577, 2.116947622670480644 ) ) ;
#93674 = CARTESIAN_POINT ( 'NONE',  ( -5.858881034796409537, 246.2141367599701312, 1.317748741875975682 ) ) ;
#93675 = AXIS2_PLACEMENT_3D ( 'NONE', #31101, #14326, #81704 ) ;
#93676 = ORIENTED_EDGE ( 'NONE', *, *, #8488, .F. ) ;
#93677 = CARTESIAN_POINT ( 'NONE',  ( 29.49710045460141927, 13.37160745013287944, -39.61402429467862873 ) ) ;
#93678 = LINE ( 'NONE', #61321, #14832 ) ;
#93679 = DIRECTION ( 'NONE',  ( -1.000000000000000000, -1.224606353822377258E-16, -0.000000000000000000 ) ) ;
#93680 =( BOUNDED_CURVE ( )  B_SPLINE_CURVE ( 2, ( #20666, #68647, #52973 ),
 .UNSPECIFIED., .F., .F. ) 
 B_SPLINE_CURVE_WITH_KNOTS ( ( 3, 3 ),
 ( 0.000000000000000000, 1.000000000000000000 ),
 .UNSPECIFIED. ) 
 CURVE ( )  GEOMETRIC_REPRESENTATION_ITEM ( )  RATIONAL_B_SPLINE_CURVE ( ( 1.000000000000000000, 1.857142857142858317, 1.000000000000000000 ) ) 
 REPRESENTATION_ITEM ( '' )  );
#93681 = CARTESIAN_POINT ( 'NONE',  ( -9.761721577538938988, 51.33878080989101278, 2.429002427542664488 ) ) ;
#93682 = ADVANCED_FACE ( 'NONE', ( #98909 ), #74478, .F. ) ;
#93683 = ORIENTED_EDGE ( 'NONE', *, *, #31857, .F. ) ;
#93684 = CARTESIAN_POINT ( 'NONE',  ( 5.469234054728515204, 41.99717949937266326, -59.59612150530382735 ) ) ;
#93685 = CARTESIAN_POINT ( 'NONE',  ( -4.861072549008415677, -2.920843450830509447, 102.3606070684416665 ) ) ;
#93686 = LINE ( 'NONE', #54787, #53988 ) ;
#93687 = CARTESIAN_POINT ( 'NONE',  ( -0.3306966981845154141, -8.469326210127452015, -7.349897473154965333 ) ) ;
#93688 = VECTOR ( 'NONE', #55178, 1000.000000000000341 ) ;
#93689 = CARTESIAN_POINT ( 'NONE',  ( 33.70225418941513595, 490.4053771885736523, 11.54106678936950381 ) ) ;
#93690 = EDGE_CURVE ( 'NONE', #91640, #103206, #101903, .T. ) ;
#93691 = EDGE_CURVE ( 'NONE', #36720, #16452, #98583, .T. ) ;
#93692 = DIRECTION ( 'NONE',  ( -1.000000000000000000, -1.224606353822377258E-16, -0.000000000000000000 ) ) ;
#93693 = CARTESIAN_POINT ( 'NONE',  ( 86.67109623895983361, -39.12583655368941749, 188.4524350337027840 ) ) ;
#93694 = CARTESIAN_POINT ( 'NONE',  ( -2.939792614951783900, 97.10348931277984263, 5.000000000000000000 ) ) ;
#93695 = ORIENTED_EDGE ( 'NONE', *, *, #22998, .F. ) ;
#93696 = CARTESIAN_POINT ( 'NONE',  ( -7.808218555861020427, 4.508077085121809269, -7.999534413642737540 ) ) ;
#93697 = DIRECTION ( 'NONE',  ( 1.000000000000000000, 1.224606353822377258E-16, 0.000000000000000000 ) ) ;
#93698 = CARTESIAN_POINT ( 'NONE',  ( 13.95408269174820148, -50.12993014906734146, 28.16184020435892421 ) ) ;
#93699 = EDGE_CURVE ( 'NONE', #30156, #82973, #89786, .T. ) ;
#93700 = DIRECTION ( 'NONE',  ( 0.000000000000000000, 1.000000000000000000, 0.000000000000000000 ) ) ;
#93701 = EDGE_CURVE ( 'NONE', #28602, #101881, #53782, .T. ) ;
#93702 = CARTESIAN_POINT ( 'NONE',  ( -92.95396129993294210, -30.00000000000000711, 105.7524778981976823 ) ) ;
#93703 = AXIS2_PLACEMENT_3D ( 'NONE', #85813, #18420, #18970 ) ;
#93704 = CARTESIAN_POINT ( 'NONE',  ( -32.14400760092462406, 464.7181002246661023, 11.03224828307551597 ) ) ;
#93705 = CARTESIAN_POINT ( 'NONE',  ( 31.99970601987291019, -57.68905111566994748, 46.55696586113492685 ) ) ;
#93707 = DIRECTION ( 'NONE',  ( -1.000000000000000000, -0.000000000000000000, -0.000000000000000000 ) ) ;
#93706 = CARTESIAN_POINT ( 'NONE',  ( 27.99999999999999645, 0.000000000000000000, 0.000000000000000000 ) ) ;
#93708 =( LENGTH_UNIT ( ) NAMED_UNIT ( * ) SI_UNIT ( .MILLI., .METRE. ) );
#93709 = CARTESIAN_POINT ( 'NONE',  ( -12.62509669329198481, -21.71534459113969717, 27.56286583360048326 ) ) ;
#93710 = CARTESIAN_POINT ( 'NONE',  ( -3.400000000000000355, 4.163799117101001052E-16, -7.554475477074167777 ) ) ;
#93711 = SURFACE_SIDE_STYLE ('',( #30583 ) ) ;
#93712 = STYLED_ITEM ( 'NONE', ( #81600 ), #54999 ) ;
#93713 = CARTESIAN_POINT ( 'NONE',  ( 47.70175436633333987, -26.95658883994271449, -28.55419944461410608 ) ) ;
#93714 = AXIS2_PLACEMENT_3D ( 'NONE', #31667, #7351, #6284 ) ;
#93715 = CARTESIAN_POINT ( 'NONE',  ( -22.70419453045296265, -46.43894835127135678, 32.52296259171259862 ) ) ;
#93716 = ORIENTED_EDGE ( 'NONE', *, *, #34746, .T. ) ;
#93717 = FILL_AREA_STYLE_COLOUR ( '', #18671 ) ;
#93718 = CARTESIAN_POINT ( 'NONE',  ( -9.253817200599836923, 106.2999272991686297, -3.791916801615159649 ) ) ;
#93719 = CARTESIAN_POINT ( 'NONE',  ( -20.41567380225452766, -49.92006620171714815, 32.77936002969759954 ) ) ;
#93721 = DIRECTION ( 'NONE',  ( -0.000000000000000000, 1.000000000000000000, -0.000000000000000000 ) ) ;
#93720 = CARTESIAN_POINT ( 'NONE',  ( 43.63933387927400531, 486.5321090506437258, 6.480556376458745937 ) ) ;
#93722 = ORIENTED_EDGE ( 'NONE', *, *, #78187, .F. ) ;
#93723 = CARTESIAN_POINT ( 'NONE',  ( -14.33580413386536812, 42.00000000000000000, -89.41414995615788541 ) ) ;
#93724 = ORIENTED_EDGE ( 'NONE', *, *, #87955, .F. ) ;
#93725 = CARTESIAN_POINT ( 'NONE',  ( 7.751021933904854500, 50.00000000000000711, -95.64136895019579754 ) ) ;
#93726 = ADVANCED_FACE ( 'NONE', ( #98396 ), #14198, .T. ) ;
#93727 = CARTESIAN_POINT ( 'NONE',  ( 6.400000000000000355, 4.618802153517005848, 7.999999999999996447 ) ) ;
#93728 = FACE_BOUND ( 'NONE', #7395, .T. ) ;
#93729 = ORIENTED_EDGE ( 'NONE', *, *, #99234, .T. ) ;
#93730 = CARTESIAN_POINT ( 'NONE',  ( 1.591643166428094558, 50.00000000000000711, -73.00000000000002842 ) ) ;
#93731 = CARTESIAN_POINT ( 'NONE',  ( 103.3943054737346046, -60.16143074633508547, 192.1485504246914786 ) ) ;
#93733 = CARTESIAN_POINT ( 'NONE',  ( -7.551560007654697593, -6.990896481930088946, -2.648022159607835491 ) ) ;
#93732 = FILL_AREA_STYLE_COLOUR ( '', #38893 ) ;
#93734 = EDGE_LOOP ( 'NONE', ( #87811, #55879, #101814, #48708 ) ) ;
#93735 = VECTOR ( 'NONE', #39836, 999.9999999999998863 ) ;
#93736 = VERTEX_POINT ( 'NONE', #24548 ) ;
#93737 = ORIENTED_EDGE ( 'NONE', *, *, #69720, .F. ) ;
#93738 = CARTESIAN_POINT ( 'NONE',  ( 24.47062261081072521, 306.7367191156716899, 9.359397442148701174 ) ) ;
#93739 = AXIS2_PLACEMENT_3D ( 'NONE', #53335, #6347, #86253 ) ;
#93740 = DIRECTION ( 'NONE',  ( 0.000000000000000000, 0.000000000000000000, -1.000000000000000000 ) ) ;
#93741 = CARTESIAN_POINT ( 'NONE',  ( 22.25669491856071858, -5.000000000000000888, 6.123233995736769241E-16 ) ) ;
#93742 = VERTEX_POINT ( 'NONE', #3434 ) ;
#93743 =( GEOMETRIC_REPRESENTATION_CONTEXT ( 3 ) GLOBAL_UNCERTAINTY_ASSIGNED_CONTEXT ( ( #40283 ) ) GLOBAL_UNIT_ASSIGNED_CONTEXT ( ( #53360, #36156, #37747 ) ) REPRESENTATION_CONTEXT ( 'NONE', 'WORKASPACE' ) );
#93744 = CYLINDRICAL_SURFACE ( 'NONE', #97826, 4.000000000000000000 ) ;
#93745 = CARTESIAN_POINT ( 'NONE',  ( -5.129365589857098229, 41.91296976309557465, -69.99827694586697646 ) ) ;
#93746 = VECTOR ( 'NONE', #11262, 1000.000000000000000 ) ;
#93747 = CARTESIAN_POINT ( 'NONE',  ( 31.35227631363202150, 438.7809971775112672, 22.96771959711079703 ) ) ;
#93748 = CARTESIAN_POINT ( 'NONE',  ( -64.13648978638106257, -59.99999999998060929, -36.96743988013938775 ) ) ;
#93749 = DIRECTION ( 'NONE',  ( 0.000000000000000000, 0.000000000000000000, 1.000000000000000000 ) ) ;
#93750 = CARTESIAN_POINT ( 'NONE',  ( -13.99014087154248109, -5.000000000000000000, 8.603192084578022758 ) ) ;
#93751 = CARTESIAN_POINT ( 'NONE',  ( -6.870856496050642193, 41.24229779879266999, -58.43742256236558319 ) ) ;
#93752 = CARTESIAN_POINT ( 'NONE',  ( -89.21220262753612928, -29.99999999999994316, 13.74661749290507906 ) ) ;
#93753 = CARTESIAN_POINT ( 'NONE',  ( -7.577668482282922113, 51.95108853748999422, 3.571063677695252458 ) ) ;
#93754 = CARTESIAN_POINT ( 'NONE',  ( -47.95171403034644442, -49.90426566354960158, 50.75745535836532696 ) ) ;
#93755 = EDGE_LOOP ( 'NONE', ( #14503, #174, #64070, #85763 ) ) ;
#93756 = CARTESIAN_POINT ( 'NONE',  ( 1.927505563446688663, -70.56453101740132183, 13.13085817996164550 ) ) ;
#93757 = EDGE_LOOP ( 'NONE', ( #19930, #4218, #67211, #87372, #14298 ) ) ;
#93758 = CARTESIAN_POINT ( 'NONE',  ( 12.50000000000000355, 1.275975694136318506, -19.12903438635300546 ) ) ;
#93759 = CARTESIAN_POINT ( 'NONE',  ( -4.926264938265286553, 301.1864079209049692, -10.01402411462996511 ) ) ;
#93760 = EDGE_CURVE ( 'NONE', #90581, #58522, #9420, .T. ) ;
#93761 = DIRECTION ( 'NONE',  ( 0.000000000000000000, 1.000000000000000000, 0.000000000000000000 ) ) ;
#93762 = VERTEX_POINT ( 'NONE', #61144 ) ;
#93763 = CARTESIAN_POINT ( 'NONE',  ( 5.475947152006322760, 246.8378226989086954, 2.462898245435130029 ) ) ;
#93764 = ORIENTED_EDGE ( 'NONE', *, *, #27938, .F. ) ;
#93765 = B_SPLINE_CURVE_WITH_KNOTS ( 'NONE', 3,
 ( #47801, #87232, #6821, #14369, #39741, #13314, #72622, #105524, #55365, #62955, #87764, #105002, #12785, #31144, #104456, #31664, #47278, #95852, #64032, #72094 ),
 .UNSPECIFIED., .F., .F.,
 ( 4, 2, 2, 2, 2, 2, 2, 2, 2, 4 ),
 ( 0.007215398811948415224, 0.007719408675872659574, 0.008223418539796903057, 0.008727428403721147407, 0.009231438267645391757, 0.009735448131569637842, 0.01023945799549388046, 0.01049146292745600090, 0.01074346785941812134, 0.01124747772334235701 ),
 .UNSPECIFIED. ) ;
#93766 = CARTESIAN_POINT ( 'NONE',  ( 54.45238581501602937, -38.34104842573536587, 79.96003652838339804 ) ) ;
#93767 = CARTESIAN_POINT ( 'NONE',  ( 0.000000000000000000, 0.000000000000000000, 5.000000000000002665 ) ) ;
#93768 = CARTESIAN_POINT ( 'NONE',  ( 3.369683342532912462, -49.08678202233288346, 104.1613013819149387 ) ) ;
#93769 = CARTESIAN_POINT ( 'NONE',  ( 6.592587067551453295, 41.82481096192319825, -59.20696708569246880 ) ) ;
#93770 = CARTESIAN_POINT ( 'NONE',  ( -23.57730434126679597, 18.64316884711713485, 30.67950393662591324 ) ) ;
#93771 = CARTESIAN_POINT ( 'NONE',  ( 90.89870986292757493, -29.99999999999999645, 190.4476607199382272 ) ) ;
#93772 = CARTESIAN_POINT ( 'NONE',  ( 25.59999999999999787, 1.533819458162526451E-15, 0.000000000000000000 ) ) ;
#93773 = CIRCLE ( 'NONE', #711, 8.000000000000000000 ) ;
#93774 = ORIENTED_EDGE ( 'NONE', *, *, #88526, .T. ) ;
#93775 = ORIENTED_EDGE ( 'NONE', *, *, #65031, .F. ) ;
#93776 = CARTESIAN_POINT ( 'NONE',  ( 54.21244330743853368, -53.37526703652106619, 64.17922940371380491 ) ) ;
#93777 = CARTESIAN_POINT ( 'NONE',  ( 5.668094422307954794, 41.44782620818911312, -58.47096533207623992 ) ) ;
#93778 = CARTESIAN_POINT ( 'NONE',  ( 9.833493305133801599, 1.593028355512270567E-15, 0.000000000000000000 ) ) ;
#93779 = ORIENTED_EDGE ( 'NONE', *, *, #68111, .T. ) ;
#93780 = CARTESIAN_POINT ( 'NONE',  ( -85.43770264849763407, -38.35986594992170495, -22.44427725120138106 ) ) ;
#93781 = ORIENTED_EDGE ( 'NONE', *, *, #91198, .T. ) ;
#93782 = CARTESIAN_POINT ( 'NONE',  ( 0.000000000000000000, 1.502314598737160017E-15, -6.500000000000000000 ) ) ;
#93783 = CARTESIAN_POINT ( 'NONE',  ( 110.8167341139307069, -38.35606656894265143, 179.0010575348368889 ) ) ;
#93784 = CARTESIAN_POINT ( 'NONE',  ( 10.24201228536178299, 16.35548964043822195, 10.08355089876082822 ) ) ;
#93785 = PRESENTATION_LAYER_ASSIGNMENT (  '', '', ( #57563 ) ) ;
#93786 = CARTESIAN_POINT ( 'NONE',  ( 86.18168139896047819, -60.14160201014042428, 16.47270778115648326 ) ) ;
#93787 = AXIS2_PLACEMENT_3D ( 'NONE', #105165, #72778, #56049 ) ;
#93788 = CARTESIAN_POINT ( 'NONE',  ( 32.00754358908571362, 333.4989015379719035, 17.37153786538196343 ) ) ;
#93789 = DIRECTION ( 'NONE',  ( 0.000000000000000000, 1.000000000000000000, 0.000000000000000000 ) ) ;
#93790 = AXIS2_PLACEMENT_3D ( 'NONE', #27563, #66371, #11307 ) ;
#93791 = CARTESIAN_POINT ( 'NONE',  ( 1.459252261608878998, -6.102732174926768671, -13.75226092436929548 ) ) ;
#93792 = CARTESIAN_POINT ( 'NONE',  ( -24.31942756636476943, 25.21064302835431548, -32.55221473460276371 ) ) ;
#93793 =( GEOMETRIC_REPRESENTATION_CONTEXT ( 3 ) GLOBAL_UNCERTAINTY_ASSIGNED_CONTEXT ( ( #84339 ) ) GLOBAL_UNIT_ASSIGNED_CONTEXT ( ( #55653, #7121, #103707 ) ) REPRESENTATION_CONTEXT ( 'NONE', 'WORKASPACE' ) );
#93794 = CARTESIAN_POINT ( 'NONE',  ( -44.21332904831276522, 435.2494715644500616, 14.45449769377424687 ) ) ;
#93795 = CARTESIAN_POINT ( 'NONE',  ( 8.020865862503733013, 47.74483808550601793, 2.456440091863195202E-12 ) ) ;
#93796 = EDGE_LOOP ( 'NONE', ( #2794, #50893, #86045, #47976 ) ) ;
#93797 = CARTESIAN_POINT ( 'NONE',  ( 0.5678959950308366533, 37.15953799686300130, 27.38331912478550478 ) ) ;
#93798 = CARTESIAN_POINT ( 'NONE',  ( 7.500000000000005329, 40.00000000000068923, -68.91429205785459544 ) ) ;
#93799 = DIRECTION ( 'NONE',  ( -1.000000000000000000, 0.000000000000000000, 0.000000000000000000 ) ) ;
#93800 = ORIENTED_EDGE ( 'NONE', *, *, #100170, .F. ) ;
#93801 = CARTESIAN_POINT ( 'NONE',  ( -23.86237914550371642, 305.6547497236389290, -8.827011597931521791 ) ) ;
#93802 = CARTESIAN_POINT ( 'NONE',  ( -38.99434193015822103, 323.4566427656836254, 16.92016985397825835 ) ) ;
#93803 = CARTESIAN_POINT ( 'NONE',  ( 0.000000000000000000, 0.000000000000000000, 5.000000000000000888 ) ) ;
#93804 = CARTESIAN_POINT ( 'NONE',  ( 8.000000000000000000, -21.49999999999999645, 0.000000000000000000 ) ) ;
#93805 = CARTESIAN_POINT ( 'NONE',  ( -14.09593269997207088, -14.81306030174825317, 31.68409824573272004 ) ) ;
#93806 = EDGE_CURVE ( 'NONE', #82046, #80206, #96844, .T. ) ;
#93807 = DIRECTION ( 'NONE',  ( -0.000000000000000000, 1.000000000000000000, -0.000000000000000000 ) ) ;
#93808 = EDGE_LOOP ( 'NONE', ( #16983, #92224, #39917, #61083 ) ) ;
#93809 = CARTESIAN_POINT ( 'NONE',  ( 86.40550120089977781, -17.76515147996571642, 175.7347892468938539 ) ) ;
#93810 = FILL_AREA_STYLE_COLOUR ( '', #70488 ) ;
#93811 = CARTESIAN_POINT ( 'NONE',  ( -15.39709502357286652, 46.16515237750015643, 5.602001606816734203 ) ) ;
#93812 = ORIENTED_EDGE ( 'NONE', *, *, #52412, .T. ) ;
#93813 = CIRCLE ( 'NONE', #57589, 5.000000000000000888 ) ;
#93814 = CARTESIAN_POINT ( 'NONE',  ( -89.89106403992835226, -52.70984408041336167, 62.30226075620301884 ) ) ;
#93815 = DIRECTION ( 'NONE',  ( 0.000000000000000000, -1.000000000000000000, 0.000000000000000000 ) ) ;
#93816 = CARTESIAN_POINT ( 'NONE',  ( 8.572890873561295422, -5.000000000000002665, -75.22730630429822440 ) ) ;
#93817 = CARTESIAN_POINT ( 'NONE',  ( 6.582279166563815842, 304.7470068806263725, 8.914713973399436497 ) ) ;
#93818 = ADVANCED_FACE ( 'NONE', ( #60628 ), #51438, .T. ) ;
#93819 = CARTESIAN_POINT ( 'NONE',  ( -8.675203801466720321, -22.30999872138366413, -38.54374433678079015 ) ) ;
#93820 = EDGE_CURVE ( 'NONE', #35302, #85207, #42876, .T. ) ;
#93821 = AXIS2_PLACEMENT_3D ( 'NONE', #53623, #5603, #62792 ) ;
#93823 = CONICAL_SURFACE ( 'NONE', #47066, 4.250000000000000000, 0.9599310885968754814 ) ;
#93822 = SURFACE_STYLE_FILL_AREA ( #4810 ) ;
#93824 = CARTESIAN_POINT ( 'NONE',  ( 17.12293775459222545, -60.00000000000000711, 39.93182275144659599 ) ) ;
#93825 = CARTESIAN_POINT ( 'NONE',  ( 36.21953432627893932, -36.13225097047772749, 45.40297091003908037 ) ) ;
#93826 =( LENGTH_UNIT ( ) NAMED_UNIT ( * ) SI_UNIT ( .MILLI., .METRE. ) );
#93827 = CARTESIAN_POINT ( 'NONE',  ( 35.66921402495393068, -24.37933129301127977, 33.74266031588260972 ) ) ;
#93829 = CARTESIAN_POINT ( 'NONE',  ( -10.64220735762159009, 12.97372309155720416, 10.01974392434693684 ) ) ;
#93828 = CARTESIAN_POINT ( 'NONE',  ( -32.31175092299783103, -33.94243246659586788, 42.05989758142741408 ) ) ;
#93830 = CARTESIAN_POINT ( 'NONE',  ( 1.853816988748078209, 295.4475851225615770, -10.00136337793448860 ) ) ;
#93831 = CARTESIAN_POINT ( 'NONE',  ( 45.31383884518383098, 362.9196860876334085, 5.161789940898600548 ) ) ;
#93832 = EDGE_CURVE ( 'NONE', #53891, #80344, #91684, .T. ) ;
#93833 = CARTESIAN_POINT ( 'NONE',  ( 22.57792046605466041, -5.000000000000000000, 0.000000000000000000 ) ) ;
#93834 = ORIENTED_EDGE ( 'NONE', *, *, #45544, .F. ) ;
#93835 = CARTESIAN_POINT ( 'NONE',  ( 36.48461538461538822, -4.171999999999999709, 0.000000000000000000 ) ) ;
#93836 = ORIENTED_EDGE ( 'NONE', *, *, #12100, .T. ) ;
#93837 = CARTESIAN_POINT ( 'NONE',  ( -12.40685984127932961, -3.384540406130107204, 20.61063982846911102 ) ) ;
#93838 = CARTESIAN_POINT ( 'NONE',  ( 46.00000000000000000, 488.1802228726408543, 2.474914525454350755 ) ) ;
#93839 = FACE_OUTER_BOUND ( 'NONE', #48108, .T. ) ;
#93840 = CARTESIAN_POINT ( 'NONE',  ( -0.001453451169200235555, -21.77031582776994512, -30.51803592518467312 ) ) ;
#93841 = CIRCLE ( 'NONE', #35362, 5.000000000000002665 ) ;
#93842 = VERTEX_POINT ( 'NONE', #2879 ) ;
#93843 = CARTESIAN_POINT ( 'NONE',  ( 28.34337590820723918, 36.34601651445377968, 8.617044493960250406 ) ) ;
#93844 = DIRECTION ( 'NONE',  ( -1.000000000000000000, -1.224606353822377258E-16, -0.000000000000000000 ) ) ;
#93845 = ORIENTED_EDGE ( 'NONE', *, *, #57170, .F. ) ;
#93846 = CARTESIAN_POINT ( 'NONE',  ( 27.10511071441204578, 34.75829513984540142, 7.556984339685363317 ) ) ;
#93847 = EDGE_CURVE ( 'NONE', #60121, #29715, #45189, .T. ) ;
#93848 = DIRECTION ( 'NONE',  ( 0.000000000000000000, -1.000000000000000000, 0.000000000000000000 ) ) ;
#93850 = B_SPLINE_CURVE_WITH_KNOTS ( 'NONE', 3,
 ( #23180, #15054, #40398, #57624, #32338 ),
 .UNSPECIFIED., .F., .F.,
 ( 4, 1, 4 ),
 ( 0.000000000000000000, 0.003752776749732572668, 0.007505553499465145335 ),
 .UNSPECIFIED. ) ;
#93849 = MECHANICAL_DESIGN_GEOMETRIC_PRESENTATION_REPRESENTATION (  '', ( #105917 ), #5987 ) ;
#93851 = CARTESIAN_POINT ( 'NONE',  ( -91.86405410517724590, -60.00000000000002132, 11.09660898435537035 ) ) ;
#93852 = ORIENTED_EDGE ( 'NONE', *, *, #52613, .F. ) ;
#93853 = DIRECTION ( 'NONE',  ( 0.000000000000000000, -1.000000000000000000, 0.000000000000000000 ) ) ;
#93854 = AXIS2_PLACEMENT_3D ( 'NONE', #30407, #63296, #96194 ) ;
#93855 = CARTESIAN_POINT ( 'NONE',  ( 89.99999999999997158, -60.00000000000000000, 196.0238439516549818 ) ) ;
#93856 = DIRECTION ( 'NONE',  ( 0.000000000000000000, -1.000000000000000000, 0.000000000000000000 ) ) ;
#93858 = DIRECTION ( 'NONE',  ( 0.000000000000000000, 0.000000000000000000, 1.000000000000000000 ) ) ;
#93857 = DIRECTION ( 'NONE',  ( -1.000000000000000000, 0.000000000000000000, 0.000000000000000000 ) ) ;
#93859 = CARTESIAN_POINT ( 'NONE',  ( -80.43703877261472712, -56.89382256290284801, 173.6098779234407345 ) ) ;
#93860 = ORIENTED_EDGE ( 'NONE', *, *, #87499, .T. ) ;
#93861 =( GEOMETRIC_REPRESENTATION_CONTEXT ( 3 ) GLOBAL_UNCERTAINTY_ASSIGNED_CONTEXT ( ( #59546 ) ) GLOBAL_UNIT_ASSIGNED_CONTEXT ( ( #77584, #37156, #52767 ) ) REPRESENTATION_CONTEXT ( 'NONE', 'WORKASPACE' ) );
#93862 = CARTESIAN_POINT ( 'NONE',  ( -43.00000000000000000, 487.9285348210879647, 8.903916466045071587 ) ) ;
#93863 = ORIENTED_EDGE ( 'NONE', *, *, #36643, .T. ) ;
#93864 = ORIENTED_EDGE ( 'NONE', *, *, #106679, .T. ) ;
#93865 = CARTESIAN_POINT ( 'NONE',  ( -18.16578424161952654, -4.332661967060594144, -1.112710490969183175 ) ) ;
#93866 = ADVANCED_FACE ( 'NONE', ( #67642 ), #59553, .T. ) ;
#93867 = CARTESIAN_POINT ( 'NONE',  ( 6.070808553813592639E-16, -8.895730773063899477, -7.917997657324742811 ) ) ;
#93868 = CARTESIAN_POINT ( 'NONE',  ( 4.472135954999578722, -65.00000000000000000, -4.000000000000002665 ) ) ;
#93869 = ORIENTED_EDGE ( 'NONE', *, *, #86675, .T. ) ;
#93870 = CARTESIAN_POINT ( 'NONE',  ( 6.289692432696785573, -1.240526984323783911E-13, -6.828989928337169779 ) ) ;
#93871 = CARTESIAN_POINT ( 'NONE',  ( -94.10527518209565301, -57.67545334945994995, 3.926124123639501029 ) ) ;
#93872 = CARTESIAN_POINT ( 'NONE',  ( -5.909259836070535066, -68.86277204242070127, -1.072443315311455647 ) ) ;
#93873 = CARTESIAN_POINT ( 'NONE',  ( 43.50250715914211952, 464.6389613228371900, 9.611700240006818774 ) ) ;
#93874 = CARTESIAN_POINT ( 'NONE',  ( 23.54393690455825094, 28.03570273098069876, 30.73873073986555937 ) ) ;
#93875 = DIRECTION ( 'NONE',  ( 0.000000000000000000, 1.000000000000000000, -0.000000000000000000 ) ) ;
#93876 = CARTESIAN_POINT ( 'NONE',  ( 3.827754797006158505, 15.98931925350938243, -9.240220675753615609 ) ) ;
#93877 = CARTESIAN_POINT ( 'NONE',  ( 100.7779335074592524, -14.21045842199434084, 117.1442511085924565 ) ) ;
#93878 = CARTESIAN_POINT ( 'NONE',  ( -100.0713701506240767, -14.21045842199444209, 196.7486061734171585 ) ) ;
#93879 = CARTESIAN_POINT ( 'NONE',  ( -56.24379992063114031, -46.44138396924517309, 65.97396921761240662 ) ) ;
#93880 = ORIENTED_EDGE ( 'NONE', *, *, #20790, .F. ) ;
#93881 = CARTESIAN_POINT ( 'NONE',  ( 28.17977184163764193, 1.482358050883964840E-15, 0.000000000000000000 ) ) ;
#93882 = ORIENTED_EDGE ( 'NONE', *, *, #5622, .F. ) ;
#93883 = CARTESIAN_POINT ( 'NONE',  ( -104.8207464962321041, -52.71021621793995848, 181.7139379092529623 ) ) ;
#93884 = DIRECTION ( 'NONE',  ( 0.000000000000000000, 0.000000000000000000, -1.000000000000000000 ) ) ;
#93885 =( NAMED_UNIT ( * ) SI_UNIT ( $, .STERADIAN. ) SOLID_ANGLE_UNIT ( ) );
#93886 = ADVANCED_FACE ( 'NONE', ( #30382 ), #50311, .T. ) ;
#93887 = EDGE_LOOP ( 'NONE', ( #55447, #106360, #45221, #51671 ) ) ;
#93889 = B_SPLINE_CURVE_WITH_KNOTS ( 'NONE', 3,
 ( #76953, #61326, #46575, #35474, #59728, #21805, #54645, #92603, #18759, #76413, #68344, #101242, #27396, #60277, #93145, #11135, #68889, #101762, #60795, #89163, #16323, #56225, #39030, #90219, #64369, #15268, #105863, #48151, #81050, #57300, #64880, #73485, #15797, #49214 ),
 .UNSPECIFIED., .F., .F.,
 ( 4, 2, 2, 2, 2, 2, 2, 2, 2, 2, 2, 2, 2, 2, 2, 2, 4 ),
 ( 0.01272238763756221476, 0.01351613129786393384, 0.01430987495816565119, 0.01510361861846737028, 0.01589736227876908936, 0.01669110593907080844, 0.01748484959937252753, 0.01827859325967424314, 0.01907233691997596223, 0.01986608058027768131, 0.02065982424057940040, 0.02145356790088111948, 0.02224731156118283509, 0.02304105522148455765, 0.02383479888178627326, 0.02462854254208799235, 0.02542228620238971143 ),
 .UNSPECIFIED. ) ;
#93888 = CARTESIAN_POINT ( 'NONE',  ( 19.50011280463133545, 50.00000000000000000, 59.90639435984937222 ) ) ;
#93890 = CARTESIAN_POINT ( 'NONE',  ( 78.22378191117061874, -38.35599095560626637, -27.52319075166474960 ) ) ;
#93891 = CARTESIAN_POINT ( 'NONE',  ( 36.81615681129832041, 25.76252507750780296, -13.21838005021004747 ) ) ;
#93892 = CARTESIAN_POINT ( 'NONE',  ( -7.188101187500002709, -15.68750000204838457, 2.977408999572648707 ) ) ;
#93893 = CARTESIAN_POINT ( 'NONE',  ( 20.97754405179121662, 294.8763868968453608, 9.942224931492262385 ) ) ;
#93894 = CARTESIAN_POINT ( 'NONE',  ( -43.00000000000001421, 462.1685671383398244, 2.813679926073832327 ) ) ;
#93895 = AXIS2_PLACEMENT_3D ( 'NONE', #57981, #81710, #40743 ) ;
#93896 = DIRECTION ( 'NONE',  ( -0.000000000000000000, 1.000000000000000000, -0.000000000000000000 ) ) ;
#93897 = CARTESIAN_POINT ( 'NONE',  ( -31.11679462788039530, 441.4271381875185511, 23.27438508043199406 ) ) ;
#93898 = DIRECTION ( 'NONE',  ( 0.000000000000000000, 1.000000000000000000, 0.000000000000000000 ) ) ;
#93899 = EDGE_CURVE ( 'NONE', #87758, #11437, #56999, .T. ) ;
#93900 = CARTESIAN_POINT ( 'NONE',  ( -9.295212903232194179, 43.59689220704109403, -14.93628917660103994 ) ) ;
#93901 = CARTESIAN_POINT ( 'NONE',  ( 13.58349330513380515, -3.851859888774471706E-31, 4.000000000000001776 ) ) ;
#93902 =( NAMED_UNIT ( * ) PLANE_ANGLE_UNIT ( ) SI_UNIT ( $, .RADIAN. ) );
#93903 = FACE_BOUND ( 'NONE', #66789, .T. ) ;
#93904 = CARTESIAN_POINT ( 'NONE',  ( -32.69584145684933674, -60.31921410685050944, 38.00927738129874456 ) ) ;
#93905 =( LENGTH_UNIT ( ) NAMED_UNIT ( * ) SI_UNIT ( .MILLI., .METRE. ) );
#93906 = CARTESIAN_POINT ( 'NONE',  ( 47.98400582330030062, -46.44011229906595872, 49.73359105907310607 ) ) ;
#93907 = DIRECTION ( 'NONE',  ( 0.000000000000000000, 1.000000000000000000, 0.000000000000000000 ) ) ;
#93908 = CARTESIAN_POINT ( 'NONE',  ( -7.743982712349856357, 88.46213014760739668, 2.020119794285906600 ) ) ;
#93909 = CARTESIAN_POINT ( 'NONE',  ( -87.79946780904923287, -38.56465307817885702, 199.8815181703243127 ) ) ;
#93910 = ORIENTED_EDGE ( 'NONE', *, *, #71262, .F. ) ;
#93912 = CYLINDRICAL_SURFACE ( 'NONE', #35366, 33.82893434829263413 ) ;
#93911 = CARTESIAN_POINT ( 'NONE',  ( -16.14595037822600432, 20.73084165116604183, 4.192529328840223890 ) ) ;
#93913 = FACE_OUTER_BOUND ( 'NONE', #31794, .T. ) ;
#93914 = CARTESIAN_POINT ( 'NONE',  ( -19.31778612519895688, 49.87566157773895270, 61.28311047971154579 ) ) ;
#93915 = CARTESIAN_POINT ( 'NONE',  ( 6.457005528859116161, 41.52802923978755700, -70.63630686878374831 ) ) ;
#93916 = CARTESIAN_POINT ( 'NONE',  ( -33.92709525147876093, 435.0559456452659219, 11.89085117398058955 ) ) ;
#93917 = CARTESIAN_POINT ( 'NONE',  ( -26.77371412052617927, 310.9345145332244442, 10.38748261951031182 ) ) ;
#93918 = CARTESIAN_POINT ( 'NONE',  ( 7.500000000000000000, -3.608439182435168924, -7.298562697733108173 ) ) ;
#93919 = CARTESIAN_POINT ( 'NONE',  ( 105.3430580151378848, -60.00000000000000000, 198.9623513283988814 ) ) ;
#93920 = ADVANCED_FACE ( 'NONE', ( #78902 ), #6600, .T. ) ;
#93921 = COLOUR_RGB ( '', 0.66274510, 0.83137255, 0.94901961) ;
#93922 = EDGE_CURVE ( 'NONE', #81281, #10685, #37758, .T. ) ;
#93923 = CARTESIAN_POINT ( 'NONE',  ( -7.934883677559682269, -68.86839177937554268, 1.051380792122688757 ) ) ;
#93924 = ORIENTED_EDGE ( 'NONE', *, *, #92924, .F. ) ;
#93925 = CARTESIAN_POINT ( 'NONE',  ( 1.910332202385215838, -49.86383299196077701, 102.2504571675874274 ) ) ;
#93926 = CONICAL_SURFACE ( 'NONE', #78434, 6.500000000000000000, 1.047197551196600296 ) ;
#93927 = CARTESIAN_POINT ( 'NONE',  ( -77.49146788675471953, -30.00000000000003197, -16.28211930504271976 ) ) ;
#93928 = ORIENTED_EDGE ( 'NONE', *, *, #101510, .T. ) ;
#93930 = CARTESIAN_POINT ( 'NONE',  ( 5.238621724886622033, 9.104318317904928293, -29.37793476824274919 ) ) ;
#93929 = CARTESIAN_POINT ( 'NONE',  ( -83.77510898144794282, -38.77500651307043711, 197.6085426658710844 ) ) ;
#93931 = CARTESIAN_POINT ( 'NONE',  ( 46.08349330513379982, 1.593028355512270567E-15, 0.000000000000000000 ) ) ;
#93932 = CARTESIAN_POINT ( 'NONE',  ( 6.800000000000000711, 0.000000000000000000, 0.000000000000000000 ) ) ;
#93933 = CARTESIAN_POINT ( 'NONE',  ( -4.651132217449170270, -5.000000000000000000, -15.66661053588738106 ) ) ;
#93934 = CARTESIAN_POINT ( 'NONE',  ( 5.082755093536325930, -13.34375000204838457, -5.082755093536325042 ) ) ;
#93935 = AXIS2_PLACEMENT_3D ( 'NONE', #80226, #95903, #72146 ) ;
#93936 = CARTESIAN_POINT ( 'NONE',  ( 7.374560640985523996, -5.000000000000002665, -94.59600210749707117 ) ) ;
#93937 = PRESENTATION_LAYER_ASSIGNMENT (  '', '', ( #14679 ) ) ;
#93938 = CIRCLE ( 'NONE', #19913, 4.000000000000000888 ) ;
#93939 = LINE ( 'NONE', #103613, #69035 ) ;
#93940 = AXIS2_PLACEMENT_3D ( 'NONE', #93056, #3519, #12650 ) ;
#93942 = VERTEX_POINT ( 'NONE', #70295 ) ;
#93941 = CARTESIAN_POINT ( 'NONE',  ( 6.281178480976146616, -3.752776749732560813, 6.500000000000004441 ) ) ;
#93943 = CARTESIAN_POINT ( 'NONE',  ( 80.80464672076368515, -60.47367659752207913, 181.9382789710017789 ) ) ;
#93944 = CARTESIAN_POINT ( 'NONE',  ( -41.96713667498163147, 484.5369099524149874, -2.773154793582960576 ) ) ;
#93945 = AXIS2_PLACEMENT_3D ( 'NONE', #88878, #39806, #74276 ) ;
#93946 = DIRECTION ( 'NONE',  ( -1.000000000000000000, -1.224606353822377258E-16, -0.000000000000000000 ) ) ;
#93947 = ORIENTED_EDGE ( 'NONE', *, *, #78702, .F. ) ;
#93948 = CARTESIAN_POINT ( 'NONE',  ( -32.95646543402917672, 485.7809766657132400, 5.067016726494657064 ) ) ;
#93949 = CARTESIAN_POINT ( 'NONE',  ( -46.78576055570702863, 18.82161635153803658, 15.45372055756467944 ) ) ;
#93950 = CARTESIAN_POINT ( 'NONE',  ( 46.00000000000000000, 500.0000000000002274, 0.000000000000000000 ) ) ;
#93951 = DIRECTION ( 'NONE',  ( 0.000000000000000000, 0.000000000000000000, -1.000000000000000000 ) ) ;
#93952 = AXIS2_PLACEMENT_3D ( 'NONE', #53488, #102572, #102026 ) ;
#93953 = CARTESIAN_POINT ( 'NONE',  ( -29.49619080111420999, 13.37262004692842865, -39.61417171781349111 ) ) ;
#93954 = CARTESIAN_POINT ( 'NONE',  ( 0.07779196254430825741, 12.91535575337009867, 51.75000000000002842 ) ) ;
#93955 = CARTESIAN_POINT ( 'NONE',  ( 9.397061706953902416, 2.827687757435164873, 14.73115738288152166 ) ) ;
#93956 = EDGE_CURVE ( 'NONE', #81058, #25843, #5029, .T. ) ;
#93957 = EDGE_LOOP ( 'NONE', ( #78414, #65673, #22349, #10740 ) ) ;
#93958 =( NAMED_UNIT ( * ) SI_UNIT ( $, .STERADIAN. ) SOLID_ANGLE_UNIT ( ) );
#93959 = CARTESIAN_POINT ( 'NONE',  ( -7.726607555805129479, 296.0525430558076323, 6.373197147326261636 ) ) ;
#93960 = EDGE_CURVE ( 'NONE', #78182, #54822, #38473, .T. ) ;
#93961 = CARTESIAN_POINT ( 'NONE',  ( 94.84444444444443434, 1.023464760207051730E-14, 0.000000000000000000 ) ) ;
#93962 = DIRECTION ( 'NONE',  ( 0.000000000000000000, 1.000000000000000000, 0.000000000000000000 ) ) ;
#93964 = CARTESIAN_POINT ( 'NONE',  ( -12.54804038502308394, 5.196493816364167628, -8.098704251221438000 ) ) ;
#93963 = DIRECTION ( 'NONE',  ( 0.000000000000000000, 0.000000000000000000, -1.000000000000000000 ) ) ;
#93965 = CARTESIAN_POINT ( 'NONE',  ( -7.188101187500001821, -26.00000000204838457, -2.977408999572651371 ) ) ;
#93966 = CARTESIAN_POINT ( 'NONE',  ( 17.36274101333847852, 302.5953464100861083, -10.05438841575618980 ) ) ;
#93967 = EDGE_CURVE ( 'NONE', #25935, #67790, #32587, .T. ) ;
#93968 = FACE_BOUND ( 'NONE', #37040, .T. ) ;
#93969 =( LENGTH_UNIT ( ) NAMED_UNIT ( * ) SI_UNIT ( .MILLI., .METRE. ) );
#93970 = VERTEX_POINT ( 'NONE', #95630 ) ;
#93971 = LINE ( 'NONE', #85896, #90512 ) ;
#93972 = CARTESIAN_POINT ( 'NONE',  ( -3.761186937365144090, 19.52715997569687190, -5.000000000000000000 ) ) ;
#93973 = CARTESIAN_POINT ( 'NONE',  ( 19.83349330513380693, 1.593028355512270962E-15, 0.000000000000000000 ) ) ;
#93974 = EDGE_CURVE ( 'NONE', #51590, #7932, #33184, .T. ) ;
#93975 = VERTEX_POINT ( 'NONE', #7651 ) ;
#93976 = CARTESIAN_POINT ( 'NONE',  ( -10.74465425721712464, 48.00000000000000000, -95.72854256505191017 ) ) ;
#93977 = EDGE_CURVE ( 'NONE', #41058, #19286, #72712, .T. ) ;
#93978 =( NAMED_UNIT ( * ) SI_UNIT ( $, .STERADIAN. ) SOLID_ANGLE_UNIT ( ) );
#93979 = CARTESIAN_POINT ( 'NONE',  ( 9.253817200599836923, 103.7000727008313845, -3.791916801615160093 ) ) ;
#93980 = CARTESIAN_POINT ( 'NONE',  ( -102.8080736368318924, -60.00000000000000711, 200.7218921456022542 ) ) ;
#93981 =( LENGTH_UNIT ( ) NAMED_UNIT ( * ) SI_UNIT ( .MILLI., .METRE. ) );
#93982 = FACE_OUTER_BOUND ( 'NONE', #91543, .T. ) ;
#93983 = CARTESIAN_POINT ( 'NONE',  ( -84.39678327578025119, -39.41870918651168409, 180.8096083365613822 ) ) ;
#93984 = MECHANICAL_DESIGN_GEOMETRIC_PRESENTATION_REPRESENTATION (  '', ( #102608 ), #105981 ) ;
#93985 = VERTEX_POINT ( 'NONE', #82626 ) ;
#93986 = CARTESIAN_POINT ( 'NONE',  ( -9.443351513663847285, 46.21199249391292341, -13.23092383815009754 ) ) ;
#93987 =( BOUNDED_CURVE ( )  B_SPLINE_CURVE ( 2, ( #26213, #18633, #80540, #14740, #22356, #38525, #29905, #38014, #6121 ),
 .UNSPECIFIED., .F., .F. ) 
 B_SPLINE_CURVE_WITH_KNOTS ( ( 3, 2, 2, 2, 3 ),
 ( 0.5735294117647059542, 0.5808823529411766273, 0.5882352941176471894, 0.5955882352941177516, 0.6029411764705883137 ),
 .UNSPECIFIED. ) 
 CURVE ( )  GEOMETRIC_REPRESENTATION_ITEM ( )  RATIONAL_B_SPLINE_CURVE ( ( 0.9999999999999988898, 0.9238795325112878487, 1.000000000000000000, 0.9238795325112867385, 1.000000000000000000, 0.9238795325112867385, 1.000000000000000000, 0.9238795325112856283, 1.000000000000001110 ) ) 
 REPRESENTATION_ITEM ( '' )  );
#93988 = EDGE_CURVE ( 'NONE', #12516, #32331, #40568, .T. ) ;
#93990 = CARTESIAN_POINT ( 'NONE',  ( 3.438773559903462118, -0.8293899918514395786, 103.7823003339744901 ) ) ;
#93989 = COLOUR_RGB ( '', 0.40784314, 0.44705882, 0.49803922) ;
#93991 = CARTESIAN_POINT ( 'NONE',  ( -83.82575208384432131, -45.26788530597328020, 5.651614345716667209 ) ) ;
#93992 = PLANE ( 'NONE',  #40868 ) ;
#93993 = CARTESIAN_POINT ( 'NONE',  ( -2.854617081844746718, 68.28765738858956524, -5.000000000000000000 ) ) ;
#93994 = FACE_OUTER_BOUND ( 'NONE', #80608, .T. ) ;
#93995 = DIRECTION ( 'NONE',  ( 0.000000000000000000, -1.000000000000000000, 0.000000000000000000 ) ) ;
#93996 = CARTESIAN_POINT ( 'NONE',  ( 71.28669324481667502, -60.00000000000002132, 168.6228882893990715 ) ) ;
#93997 = CARTESIAN_POINT ( 'NONE',  ( -93.94019401501873290, -59.99999999999992895, -15.95863606727341022 ) ) ;
#93998 = CARTESIAN_POINT ( 'NONE',  ( -67.38458195274520790, -18.62889978042072059, 82.16052029329225093 ) ) ;
#93999 = VERTEX_POINT ( 'NONE', #16288 ) ;
#94000 = CARTESIAN_POINT ( 'NONE',  ( 97.80297141475710987, -14.21045842199415432, 197.6895799465713708 ) ) ;
#94001 = CARTESIAN_POINT ( 'NONE',  ( 62.40452586790289047, 40.83862041121656716, 18.42722372817474152 ) ) ;
#94002 = CARTESIAN_POINT ( 'NONE',  ( 21.58919157199202843, -60.00000000000991207, 42.83841619683437330 ) ) ;
#94003 = CIRCLE ( 'NONE', #63060, 5.000000000000002665 ) ;
#94005 = ORIENTED_EDGE ( 'NONE', *, *, #77380, .T. ) ;
#94004 = CONICAL_SURFACE ( 'NONE', #47487, 10.39117206796836257, 1.221730476396047926 ) ;
#94006 = CARTESIAN_POINT ( 'NONE',  ( 13.99657022045423282, -57.97469379117722355, 26.59685899168112400 ) ) ;
#94008 = AXIS2_PLACEMENT_3D ( 'NONE', #8682, #7604, #98737 ) ;
#94007 = CARTESIAN_POINT ( 'NONE',  ( -2.977408999572650039, -26.56250000204838457, -7.188101187500000933 ) ) ;
#94009 = CARTESIAN_POINT ( 'NONE',  ( 30.00000000000000000, 450.0000000000002274, 1.202422573753698876 ) ) ;
#94010 = ORIENTED_EDGE ( 'NONE', *, *, #86082, .F. ) ;
#94011 = PRODUCT_DEFINITION_SHAPE ( 'NONE', 'NONE',  #106790 ) ;
#94012 = DIRECTION ( 'NONE',  ( 1.000000000000000000, 1.224606353822377258E-16, 0.000000000000000000 ) ) ;
#94013 = EDGE_LOOP ( 'NONE', ( #9499, #23559, #99815, #85218, #79183, #48131 ) ) ;
#94014 = CARTESIAN_POINT ( 'NONE',  ( -1.735558044529530664, 39.99999999999999289, -69.74083754113279099 ) ) ;
#94015 = CARTESIAN_POINT ( 'NONE',  ( -40.33183555103232720, 485.8341092017944902, -4.932519190552891786 ) ) ;
#94016 = CARTESIAN_POINT ( 'NONE',  ( -27.82884491182329612, -60.00000000000002132, -41.18721216356012604 ) ) ;
#94017 = CARTESIAN_POINT ( 'NONE',  ( -11.30498485061268354, 43.19237185749400254, 14.90159096885996703 ) ) ;
#94018 = CARTESIAN_POINT ( 'NONE',  ( -7.188101187500001821, -32.37500000204838813, -2.977408999572651371 ) ) ;
#94019 = CARTESIAN_POINT ( 'NONE',  ( -80.00000000000000000, -60.00000000000000000, -19.09707704303353282 ) ) ;
#94020 = CIRCLE ( 'NONE', #95714, 24.55262289886175964 ) ;
#94021 =( LENGTH_UNIT ( ) NAMED_UNIT ( * ) SI_UNIT ( .MILLI., .METRE. ) );
#94022 = ADVANCED_FACE ( 'NONE', ( #57263 ), #31969, .T. ) ;
#94023 = CARTESIAN_POINT ( 'NONE',  ( -7.744991119775240129, 108.4643878542513278, -2.016316005557099444 ) ) ;
#94024 = CARTESIAN_POINT ( 'NONE',  ( 39.20264847829687938, 436.8475545326444944, 5.145470557644901355 ) ) ;
#94025 = ORIENTED_EDGE ( 'NONE', *, *, #23380, .F. ) ;
#94026 = CARTESIAN_POINT ( 'NONE',  ( -7.251642494156320673, 41.54835750584366849, -68.91429205799529711 ) ) ;
#94028 = CARTESIAN_POINT ( 'NONE',  ( 32.69486656708485128, -25.62054887169689010, 31.60347500623590733 ) ) ;
#94027 = CARTESIAN_POINT ( 'NONE',  ( -3.349796915293434374, -48.86785030187986223, 104.5044954676190798 ) ) ;
#94029 = ORIENTED_EDGE ( 'NONE', *, *, #24415, .F. ) ;
#94030 = EDGE_CURVE ( 'NONE', #40814, #87422, #63331, .T. ) ;
#94031 = CARTESIAN_POINT ( 'NONE',  ( 38.23020704518827273, 485.0116943706019015, -3.938850139312762622 ) ) ;
#94033 = CARTESIAN_POINT ( 'NONE',  ( 7.036764706176849238, 40.29466777802799271, -71.06385277369803077 ) ) ;
#94032 = DIRECTION ( 'NONE',  ( 0.000000000000000000, -1.000000000000000000, 0.000000000000000000 ) ) ;
#94034 = DIRECTION ( 'NONE',  ( -0.000000000000000000, 1.000000000000000000, -0.000000000000000000 ) ) ;
#94035 = CARTESIAN_POINT ( 'NONE',  ( -43.68669919770279364, 485.1453384654006982, 2.541696494117124061 ) ) ;
#94036 = CARTESIAN_POINT ( 'NONE',  ( 4.898587196589412829E-16, -10.81250000409677092, -8.000000000000000000 ) ) ;
#94037 = CARTESIAN_POINT ( 'NONE',  ( 6.249999999999997335, 5.051814855409223703, -7.198902722707428481 ) ) ;
#94038 = CARTESIAN_POINT ( 'NONE',  ( 32.66787492829552519, 465.0722615638334219, 12.52936269480703757 ) ) ;
#94039 = CARTESIAN_POINT ( 'NONE',  ( -34.68490551324223503, 463.9993046474211269, 18.60480341025479234 ) ) ;
#94040 = ORIENTED_EDGE ( 'NONE', *, *, #80520, .T. ) ;
#94041 = CARTESIAN_POINT ( 'NONE',  ( 92.00108026731086852, -60.00000000000000711, 6.185581164671163812 ) ) ;
#94042 = LINE ( 'NONE', #61706, #86020 ) ;
#94044 = ADVANCED_FACE ( 'NONE', ( #23894 ), #90722, .T. ) ;
#94043 = CARTESIAN_POINT ( 'NONE',  ( 33.21051451589296732, 465.5912171647664763, 15.87385029326350505 ) ) ;
#94045 = CARTESIAN_POINT ( 'NONE',  ( -35.65409554988107033, 370.7248284907977904, 3.823559223723805189 ) ) ;
#94046 = AXIS2_PLACEMENT_3D ( 'NONE', #32077, #71984, #63389 ) ;
#94047 = CARTESIAN_POINT ( 'NONE',  ( -4.872636585019907152, 41.00341550150753278, -70.74912563391391984 ) ) ;
#94048 = CARTESIAN_POINT ( 'NONE',  ( -11.53880497916332004, 12.39660325957438225, -9.988508027600554229 ) ) ;
#94049 = ORIENTED_EDGE ( 'NONE', *, *, #33268, .T. ) ;
#94050 = CARTESIAN_POINT ( 'NONE',  ( -97.19700283461635593, -30.00000000007960921, 80.76470468910331135 ) ) ;
#94051 = ORIENTED_EDGE ( 'NONE', *, *, #55535, .F. ) ;
#94052 = CARTESIAN_POINT ( 'NONE',  ( -9.215420734788356327, -54.00000000000001421, 23.11721482942554928 ) ) ;
#94053 = DIRECTION ( 'NONE',  ( -1.000000000000000000, -1.224606353822377258E-16, -0.000000000000000000 ) ) ;
#94054 = DIRECTION ( 'NONE',  ( -1.000000000000000000, -1.224606353822377258E-16, -0.000000000000000000 ) ) ;
#94055 = CARTESIAN_POINT ( 'NONE',  ( 15.79412934197706875, 22.74951556322536561, -1.014593669854217950 ) ) ;
#94056 = CARTESIAN_POINT ( 'NONE',  ( 84.92072808231688441, -52.75190680617863137, -13.22419148268572719 ) ) ;
#94057 = CARTESIAN_POINT ( 'NONE',  ( 5.082755093536324154, -28.71875000204838813, 5.082755093536326818 ) ) ;
#94058 = CARTESIAN_POINT ( 'NONE',  ( -16.75187969033532553, 34.25544727262118982, 24.30698433968612449 ) ) ;
#94059 = CARTESIAN_POINT ( 'NONE',  ( 73.19785846594415091, -56.33009803196139842, -24.31540027847616869 ) ) ;
#94060 = ORIENTED_EDGE ( 'NONE', *, *, #68341, .T. ) ;
#94061 = DIRECTION ( 'NONE',  ( 0.000000000000000000, 0.000000000000000000, 1.000000000000000000 ) ) ;
#94062 = ORIENTED_EDGE ( 'NONE', *, *, #97424, .T. ) ;
#94063 = CARTESIAN_POINT ( 'NONE',  ( 48.87659302348946966, 8.116727071898608870, -16.52478270335645405 ) ) ;
#94064 = LINE ( 'NONE', #10474, #102402 ) ;
#94065 = B_SPLINE_CURVE_WITH_KNOTS ( 'NONE', 3,
 ( #97298, #30476, #55241, #105914, #46632, #39093, #22920, #54705, #13188, #103805, #22398, #15324, #80578, #88166 ),
 .UNSPECIFIED., .F., .F.,
 ( 4, 2, 2, 2, 2, 2, 4 ),
 ( 1.430489624538199204E-17, 0.0003846054458897452057, 0.0007692108917794760999, 0.001153816337669206831, 0.001538421783558937888, 0.002307632675338383305, 0.003076843567117829373 ),
 .UNSPECIFIED. ) ;
#94067 = ORIENTED_EDGE ( 'NONE', *, *, #80167, .F. ) ;
#94066 = CARTESIAN_POINT ( 'NONE',  ( -4.250000000000000000, 5.204748896376250699E-16, -1.971869939371574620 ) ) ;
#94068 = CARTESIAN_POINT ( 'NONE',  ( 82.56818838668320382, -18.68756746491115095, 139.1075167907083596 ) ) ;
#94069 = B_SPLINE_CURVE_WITH_KNOTS ( 'NONE', 3,
 ( #60008, #92865, #62131, #28711, #36281, #3337, #37334, #76146, #103101, #51870 ),
 .UNSPECIFIED., .F., .F.,
 ( 4, 2, 2, 2, 4 ),
 ( 0.000000000000000000, 0.001989602278884367460, 0.003979204557768734919, 0.005968806836653102812, 0.007958409115537469838 ),
 .UNSPECIFIED. ) ;
#94070 = ORIENTED_EDGE ( 'NONE', *, *, #96113, .F. ) ;
#94071 = CARTESIAN_POINT ( 'NONE',  ( 2.300474593523000433, -49.78500928328203656, 44.63801405044423376 ) ) ;
#94072 = CARTESIAN_POINT ( 'NONE',  ( -2.977408999572654480, -19.62500000204838457, 7.188101187499999156 ) ) ;
#94073 = CARTESIAN_POINT ( 'NONE',  ( -94.30950767697063952, -57.61975185784459086, 204.5257163505249309 ) ) ;
#94074 = EDGE_CURVE ( 'NONE', #28693, #13329, #93453, .T. ) ;
#94075 = CIRCLE ( 'NONE', #85458, 8.000000000000000000 ) ;
#94076 = VERTEX_POINT ( 'NONE', #16836 ) ;
#94077 =( GEOMETRIC_REPRESENTATION_CONTEXT ( 3 ) GLOBAL_UNCERTAINTY_ASSIGNED_CONTEXT ( ( #94715 ) ) GLOBAL_UNIT_ASSIGNED_CONTEXT ( ( #38904, #31365, #49081 ) ) REPRESENTATION_CONTEXT ( 'NONE', 'WORKASPACE' ) );
#94078 = CARTESIAN_POINT ( 'NONE',  ( 3.996139059897772405, 15.12531320464965390, 4.999999999999999112 ) ) ;
#94079 = EDGE_CURVE ( 'NONE', #23687, #84521, #99866, .T. ) ;
#94080 = CARTESIAN_POINT ( 'NONE',  ( 6.076047337594906672, 51.26610334597046403, -8.267531848790646620 ) ) ;
#94081 = CARTESIAN_POINT ( 'NONE',  ( 36.84999999999999432, 3.309500000000003439, 0.000000000000000000 ) ) ;
#94082 = VECTOR ( 'NONE', #39906, 1000.000000000000341 ) ;
#94083 = CARTESIAN_POINT ( 'NONE',  ( -5.656854249492379694, -16.62500000409677270, -5.656854249492380582 ) ) ;
#94084 = AXIS2_PLACEMENT_3D ( 'NONE', #59169, #53717, #94736 ) ;
#94085 = CARTESIAN_POINT ( 'NONE',  ( -39.97223656545506287, -26.31402483469310027, 35.94295830377559042 ) ) ;
#94086 = DIRECTION ( 'NONE',  ( 0.000000000000000000, -1.000000000000000000, 0.000000000000000000 ) ) ;
#94087 = CIRCLE ( 'NONE', #21742, 4.000000000000000888 ) ;
#94088 = FACE_OUTER_BOUND ( 'NONE', #51057, .T. ) ;
#94089 = CARTESIAN_POINT ( 'NONE',  ( -9.253817200599835147, 86.29992729916862970, -3.791916801615157873 ) ) ;
#94090 = CARTESIAN_POINT ( 'NONE',  ( 10.50000000000000533, -5.000000000000000000, -55.73109922009992800 ) ) ;
#94091 = APPLICATION_PROTOCOL_DEFINITION ( 'draft international standard', 'automotive_design', 1998, #106482 ) ;
#94092 = DIRECTION ( 'NONE',  ( -1.000000000000000000, 0.000000000000000000, 0.000000000000000000 ) ) ;
#94093 = EDGE_LOOP ( 'NONE', ( #77073, #28768, #100822, #56277, #46371 ) ) ;
#94094 =( LENGTH_UNIT ( ) NAMED_UNIT ( * ) SI_UNIT ( .MILLI., .METRE. ) );
#94095 = DIRECTION ( 'NONE',  ( 1.000000000000000000, 1.224606353822377258E-16, 0.000000000000000000 ) ) ;
#94096 = DIRECTION ( 'NONE',  ( -0.000000000000000000, 1.000000000000000000, -0.000000000000000000 ) ) ;
#94097 = CARTESIAN_POINT ( 'NONE',  ( 51.30196405314951846, -28.81598073202483690, -34.78016533206015737 ) ) ;
#94098 = CARTESIAN_POINT ( 'NONE',  ( -62.55748708953316850, -29.99999999999999289, 73.50292915578185671 ) ) ;
#94099 = VERTEX_POINT ( 'NONE', #89662 ) ;
#94100 = CARTESIAN_POINT ( 'NONE',  ( -15.83991689165957517, -4.333298119783902003, 8.379008989716211886 ) ) ;
#94101 = CARTESIAN_POINT ( 'NONE',  ( 75.17713619727400953, -57.57008159638389344, 191.1469172435081987 ) ) ;
#94102 = CARTESIAN_POINT ( 'NONE',  ( 6.123233995736763324E-16, 48.00000000000000000, -95.00000000000000000 ) ) ;
#94103 = CARTESIAN_POINT ( 'NONE',  ( 48.07208864154289785, -35.12482717350385997, -36.45831645058230919 ) ) ;
#94104 = CARTESIAN_POINT ( 'NONE',  ( 104.3757837139179117, 1.016364837396684119E-14, 0.000000000000000000 ) ) ;
#94105 = PRODUCT ( 'hex flange nut_din_Hexagon Flange Nut DIN 6923 - M8 - S', 'hex flange nut_din_Hexagon Flange Nut DIN 6923 - M8 - S', '', ( #97263 ) ) ;
#94106 = CARTESIAN_POINT ( 'NONE',  ( -53.29227158861940694, -60.00000000000000711, 80.45665323453354745 ) ) ;
#94107 = CYLINDRICAL_SURFACE ( 'NONE', #15830, 5.000000000000000888 ) ;
#94108 =( NAMED_UNIT ( * ) SI_UNIT ( $, .STERADIAN. ) SOLID_ANGLE_UNIT ( ) );
#94109 = AXIS2_PLACEMENT_3D ( 'NONE', #101168, #27330, #60208 ) ;
#94110 = CARTESIAN_POINT ( 'NONE',  ( -84.61722220583241949, -53.82794903670232856, 190.0724395252715340 ) ) ;
#94111 = VERTEX_POINT ( 'NONE', #91268 ) ;
#94112 = CARTESIAN_POINT ( 'NONE',  ( -27.10511071441183262, 34.47735702144344572, 10.05698433968616001 ) ) ;
#94113 = CARTESIAN_POINT ( 'NONE',  ( -5.121394014575314735, -49.92081713162068723, 32.19947040910868452 ) ) ;
#94114 = TOROIDAL_SURFACE ( 'NONE', #33862, 8.000000000000000000, 1.000000000000000000 ) ;
#94115 = CARTESIAN_POINT ( 'NONE',  ( -6.711450970696149376, 41.78336452847950966, -59.19447405778233673 ) ) ;
#94116 = CARTESIAN_POINT ( 'NONE',  ( 6.394343112843832166, 3.776352960569632877, 6.540835195019754522 ) ) ;
#94117 = CARTESIAN_POINT ( 'NONE',  ( 36.08349330513379982, -3.851859888774471706E-31, 4.000000000000001776 ) ) ;
#94118 = ORIENTED_EDGE ( 'NONE', *, *, #15713, .F. ) ;
#94119 = DIRECTION ( 'NONE',  ( -0.000000000000000000, -0.000000000000000000, -1.000000000000000000 ) ) ;
#94120 = CARTESIAN_POINT ( 'NONE',  ( 6.400000000000000355, 0.000000000000000000, 0.000000000000000000 ) ) ;
#94121 = CARTESIAN_POINT ( 'NONE',  ( 26.08349330513380693, 4.000000000000002665, 0.000000000000000000 ) ) ;
#94122 = CARTESIAN_POINT ( 'NONE',  ( -30.77294675439362592, 10.36444884528812871, -40.23167857000805014 ) ) ;
#94123 = EDGE_LOOP ( 'NONE', ( #77358, #72677, #77377, #92102, #103171 ) ) ;
#94124 = CARTESIAN_POINT ( 'NONE',  ( 27.97875226823191497, 296.5289436826013230, -9.637143995970028243 ) ) ;
#94125 = LINE ( 'NONE', #20293, #88065 ) ;
#94126 = CARTESIAN_POINT ( 'NONE',  ( -2.910977163136218682, -8.673617379884035472E-16, 22.23822744035697241 ) ) ;
#94127 = DIRECTION ( 'NONE',  ( 0.000000000000000000, -0.8299985787546592109, 0.5577655056251200616 ) ) ;
#94128 = B_SPLINE_CURVE_WITH_KNOTS ( 'NONE', 3,
 ( #75609, #75063, #99333, #10857, #1156, #34129 ),
 .UNSPECIFIED., .F., .F.,
 ( 4, 2, 4 ),
 ( 0.000000000000000000, 0.5000000000000000000, 1.000000000000000000 ),
 .UNSPECIFIED. ) ;
#94129 = CARTESIAN_POINT ( 'NONE',  ( 88.56622727954015772, -14.21045842199445630, 40.39835639566682346 ) ) ;
#94130 = CARTESIAN_POINT ( 'NONE',  ( -81.68110744402518719, -32.56240651117416007, 148.9491915846473660 ) ) ;
#94131 = VERTEX_POINT ( 'NONE', #58348 ) ;
#94132 = CARTESIAN_POINT ( 'NONE',  ( 43.51595707245915889, 485.1238408984536363, -1.707557185930880905 ) ) ;
#94133 = CARTESIAN_POINT ( 'NONE',  ( 10.12668159690567649, 0.000000000000000000, -10.00000000000000000 ) ) ;
#94134 = CARTESIAN_POINT ( 'NONE',  ( 42.58655652176065587, -57.68666533375992600, 60.21381296430073604 ) ) ;
#94135 = SURFACE_STYLE_FILL_AREA ( #6168 ) ;
#94136 = AXIS2_PLACEMENT_3D ( 'NONE', #5602, #55200, #63332 ) ;
#94137 = CARTESIAN_POINT ( 'NONE',  ( 40.61472136851750747, 317.8474547289473549, 3.573214933882146838 ) ) ;
#94138 = CARTESIAN_POINT ( 'NONE',  ( 89.93133926947346879, 5.000000000000023093, 6.123233995736781074E-16 ) ) ;
#94139 = ORIENTED_EDGE ( 'NONE', *, *, #720, .T. ) ;
#94140 = AXIS2_PLACEMENT_3D ( 'NONE', #7412, #47869, #39811 ) ;
#94141 = CARTESIAN_POINT ( 'NONE',  ( 4.446365519863139326, 54.30554020026675488, -6.355018452323170308 ) ) ;
#94142 = CARTESIAN_POINT ( 'NONE',  ( 31.45629285601395608, 439.3226217137470258, 23.14484626223100960 ) ) ;
#94143 = CARTESIAN_POINT ( 'NONE',  ( -7.188101187500002709, -24.31250000204838813, 2.977408999572648707 ) ) ;
#94144 = ORIENTED_EDGE ( 'NONE', *, *, #65597, .T. ) ;
#94145 = FILL_AREA_STYLE_COLOUR ( '', #31107 ) ;
#94146 = CARTESIAN_POINT ( 'NONE',  ( -0.3539438260514402579, 15.11738935797732886, 10.00000000000000000 ) ) ;
#94147 = CARTESIAN_POINT ( 'NONE',  ( 6.528715076640351000, 41.70354536979574078, -70.35321457523596678 ) ) ;
#94148 = ADVANCED_FACE ( 'NONE', ( #74519 ), #48603, .T. ) ;
#94149 = AXIS2_PLACEMENT_3D ( 'NONE', #74303, #34431, #74827 ) ;
#94150 = CARTESIAN_POINT ( 'NONE',  ( -37.84772257691307829, 50.00000000000000000, 50.69408796163851605 ) ) ;
#94151 = CYLINDRICAL_SURFACE ( 'NONE', #104161, 4.000000000000000000 ) ;
#94152 = EDGE_CURVE ( 'NONE', #89178, #49420, #21122, .T. ) ;
#94153 = DIRECTION ( 'NONE',  ( 1.000000000000000000, -0.000000000000000000, -0.000000000000000000 ) ) ;
#94154 = ORIENTED_EDGE ( 'NONE', *, *, #63635, .F. ) ;
#94155 = CARTESIAN_POINT ( 'NONE',  ( 91.67460378421274925, -59.99999999999997868, -15.10447286846676107 ) ) ;
#94156 = VECTOR ( 'NONE', #43300, 1000.000000000000000 ) ;
#94158 = CARTESIAN_POINT ( 'NONE',  ( 22.60328433090425904, -42.95462652055326913, 31.91884077397672570 ) ) ;
#94157 = CARTESIAN_POINT ( 'NONE',  ( -36.05833693101251214, -60.00000000000004263, 50.77755985414292184 ) ) ;
#94159 = CARTESIAN_POINT ( 'NONE',  ( 1.499834883077714618E-14, 1.499999999999992450, -61.23540616453487218 ) ) ;
#94160 =( BOUNDED_SURFACE ( )  B_SPLINE_SURFACE ( 3, 2, ( 
 ( #6262, #37636, #72076 ),
 ( #31129, #23026, #70500 ),
 ( #12241, #81208, #74186 ),
 ( #25147, #32709, #40763 ) ),
 .UNSPECIFIED., .F., .F., .F. ) 
 B_SPLINE_SURFACE_WITH_KNOTS ( ( 4, 4 ),
 ( 3, 3 ),
 ( 0.02391116761306513738, 0.02588704022068540056 ),
 ( 0.000000000000000000, 1.000000000000000000 ),
 .UNSPECIFIED. ) 
 GEOMETRIC_REPRESENTATION_ITEM ( )  RATIONAL_B_SPLINE_SURFACE ( (
 ( 1.000000000000000000, 0.9661530732048717596, 1.000000000000000000),
 ( 1.000000000000000000, 0.9668590359504447562, 1.000000000000000000),
 ( 1.000000000000000000, 0.9668459061114134112, 1.000000000000000000),
 ( 1.000000000000000000, 0.9661530732048707604, 1.000000000000000000) ) ) 
 REPRESENTATION_ITEM ( '' )  SURFACE ( )  );
#94161 = EDGE_CURVE ( 'NONE', #26151, #29545, #58898, .T. ) ;
#94162 = CARTESIAN_POINT ( 'NONE',  ( -38.04192487099758324, -60.27676763154023121, 41.50750820892533000 ) ) ;
#94163 = ORIENTED_EDGE ( 'NONE', *, *, #36130, .T. ) ;
#94164 = CARTESIAN_POINT ( 'NONE',  ( 34.06044893294480147, 463.4179081129763631, 6.463777546522439188 ) ) ;
#94165 =( GEOMETRIC_REPRESENTATION_CONTEXT ( 3 ) GLOBAL_UNCERTAINTY_ASSIGNED_CONTEXT ( ( #30866 ) ) GLOBAL_UNIT_ASSIGNED_CONTEXT ( ( #11343, #42670, #10295 ) ) REPRESENTATION_CONTEXT ( 'NONE', 'WORKASPACE' ) );
#94166 = CYLINDRICAL_SURFACE ( 'NONE', #69768, 7.000000000000006217 ) ;
#94167 = LINE ( 'NONE', #18712, #89582 ) ;
#94168 = AXIS2_PLACEMENT_3D ( 'NONE', #90196, #8738, #25502 ) ;
#94169 = AXIS2_PLACEMENT_3D ( 'NONE', #40006, #41595, #7091 ) ;
#94170 = DIRECTION ( 'NONE',  ( -1.000000000000000000, -1.224606353822377258E-16, -0.000000000000000000 ) ) ;
#94171 =( BOUNDED_SURFACE ( )  B_SPLINE_SURFACE ( 3, 2, ( 
 ( #83307, #83836, #32670 ),
 ( #49875, #98942, #26191 ),
 ( #65540, #82240, #66064 ),
 ( #49332, #91420, #41257 ) ),
 .UNSPECIFIED., .F., .F., .T. ) 
 B_SPLINE_SURFACE_WITH_KNOTS ( ( 4, 4 ),
 ( 3, 3 ),
 ( 7.589415207398531038E-19, 0.0009806926547533865134 ),
 ( 0.000000000000000000, 1.000000000000000000 ),
 .UNSPECIFIED. ) 
 GEOMETRIC_REPRESENTATION_ITEM ( )  RATIONAL_B_SPLINE_SURFACE ( (
 ( 1.000000000000000000, 0.9603284238771502279, 1.000000000000000000),
 ( 1.000000000000000000, 0.9551945799212738786, 1.000000000000000000),
 ( 1.000000000000000000, 0.9458776633876959661, 1.000000000000000000),
 ( 1.000000000000000000, 0.9359444767143307864, 1.000000000000000000) ) ) 
 REPRESENTATION_ITEM ( '' )  SURFACE ( )  );
#94172 = CARTESIAN_POINT ( 'NONE',  ( 6.289692432696588398, 5.239086202714920759, 4.583616368337912306 ) ) ;
#94173 = CARTESIAN_POINT ( 'NONE',  ( 12.39255972526328087, -3.227357870849989041, 20.63924567340875527 ) ) ;
#94174 = ORIENTED_EDGE ( 'NONE', *, *, #78052, .F. ) ;
#94175 = CARTESIAN_POINT ( 'NONE',  ( -64.25342926545496880, -38.33908962693352152, 110.6569961331102121 ) ) ;
#94176 = DIRECTION ( 'NONE',  ( 0.000000000000000000, 0.000000000000000000, -1.000000000000000000 ) ) ;
#94177 = CARTESIAN_POINT ( 'NONE',  ( 99.84195935041229575, -29.99999999999997868, 186.2662609802098075 ) ) ;
#94178 = CARTESIAN_POINT ( 'NONE',  ( -13.00575196869246852, 4.333941897774360896, -7.384322708455154149 ) ) ;
#94179 = CIRCLE ( 'NONE', #13236, 7.500000000000000000 ) ;
#94181 = EDGE_CURVE ( 'NONE', #67261, #63106, #15910, .T. ) ;
#94180 = CARTESIAN_POINT ( 'NONE',  ( -5.999787407977321685, -81.00031888815553316, 0.2740427891043037412 ) ) ;
#94182 = CIRCLE ( 'NONE', #33911, 4.000000000000000888 ) ;
#94183 = CARTESIAN_POINT ( 'NONE',  ( 81.59412300828947195, -30.00000000000000000, -6.883953906076696327 ) ) ;
#94184 = CARTESIAN_POINT ( 'NONE',  ( 6.499999999999999112, -1.280811194704862377, -0.07768058122908151619 ) ) ;
#94185 = ORIENTED_EDGE ( 'NONE', *, *, #64924, .F. ) ;
#94186 = VERTEX_POINT ( 'NONE', #7132 ) ;
#94187 = EDGE_LOOP ( 'NONE', ( #74991, #89544, #63128, #103861 ) ) ;
#94188 = CARTESIAN_POINT ( 'NONE',  ( 1.000000000000000000, -69.59657292934913642, 12.76848391599222765 ) ) ;
#94189 = DIRECTION ( 'NONE',  ( 1.000000000000000000, -0.000000000000000000, 1.224646799147353207E-16 ) ) ;
#94190 = CARTESIAN_POINT ( 'NONE',  ( 0.000000000000000000, 4.898587196589412829E-16, -4.000000000000000000 ) ) ;
#94191 = CARTESIAN_POINT ( 'NONE',  ( -37.71419144549415137, 397.5045696453483401, 6.418798809479165257 ) ) ;
#94192 = CARTESIAN_POINT ( 'NONE',  ( 10.50000000000000178, -5.000000000000000000, -12.52300748975612166 ) ) ;
#94193 = CARTESIAN_POINT ( 'NONE',  ( 52.56483885390524335, 49.99999999999999289, -38.23529411764707220 ) ) ;
#94194 = ORIENTED_EDGE ( 'NONE', *, *, #38891, .F. ) ;
#94195 = CARTESIAN_POINT ( 'NONE',  ( -2.617478844992341180, 49.99999999999999289, -75.26027323389158141 ) ) ;
#94196 = ORIENTED_EDGE ( 'NONE', *, *, #73604, .T. ) ;
#94197 = CARTESIAN_POINT ( 'NONE',  ( -4.472135954999578722, -65.00000000000000000, 4.000000000000002665 ) ) ;
#94198 = CARTESIAN_POINT ( 'NONE',  ( 36.08349330513379982, 4.898587196589411843E-16, -4.000000000000001776 ) ) ;
#94199 = CARTESIAN_POINT ( 'NONE',  ( 25.53945892759312031, 5.000000000000004441, 6.123233995736770227E-16 ) ) ;
#94200 = CARTESIAN_POINT ( 'NONE',  ( 29.13916688973899483, 297.4007265668975606, 2.495279913412661088 ) ) ;
#94201 = AXIS2_PLACEMENT_3D ( 'NONE', #49822, #8299, #81637 ) ;
#94202 = LINE ( 'NONE', #12204, #82020 ) ;
#94203 = CARTESIAN_POINT ( 'NONE',  ( 59.97286723080061677, -22.12426351543174619, 64.13356965173628055 ) ) ;
#94204 = ORIENTED_EDGE ( 'NONE', *, *, #84869, .T. ) ;
#94205 = CARTESIAN_POINT ( 'NONE',  ( 29.27148335582070615, 13.57837266936924081, -39.67318301868883168 ) ) ;
#94206 = AXIS2_PLACEMENT_3D ( 'NONE', #8982, #96944, #32769 ) ;
#94207 = DIRECTION ( 'NONE',  ( -0.8191520442889974607, 0.000000000000000000, -0.5735764363510380548 ) ) ;
#94208 = DIRECTION ( 'NONE',  ( -0.000000000000000000, -0.000000000000000000, -1.000000000000000000 ) ) ;
#94209 = CARTESIAN_POINT ( 'NONE',  ( 81.26467260280679739, 1.016364837396684119E-14, 0.000000000000000000 ) ) ;
#94210 = ADVANCED_FACE ( 'NONE', ( #40043 ), #41779, .T. ) ;
#94211 = ORIENTED_EDGE ( 'NONE', *, *, #54219, .T. ) ;
#94212 = CARTESIAN_POINT ( 'NONE',  ( -20.00000000000000000, 12.99999999999999467, -6.999999999999999112 ) ) ;
#94213 = CARTESIAN_POINT ( 'NONE',  ( 11.89131030317610183, 1.482358050883964840E-15, 0.000000000000000000 ) ) ;
#94214 = CARTESIAN_POINT ( 'NONE',  ( 16.75187969033515145, 34.99134772383131775, -21.80698433968624528 ) ) ;
#94215 = CARTESIAN_POINT ( 'NONE',  ( 105.5353273971932140, 6.123233995736568081E-16, -5.000000000000011546 ) ) ;
#94216 = EDGE_CURVE ( 'NONE', #64733, #95564, #71031, .T. ) ;
#94217 = ADVANCED_FACE ( 'NONE', ( #67516 ), #34647, .F. ) ;
#94218 = CARTESIAN_POINT ( 'NONE',  ( -7.551560007654696705, 101.9908964819301076, -2.648022159607842596 ) ) ;
#94219 = CARTESIAN_POINT ( 'NONE',  ( -39.56197461363974099, -0.1944580884125578779, 19.78098730681987760 ) ) ;
#94220 = CARTESIAN_POINT ( 'NONE',  ( -0.2259792476677689177, 7.636022678937404606, -6.470294263593365791 ) ) ;
#94221 = CARTESIAN_POINT ( 'NONE',  ( 86.37779416861748416, -20.93961008912989286, 181.4651759308039232 ) ) ;
#94222 = CIRCLE ( 'NONE', #39176, 7.500000000000000000 ) ;
#94223 = CARTESIAN_POINT ( 'NONE',  ( -5.209583662784837088, 5.600999057173902784, -26.19773573556262392 ) ) ;
#94224 = CIRCLE ( 'NONE', #45943, 4.000000000000001776 ) ;
#94225 = CARTESIAN_POINT ( 'NONE',  ( -3.002903359416353002, 102.9618411113580834, 5.000000000000000000 ) ) ;
#94226 = ORIENTED_EDGE ( 'NONE', *, *, #18018, .T. ) ;
#94227 = CARTESIAN_POINT ( 'NONE',  ( -7.549004593702460575, 4.358419834287831307, -7.700121441565837443 ) ) ;
#94228 = CARTESIAN_POINT ( 'NONE',  ( 83.86866073052654258, 1.030564683017419500E-14, 0.000000000000000000 ) ) ;
#94229 = DIRECTION ( 'NONE',  ( -0.5735764363510512664, 0.8191520442889881348, 1.003171929053520309E-16 ) ) ;
#94230 = CARTESIAN_POINT ( 'NONE',  ( 34.87160327596053833, 435.0271987811416921, 7.834040158382404861 ) ) ;
#94231 = CARTESIAN_POINT ( 'NONE',  ( -85.32909183395112507, -29.99999999999999645, 59.83043280556380950 ) ) ;
#94232 = EDGE_CURVE ( 'NONE', #54015, #28073, #5592, .T. ) ;
#94233 = AXIS2_PLACEMENT_3D ( 'NONE', #86188, #12260, #45191 ) ;
#94234 = CARTESIAN_POINT ( 'NONE',  ( -37.52579488121514117, 438.0832148649091096, 4.091984033318601277 ) ) ;
#94235 = AXIS2_PLACEMENT_3D ( 'NONE', #36587, #4178, #86183 ) ;
#94236 = CARTESIAN_POINT ( 'NONE',  ( 14.56780743600302586, -57.67141137934046924, 41.74351479442032087 ) ) ;
#94238 = CARTESIAN_POINT ( 'NONE',  ( 18.41162169223098033, 304.6294254666754568, 9.889731659030220001 ) ) ;
#94237 = CARTESIAN_POINT ( 'NONE',  ( 9.204625048146249711, 43.65511487171167460, 14.80422153561283771 ) ) ;
#94239 = EDGE_CURVE ( 'NONE', #54290, #54096, #11915, .T. ) ;
#94240 = CARTESIAN_POINT ( 'NONE',  ( 2.399714434301968069, -53.72915769422170484, 40.79469093396801327 ) ) ;
#94241 = CARTESIAN_POINT ( 'NONE',  ( -10.00000000000000000, 15.00000000000000000, 10.00000000000000000 ) ) ;
#94242 = CARTESIAN_POINT ( 'NONE',  ( -18.87830327030985345, 49.99999999999999289, 60.75080805445377763 ) ) ;
#94243 = CARTESIAN_POINT ( 'NONE',  ( -43.63930228691581448, 486.5321682125791654, 6.480714085072397879 ) ) ;
#94244 = DIRECTION ( 'NONE',  ( -1.000000000000000000, -1.224606353822377258E-16, -0.000000000000000000 ) ) ;
#94245 = PRESENTATION_LAYER_ASSIGNMENT (  '', '', ( #66668 ) ) ;
#94246 = VECTOR ( 'NONE', #62577, 999.9999999999998863 ) ;
#94247 = EDGE_CURVE ( 'NONE', #18823, #26788, #56792, .T. ) ;
#94248 = CARTESIAN_POINT ( 'NONE',  ( 22.09068723947702395, -19.16686062785725753, -33.43374534816550891 ) ) ;
#94249 = DIRECTION ( 'NONE',  ( 0.000000000000000000, 0.000000000000000000, -1.000000000000000000 ) ) ;
#94250 = CARTESIAN_POINT ( 'NONE',  ( -23.68218076818291706, -39.47912890587980428, 31.49652407728643055 ) ) ;
#94251 = VERTEX_POINT ( 'NONE', #59430 ) ;
#94252 = CARTESIAN_POINT ( 'NONE',  ( 39.28947510688216482, 485.2043936288979467, -4.359233426732569860 ) ) ;
#94253 = CARTESIAN_POINT ( 'NONE',  ( 76.12557658274099026, -38.35599704320051018, -28.58424740099938077 ) ) ;
#94254 = CARTESIAN_POINT ( 'NONE',  ( -18.86856976124040486, -32.51467859884330380, 29.71142835944370830 ) ) ;
#94256 = CARTESIAN_POINT ( 'NONE',  ( 1.219931503106709281, 36.63069750044676454, -28.81634217350109495 ) ) ;
#94255 = CARTESIAN_POINT ( 'NONE',  ( -1.219521042794267762, 27.62924000314889739, 39.81737217016015506 ) ) ;
#94257 = ORIENTED_EDGE ( 'NONE', *, *, #41675, .F. ) ;
#94258 = B_SPLINE_CURVE_WITH_KNOTS ( 'NONE', 3,
 ( #95588, #28232, #21724, #21204, #54566, #20152, #87502, #77812 ),
 .UNSPECIFIED., .F., .F.,
 ( 4, 2, 2, 4 ),
 ( 3.469446951953614189E-18, 0.002163004473986925285, 0.003244506710980385976, 0.004326008947973847100 ),
 .UNSPECIFIED. ) ;
#94259 = ORIENTED_EDGE ( 'NONE', *, *, #106628, .T. ) ;
#94260 = CARTESIAN_POINT ( 'NONE',  ( 20.19615384615384457, 4.172000000000003261, 5.109226446042759579E-16 ) ) ;
#94261 = CARTESIAN_POINT ( 'NONE',  ( 24.83349330513380693, -4.000000000000000888, 4.898587196589416773E-16 ) ) ;
#94262 = CARTESIAN_POINT ( 'NONE',  ( -5.656854249492379694, -24.12500000409677270, -5.656854249492380582 ) ) ;
#94263 = B_SPLINE_CURVE_WITH_KNOTS ( 'NONE', 3,
 ( #63120, #22147, #79819, #87407 ),
 .UNSPECIFIED., .F., .F.,
 ( 4, 4 ),
 ( 8.270465868445859332E-17, 0.003416952886430538790 ),
 .UNSPECIFIED. ) ;
#94264 = ORIENTED_EDGE ( 'NONE', *, *, #91986, .F. ) ;
#94265 = CARTESIAN_POINT ( 'NONE',  ( 6.062025480873725947, 50.00000000000000000, -74.52240934977429276 ) ) ;
#94266 = CARTESIAN_POINT ( 'NONE',  ( 100.4946997161162443, -37.84604486669937984, 189.5797555323898962 ) ) ;
#94268 = CARTESIAN_POINT ( 'NONE',  ( -47.90408546931278266, 11.89605000366066889, 14.35535821593516737 ) ) ;
#94267 = CARTESIAN_POINT ( 'NONE',  ( 49.18359670589789090, -37.81820580435596213, 48.86208063644627941 ) ) ;
#94269 = VERTEX_POINT ( 'NONE', #28677 ) ;
#94270 = B_SPLINE_CURVE_WITH_KNOTS ( 'NONE', 3,
 ( #98644, #88979, #47963, #57648, #99174, #6446, #6981, #39899, #72773, #105679, #64702, #44153, #43088, #34503, #2072, #85136, #59814, #978, #68434, #35024, #58748, #25891, #1536, #101846, #51154, #101327, #74894, #11227, #10172, #33961 ),
 .UNSPECIFIED., .F., .F.,
 ( 4, 2, 2, 2, 2, 2, 2, 2, 2, 2, 2, 2, 2, 2, 4 ),
 ( 0.01188303771272031933, 0.01280230725828193292, 0.01326194203106274318, 0.01372157680384355344, 0.01418121157662436196, 0.01441102896301475929, 0.01464084634940515488, 0.01487066373579555220, 0.01510048112218594432, 0.01556011589496672856, 0.01601975066774751280, 0.01647938544052829704, 0.01739865498608986205, 0.01831792453165143053, 0.01923719407721299207 ),
 .UNSPECIFIED. ) ;
#94271 = VERTEX_POINT ( 'NONE', #77732 ) ;
#94272 = AXIS2_PLACEMENT_3D ( 'NONE', #55418, #95374, #80230 ) ;
#94273 = EDGE_LOOP ( 'NONE', ( #24840, #51916, #59688, #51032 ) ) ;
#94274 = CARTESIAN_POINT ( 'NONE',  ( 26.27519682077350893, 310.0374129758119466, 11.16578451142825656 ) ) ;
#94275 = DIRECTION ( 'NONE',  ( 0.000000000000000000, 0.000000000000000000, 1.000000000000000000 ) ) ;
#94276 = ORIENTED_EDGE ( 'NONE', *, *, #28804, .T. ) ;
#94277 = EDGE_CURVE ( 'NONE', #25041, #82621, #8965, .T. ) ;
#94278 = DIRECTION ( 'NONE',  ( 0.000000000000000000, -1.000000000000000000, 0.000000000000000000 ) ) ;
#94279 = CARTESIAN_POINT ( 'NONE',  ( -7.263014275236301387, 5.510894801153387590, -4.742459152899539454 ) ) ;
#94280 = CARTESIAN_POINT ( 'NONE',  ( -94.91350004442121246, -59.99999999999032951, -11.18889123746408920 ) ) ;
#94281 = DIRECTION ( 'NONE',  ( -1.000000000000000000, -1.224606353822377258E-16, -0.000000000000000000 ) ) ;
#94282 = CARTESIAN_POINT ( 'NONE',  ( 32.54749815468527885, -60.00000000000002132, 44.51763105449811064 ) ) ;
#94283 = CARTESIAN_POINT ( 'NONE',  ( 16.14595037822613932, 12.99999999999999289, 0.000000000000000000 ) ) ;
#94284 = CARTESIAN_POINT ( 'NONE',  ( -6.338673264423879239, 41.81695718870634693, -59.02782128990620691 ) ) ;
#94286 = CARTESIAN_POINT ( 'NONE',  ( 6.227159620205909185, -60.35885591111542681, 33.93934178768890320 ) ) ;
#94285 = CARTESIAN_POINT ( 'NONE',  ( -94.62342829788488530, -14.21045842199438525, 80.85070941463327188 ) ) ;
#94287 = EDGE_CURVE ( 'NONE', #72439, #9941, #64203, .T. ) ;
#94288 = FACE_OUTER_BOUND ( 'NONE', #11112, .T. ) ;
#94289 = AXIS2_PLACEMENT_3D ( 'NONE', #10302, #27073, #1671 ) ;
#94290 = EDGE_CURVE ( 'NONE', #49400, #57533, #37568, .T. ) ;
#94291 = CARTESIAN_POINT ( 'NONE',  ( -47.58650698943795021, -56.82114114556742379, 52.30438436347986908 ) ) ;
#94292 = VERTEX_POINT ( 'NONE', #11370 ) ;
#94293 = CARTESIAN_POINT ( 'NONE',  ( 3.553996988732007534, -69.76421179181549803, 13.45721127476620005 ) ) ;
#94294 = ORIENTED_EDGE ( 'NONE', *, *, #82894, .T. ) ;
#94295 = CARTESIAN_POINT ( 'NONE',  ( 30.59999999999999787, -3.309499999999999886, 0.000000000000000000 ) ) ;
#94296 = CARTESIAN_POINT ( 'NONE',  ( 18.00631980831534307, 36.44533851663729251, 23.17937010874015158 ) ) ;
#94297 = EDGE_CURVE ( 'NONE', #22931, #59650, #10318, .T. ) ;
#94298 = CARTESIAN_POINT ( 'NONE',  ( 5.996380728650903436, 2.731133088746460658, 6.499999999999999112 ) ) ;
#94299 = ORIENTED_EDGE ( 'NONE', *, *, #6506, .F. ) ;
#94300 = CARTESIAN_POINT ( 'NONE',  ( 5.858824175751778718, 246.2142093912763698, -1.318356988357147097 ) ) ;
#94301 = STYLED_ITEM ( 'NONE', ( #71239 ), #67118 ) ;
#94302 = ORIENTED_EDGE ( 'NONE', *, *, #71134, .F. ) ;
#94303 = CARTESIAN_POINT ( 'NONE',  ( 92.64207125262521458, -29.99999999987929655, 51.61815748969144124 ) ) ;
#94304 = EDGE_CURVE ( 'NONE', #62753, #1547, #19613, .T. ) ;
#94305 = CARTESIAN_POINT ( 'NONE',  ( 3.365451957726352639, -49.06858650466293881, 104.1992105446093859 ) ) ;
#94307 = EDGE_CURVE ( 'NONE', #51964, #102392, #65793, .T. ) ;
#94306 = DIRECTION ( 'NONE',  ( 0.9090909090909086165, 0.000000000000000000, 0.4165977904505319684 ) ) ;
#94308 = CARTESIAN_POINT ( 'NONE',  ( 7.754160006592983656, 42.00000000000000711, 59.23741894013591036 ) ) ;
#94309 = CARTESIAN_POINT ( 'NONE',  ( 98.19688506443435472, -30.00000000000000355, 190.3059900313137689 ) ) ;
#94310 =( BOUNDED_CURVE ( )  B_SPLINE_CURVE ( 2, ( #61629, #2278, #27687, #94522, #93451, #2821, #52981, #20671, #53512 ),
 .UNSPECIFIED., .F., .F. ) 
 B_SPLINE_CURVE_WITH_KNOTS ( ( 3, 2, 2, 2, 3 ),
 ( 0.6911764705882353921, 0.6985294117647059542, 0.7058823529411766273, 0.7132352941176471894, 0.7205882352941177516 ),
 .UNSPECIFIED. ) 
 CURVE ( )  GEOMETRIC_REPRESENTATION_ITEM ( )  RATIONAL_B_SPLINE_CURVE ( ( 0.9999999999999988898, 0.9238795325112878487, 1.000000000000000000, 0.9238795325112867385, 1.000000000000000000, 0.9238795325112867385, 1.000000000000000000, 0.9238795325112856283, 1.000000000000001110 ) ) 
 REPRESENTATION_ITEM ( '' )  );
#94311 = FACE_OUTER_BOUND ( 'NONE', #45397, .T. ) ;
#94312 = VERTEX_POINT ( 'NONE', #103353 ) ;
#94313 = B_SPLINE_CURVE_WITH_KNOTS ( 'NONE', 3,
 ( #60757, #12171, #4099, #93645, #86635, #2482, #60235, #101197, #27356, #45103, #19793, #93103, #61825, #35974, #18715, #52627, #19275, #52103, #37027, #85012, #11096, #69896, #44021, #84485, #76914, #69372, #27890, #3024, #36505, #68846, #85560, #102794, #11635, #44568 ),
 .UNSPECIFIED., .F., .F.,
 ( 4, 2, 2, 2, 2, 2, 2, 2, 2, 2, 2, 2, 2, 2, 2, 2, 4 ),
 ( 0.000000000000000000, 0.0007951492273476290984, 0.001590298454695258197, 0.002385447682042887187, 0.003180596909390516393, 0.003975746136738159478, 0.004770895364085802996, 0.005566044591433445647, 0.006361193818781088298, 0.007156343046128731816, 0.007951492273476374467, 0.008746641500824017118, 0.009541790728171658034, 0.01033693995551929895, 0.01113208918286694160, 0.01192723841021458425, 0.01272238763756222690 ),
 .UNSPECIFIED. ) ;
#94314 = ORIENTED_EDGE ( 'NONE', *, *, #91802, .F. ) ;
#94315 = EDGE_LOOP ( 'NONE', ( #69740, #26365, #33235, #65002, #88937 ) ) ;
#94316 = CARTESIAN_POINT ( 'NONE',  ( 54.63781606259024670, -32.56084225145857403, 56.78402738445370090 ) ) ;
#94317 = AXIS2_PLACEMENT_3D ( 'NONE', #89352, #40255, #25167 ) ;
#94318 = CARTESIAN_POINT ( 'NONE',  ( 56.48317336153285595, 6.856755485862130937E-15, 0.000000000000000000 ) ) ;
#94319 = CONICAL_SURFACE ( 'NONE', #70128, 3.309500000000001663, 0.9599310885968770357 ) ;
#94320 = CARTESIAN_POINT ( 'NONE',  ( 26.84999999999999787, 3.309500000000003439, 0.000000000000000000 ) ) ;
#94321 = VERTEX_POINT ( 'NONE', #54234 ) ;
#94322 = CARTESIAN_POINT ( 'NONE',  ( -91.32775393698508992, -38.36579091124441021, -2.591198299663252325 ) ) ;
#94323 = ORIENTED_EDGE ( 'NONE', *, *, #62426, .T. ) ;
#94324 = CARTESIAN_POINT ( 'NONE',  ( 0.5984201754795559491, 8.314755988442765755, -0.7022220667781327030 ) ) ;
#94325 = CARTESIAN_POINT ( 'NONE',  ( 94.69161108849048958, -38.49000774377354617, 201.2185778078309113 ) ) ;
#94326 = CARTESIAN_POINT ( 'NONE',  ( 12.80938200527896420, 18.86218302254438939, 8.106113376688432126 ) ) ;
#94328 = CARTESIAN_POINT ( 'NONE',  ( 83.72129867378865242, -45.28294897705733035, 15.97319318370404773 ) ) ;
#94327 = AXIS2_PLACEMENT_3D ( 'NONE', #40460, #15119, #48005 ) ;
#94329 = CIRCLE ( 'NONE', #11681, 4.000000000000001776 ) ;
#94330 = CARTESIAN_POINT ( 'NONE',  ( 32.95763196807708795, 360.4691531110863139, 22.50890827065293109 ) ) ;
#94331 = CARTESIAN_POINT ( 'NONE',  ( 2.152702816551222309, -7.044814775684611341, -13.28738398835386292 ) ) ;
#94332 = CARTESIAN_POINT ( 'NONE',  ( -43.77664590664327449, 434.3717993398990984, 11.97532627841979469 ) ) ;
#94333 = CARTESIAN_POINT ( 'NONE',  ( 3.021274963869413188, 104.3221744949810414, 5.000000000000000000 ) ) ;
#94334 = AXIS2_PLACEMENT_3D ( 'NONE', #78098, #4215, #61944 ) ;
#94335 = ORIENTED_EDGE ( 'NONE', *, *, #82081, .T. ) ;
#94336 = DIRECTION ( 'NONE',  ( -0.000000000000000000, 1.000000000000000000, -0.000000000000000000 ) ) ;
#94337 = CARTESIAN_POINT ( 'NONE',  ( 7.499999999993815614, 40.28819020807626572, -69.28872355931217442 ) ) ;
#94339 = CARTESIAN_POINT ( 'NONE',  ( 0.000000000000000000, 0.000000000000000000, -4.289342857142857568 ) ) ;
#94338 = B_SPLINE_CURVE_WITH_KNOTS ( 'NONE', 3,
 ( #99338, #11794, #29116, #60387, #37185, #93264, #70047, #44726, #3732, #85171, #102418, #94876, #19426, #102952, #61985, #25517, #21016, #53856, #41657, #74545 ),
 .UNSPECIFIED., .F., .F.,
 ( 4, 2, 2, 2, 2, 2, 2, 2, 2, 4 ),
 ( 0.0009441224788332248452, 0.001448919914566970018, 0.001953717350300715298, 0.002458514786034460362, 0.002963312221768203258, 0.003468109657501946153, 0.003972907093235689482, 0.004225305811102560496, 0.004477704528969431511, 0.004982501964703167467 ),
 .UNSPECIFIED. ) ;
#94340 = ORIENTED_EDGE ( 'NONE', *, *, #25446, .T. ) ;
#94341 = VECTOR ( 'NONE', #10893, 1000.000000000000000 ) ;
#94342 = DIRECTION ( 'NONE',  ( 0.000000000000000000, 1.000000000000000000, 0.000000000000000000 ) ) ;
#94343 = CARTESIAN_POINT ( 'NONE',  ( -39.14206789509485418, 314.2215094627067629, 6.606931266694046734 ) ) ;
#94344 = CARTESIAN_POINT ( 'NONE',  ( -7.150000000000001243, 41.64999999999999147, -68.91429205801802027 ) ) ;
#94345 = CARTESIAN_POINT ( 'NONE',  ( -14.90155531858861870, 42.58002643027919021, -90.01374843399875658 ) ) ;
#94346 = CARTESIAN_POINT ( 'NONE',  ( 8.000000000000000000, -19.99999999999999289, 0.000000000000000000 ) ) ;
#94347 = CARTESIAN_POINT ( 'NONE',  ( 14.68095810428979853, -17.65437676951217227, 35.02762473332876425 ) ) ;
#94348 = EDGE_CURVE ( 'NONE', #77934, #6808, #102280, .T. ) ;
#94349 = CONICAL_SURFACE ( 'NONE', #8164, 2747.477419454587107, 1.221730476396026610 ) ;
#94350 = FACE_OUTER_BOUND ( 'NONE', #39597, .T. ) ;
#94351 = ORIENTED_EDGE ( 'NONE', *, *, #95120, .F. ) ;
#94352 = CARTESIAN_POINT ( 'NONE',  ( 85.48291297220137608, -32.15055455726690070, 180.9890288920893511 ) ) ;
#94354 = AXIS2_PLACEMENT_3D ( 'NONE', #5284, #13346, #37688 ) ;
#94353 = CARTESIAN_POINT ( 'NONE',  ( -48.90200833301644678, 9.381371963275082493, 14.70088518568426927 ) ) ;
#94355 = CYLINDRICAL_SURFACE ( 'NONE', #33173, 4.000000000000000888 ) ;
#94356 = ORIENTED_EDGE ( 'NONE', *, *, #48252, .F. ) ;
#94357 = CARTESIAN_POINT ( 'NONE',  ( -92.21955131628659785, -52.71021242866512324, 76.94161136100676401 ) ) ;
#94358 = CARTESIAN_POINT ( 'NONE',  ( 59.89460441624491693, 4.000000000000013323, 0.000000000000000000 ) ) ;
#94359 = CARTESIAN_POINT ( 'NONE',  ( -13.14930780082137396, -5.000000000000002665, -86.33530272370370540 ) ) ;
#94360 = CARTESIAN_POINT ( 'NONE',  ( -29.87373162892149026, 8.058069557479628386, 42.09632259471302973 ) ) ;
#94361 = PRESENTATION_LAYER_ASSIGNMENT (  '', '', ( #47809 ) ) ;
#94362 =( LENGTH_UNIT ( ) NAMED_UNIT ( * ) SI_UNIT ( .MILLI., .METRE. ) );
#94363 = CARTESIAN_POINT ( 'NONE',  ( 21.30699193799562252, -60.00000000000000711, 40.40681636397585663 ) ) ;
#94364 = CARTESIAN_POINT ( 'NONE',  ( -86.78976035038994041, -38.00000000000004974, 188.4439161865618644 ) ) ;
#94365 = CARTESIAN_POINT ( 'NONE',  ( 39.79890337217759821, -26.23938249810791845, 35.83377390011310126 ) ) ;
#94366 =( GEOMETRIC_REPRESENTATION_CONTEXT ( 3 ) GLOBAL_UNCERTAINTY_ASSIGNED_CONTEXT ( ( #89048 ) ) GLOBAL_UNIT_ASSIGNED_CONTEXT ( ( #8046, #5921, #105162 ) ) REPRESENTATION_CONTEXT ( 'NONE', 'WORKASPACE' ) );
#94368 = CARTESIAN_POINT ( 'NONE',  ( -12.86856004683486709, 21.39988744414081268, 5.451043748370874020 ) ) ;
#94367 = CARTESIAN_POINT ( 'NONE',  ( -29.55526716209243077, -32.15409974475024768, 40.32020078543521180 ) ) ;
#94369 = EDGE_CURVE ( 'NONE', #49452, #26937, #3904, .T. ) ;
#94370 = CARTESIAN_POINT ( 'NONE',  ( -1.435124379509183671E-09, 294.8518027762758038, -10.00000000000000178 ) ) ;
#94371 = CARTESIAN_POINT ( 'NONE',  ( 45.33180403702434091, 464.4945808635454227, 2.178908857919817699 ) ) ;
#94372 = CARTESIAN_POINT ( 'NONE',  ( 42.49652511093216134, 334.4904238026493886, 7.585808180445239302 ) ) ;
#94373 = CARTESIAN_POINT ( 'NONE',  ( 35.58361799548379167, 1.482358050883964840E-15, 0.000000000000000000 ) ) ;
#94374 = CARTESIAN_POINT ( 'NONE',  ( 4.250000000000000000, 0.000000000000000000, -3.393184225085859929 ) ) ;
#94375 = ORIENTED_EDGE ( 'NONE', *, *, #79970, .T. ) ;
#94376 = EDGE_CURVE ( 'NONE', #105760, #23483, #79904, .T. ) ;
#94377 = CARTESIAN_POINT ( 'NONE',  ( 5.450967621166023847, -4.358435876041018453, -0.3607371497494629708 ) ) ;
#94378 = AXIS2_PLACEMENT_3D ( 'NONE', #95811, #80132, #94764 ) ;
#94379 = DIRECTION ( 'NONE',  ( 0.000000000000000000, 0.000000000000000000, -1.000000000000000000 ) ) ;
#94380 = VERTEX_POINT ( 'NONE', #77483 ) ;
#94381 = CARTESIAN_POINT ( 'NONE',  ( -11.08629307112589224, -1.234131506493649333, 20.41691545949602826 ) ) ;
#94382 = DIRECTION ( 'NONE',  ( 1.000000000000000000, -0.000000000000000000, -0.000000000000000000 ) ) ;
#94383 = DIRECTION ( 'NONE',  ( -1.000000000000000000, -0.000000000000000000, -0.000000000000000000 ) ) ;
#94384 = CARTESIAN_POINT ( 'NONE',  ( -4.829386694092057120, -60.22815139279438057, -36.87030747315908030 ) ) ;
#94385 = ORIENTED_EDGE ( 'NONE', *, *, #17917, .T. ) ;
#94386 = CARTESIAN_POINT ( 'NONE',  ( 1.469576158976828483E-15, 1.000000000000000888, 12.00000000000003908 ) ) ;
#94387 = SURFACE_STYLE_FILL_AREA ( #3779 ) ;
#94388 = AXIS2_PLACEMENT_3D ( 'NONE', #9083, #81904, #81370 ) ;
#94389 = EDGE_LOOP ( 'NONE', ( #27494, #7736, #37335, #14439 ) ) ;
#94390 = CARTESIAN_POINT ( 'NONE',  ( -3.321851460894552355E-15, 5.469921996229796690, -3.525817189091414949 ) ) ;
#94391 = DIRECTION ( 'NONE',  ( 1.000000000000000000, 1.224606353822377258E-16, 0.000000000000000000 ) ) ;
#94392 = PRODUCT_RELATED_PRODUCT_CATEGORY ( 'part', '', ( #19209 ) ) ;
#94393 = CARTESIAN_POINT ( 'NONE',  ( -94.46259299136239918, -59.99999999999999289, 45.00074042340703784 ) ) ;
#94394 =( GEOMETRIC_REPRESENTATION_CONTEXT ( 3 ) GLOBAL_UNCERTAINTY_ASSIGNED_CONTEXT ( ( #44913 ) ) GLOBAL_UNIT_ASSIGNED_CONTEXT ( ( #37370, #85354, #70235 ) ) REPRESENTATION_CONTEXT ( 'NONE', 'WORKASPACE' ) );
#94395 = ORIENTED_EDGE ( 'NONE', *, *, #91013, .T. ) ;
#94396 = CARTESIAN_POINT ( 'NONE',  ( -8.369914041613094824, 42.00000000000000000, -59.54702718917638293 ) ) ;
#94397 = CARTESIAN_POINT ( 'NONE',  ( -5.000000000000000000, 0.000000000000000000, -9.974599999999998801 ) ) ;
#94398 = STYLED_ITEM ( 'NONE', ( #100001 ), #38431 ) ;
#94399 = CARTESIAN_POINT ( 'NONE',  ( 32.62207953394533178, 1.482358050883964840E-15, 0.000000000000000000 ) ) ;
#94400 = CARTESIAN_POINT ( 'NONE',  ( -9.797372177749753774, 26.53490505152436185, 2.014953862275842944 ) ) ;
#94402 = DIRECTION ( 'NONE',  ( -0.000000000000000000, 1.000000000000000000, -0.000000000000000000 ) ) ;
#94401 = CARTESIAN_POINT ( 'NONE',  ( 44.13784562318636517, 464.3950638386343712, 9.689741638646596655 ) ) ;
#94403 = CARTESIAN_POINT ( 'NONE',  ( -84.24477676735598664, -29.03027281900111589, 164.8630760665813284 ) ) ;
#94404 = ORIENTED_EDGE ( 'NONE', *, *, #17831, .T. ) ;
#94405 = FACE_OUTER_BOUND ( 'NONE', #41474, .T. ) ;
#94406 = ORIENTED_EDGE ( 'NONE', *, *, #105091, .F. ) ;
#94407 = ORIENTED_EDGE ( 'NONE', *, *, #91402, .T. ) ;
#94408 = CARTESIAN_POINT ( 'NONE',  ( -17.39901153685596924, -5.000000000000000888, 2.593512410382273536 ) ) ;
#94409 = CARTESIAN_POINT ( 'NONE',  ( -7.000000000000007105, -12.54465221550630716, 8.223849511754988129 ) ) ;
#94410 = SURFACE_STYLE_FILL_AREA ( #4857 ) ;
#94411 = ORIENTED_EDGE ( 'NONE', *, *, #17302, .F. ) ;
#94412 = DIRECTION ( 'NONE',  ( 0.000000000000000000, 0.000000000000000000, -1.000000000000000000 ) ) ;
#94413 = AXIS2_PLACEMENT_3D ( 'NONE', #19346, #58693, #75388 ) ;
#94414 = PRESENTATION_STYLE_ASSIGNMENT (( #77151 ) ) ;
#94415 = CARTESIAN_POINT ( 'NONE',  ( -94.70367724826090239, -57.65721615037961811, -8.919493359160306056 ) ) ;
#94416 = CARTESIAN_POINT ( 'NONE',  ( 7.213352437320217803, -12.01836473007682038, -3.463014597543478068 ) ) ;
#94417 = EDGE_CURVE ( 'NONE', #66540, #9203, #62376, .T. ) ;
#94418 = DIRECTION ( 'NONE',  ( -1.000000000000000000, -0.000000000000000000, -0.000000000000000000 ) ) ;
#94419 = CARTESIAN_POINT ( 'NONE',  ( 24.44497366060289067, 27.40106161504759896, 32.24452914909036849 ) ) ;
#94420 = FACE_OUTER_BOUND ( 'NONE', #59551, .T. ) ;
#94421 = CARTESIAN_POINT ( 'NONE',  ( 71.63670194497801447, -60.00000000000009948, -34.46961289685300045 ) ) ;
#94422 = EDGE_CURVE ( 'NONE', #98735, #75420, #84906, .T. ) ;
#94423 = CARTESIAN_POINT ( 'NONE',  ( -39.49898250731507687, -29.99999999999994316, 47.07929020003657428 ) ) ;
#94424 = CARTESIAN_POINT ( 'NONE',  ( -55.26582361395064424, -29.09120361102063157, 56.68308257653641391 ) ) ;
#94425 = MECHANICAL_DESIGN_GEOMETRIC_PRESENTATION_REPRESENTATION (  '', ( #73110 ), #65065 ) ;
#94426 = ORIENTED_EDGE ( 'NONE', *, *, #27705, .F. ) ;
#94427 = CARTESIAN_POINT ( 'NONE',  ( 6.925180474901644345, 16.86781820218113026, -1.053794444618463721 ) ) ;
#94428 = EDGE_LOOP ( 'NONE', ( #60364, #87667, #9078, #38050, #78984, #10202 ) ) ;
#94429 = CARTESIAN_POINT ( 'NONE',  ( -101.7716104940794537, -52.71911127419147647, 192.4179177423009151 ) ) ;
#94430 = CARTESIAN_POINT ( 'NONE',  ( 99.81081141497985243, -37.99999999999998579, 138.1205616140921961 ) ) ;
#94431 = CARTESIAN_POINT ( 'NONE',  ( 39.83349330513380693, -7.703719777548943412E-31, 4.000000000000001776 ) ) ;
#94432 = AXIS2_PLACEMENT_3D ( 'NONE', #90049, #97589, #31834 ) ;
#94433 = VERTEX_POINT ( 'NONE', #94198 ) ;
#94434 = CARTESIAN_POINT ( 'NONE',  ( 19.49140471140582775, 49.99885313499811446, 60.08881260961068449 ) ) ;
#94435 = PRESENTATION_STYLE_ASSIGNMENT (( #79287 ) ) ;
#94436 = DIRECTION ( 'NONE',  ( -1.000000000000000000, -1.224606353822377258E-16, -0.000000000000000000 ) ) ;
#94437 = CARTESIAN_POINT ( 'NONE',  ( 4.401442555609581635E-16, -17.65625000204838813, -7.188101187500000044 ) ) ;
#94438 = CARTESIAN_POINT ( 'NONE',  ( -3.504981525174552193, -68.37518638738055188, 13.08580713192159095 ) ) ;
#94440 = EDGE_CURVE ( 'NONE', #13812, #95088, #94747, .T. ) ;
#94439 = DIRECTION ( 'NONE',  ( -1.000000000000000000, -1.224606353822377258E-16, -0.000000000000000000 ) ) ;
#94441 = CARTESIAN_POINT ( 'NONE',  ( 7.800703710507056243, -81.41404307342060065, 1.791736796405269061 ) ) ;
#94442 = CARTESIAN_POINT ( 'NONE',  ( -40.73878142687892279, 503.7113041876743864, 10.19672445236252045 ) ) ;
#94443 = CARTESIAN_POINT ( 'NONE',  ( 22.91885868373643831, 305.6172567281201964, 10.10309701371861912 ) ) ;
#94444 = EDGE_CURVE ( 'NONE', #46291, #47279, #95229, .T. ) ;
#94445 = CARTESIAN_POINT ( 'NONE',  ( -8.725698932544442954, 131.8165386195289273, -2.602085213965210642E-15 ) ) ;
#94446 = CARTESIAN_POINT ( 'NONE',  ( 13.50000000000000355, -5.228219631169433335, -12.46710323223870809 ) ) ;
#94447 = CARTESIAN_POINT ( 'NONE',  ( -7.500000000000003553, 11.93422428098184263, -34.62196993281244062 ) ) ;
#94448 = UNCERTAINTY_MEASURE_WITH_UNIT (LENGTH_MEASURE( 1.000000000000000082E-05 ), #6802, 'distance_accuracy_value', 'NONE');
#94449 = CARTESIAN_POINT ( 'NONE',  ( -29.01219337864047532, -36.01131291592842842, 32.18479342621510852 ) ) ;
#94451 = EDGE_CURVE ( 'NONE', #50869, #70854, #78527, .T. ) ;
#94450 = AXIS2_PLACEMENT_3D ( 'NONE', #79370, #38927, #62676 ) ;
#94452 = CARTESIAN_POINT ( 'NONE',  ( 47.63708399370681690, -49.89836957298526698, 50.26224229957048095 ) ) ;
#94454 =( GEOMETRIC_REPRESENTATION_CONTEXT ( 3 ) GLOBAL_UNCERTAINTY_ASSIGNED_CONTEXT ( ( #85829 ) ) GLOBAL_UNIT_ASSIGNED_CONTEXT ( ( #18046, #42292, #34245 ) ) REPRESENTATION_CONTEXT ( 'NONE', 'WORKASPACE' ) );
#94453 = CARTESIAN_POINT ( 'NONE',  ( -1.099991320666667161, 45.96958673343657864, 16.88535858699162517 ) ) ;
#94455 = CARTESIAN_POINT ( 'NONE',  ( -89.60598034427661673, -38.52158010613944583, 200.4661439829993697 ) ) ;
#94456 = ORIENTED_EDGE ( 'NONE', *, *, #83081, .T. ) ;
#94457 = DIRECTION ( 'NONE',  ( 0.000000000000000000, -1.000000000000000000, 0.000000000000000000 ) ) ;
#94458 = CARTESIAN_POINT ( 'NONE',  ( 13.76261248551633010, 4.889473877509565192, -5.883208202484460081 ) ) ;
#94459 = CARTESIAN_POINT ( 'NONE',  ( -48.26727629737658987, 11.05468605157632744, -14.37283805632304912 ) ) ;
#94460 = CARTESIAN_POINT ( 'NONE',  ( 6.040020869836456363, 40.93519827235615338, -71.09856442099673757 ) ) ;
#94461 = CARTESIAN_POINT ( 'NONE',  ( -32.39696999578760028, 435.1504553356452334, 14.90852356088227459 ) ) ;
#94462 = DIRECTION ( 'NONE',  ( 0.000000000000000000, 0.000000000000000000, 1.000000000000000000 ) ) ;
#94463 = CIRCLE ( 'NONE', #42704, 0.9999999999999859002 ) ;
#94464 = CARTESIAN_POINT ( 'NONE',  ( 112.1444936845196594, -59.99999999999999289, 176.9640175347291233 ) ) ;
#94465 = CARTESIAN_POINT ( 'NONE',  ( -7.002641335706725201, -66.05087262680832794, 3.868676264653295949 ) ) ;
#94466 = EDGE_LOOP ( 'NONE', ( #84573, #52203 ) ) ;
#94467 = DIRECTION ( 'NONE',  ( -1.000000000000000000, -1.224606353822377258E-16, -0.000000000000000000 ) ) ;
#94468 = CARTESIAN_POINT ( 'NONE',  ( -80.42593251586281156, -30.00000000000000000, -13.16377588536598786 ) ) ;
#94469 = VERTEX_POINT ( 'NONE', #78008 ) ;
#94471 = CARTESIAN_POINT ( 'NONE',  ( 5.322129082409281509, 24.97845467789381857, -43.70420610338506151 ) ) ;
#94470 = CARTESIAN_POINT ( 'NONE',  ( -74.84880931779602520, -38.33446659060637529, 168.0768817207809036 ) ) ;
#94472 = CARTESIAN_POINT ( 'NONE',  ( 12.48545062700847019, -3.553405299047675658, -13.69229322019752537 ) ) ;
#94473 = DIRECTION ( 'NONE',  ( -1.000000000000000000, -1.224606353822377258E-16, -0.000000000000000000 ) ) ;
#94475 = CARTESIAN_POINT ( 'NONE',  ( 40.03012460245055593, 436.4820657380745956, 5.641945619390446254 ) ) ;
#94474 = STYLED_ITEM ( 'NONE', ( #55381 ), #27260 ) ;
#94476 = TOROIDAL_SURFACE ( 'NONE', #68608, 18.00000000000000355, 4.000000000000000000 ) ;
#94477 = CARTESIAN_POINT ( 'NONE',  ( 7.188101187500000044, -13.53125000204838457, 0.000000000000000000 ) ) ;
#94478 = CIRCLE ( 'NONE', #1427, 4.172000000000001485 ) ;
#94479 = CARTESIAN_POINT ( 'NONE',  ( -1.570796324976843295, -5.000000000000002665, -97.00000000000000000 ) ) ;
#94480 = AXIS2_PLACEMENT_3D ( 'NONE', #37847, #55555, #70177 ) ;
#94481 = EDGE_CURVE ( 'NONE', #64798, #48783, #34957, .T. ) ;
#94482 =( GEOMETRIC_REPRESENTATION_CONTEXT ( 3 ) GLOBAL_UNCERTAINTY_ASSIGNED_CONTEXT ( ( #14986 ) ) GLOBAL_UNIT_ASSIGNED_CONTEXT ( ( #40075, #82111, #16874 ) ) REPRESENTATION_CONTEXT ( 'NONE', 'WORKASPACE' ) );
#94483 = DIRECTION ( 'NONE',  ( 1.000000000000000000, 0.000000000000000000, 0.000000000000000000 ) ) ;
#94485 = ORIENTED_EDGE ( 'NONE', *, *, #106145, .T. ) ;
#94484 = SURFACE_SIDE_STYLE ('',( #11399 ) ) ;
#94486 = CARTESIAN_POINT ( 'NONE',  ( 81.53291621683337098, -53.45972034811280338, 178.0932871262222079 ) ) ;
#94487 = CARTESIAN_POINT ( 'NONE',  ( -44.09596412089000950, 463.0936910176846482, 6.209435503086969455 ) ) ;
#94488 = DIRECTION ( 'NONE',  ( 0.000000000000000000, -2.311253228826402606E-16, -1.000000000000000000 ) ) ;
#94489 = ORIENTED_EDGE ( 'NONE', *, *, #57976, .T. ) ;
#94490 = CARTESIAN_POINT ( 'NONE',  ( 4.898587196589412829E-16, 0.000000000000000000, 4.000000000000000000 ) ) ;
#94491 = CARTESIAN_POINT ( 'NONE',  ( 16.91579475168075319, 34.95500323700078837, 21.80698433968581185 ) ) ;
#94492 =( NAMED_UNIT ( * ) SI_UNIT ( $, .STERADIAN. ) SOLID_ANGLE_UNIT ( ) );
#94493 = DIRECTION ( 'NONE',  ( -0.000000000000000000, 1.000000000000000000, -0.000000000000000000 ) ) ;
#94494 = CARTESIAN_POINT ( 'NONE',  ( -29.68315524077005207, 13.12249633091091816, -39.60535821593474282 ) ) ;
#94495 = CARTESIAN_POINT ( 'NONE',  ( 1.160519905071935698, 17.00675097771450339, 50.01991939293108658 ) ) ;
#94496 = DIRECTION ( 'NONE',  ( -0.000000000000000000, 1.000000000000000000, -0.000000000000000000 ) ) ;
#94497 = ADVANCED_FACE ( 'NONE', ( #87174 ), #37810, .T. ) ;
#94498 = ORIENTED_EDGE ( 'NONE', *, *, #89783, .T. ) ;
#94499 = PRESENTATION_STYLE_ASSIGNMENT (( #102030 ) ) ;
#94500 = CONICAL_SURFACE ( 'NONE', #8384, 8.000000000000000000, 1.047197551196600296 ) ;
#94501 = CARTESIAN_POINT ( 'NONE',  ( -9.819056950928635175, 294.6481068335448299, 1.893705519456528652 ) ) ;
#94502 = CARTESIAN_POINT ( 'NONE',  ( 18.86650669486618881, 1.474610560812782335E-15, 0.000000000000000000 ) ) ;
#94503 = CARTESIAN_POINT ( 'NONE',  ( 14.82219693887339496, 22.90781324648665063, -1.994990707544676445 ) ) ;
#94506 = CIRCLE ( 'NONE', #75526, 4.000000000000007105 ) ;
#94505 = CARTESIAN_POINT ( 'NONE',  ( 0.000000000000000000, 0.000000000000000000, 0.000000000000000000 ) ) ;
#94504 = DIRECTION ( 'NONE',  ( 1.000000000000000000, 0.000000000000000000, -0.000000000000000000 ) ) ;
#94507 = AXIS2_PLACEMENT_3D ( 'NONE', #106489, #80620, #71470 ) ;
#94508 = CARTESIAN_POINT ( 'NONE',  ( 5.082755093536324154, -23.84375000204838457, 5.082755093536326818 ) ) ;
#94509 = CARTESIAN_POINT ( 'NONE',  ( 15.38309070169586690, 302.5568164900287229, -10.06270155509156083 ) ) ;
#94510 = DIRECTION ( 'NONE',  ( -0.5735764363510497121, 0.8191520442889892450, 1.003171929053521665E-16 ) ) ;
#94511 = EDGE_CURVE ( 'NONE', #18077, #13857, #76268, .T. ) ;
#94512 = CARTESIAN_POINT ( 'NONE',  ( 3.122594241928703163, -5.000000000000000888, -73.30485703407919118 ) ) ;
#94513 = CONTEXT_DEPENDENT_SHAPE_REPRESENTATION ( #30133, #19271 ) ;
#94514 = EDGE_LOOP ( 'NONE', ( #101103, #79324, #60478, #27987 ) ) ;
#94515 = CARTESIAN_POINT ( 'NONE',  ( 54.03872891708841308, 4.898587196589294500E-16, -4.000000000000007105 ) ) ;
#94516 = FACE_OUTER_BOUND ( 'NONE', #42506, .T. ) ;
#94517 = CARTESIAN_POINT ( 'NONE',  ( -7.883628181795526935, 62.00818940279086178, -4.999999999999999112 ) ) ;
#94518 = ADVANCED_FACE ( 'NONE', ( #56893 ), #102385, .F. ) ;
#94519 = CARTESIAN_POINT ( 'NONE',  ( -20.00000000000000000, 12.99999999999999289, -4.000000000000000000 ) ) ;
#94520 = ORIENTED_EDGE ( 'NONE', *, *, #49192, .F. ) ;
#94521 = PRESENTATION_LAYER_ASSIGNMENT (  '', '', ( #84110 ) ) ;
#94522 = CARTESIAN_POINT ( 'NONE',  ( 7.999999999999998224, -17.09374999999999289, 3.313708498984766049 ) ) ;
#94523 = FACE_OUTER_BOUND ( 'NONE', #65936, .T. ) ;
#94524 = ORIENTED_EDGE ( 'NONE', *, *, #21411, .T. ) ;
#94525 = CARTESIAN_POINT ( 'NONE',  ( -0.9999999999999943379, -1.409462824231155764E-15, 101.0455488498966758 ) ) ;
#94526 = CARTESIAN_POINT ( 'NONE',  ( 9.165151389911681434, 104.7368049370512040, 4.000000000000002665 ) ) ;
#94527 = CARTESIAN_POINT ( 'NONE',  ( -16.83431405849851359, 36.36677671467317197, 24.30698433968613870 ) ) ;
#94528 = UNCERTAINTY_MEASURE_WITH_UNIT (LENGTH_MEASURE( 1.000000000000000082E-05 ), #73383, 'distance_accuracy_value', 'NONE');
#94529 = CARTESIAN_POINT ( 'NONE',  ( -96.53420287613388950, -59.99999999999998579, 202.5374593177585325 ) ) ;
#94530 = CARTESIAN_POINT ( 'NONE',  ( 18.91781669292794987, 48.00000000000000000, 62.18610382930901892 ) ) ;
#94531 = FACE_OUTER_BOUND ( 'NONE', #80306, .T. ) ;
#94532 = CARTESIAN_POINT ( 'NONE',  ( 5.855955192086414129, 53.40184725084972683, -8.398893590963069755 ) ) ;
#94533 = CARTESIAN_POINT ( 'NONE',  ( 6.499999999999999112, -3.752776749732586126, -6.064240316920402663 ) ) ;
#94534 = CONICAL_SURFACE ( 'NONE', #18795, 5.000000000000001776, 0.9599310885968803664 ) ;
#94535 = CARTESIAN_POINT ( 'NONE',  ( -82.76397134495906016, -53.63233267313180619, 185.2452585357339103 ) ) ;
#94536 = EDGE_CURVE ( 'NONE', #9488, #14549, #86452, .T. ) ;
#94537 = CARTESIAN_POINT ( 'NONE',  ( 28.01586531120660339, 43.41400263758725231, -71.98455296551246363 ) ) ;
#94538 = ORIENTED_EDGE ( 'NONE', *, *, #80652, .F. ) ;
#94539 = CARTESIAN_POINT ( 'NONE',  ( -9.523267564283898423, 45.61198619316642322, -15.16070064068362200 ) ) ;
#94540 = CARTESIAN_POINT ( 'NONE',  ( 5.191144708981716427, -67.64030085521270053, 3.015512395308852067 ) ) ;
#94541 = CARTESIAN_POINT ( 'NONE',  ( -84.30425635789666217, -45.26998071672124979, -1.773480528068236417 ) ) ;
#94542 = CARTESIAN_POINT ( 'NONE',  ( 31.36650669486618881, 1.474610560812782335E-15, 0.000000000000000000 ) ) ;
#94543 = CARTESIAN_POINT ( 'NONE',  ( -3.151712658830499780, 111.9492514448680822, -4.999999999999998224 ) ) ;
#94544 = CARTESIAN_POINT ( 'NONE',  ( 8.020865862504424015, 104.2551619145339714, 0.000000000000000000 ) ) ;
#94545 = CARTESIAN_POINT ( 'NONE',  ( 36.87655955837850286, 437.4206410680705517, 3.315070609669402035 ) ) ;
#94546 = CARTESIAN_POINT ( 'NONE',  ( 51.76085035120648570, 42.00000000008225953, -29.83308852628573860 ) ) ;
#94547 = AXIS2_PLACEMENT_3D ( 'NONE', #25244, #58099, #99622 ) ;
#94548 = CARTESIAN_POINT ( 'NONE',  ( 78.42589391212746364, -14.21045842199428222, 185.4806485215488010 ) ) ;
#94549 = CARTESIAN_POINT ( 'NONE',  ( 0.000000000000000000, 152.0000000000000000, 0.000000000000000000 ) ) ;
#94550 = CARTESIAN_POINT ( 'NONE',  ( -94.33288967953484416, -60.00000000000004263, 18.12646456170910625 ) ) ;
#94551 = CARTESIAN_POINT ( 'NONE',  ( -65.58664656726918452, -25.57963682766552438, 80.66977220019482786 ) ) ;
#94552 = ORIENTED_EDGE ( 'NONE', *, *, #53118, .F. ) ;
#94553 = CARTESIAN_POINT ( 'NONE',  ( 105.0775402602081954, -59.99999999999994316, 202.2121962084956976 ) ) ;
#94554 = CARTESIAN_POINT ( 'NONE',  ( 64.91130259009537440, 39.42582562355791254, 6.834900822117297103 ) ) ;
#94555 = EDGE_LOOP ( 'NONE', ( #65465, #66109, #70133, #87169, #12999 ) ) ;
#94556 = CARTESIAN_POINT ( 'NONE',  ( 2.435348427764908250E-07, -57.67120202539301488, -44.61186700419774098 ) ) ;
#94557 = AXIS2_PLACEMENT_3D ( 'NONE', #99111, #106138, #24735 ) ;
#94558 = EDGE_LOOP ( 'NONE', ( #13496, #89080, #47395, #28287, #7698 ) ) ;
#94559 = CARTESIAN_POINT ( 'NONE',  ( 13.87268571384243465, -57.59061059622465706, 28.89968788215285755 ) ) ;
#94560 = CARTESIAN_POINT ( 'NONE',  ( -1.320432766682874540E-15, -27.40625000204838813, 7.188101187500000044 ) ) ;
#94561 = CARTESIAN_POINT ( 'NONE',  ( -6.000208918519487789, -5.999686622100329991, -0.2646532170642320048 ) ) ;
#94562 = VERTEX_POINT ( 'NONE', #40191 ) ;
#94563 = PRESENTATION_STYLE_ASSIGNMENT (( #27732 ) ) ;
#94564 = ORIENTED_EDGE ( 'NONE', *, *, #89855, .T. ) ;
#94565 = CARTESIAN_POINT ( 'NONE',  ( 91.95555555555554861, 1.023464760207051730E-14, 0.000000000000000000 ) ) ;
#94566 = PRESENTATION_STYLE_ASSIGNMENT (( #46518 ) ) ;
#94567 = CARTESIAN_POINT ( 'NONE',  ( -89.41502101575679262, -59.99999999999998579, -19.75460450551653224 ) ) ;
#94568 = DIRECTION ( 'NONE',  ( -1.000000000000000000, -1.224606353822377258E-16, -0.000000000000000000 ) ) ;
#94569 = CARTESIAN_POINT ( 'NONE',  ( -7.188101187500001821, -9.500000002048386349, -2.977408999572651371 ) ) ;
#94570 = CARTESIAN_POINT ( 'NONE',  ( 96.86866073052655679, -5.000000000000000000, 6.123233995736778115E-16 ) ) ;
#94571 = ADVANCED_FACE ( 'NONE', ( #32122 ), #106513, .F. ) ;
#94572 = CARTESIAN_POINT ( 'NONE',  ( -32.74728942619589844, 438.8764684952981838, 23.82517967440724149 ) ) ;
#94573 = CARTESIAN_POINT ( 'NONE',  ( 3.778364440264287083, -48.87981973393538482, 103.2432911248130978 ) ) ;
#94574 = CARTESIAN_POINT ( 'NONE',  ( -11.99999999999999467, 50.00000000000000000, -83.42920367502570400 ) ) ;
#94575 = EDGE_CURVE ( 'NONE', #102923, #29452, #29800, .T. ) ;
#94576 = CARTESIAN_POINT ( 'NONE',  ( -46.00000000000000711, 437.9213588505599546, 13.73447927187000595 ) ) ;
#94577 = SURFACE_STYLE_USAGE ( .BOTH. , #19653 ) ;
#94578 = CIRCLE ( 'NONE', #104957, 60.00000000000000000 ) ;
#94579 = ORIENTED_EDGE ( 'NONE', *, *, #78109, .T. ) ;
#94580 = LINE ( 'NONE', #91512, #40193 ) ;
#94581 = CARTESIAN_POINT ( 'NONE',  ( 4.031080902170319114, -1.378107924927665318, 103.0284855429829207 ) ) ;
#94583 = CARTESIAN_POINT ( 'NONE',  ( 33.88146361334444379, -25.63312173870950517, 32.08093021307823989 ) ) ;
#94582 = CARTESIAN_POINT ( 'NONE',  ( 4.071647195599044089, 52.05561507541640509, -6.990456272512426850 ) ) ;
#94584 = CARTESIAN_POINT ( 'NONE',  ( -12.70248734012553804, -4.285714285715715555, -22.03900363279001340 ) ) ;
#94585 = EDGE_CURVE ( 'NONE', #2579, #31239, #57310, .T. ) ;
#94586 = VERTEX_POINT ( 'NONE', #55305 ) ;
#94587 = CARTESIAN_POINT ( 'NONE',  ( 34.56726037194530221, 484.1545686971866189, -0.1516737162341373901 ) ) ;
#94588 = AXIS2_PLACEMENT_3D ( 'NONE', #91274, #93394, #34653 ) ;
#94589 = VECTOR ( 'NONE', #90246, 1000.000000000000000 ) ;
#94590 = CARTESIAN_POINT ( 'NONE',  ( -26.27902093981875709, 306.9027577142574614, -9.548073367147230428 ) ) ;
#94591 = DIRECTION ( 'NONE',  ( -0.000000000000000000, -1.000000000000000000, -0.000000000000000000 ) ) ;
#94592 = CARTESIAN_POINT ( 'NONE',  ( -43.69219460922278842, 484.4832989965429419, 2.442496667980163405 ) ) ;
#94593 = CARTESIAN_POINT ( 'NONE',  ( -41.92198544131502302, 435.4206365487660264, 7.395723383300994769 ) ) ;
#94594 = DIRECTION ( 'NONE',  ( 0.000000000000000000, -1.000000000000000000, 0.000000000000000000 ) ) ;
#94595 = CARTESIAN_POINT ( 'NONE',  ( 0.000000000000000000, 0.000000000000000000, 0.000000000000000000 ) ) ;
#94597 = ORIENTED_EDGE ( 'NONE', *, *, #39083, .T. ) ;
#94596 = AXIS2_PLACEMENT_3D ( 'NONE', #28935, #37544, #39110 ) ;
#94598 = CARTESIAN_POINT ( 'NONE',  ( 92.66631810923314561, -60.00000000000001421, -4.015254816811776983 ) ) ;
#94599 = DIRECTION ( 'NONE',  ( -0.000000000000000000, -1.000000000000000000, -0.000000000000000000 ) ) ;
#94600 = FACE_OUTER_BOUND ( 'NONE', #85810, .T. ) ;
#94601 = CARTESIAN_POINT ( 'NONE',  ( -5.273744844849142410, 41.55406142698797822, -70.69180546971138313 ) ) ;
#94602 = CARTESIAN_POINT ( 'NONE',  ( -11.48299332337337120, 12.76511049892793181, -10.00418054026044778 ) ) ;
#94603 = ORIENTED_EDGE ( 'NONE', *, *, #57748, .F. ) ;
#94604 = B_SPLINE_CURVE_WITH_KNOTS ( 'NONE', 3,
 ( #67698, #59076, #92487, #90911 ),
 .UNSPECIFIED., .F., .F.,
 ( 4, 4 ),
 ( 0.000000000000000000, 0.0006941752209892062099 ),
 .UNSPECIFIED. ) ;
#94605 = CARTESIAN_POINT ( 'NONE',  ( -102.6614301708703181, -29.99999999999975486, 197.7212064138423386 ) ) ;
#94606 = EDGE_LOOP ( 'NONE', ( #91401, #65839, #6693, #27797 ) ) ;
#94607 = LINE ( 'NONE', #87563, #88298 ) ;
#94608 = PRESENTATION_STYLE_ASSIGNMENT (( #102677 ) ) ;
#94609 = DIRECTION ( 'NONE',  ( -1.000000000000000000, -1.224606353822377258E-16, -0.000000000000000000 ) ) ;
#94610 = CARTESIAN_POINT ( 'NONE',  ( 83.97033530527313872, -52.73435016161096911, -15.30432209802549437 ) ) ;
#94611 = CARTESIAN_POINT ( 'NONE',  ( 5.082755093536324154, -31.71875000204838457, 5.082755093536326818 ) ) ;
#94612 = CARTESIAN_POINT ( 'NONE',  ( -17.99173077915196828, 34.45868671117904114, 22.69654071649677718 ) ) ;
#94613 = DIRECTION ( 'NONE',  ( 0.000000000000000000, 0.000000000000000000, -1.000000000000000000 ) ) ;
#94614 = CLOSED_SHELL ( 'NONE', ( #43456, #35760, #30500, #89412, #56842, #44745, #92497, #47980, #28237, #35548, #3016, #102332, #21921, #80589, #13356, #33339, #35984, #39510, #80222, #7796, #44377, #80143, #63507 ) ) ;
#94615 = DIRECTION ( 'NONE',  ( 0.7071067811865431318, 0.000000000000000000, -0.7071067811865517916 ) ) ;
#94616 = EDGE_LOOP ( 'NONE', ( #87915, #2088, #63777, #73861, #89000 ) ) ;
#94617 = ADVANCED_FACE ( 'NONE', ( #14312 ), #89439, .T. ) ;
#94618 = DIRECTION ( 'NONE',  ( 0.000000000000000000, 0.7863624351912762434, -0.6177654251575154243 ) ) ;
#94619 = STYLED_ITEM ( 'NONE', ( #85419 ), #12484 ) ;
#94621 = ORIENTED_EDGE ( 'NONE', *, *, #43207, .F. ) ;
#94620 = CARTESIAN_POINT ( 'NONE',  ( 0.000000000000000000, 0.000000000000000000, 0.000000000000000000 ) ) ;
#94622 = CARTESIAN_POINT ( 'NONE',  ( 79.26994885458404383, -32.55667777107090188, 134.6539744698178538 ) ) ;
#94623 = EDGE_CURVE ( 'NONE', #103960, #54493, #20627, .T. ) ;
#94624 = AXIS2_PLACEMENT_3D ( 'NONE', #50825, #42753, #28212 ) ;
#94625 = VERTEX_POINT ( 'NONE', #51318 ) ;
#94626 = CARTESIAN_POINT ( 'NONE',  ( 2.423637387739231652, -49.74034360832548884, 44.58576659056175373 ) ) ;
#94627 = CARTESIAN_POINT ( 'NONE',  ( 7.188101187500000044, -20.65625000204838813, 0.000000000000000000 ) ) ;
#94628 =( BOUNDED_SURFACE ( )  B_SPLINE_SURFACE ( 3, 2, ( 
 ( #23710, #62563, #95449 ),
 ( #87373, #104593, #79263 ),
 ( #14504, #47416, #6419 ),
 ( #39357, #72234, #105137 ),
 ( #75416, #50076, #92127 ),
 ( #40926, #32863, #73819 ),
 ( #18275, #1509, #41983 ),
 ( #48997, #74865, #51130 ),
 ( #955, #74345, #99149 ),
 ( #8552, #32333, #33935 ),
 ( #57616, #98619, #90544 ),
 ( #66804, #24247, #16652 ),
 ( #17200, #84047, #100222 ),
 ( #25308, #67344, #10149 ),
 ( #82982, #99692, #26390 ),
 ( #422, #59252, #50587 ),
 ( #43064, #82448, #33388 ),
 ( #91620, #106171, #34474 ),
 ( #65739, #41454, #24769 ),
 ( #49542, #98096, #65201 ),
 ( #66262, #8017, #9079 ),
 ( #90010, #42517, #57094 ),
 ( #58719, #16113, #58166 ),
 ( #81899, #106712, #91094 ),
 ( #17729, #25864, #83503 ),
 ( #9604, #69991, #43587 ),
 ( #3130, #75950, #67863 ),
 ( #102893, #100748, #11729 ),
 ( #53797, #2051, #84588 ),
 ( #29056, #94274, #26914 ),
 ( #34997, #53279, #61926 ),
 ( #59789, #92665, #18824 ),
 ( #77553, #68408, #86725 ),
 ( #36604, #51666, #78079 ),
 ( #11195, #10669, #76471 ),
 ( #2583, #60851, #45203 ),
 ( #94816, #93203, #69468 ),
 ( #93738, #20963, #35533 ),
 ( #44130, #44668, #27450 ),
 ( #101301, #3670, #37127 ),
 ( #52735, #85110, #60330 ),
 ( #4193, #102352, #19368 ),
 ( #28499, #12798, #52199 ),
 ( #77013, #36074, #68945 ),
 ( #61385, #20439, #101818 ),
 ( #27983, #86199, #12272 ),
 ( #19894, #85659, #31676 ),
 ( #13858, #87777, #88307 ),
 ( #5777, #46249, #47289 ),
 ( #87248, #79136, #13326 ),
 ( #64558, #47812, #14384 ),
 ( #72632, #71047, #105534 ),
 ( #80188, #46771, #38699 ),
 ( #54848, #78597, #6293 ) ),
 .UNSPECIFIED., .F., .F., .T. ) 
 B_SPLINE_SURFACE_WITH_KNOTS ( ( 4, 2, 2, 2, 2, 2, 2, 2, 2, 2, 2, 2, 2, 2, 2, 2, 2, 2, 2, 2, 2, 2, 2, 2, 2, 2, 4 ),
 ( 3, 3 ),
 ( 0.04676915544590774798, 0.05566498745926091313, 0.06456081947261407827, 0.08235248349932039469, 0.1001441475260267250, 0.1179358115527330553, 0.1357274755794393717, 0.1446233075927925438, 0.1535191396061457159, 0.1579670556128223158, 0.1624149716194988879, 0.1668628876261754601, 0.1713108036328520600, 0.1757587196395286322, 0.1779826776428669044, 0.1802066356462052044, 0.1813186146478743543, 0.1824305936495435043, 0.1829865831503780793, 0.1835425726512126543, 0.1846545516528818043, 0.1852105411537163793, 0.1857665306545509543, 0.1863225201553855293, 0.1868785096562201042, 0.1879904886578892542, 0.1891024676595583764 ),
 ( 0.000000000000000000, 1.000000000000000000 ),
 .UNSPECIFIED. ) 
 GEOMETRIC_REPRESENTATION_ITEM ( )  RATIONAL_B_SPLINE_SURFACE ( (
 ( 1.000000000000000000, 0.7071068714016401913, 1.000000000000000000),
 ( 1.000000000000000000, 0.7071068931780433164, 1.000000000000000000),
 ( 1.000000000000000000, 0.7071068799845713349, 1.000000000000000000),
 ( 1.000000000000000000, 0.7071068180475085230, 1.000000000000000000),
 ( 1.000000000000000000, 0.7071067808201265681, 1.000000000000000000),
 ( 1.000000000000000000, 0.7071067808201265681, 1.000000000000000000),
 ( 1.000000000000000000, 0.7071067795786223353, 1.000000000000000000),
 ( 1.000000000000000000, 0.7071067795786223353, 1.000000000000000000),
 ( 1.000000000000000000, 0.7071059182714053426, 1.000000000000000000),
 ( 1.000000000000000000, 0.7071040218720007209, 1.000000000000000000),
 ( 1.000000000000000000, 0.7071071124652589246, 1.000000000000000000),
 ( 1.000000000000000000, 0.7071064137913863901, 1.000000000000000000),
 ( 1.000000000000000000, 0.7071032629227845812, 1.000000000000000000),
 ( 1.000000000000000000, 0.7071054820452861156, 1.000000000000000000),
 ( 1.000000000000000000, 0.7071073498263017454, 1.000000000000000000),
 ( 1.000000000000000000, 0.7071060860965120431, 1.000000000000000000),
 ( 1.000000000000000000, 0.7071042701190503044, 1.000000000000000000),
 ( 1.000000000000000000, 0.7071061861960223904, 1.000000000000000000),
 ( 1.000000000000000000, 0.7071092265142245870, 1.000000000000000000),
 ( 1.000000000000000000, 0.7071028837941631950, 1.000000000000000000),
 ( 1.000000000000000000, 0.7070914420358777042, 1.000000000000000000),
 ( 1.000000000000000000, 0.7070821610321850192, 1.000000000000000000),
 ( 1.000000000000000000, 0.7070849129775590436, 1.000000000000000000),
 ( 1.000000000000000000, 0.7071004802399988298, 1.000000000000000000),
 ( 1.000000000000000000, 0.7071085105257672865, 1.000000000000000000),
 ( 1.000000000000000000, 0.7071013087433613009, 1.000000000000000000),
 ( 1.000000000000000000, 0.7071049945832310613, 1.000000000000000000),
 ( 1.000000000000000000, 0.7071073724018395179, 1.000000000000000000),
 ( 1.000000000000000000, 0.7070679728041205925, 1.000000000000000000),
 ( 1.000000000000000000, 0.7070088173080720795, 1.000000000000000000),
 ( 1.000000000000000000, 0.7070194258748161431, 1.000000000000000000),
 ( 1.000000000000000000, 0.7070840790032983936, 1.000000000000000000),
 ( 1.000000000000000000, 0.7071075161209789961, 1.000000000000000000),
 ( 1.000000000000000000, 0.7071058500867670737, 1.000000000000000000),
 ( 1.000000000000000000, 0.7071008551465617353, 1.000000000000000000),
 ( 1.000000000000000000, 0.7071023055844545269, 1.000000000000000000),
 ( 1.000000000000000000, 0.7071042320260993996, 1.000000000000000000),
 ( 1.000000000000000000, 0.7071072094748438452, 1.000000000000000000),
 ( 1.000000000000000000, 0.7071072778665237202, 1.000000000000000000),
 ( 1.000000000000000000, 0.7071144736285724930, 1.000000000000000000),
 ( 1.000000000000000000, 0.7071122659468992433, 1.000000000000000000),
 ( 1.000000000000000000, 0.7071060123279735432, 1.000000000000000000),
 ( 1.000000000000000000, 0.7071046393532877117, 1.000000000000000000),
 ( 1.000000000000000000, 0.7070933101913624563, 1.000000000000000000),
 ( 1.000000000000000000, 0.7070896596052901328, 1.000000000000000000),
 ( 1.000000000000000000, 0.7070919439014947683, 1.000000000000000000),
 ( 1.000000000000000000, 0.7070971265612475687, 1.000000000000000000),
 ( 1.000000000000000000, 0.7071056421788293189, 1.000000000000000000),
 ( 1.000000000000000000, 0.7071090411609283199, 1.000000000000000000),
 ( 1.000000000000000000, 0.7070957058651622384, 1.000000000000000000),
 ( 1.000000000000000000, 0.7070787487242025104, 1.000000000000000000),
 ( 1.000000000000000000, 0.7070875582157836181, 1.000000000000000000),
 ( 1.000000000000000000, 0.7071060045247833381, 1.000000000000000000),
 ( 1.000000000000000000, 0.7071067811865683339, 1.000000000000000000) ) ) 
 REPRESENTATION_ITEM ( '' )  SURFACE ( )  );
#94629 = CARTESIAN_POINT ( 'NONE',  ( -70.79351044798765713, -57.68242073007258597, 160.4532249112098157 ) ) ;
#94630 = EDGE_CURVE ( 'NONE', #57770, #11179, #53467, .T. ) ;
#94631 = ORIENTED_EDGE ( 'NONE', *, *, #66217, .T. ) ;
#94632 = SURFACE_STYLE_FILL_AREA ( #61190 ) ;
#94633 = CARTESIAN_POINT ( 'NONE',  ( -5.382057749264597568, -12.99826798403944572, -2.659775980967104658 ) ) ;
#94634 = CARTESIAN_POINT ( 'NONE',  ( 7.043654982242377294, 41.66078771780808410, -59.26734080171946317 ) ) ;
#94635 = CARTESIAN_POINT ( 'NONE',  ( 0.000000000000000000, 0.000000000000000000, -4.425378966781146950 ) ) ;
#94636 = CARTESIAN_POINT ( 'NONE',  ( 8.000000000000000000, -18.59375000409677270, -3.313708498984761608 ) ) ;
#94637 = CARTESIAN_POINT ( 'NONE',  ( -52.01488423272231643, -29.95943715781152505, 50.12585609927782571 ) ) ;
#94638 = VECTOR ( 'NONE', #74582, 1000.000000000000000 ) ;
#94639 = CARTESIAN_POINT ( 'NONE',  ( 9.403185743875125624, 15.24615751665866981, 3.409011323177099317 ) ) ;
#94640 = PRESENTATION_LAYER_ASSIGNMENT (  '', '', ( #1579 ) ) ;
#94641 = CARTESIAN_POINT ( 'NONE',  ( -46.00000000000003553, 486.4340384878602208, 3.748479173867791392 ) ) ;
#94642 = B_SPLINE_CURVE_WITH_KNOTS ( 'NONE', 3,
 ( #10294, #101446, #60481, #43206, #71704, #79812, #38841, #46394, #70141, #78225, #22674, #86869, #5914, #103045, #104619, #45347, #79284, #103563, #55512, #29201, #53431, #6441, #53936, #38328, #80327, #30768, #62076, #54989, #104084, #71189 ),
 .UNSPECIFIED., .F., .F.,
 ( 4, 2, 2, 2, 2, 2, 2, 2, 2, 2, 2, 2, 2, 2, 4 ),
 ( 0.01423689679755360885, 0.01470129771271631511, 0.01493349817029766477, 0.01516569862787901443, 0.01539789908546036236, 0.01563009954304171029, 0.01586230000062305995, 0.01609450045820440961, 0.01655890137336709506, 0.01702330228852978050, 0.01795210411885515486, 0.01888090594918052922, 0.01980970777950590705, 0.02073850960983128142, 0.02166731144015665578 ),
 .UNSPECIFIED. ) ;
#94643 = CARTESIAN_POINT ( 'NONE',  ( -0.9999999999999943379, -50.00000000000000000, 101.0455488498966758 ) ) ;
#94644 = CARTESIAN_POINT ( 'NONE',  ( 4.080274524171334072, 51.84966241523257224, 7.633405385586866210 ) ) ;
#94645 = DIRECTION ( 'NONE',  ( 2.775557561562890118E-17, 0.9999380666134188855, 0.01112937273244818219 ) ) ;
#94646 = CARTESIAN_POINT ( 'NONE',  ( -46.00000000000000000, 500.0000000000002274, 0.000000000000000000 ) ) ;
#94647 = ORIENTED_EDGE ( 'NONE', *, *, #93339, .T. ) ;
#94648 = CARTESIAN_POINT ( 'NONE',  ( -4.464818165989834498, -48.01567804769277359, 43.16242680068418736 ) ) ;
#94649 = CARTESIAN_POINT ( 'NONE',  ( 11.09711298024378046, -4.982652786778980492, -12.57750780562587423 ) ) ;
#94650 = CARTESIAN_POINT ( 'NONE',  ( -3.972507935376086596, 17.31478156112088485, -5.763960839875241327 ) ) ;
#94651 = CARTESIAN_POINT ( 'NONE',  ( -33.19001599143121695, -22.73732675021535954, -31.63514692089995606 ) ) ;
#94652 = CARTESIAN_POINT ( 'NONE',  ( -66.43834448911053414, -30.00000000000000000, 84.40165359335730955 ) ) ;
#94653 = ADVANCED_FACE ( 'NONE', ( #78264 ), #84769, .F. ) ;
#94654 = FACE_OUTER_BOUND ( 'NONE', #34643, .T. ) ;
#94655 = VERTEX_POINT ( 'NONE', #68602 ) ;
#94656 = CARTESIAN_POINT ( 'NONE',  ( -17.82150094935625972, -4.333298119783937530, -1.872127852610514731 ) ) ;
#94657 = CARTESIAN_POINT ( 'NONE',  ( 78.25717990118528178, -57.50986624554720805, 196.9151558317045385 ) ) ;
#94658 = FACE_OUTER_BOUND ( 'NONE', #65282, .T. ) ;
#94659 = EDGE_CURVE ( 'NONE', #25863, #101939, #45265, .T. ) ;
#94660 = MECHANICAL_DESIGN_GEOMETRIC_PRESENTATION_REPRESENTATION (  '', ( #51589 ), #80829 ) ;
#94661 = LINE ( 'NONE', #95699, #646 ) ;
#94662 = SURFACE_SIDE_STYLE ('',( #102193 ) ) ;
#94663 = CARTESIAN_POINT ( 'NONE',  ( -53.46014380037404834, -59.99999999999999289, 80.92137724076353322 ) ) ;
#94664 = EDGE_CURVE ( 'NONE', #79700, #60134, #33724, .T. ) ;
#94665 = CARTESIAN_POINT ( 'NONE',  ( -6.725979247667767780, 3.622307570260298704, -6.470294263593356909 ) ) ;
#94666 = FACE_OUTER_BOUND ( 'NONE', #67534, .T. ) ;
#94667 = CIRCLE ( 'NONE', #48123, 4.000000000000000888 ) ;
#94668 = CARTESIAN_POINT ( 'NONE',  ( 63.03617022297318329, 49.99999999997997691, -16.93907820452584545 ) ) ;
#94669 = CARTESIAN_POINT ( 'NONE',  ( -86.39277916084785147, -17.36997147719805668, 179.6821819924676333 ) ) ;
#94670 = ORIENTED_EDGE ( 'NONE', *, *, #47989, .F. ) ;
#94671 = CARTESIAN_POINT ( 'NONE',  ( 33.48975799666246900, 326.8007346975397240, -3.612220824777813810 ) ) ;
#94672 = CARTESIAN_POINT ( 'NONE',  ( -5.156364120415605434, -56.88410093696714398, 33.35976719709237415 ) ) ;
#94673 = CARTESIAN_POINT ( 'NONE',  ( -5.469234196618169896, 41.99717955803384939, -59.59612311059226641 ) ) ;
#94674 = FACE_BOUND ( 'NONE', #97702, .T. ) ;
#94675 = CARTESIAN_POINT ( 'NONE',  ( 34.42407431220851066, 1.340359594676612611E-15, 0.000000000000000000 ) ) ;
#94676 = CARTESIAN_POINT ( 'NONE',  ( 39.19091519714796590, 489.8676313716377990, 11.78787226601978944 ) ) ;
#94677 = VECTOR ( 'NONE', #44203, 1000.000000000000000 ) ;
#94678 = DIRECTION ( 'NONE',  ( 0.000000000000000000, 0.000000000000000000, -1.000000000000000000 ) ) ;
#94679 = DIRECTION ( 'NONE',  ( 0.000000000000000000, 1.000000000000000000, 0.000000000000000000 ) ) ;
#94680 = ORIENTED_EDGE ( 'NONE', *, *, #5600, .T. ) ;
#94681 = CARTESIAN_POINT ( 'NONE',  ( 18.48567378316023735, 49.99999999999999289, 61.27610688997057053 ) ) ;
#94682 = CARTESIAN_POINT ( 'NONE',  ( 13.28477689701638731, 24.21911917246261226, 3.176269128160213118 ) ) ;
#94683 = CARTESIAN_POINT ( 'NONE',  ( -22.03900363279597840, -4.285714285713229543, -12.70248734010661451 ) ) ;
#94684 = SURFACE_SIDE_STYLE ('',( #86064 ) ) ;
#94685 = CIRCLE ( 'NONE', #50071, 7.000000000000000000 ) ;
#94686 = CARTESIAN_POINT ( 'NONE',  ( 101.2959083255158390, -29.99999999999995026, 104.2725399938968707 ) ) ;
#94687 = CARTESIAN_POINT ( 'NONE',  ( -82.56867337363084403, -18.68741499447245502, 139.1104154598086495 ) ) ;
#94688 = ORIENTED_EDGE ( 'NONE', *, *, #39752, .T. ) ;
#94689 = CARTESIAN_POINT ( 'NONE',  ( 42.88788165728912105, 484.9809715184047150, -1.409177641729580932 ) ) ;
#94690 = CARTESIAN_POINT ( 'NONE',  ( 27.61650669486618881, 1.474610560812782335E-15, 0.000000000000000000 ) ) ;
#94691 = CARTESIAN_POINT ( 'NONE',  ( 40.58563001615174670, -57.69103653720686253, 56.61367073664153793 ) ) ;
#94692 = CARTESIAN_POINT ( 'NONE',  ( 37.60572600703760315, 371.3193617627527487, 4.346622703349591887 ) ) ;
#94693 = AXIS2_PLACEMENT_3D ( 'NONE', #10654, #45188, #43572 ) ;
#94694 = CARTESIAN_POINT ( 'NONE',  ( 0.000000000000000000, 0.000000000000000000, 0.000000000000000000 ) ) ;
#94695 = VERTEX_POINT ( 'NONE', #80909 ) ;
#94696 = CARTESIAN_POINT ( 'NONE',  ( -7.093721425956736049, 304.7303285792975771, 9.911179277710184365 ) ) ;
#94697 = CARTESIAN_POINT ( 'NONE',  ( 24.83349330513380693, 1.593028355512270962E-15, 0.000000000000000000 ) ) ;
#94698 = CARTESIAN_POINT ( 'NONE',  ( 2.977408999572650927, -23.37500000204838813, -7.188101187500001821 ) ) ;
#94699 = ORIENTED_EDGE ( 'NONE', *, *, #40415, .F. ) ;
#94700 = CARTESIAN_POINT ( 'NONE',  ( 44.24885999147007709, 485.2873706794222812, 1.656249348736088312 ) ) ;
#94701 = FACE_OUTER_BOUND ( 'NONE', #45845, .T. ) ;
#94702 = CARTESIAN_POINT ( 'NONE',  ( 5.385153946026782990, 41.85687303129803638, -70.29203007274306003 ) ) ;
#94703 = ADVANCED_FACE ( 'NONE', ( #31345 ), #460, .T. ) ;
#94704 = CARTESIAN_POINT ( 'NONE',  ( 0.01688885742776976423, -7.321065037175430668, -3.319543390096034052 ) ) ;
#94705 = DIRECTION ( 'NONE',  ( 0.000000000000000000, 0.000000000000000000, 1.000000000000000000 ) ) ;
#94706 = DIRECTION ( 'NONE',  ( -1.000000000000000000, -0.000000000000000000, -0.000000000000000000 ) ) ;
#94707 = ORIENTED_EDGE ( 'NONE', *, *, #86814, .F. ) ;
#94708 = CARTESIAN_POINT ( 'NONE',  ( 86.68221780050056680, -59.99999999999997868, -23.04089234932559549 ) ) ;
#94710 = CARTESIAN_POINT ( 'NONE',  ( 26.29730120201151067, -29.04676451314565711, 30.24640415352105549 ) ) ;
#94709 = CARTESIAN_POINT ( 'NONE',  ( -69.35428882245668092, -14.21045842199431064, 113.5922931172439263 ) ) ;
#94711 = PRESENTATION_LAYER_ASSIGNMENT (  '', '', ( #48159 ) ) ;
#94712 = CARTESIAN_POINT ( 'NONE',  ( 1.347636720419746323E-14, 17.51648154115788714, -55.02144460582525909 ) ) ;
#94713 = EDGE_CURVE ( 'NONE', #70179, #44397, #74746, .T. ) ;
#94714 = VERTEX_POINT ( 'NONE', #78784 ) ;
#94715 = UNCERTAINTY_MEASURE_WITH_UNIT (LENGTH_MEASURE( 1.000000000000000082E-05 ), #38904, 'distance_accuracy_value', 'NONE');
#94716 = EDGE_LOOP ( 'NONE', ( #81677, #42455, #94211, #1912, #53234 ) ) ;
#94717 = CARTESIAN_POINT ( 'NONE',  ( -24.41571844174603001, -4.285714285714296246, -6.539732759932831208 ) ) ;
#94718 = CARTESIAN_POINT ( 'NONE',  ( -13.99656100229485389, -57.97463508733147819, 26.59581618167199579 ) ) ;
#94719 =( GEOMETRIC_REPRESENTATION_CONTEXT ( 3 ) GLOBAL_UNCERTAINTY_ASSIGNED_CONTEXT ( ( #983 ) ) GLOBAL_UNIT_ASSIGNED_CONTEXT ( ( #44724, #94874, #37724 ) ) REPRESENTATION_CONTEXT ( 'NONE', 'WORKASPACE' ) );
#94720 = CARTESIAN_POINT ( 'NONE',  ( 9.757377548409222196E-14, 52.17923068443732149, -7.749999999998994582 ) ) ;
#94721 = DIRECTION ( 'NONE',  ( -0.5735764363510512664, 0.8191520442889881348, 1.003171929053520309E-16 ) ) ;
#94722 = CARTESIAN_POINT ( 'NONE',  ( 0.06682554136338200723, -6.264794173742283867, -2.149058192116893196 ) ) ;
#94723 = ORIENTED_EDGE ( 'NONE', *, *, #36163, .T. ) ;
#94724 = CARTESIAN_POINT ( 'NONE',  ( -54.49732025174689909, -38.34336403967661511, 80.08277365667782988 ) ) ;
#94725 = DIRECTION ( 'NONE',  ( 1.000000000000000000, 0.000000000000000000, 0.000000000000000000 ) ) ;
#94726 = CARTESIAN_POINT ( 'NONE',  ( 100.1751865587538646, -29.99999999999997868, 184.8388631958245583 ) ) ;
#94727 = CARTESIAN_POINT ( 'NONE',  ( -11.09178706276765247, 8.457831532506155270, -9.831605721811831344 ) ) ;
#94728 = DIRECTION ( 'NONE',  ( -1.000000000000000000, -1.224606353822377258E-16, -0.000000000000000000 ) ) ;
#94729 = CARTESIAN_POINT ( 'NONE',  ( 81.33861762675972784, -30.00000000000000711, -1.059591593001759868 ) ) ;
#94730 = CARTESIAN_POINT ( 'NONE',  ( 6.249999999999998224, 4.618802153517004960, 7.999999999999998224 ) ) ;
#94731 = ORIENTED_EDGE ( 'NONE', *, *, #54250, .T. ) ;
#94732 = ADVANCED_FACE ( 'NONE', ( #38881 ), #102142, .T. ) ;
#94733 = ORIENTED_EDGE ( 'NONE', *, *, #105654, .T. ) ;
#94734 = ORIENTED_EDGE ( 'NONE', *, *, #39252, .F. ) ;
#94735 = CARTESIAN_POINT ( 'NONE',  ( 14.54015256618498775, 9.738273119607207207, 0.000000000000000000 ) ) ;
#94736 = DIRECTION ( 'NONE',  ( 0.000000000000000000, -1.000000000000000000, 0.000000000000000000 ) ) ;
#94737 = FACE_OUTER_BOUND ( 'NONE', #49042, .T. ) ;
#94738 = CARTESIAN_POINT ( 'NONE',  ( -37.68817371937168303, 414.9405981843138989, 6.370433777595585489 ) ) ;
#94739 = CARTESIAN_POINT ( 'NONE',  ( -7.343637806710343163, -87.44363121900614999, 3.177475076494674866 ) ) ;
#94740 = CARTESIAN_POINT ( 'NONE',  ( 64.78349330513380266, 6.975173280561618775E-15, 0.000000000000000000 ) ) ;
#94742 = VERTEX_POINT ( 'NONE', #13514 ) ;
#94741 = CIRCLE ( 'NONE', #8536, 3.309500000000001663 ) ;
#94743 = CARTESIAN_POINT ( 'NONE',  ( 6.145467200821944864, 49.99999999999999289, -77.00333157708759302 ) ) ;
#94744 = ORIENTED_EDGE ( 'NONE', *, *, #81838, .F. ) ;
#94745 = EDGE_CURVE ( 'NONE', #60803, #50381, #50387, .T. ) ;
#94746 = CARTESIAN_POINT ( 'NONE',  ( 0.000000000000000000, 15.00000000000000000, -10.00000000000000000 ) ) ;
#94747 = LINE ( 'NONE', #28428, #14278 ) ;
#94748 = CARTESIAN_POINT ( 'NONE',  ( 24.36021057821819724, 304.1488456854494302, 10.22118185489211939 ) ) ;
#94749 = B_SPLINE_CURVE_WITH_KNOTS ( 'NONE', 3,
 ( #50070, #9073, #16108, #49536, #82444, #17722, #6952, #48993, #81894, #50582, #8545, #33383, #25303, #97542, #105646, #31786, #73813, #17196, #48469, #82978, #40386, #106707, #106165, #32325, #99143, #41977, #94268, #11190 ),
 .UNSPECIFIED., .F., .F.,
 ( 4, 2, 2, 2, 2, 2, 2, 2, 2, 2, 2, 2, 2, 4 ),
 ( 0.002626378601955878331, 0.003560090090687870537, 0.004493801579419862309, 0.005427513068151854081, 0.006361224556883846720, 0.006828080301249843040, 0.007061508173432842067, 0.007294936045615841094, 0.007528363917798841856, 0.007761791789981840883, 0.008228647534347842407, 0.008695503278713843931, 0.009162359023079845455, 0.01009607051181185544 ),
 .UNSPECIFIED. ) ;
#94750 = CARTESIAN_POINT ( 'NONE',  ( 1.954498338103932698, 298.2604654188854170, -10.00252163445081521 ) ) ;
#94751 = CARTESIAN_POINT ( 'NONE',  ( 65.34791356701451548, -18.62574154944152838, 76.43348303465126037 ) ) ;
#94752 = ORIENTED_EDGE ( 'NONE', *, *, #90517, .F. ) ;
#94753 = CARTESIAN_POINT ( 'NONE',  ( 29.09616027395232507, 9.373446874598327483, -41.96755440745717181 ) ) ;
#94754 = CARTESIAN_POINT ( 'NONE',  ( -52.11024624342783795, -36.01363760906497902, -35.80679646664415117 ) ) ;
#94755 = DIRECTION ( 'NONE',  ( 1.000000000000000000, 1.224606353822377258E-16, 0.000000000000000000 ) ) ;
#94756 = AXIS2_PLACEMENT_3D ( 'NONE', #46796, #73168, #21489 ) ;
#94757 = DIRECTION ( 'NONE',  ( -1.000000000000000000, -0.000000000000000000, -0.000000000000000000 ) ) ;
#94758 = EDGE_CURVE ( 'NONE', #5324, #76499, #25926, .T. ) ;
#94759 = ORIENTED_EDGE ( 'NONE', *, *, #55753, .T. ) ;
#94760 = AXIS2_PLACEMENT_3D ( 'NONE', #2933, #103238, #101647 ) ;
#94761 =( NAMED_UNIT ( * ) PLANE_ANGLE_UNIT ( ) SI_UNIT ( $, .RADIAN. ) );
#94762 = DIRECTION ( 'NONE',  ( -1.000000000000000000, -1.224606353822377258E-16, -0.000000000000000000 ) ) ;
#94763 = FACE_OUTER_BOUND ( 'NONE', #8723, .T. ) ;
#94764 = DIRECTION ( 'NONE',  ( 0.000000000000000000, 1.000000000000000000, 0.000000000000000000 ) ) ;
#94765 = CIRCLE ( 'NONE', #82653, 3.309500000000001663 ) ;
#94766 = DIRECTION ( 'NONE',  ( -1.000000000000000000, 0.000000000000000000, 0.000000000000000000 ) ) ;
#94767 = CARTESIAN_POINT ( 'NONE',  ( 29.66054107240687543, 3.851859888774471706E-31, 5.000000000000001776 ) ) ;
#94768 = CARTESIAN_POINT ( 'NONE',  ( 85.99512895147944391, -46.52335532650928940, 189.5191995827347284 ) ) ;
#94769 = CARTESIAN_POINT ( 'NONE',  ( -5.293182415613770786, 18.41909107384472932, -37.79627497856930773 ) ) ;
#94770 = AXIS2_PLACEMENT_3D ( 'NONE', #5636, #45586, #13183 ) ;
#94771 = CARTESIAN_POINT ( 'NONE',  ( -5.838394382201822275, 4.727980164709353339, 5.000000000000000888 ) ) ;
#94772 = VERTEX_POINT ( 'NONE', #9137 ) ;
#94773 = CARTESIAN_POINT ( 'NONE',  ( -7.922281120364393914, 4.573931137438267847, -8.047472243342932430 ) ) ;
#94774 = CARTESIAN_POINT ( 'NONE',  ( -17.80527173634003191, -17.90131026958873406, -34.03118370072504462 ) ) ;
#94775 = CARTESIAN_POINT ( 'NONE',  ( 8.099999999999999645, 7.505553499465140277, 0.000000000000000000 ) ) ;
#94776 = CARTESIAN_POINT ( 'NONE',  ( -6.757705282517541434, 41.35007050579768162, -70.67351639275690900 ) ) ;
#94777 = CARTESIAN_POINT ( 'NONE',  ( 33.92709525147886751, 435.0559456452658651, 11.89085117398060021 ) ) ;
#94778 = CARTESIAN_POINT ( 'NONE',  ( -100.7719193891408338, -30.00000000000000000, 180.5683480488255270 ) ) ;
#94779 = EDGE_CURVE ( 'NONE', #55395, #35042, #100355, .T. ) ;
#94780 = B_SPLINE_CURVE_WITH_KNOTS ( 'NONE', 3,
 ( #77074, #28559, #29625, #53337, #30681, #3731, #13915, #63568, #78133, #12330 ),
 .UNSPECIFIED., .F., .F.,
 ( 4, 2, 2, 2, 4 ),
 ( 0.000000000000000000, 0.001118707926289529489, 0.002237415852579058978, 0.003356123778868585431, 0.004474831705158112752 ),
 .UNSPECIFIED. ) ;
#94781 = DIRECTION ( 'NONE',  ( -0.000000000000000000, -0.000000000000000000, 1.000000000000000000 ) ) ;
#94782 = CARTESIAN_POINT ( 'NONE',  ( 28.28340439371653048, -57.67994101532651285, 44.40698028540107600 ) ) ;
#94783 = VECTOR ( 'NONE', #66485, 1000.000000000000000 ) ;
#94785 = CARTESIAN_POINT ( 'NONE',  ( 0.000000000000000000, 304.8518027762758038, 9.936999415352289589 ) ) ;
#94784 = DIRECTION ( 'NONE',  ( 0.000000000000000000, -1.000000000000000000, 0.000000000000000000 ) ) ;
#94786 = EDGE_CURVE ( 'NONE', #26788, #12195, #73614, .T. ) ;
#94787 = CARTESIAN_POINT ( 'NONE',  ( -17.61824857587188831, 50.00000000000002132, 62.61717692869397922 ) ) ;
#94788 = CARTESIAN_POINT ( 'NONE',  ( -43.75401118688381530, 486.3173572309548831, 5.908089951475188784 ) ) ;
#94789 =( NAMED_UNIT ( * ) PLANE_ANGLE_UNIT ( ) SI_UNIT ( $, .RADIAN. ) );
#94790 = CARTESIAN_POINT ( 'NONE',  ( 7.575153643621726829, -15.84894062807185122, -34.99671955924535638 ) ) ;
#94791 = CARTESIAN_POINT ( 'NONE',  ( 0.000000000000000000, 0.000000000000000000, -1.971869939371574620 ) ) ;
#94792 = EDGE_CURVE ( 'NONE', #60249, #106756, #21186, .T. ) ;
#94793 = VERTEX_POINT ( 'NONE', #8085 ) ;
#94794 = CARTESIAN_POINT ( 'NONE',  ( 39.65933660911757386, 485.2174287600339539, -4.382854859801245340 ) ) ;
#94795 = CARTESIAN_POINT ( 'NONE',  ( -9.698972129396508990, 108.1762971274194030, -2.445345647270322775 ) ) ;
#94796 = CARTESIAN_POINT ( 'NONE',  ( -17.74239981412279832, -32.51404901966539995, 29.61011661303510323 ) ) ;
#94798 = CARTESIAN_POINT ( 'NONE',  ( 6.999999999999996447, -4.000000000000003553, 39.12435565298213902 ) ) ;
#94797 = CARTESIAN_POINT ( 'NONE',  ( 102.6464385083043283, -5.000000000000000000, 6.123233995736778115E-16 ) ) ;
#94799 = ORIENTED_EDGE ( 'NONE', *, *, #33526, .T. ) ;
#94800 = AXIS2_PLACEMENT_3D ( 'NONE', #10568, #50484, #83397 ) ;
#94801 = ORIENTED_EDGE ( 'NONE', *, *, #41743, .F. ) ;
#94802 = CARTESIAN_POINT ( 'NONE',  ( -13.43927643640219571, 42.84659330639521357, -92.02404953342519889 ) ) ;
#94803 = VECTOR ( 'NONE', #27823, 1000.000000000000000 ) ;
#94804 = CARTESIAN_POINT ( 'NONE',  ( 15.13304769501646341, 3.593526407993296257, -4.245863293343404621 ) ) ;
#94805 = CARTESIAN_POINT ( 'NONE',  ( -33.56345473223404241, 299.9083031499212666, -8.874823776836098688 ) ) ;
#94806 = ORIENTED_EDGE ( 'NONE', *, *, #11565, .T. ) ;
#94807 = DIRECTION ( 'NONE',  ( 0.000000000000000000, 1.000000000000000000, 0.000000000000000000 ) ) ;
#94808 = DIRECTION ( 'NONE',  ( -0.000000000000000000, -0.000000000000000000, -1.000000000000000000 ) ) ;
#94809 = CARTESIAN_POINT ( 'NONE',  ( 104.0800975233037775, -60.15442106764426455, 190.6471068656633747 ) ) ;
#94811 = DIRECTION ( 'NONE',  ( 0.000000000000000000, -0.9746667163790283528, 0.2236622274388831710 ) ) ;
#94810 = CARTESIAN_POINT ( 'NONE',  ( 39.19831989819565621, -34.84122234843880506, 37.04583787359052849 ) ) ;
#94812 = EDGE_LOOP ( 'NONE', ( #65112, #24523, #89549, #86996 ) ) ;
#94813 = VECTOR ( 'NONE', #38621, 1000.000000000000000 ) ;
#94814 = ORIENTED_EDGE ( 'NONE', *, *, #6750, .T. ) ;
#94815 = ORIENTED_EDGE ( 'NONE', *, *, #57974, .F. ) ;
#94816 = CARTESIAN_POINT ( 'NONE',  ( 24.68056467888841254, 306.9732456607671338, 9.415188885530078267 ) ) ;
#94817 = CIRCLE ( 'NONE', #48282, 5.000000000000010658 ) ;
#94818 = FACE_OUTER_BOUND ( 'NONE', #12307, .T. ) ;
#94819 = VERTEX_POINT ( 'NONE', #40989 ) ;
#94820 = EDGE_CURVE ( 'NONE', #29485, #25032, #67405, .T. ) ;
#94821 = CARTESIAN_POINT ( 'NONE',  ( -5.754767142552475789, 41.95837106010883133, -69.99684969509513621 ) ) ;
#94822 = CARTESIAN_POINT ( 'NONE',  ( -98.65929570741894850, -59.99999999996092015, 58.00980118487002102 ) ) ;
#94823 = AXIS2_PLACEMENT_3D ( 'NONE', #45938, #21173, #86942 ) ;
#94824 = CARTESIAN_POINT ( 'NONE',  ( 7.801642220026309360, -68.58796826149033166, 1.787233835843584862 ) ) ;
#94825 = CARTESIAN_POINT ( 'NONE',  ( 31.02726165664941860, -59.99999999999998579, 43.58380924251923716 ) ) ;
#94826 = CARTESIAN_POINT ( 'NONE',  ( 6.162888688655344005, 3.752776749732561257, -6.499999999999999112 ) ) ;
#94827 = CARTESIAN_POINT ( 'NONE',  ( -5.668093984624058557, 41.44782703750503572, -58.47096610491104229 ) ) ;
#94829 = CARTESIAN_POINT ( 'NONE',  ( 9.022935735952771097, -18.58636217958399328, 26.98789801028366142 ) ) ;
#94828 = CARTESIAN_POINT ( 'NONE',  ( -91.01385585952614576, -29.99999999999999289, 38.60219201899132457 ) ) ;
#94830 = EDGE_CURVE ( 'NONE', #4153, #106581, #100441, .T. ) ;
#94832 = ADVANCED_FACE ( 'NONE', ( #26969 ), #56330, .F. ) ;
#94831 = CARTESIAN_POINT ( 'NONE',  ( -7.433075656983189283, 52.17533548997528214, 2.232706251697821997 ) ) ;
#94833 = CARTESIAN_POINT ( 'NONE',  ( -47.70095744468055443, -39.52629137943383597, 47.20404219366211152 ) ) ;
#94834 = VECTOR ( 'NONE', #103717, 1000.000000000000000 ) ;
#94835 = CARTESIAN_POINT ( 'NONE',  ( 5.484304246340809819, -66.41744476707179956, 14.11761977215489061 ) ) ;
#94836 = ORIENTED_EDGE ( 'NONE', *, *, #30311, .F. ) ;
#94837 = FACE_OUTER_BOUND ( 'NONE', #45952, .T. ) ;
#94838 = FILL_AREA_STYLE ('',( #104491 ) ) ;
#94839 = CARTESIAN_POINT ( 'NONE',  ( 35.90484354297773706, 5.000000000000004441, 6.123233995736770227E-16 ) ) ;
#94840 = ORIENTED_EDGE ( 'NONE', *, *, #52145, .T. ) ;
#94841 = CARTESIAN_POINT ( 'NONE',  ( -6.223369765831527012, -7.361822309467675574, 13.83569840248939897 ) ) ;
#94842 = EDGE_LOOP ( 'NONE', ( #103248, #92515, #99831, #104388 ) ) ;
#94843 = CARTESIAN_POINT ( 'NONE',  ( 59.26090642338721182, -38.34351558597094112, 94.03560012898597620 ) ) ;
#94844 = CARTESIAN_POINT ( 'NONE',  ( 3.438773559904778843, -49.17061000814753413, 103.7823003339739074 ) ) ;
#94845 = PLANE ( 'NONE',  #49613 ) ;
#94846 = CARTESIAN_POINT ( 'NONE',  ( -37.36680950590233863, 18.64316884713579725, 10.04205104295027517 ) ) ;
#94847 = CARTESIAN_POINT ( 'NONE',  ( 98.45347978416359069, -30.00000000000000000, 189.9177565486554613 ) ) ;
#94848 = CARTESIAN_POINT ( 'NONE',  ( 3.636386562469240082E-15, 36.30024107553216339, 29.75000000000000355 ) ) ;
#94849 = ORIENTED_EDGE ( 'NONE', *, *, #66504, .F. ) ;
#94850 = ADVANCED_FACE ( 'NONE', ( #102420 ), #57389, .T. ) ;
#94851 = EDGE_LOOP ( 'NONE', ( #33330, #15730, #37958, #86326, #48083 ) ) ;
#94852 = EDGE_LOOP ( 'NONE', ( #96743, #43203, #20628, #34739 ) ) ;
#94853 = CARTESIAN_POINT ( 'NONE',  ( 54.32622272398685226, -60.31656904070205627, 67.31739225095211054 ) ) ;
#94854 = LINE ( 'NONE', #104509, #9429 ) ;
#94855 = CIRCLE ( 'NONE', #36294, 4.000000000000000888 ) ;
#94856 = CARTESIAN_POINT ( 'NONE',  ( 21.51569398614863715, 294.9107018935607130, -9.987480606144506723 ) ) ;
#94857 = EDGE_CURVE ( 'NONE', #27527, #54223, #52239, .T. ) ;
#94858 = VERTEX_POINT ( 'NONE', #34533 ) ;
#94859 = CARTESIAN_POINT ( 'NONE',  ( -16.02749411895511855, 4.188372957640357441, 2.551519145336385463 ) ) ;
#94860 = AXIS2_PLACEMENT_3D ( 'NONE', #54892, #39804, #71612 ) ;
#94861 = EDGE_LOOP ( 'NONE', ( #64367, #92707, #68320, #39910 ) ) ;
#94862 = CARTESIAN_POINT ( 'NONE',  ( 3.093157300003886334, 6.874418838041290059, 2.297153352953662914E-15 ) ) ;
#94863 = CARTESIAN_POINT ( 'NONE',  ( 92.73232662571349749, -38.49779465622716401, 201.0880014169763115 ) ) ;
#94864 = CARTESIAN_POINT ( 'NONE',  ( 10.77037052812252327, 15.77472040317956470, 9.613292503973772440 ) ) ;
#94865 = CARTESIAN_POINT ( 'NONE',  ( 82.42441318170639875, -37.85770433546145597, 11.94012267114784187 ) ) ;
#94866 = DIRECTION ( 'NONE',  ( -0.000000000000000000, -0.000000000000000000, -1.000000000000000000 ) ) ;
#94867 = CARTESIAN_POINT ( 'NONE',  ( 0.000000000000000000, -1.500000000000000000, -8.000000000000000000 ) ) ;
#94868 = CARTESIAN_POINT ( 'NONE',  ( 41.72794603366077126, 484.6317694608904389, -3.103777363573142267 ) ) ;
#94869 = APPLICATION_CONTEXT ( 'automotive_design' ) ;
#94870 = CARTESIAN_POINT ( 'NONE',  ( 0.000000000000000000, 0.000000000000000000, -0.02540000000000007530 ) ) ;
#94871 = CARTESIAN_POINT ( 'NONE',  ( -39.83854393464088162, 460.2189570659085120, 2.210463671045205913 ) ) ;
#94872 = DIRECTION ( 'NONE',  ( 1.000000000000000000, 0.000000000000000000, 0.000000000000000000 ) ) ;
#94873 = ORIENTED_EDGE ( 'NONE', *, *, #54122, .F. ) ;
#94874 =( NAMED_UNIT ( * ) PLANE_ANGLE_UNIT ( ) SI_UNIT ( $, .RADIAN. ) );
#94875 = ADVANCED_BREP_SHAPE_REPRESENTATION ( '', ( #55444, #10728 ), #52234 ) ;
#94876 = CARTESIAN_POINT ( 'NONE',  ( 15.64282023038906111, 37.16738321503569153, -22.45670599646780374 ) ) ;
#94877 = COLOUR_RGB ( '', 0.66274510, 0.83137255, 0.94901961) ;
#94878 = CARTESIAN_POINT ( 'NONE',  ( -26.34322927111401214, 37.12867781788141031, 7.801957073146333244 ) ) ;
#94879 = ORIENTED_EDGE ( 'NONE', *, *, #63856, .T. ) ;
#94880 = CARTESIAN_POINT ( 'NONE',  ( -5.285714285714275817, -50.19912527334259522, 103.1763305333244318 ) ) ;
#94881 = CARTESIAN_POINT ( 'NONE',  ( -38.37222421136043238, 311.1670517065257968, 5.835050788717471626 ) ) ;
#94882 = LINE ( 'NONE', #93803, #208 ) ;
#94883 =( NAMED_UNIT ( * ) PLANE_ANGLE_UNIT ( ) SI_UNIT ( $, .RADIAN. ) );
#94884 = CARTESIAN_POINT ( 'NONE',  ( -8.000000000000000000, -19.34374999999999289, -3.313708498984762496 ) ) ;
#94885 = CARTESIAN_POINT ( 'NONE',  ( -42.02846191695555689, -38.14260630011440867, 52.77835525687510199 ) ) ;
#94886 = CARTESIAN_POINT ( 'NONE',  ( 41.58031631500816871, 436.8046394031030673, 6.058257849348906987 ) ) ;
#94887 = ORIENTED_EDGE ( 'NONE', *, *, #63054, .F. ) ;
#94888 = CARTESIAN_POINT ( 'NONE',  ( 84.96975805255164005, -35.80893149064998227, 180.8542816627177956 ) ) ;
#94889 = DIRECTION ( 'NONE',  ( 0.000000000000000000, -1.000000000000000000, 0.000000000000000000 ) ) ;
#94890 = FILL_AREA_STYLE_COLOUR ( '', #36660 ) ;
#94891 = ORIENTED_EDGE ( 'NONE', *, *, #103459, .F. ) ;
#94892 = CARTESIAN_POINT ( 'NONE',  ( -88.26195796627457923, -60.15288368548232967, 41.81127973269768461 ) ) ;
#94893 = AXIS2_PLACEMENT_3D ( 'NONE', #97747, #6093, #63823 ) ;
#94894 = CARTESIAN_POINT ( 'NONE',  ( 33.00000000000000000, 461.8802764867031669, 14.89328939272360941 ) ) ;
#94895 = CARTESIAN_POINT ( 'NONE',  ( 12.67000837003893210, -5.000000000000002665, -88.76274061128376047 ) ) ;
#94896 = CARTESIAN_POINT ( 'NONE',  ( -30.93163070004102266, 9.246556120444287430, 40.70059110212513076 ) ) ;
#94897 =( NAMED_UNIT ( * ) SI_UNIT ( $, .STERADIAN. ) SOLID_ANGLE_UNIT ( ) );
#94898 = EDGE_CURVE ( 'NONE', #104615, #38361, #90118, .T. ) ;
#94899 = VECTOR ( 'NONE', #74974, 1000.000000000000000 ) ;
#94900 = CARTESIAN_POINT ( 'NONE',  ( 17.26102777918536546, -23.99532633086393574, 36.28153977239290384 ) ) ;
#94901 = PRESENTATION_LAYER_ASSIGNMENT (  '', '', ( #19177 ) ) ;
#94902 = CARTESIAN_POINT ( 'NONE',  ( 3.498313567328457108, -0.8571732103886707810, 104.2430177423142936 ) ) ;
#94903 = CARTESIAN_POINT ( 'NONE',  ( 49.50347019672712889, -29.59020143643714817, 45.82998437115109169 ) ) ;
#94904 = EDGE_CURVE ( 'NONE', #29309, #103578, #84644, .T. ) ;
#94906 = CARTESIAN_POINT ( 'NONE',  ( -14.20297455945173226, 21.13968428940458111, 5.815581957642580235 ) ) ;
#94905 = FILL_AREA_STYLE_COLOUR ( '', #62116 ) ;
#94907 = EDGE_CURVE ( 'NONE', #91741, #62962, #62575, .T. ) ;
#94908 = AXIS2_PLACEMENT_3D ( 'NONE', #26983, #93277, #10218 ) ;
#94909 = CARTESIAN_POINT ( 'NONE',  ( 8.392508714390126912, 295.8888084830643379, -10.03187903922701629 ) ) ;
#94910 = CARTESIAN_POINT ( 'NONE',  ( -15.64685761340797754, 44.06059264762727423, -4.635351185647528460 ) ) ;
#94911 = ORIENTED_EDGE ( 'NONE', *, *, #22824, .F. ) ;
#94912 = CARTESIAN_POINT ( 'NONE',  ( 43.61687001562553689, 428.0553245671831064, 15.22863618831378218 ) ) ;
#94913 = DIRECTION ( 'NONE',  ( 0.000000000000000000, 0.000000000000000000, 1.000000000000000000 ) ) ;
#94914 = EDGE_CURVE ( 'NONE', #63799, #72871, #38496, .T. ) ;
#94915 = CARTESIAN_POINT ( 'NONE',  ( -83.25840715934710090, -38.00000000000002842, -8.522864994567452612 ) ) ;
#94916 = EDGE_CURVE ( 'NONE', #77294, #35660, #75476, .T. ) ;
#94917 = ORIENTED_EDGE ( 'NONE', *, *, #41698, .T. ) ;
#94918 = CARTESIAN_POINT ( 'NONE',  ( -11.47498123831195649, 2.263339934408738152, 14.82868161565088450 ) ) ;
#94919 =( NAMED_UNIT ( * ) PLANE_ANGLE_UNIT ( ) SI_UNIT ( $, .RADIAN. ) );
#94921 = CARTESIAN_POINT ( 'NONE',  ( -9.688912271943010524, -60.22816138548923703, -36.71155112804019183 ) ) ;
#94920 = CARTESIAN_POINT ( 'NONE',  ( 0.000000000000000000, -20.00000000000001776, -9.000000000000007105 ) ) ;
#94922 = ORIENTED_EDGE ( 'NONE', *, *, #12027, .F. ) ;
#94923 = AXIS2_PLACEMENT_3D ( 'NONE', #20562, #29169, #70105 ) ;
#94924 = DIRECTION ( 'NONE',  ( 0.000000000000000000, -1.000000000000000000, 0.000000000000000000 ) ) ;
#94925 = CARTESIAN_POINT ( 'NONE',  ( 8.866506694866188809, 1.474610560812782335E-15, 0.000000000000000000 ) ) ;
#94926 = ORIENTED_EDGE ( 'NONE', *, *, #72594, .F. ) ;
#94927 = VECTOR ( 'NONE', #4289, 1000.000000000000227 ) ;
#94928 = CARTESIAN_POINT ( 'NONE',  ( -10.00000000000000355, 85.00000000000000000, 0.000000000000000000 ) ) ;
#94929 = VECTOR ( 'NONE', #91019, 1000.000000000000000 ) ;
#94930 = FACE_OUTER_BOUND ( 'NONE', #2602, .T. ) ;
#94931 = CARTESIAN_POINT ( 'NONE',  ( -93.39135768774528401, -60.00000000000000000, 36.04682483438401164 ) ) ;
#94932 = ORIENTED_EDGE ( 'NONE', *, *, #40476, .F. ) ;
#94933 = CARTESIAN_POINT ( 'NONE',  ( 1.816153886384288096, 42.00000000001274714, -59.31995585001071447 ) ) ;
#94934 = CYLINDRICAL_SURFACE ( 'NONE', #69544, 1.250000000000001110 ) ;
#94935 = SURFACE_SIDE_STYLE ('',( #6277 ) ) ;
#94936 = CARTESIAN_POINT ( 'NONE',  ( 17.41226678943441897, 294.5863878355755787, 1.881106500063166598 ) ) ;
#94938 = CARTESIAN_POINT ( 'NONE',  ( 27.59999999999999787, 1.411358822780289120E-15, 0.000000000000000000 ) ) ;
#94937 = SURFACE_SIDE_STYLE ('',( #22109 ) ) ;
#94939 = CARTESIAN_POINT ( 'NONE',  ( -83.26671734593782048, -36.00732091460121609, 166.7895401501197057 ) ) ;
#94940 = ORIENTED_EDGE ( 'NONE', *, *, #3808, .T. ) ;
#94941 = CARTESIAN_POINT ( 'NONE',  ( -42.74220749418430643, 488.2672406020914764, 9.363116084198825462 ) ) ;
#94942 = ORIENTED_EDGE ( 'NONE', *, *, #18018, .F. ) ;
#94943 = VERTEX_POINT ( 'NONE', #60911 ) ;
#94945 =( BOUNDED_SURFACE ( )  B_SPLINE_SURFACE ( 2, 3, ( 
 ( #67392, #59301, #41505, #74393 ),
 ( #472, #83552, #67911, #75465 ),
 ( #91145, #100274, #50126, #10718 ) ),
 .UNSPECIFIED., .F., .F., .T. ) 
 B_SPLINE_SURFACE_WITH_KNOTS ( ( 3, 3 ),
 ( 4, 4 ),
 ( 0.000000000000000000, 1.000000000000000000 ),
 ( 2.852999002495562930, 3.430186304684023302 ),
 .UNSPECIFIED. ) 
 GEOMETRIC_REPRESENTATION_ITEM ( )  RATIONAL_B_SPLINE_SURFACE ( (
 ( 1.000000000000000000, 1.000000000000000000, 1.000000000000000000, 1.000000000000000000),
 ( 1.857142857142858317, 1.857142857142858317, 1.857142857142858317, 1.857142857142858317),
 ( 1.000000000000000000, 1.000000000000000000, 1.000000000000000000, 1.000000000000000000) ) ) 
 REPRESENTATION_ITEM ( '' )  SURFACE ( )  );
#94944 = CARTESIAN_POINT ( 'NONE',  ( 6.648792466258503175, -5.000000000000000000, 15.29529797603218810 ) ) ;
#94946 = CARTESIAN_POINT ( 'NONE',  ( -0.8750000000009734435, -70.58759490697451611, 13.02737050516266315 ) ) ;
#94947 = ORIENTED_EDGE ( 'NONE', *, *, #59341, .T. ) ;
#94948 = EDGE_CURVE ( 'NONE', #1766, #67861, #16059, .T. ) ;
#94949 = CARTESIAN_POINT ( 'NONE',  ( -4.425930005958662145E-15, 43.22324503868515677, 36.14046114390016839 ) ) ;
#94950 = CARTESIAN_POINT ( 'NONE',  ( 9.797174393178825657E-16, -30.00000000000000000, -8.000000000000000000 ) ) ;
#94951 = CARTESIAN_POINT ( 'NONE',  ( -94.41147650277389403, -57.65372982601817853, -11.88746169270405773 ) ) ;
#94952 = CARTESIAN_POINT ( 'NONE',  ( 7.999885325681428405, -13.99977065129938048, 0.2682325777720028781 ) ) ;
#94953 = CARTESIAN_POINT ( 'NONE',  ( -43.02661387979790675, 465.7449615347597387, 11.43319743843399827 ) ) ;
#94954 = CARTESIAN_POINT ( 'NONE',  ( -9.333555687487613994, 103.2189730339102738, 3.591168747312690090 ) ) ;
#94955 = CARTESIAN_POINT ( 'NONE',  ( -16.75187969033554936, -1.200000000000000030E-05, -23.05698433968595751 ) ) ;
#94956 = CARTESIAN_POINT ( 'NONE',  ( 59.37626172009473180, -60.00000000000000000, -38.24869620007160620 ) ) ;
#94957 = EDGE_CURVE ( 'NONE', #87415, #48427, #98722, .T. ) ;
#94959 = EDGE_CURVE ( 'NONE', #36949, #94292, #95296, .T. ) ;
#94958 = CARTESIAN_POINT ( 'NONE',  ( -68.63253095932553549, -60.00000000000002842, 147.4008728361381486 ) ) ;
#94960 = CARTESIAN_POINT ( 'NONE',  ( -54.81653371739410119, -39.50102972048344441, 59.89691189185823106 ) ) ;
#94961 = ORIENTED_EDGE ( 'NONE', *, *, #22623, .F. ) ;
#94962 = ORIENTED_EDGE ( 'NONE', *, *, #47450, .F. ) ;
#94963 = CARTESIAN_POINT ( 'NONE',  ( -99.71594338102195820, -37.80910377345113460, 191.0446671273005279 ) ) ;
#94964 = CARTESIAN_POINT ( 'NONE',  ( 43.00000000000000000, 459.9277931459794218, 6.461582622334586468 ) ) ;
#94965 = ORIENTED_EDGE ( 'NONE', *, *, #59770, .T. ) ;
#94966 = CARTESIAN_POINT ( 'NONE',  ( 18.95131366490356939, 49.31567518127548766, 62.02443497815841056 ) ) ;
#94968 = PRESENTATION_LAYER_ASSIGNMENT (  '', '', ( #15707 ) ) ;
#94967 = CARTESIAN_POINT ( 'NONE',  ( 8.572527594031473190E-16, 34.00000000000000000, -7.000000000000000000 ) ) ;
#94969 = FACE_BOUND ( 'NONE', #16068, .T. ) ;
#94970 = CARTESIAN_POINT ( 'NONE',  ( 5.082755093536325930, -14.84375000204838457, -5.082755093536325042 ) ) ;
#94971 = VECTOR ( 'NONE', #15781, 999.9999999999998863 ) ;
#94972 = CARTESIAN_POINT ( 'NONE',  ( -3.223917338551602008, -68.72997618365062067, 13.04841264822337443 ) ) ;
#94973 = SURFACE_SIDE_STYLE ('',( #44826 ) ) ;
#94974 = CARTESIAN_POINT ( 'NONE',  ( 42.33349330513380693, 1.593028355512270567E-15, 0.000000000000000000 ) ) ;
#94975 = CARTESIAN_POINT ( 'NONE',  ( 65.65137904215926312, -29.99999999999999645, 82.10676440717566038 ) ) ;
#94976 = VECTOR ( 'NONE', #55299, 1000.000000000000000 ) ;
#94977 = CARTESIAN_POINT ( 'NONE',  ( 39.44615384615384812, 1.411358822780289120E-15, 0.000000000000000000 ) ) ;
#94978 = CARTESIAN_POINT ( 'NONE',  ( -37.50031168351941346, 491.1141709719065034, 12.27711733876853906 ) ) ;
#94979 = CARTESIAN_POINT ( 'NONE',  ( -33.00000000000000711, 485.0303364503728289, 0.9535057477320370012 ) ) ;
#94980 = CARTESIAN_POINT ( 'NONE',  ( -28.55605187411735457, -39.48529133943618064, 32.65731791215971214 ) ) ;
#94981 = CIRCLE ( 'NONE', #65698, 4.000000000000007105 ) ;
#94982 = ORIENTED_EDGE ( 'NONE', *, *, #44856, .F. ) ;
#94983 = CARTESIAN_POINT ( 'NONE',  ( 48.29725937789723389, -46.43994943433606437, 50.22590090644417415 ) ) ;
#94984 = CARTESIAN_POINT ( 'NONE',  ( -0.9887052094731583196, 12.53211684992026420, 49.73207603363582763 ) ) ;
#94985 = CIRCLE ( 'NONE', #48435, 2.000000000000000000 ) ;
#94986 = CARTESIAN_POINT ( 'NONE',  ( -6.084941413214105310, 15.01651929834134336, -3.464128533964753842 ) ) ;
#94987 = CIRCLE ( 'NONE', #65780, 4.000000000000007105 ) ;
#94988 = CARTESIAN_POINT ( 'NONE',  ( -92.77767653423819638, -38.49725484616736537, 201.0877250123326974 ) ) ;
#94989 = EDGE_LOOP ( 'NONE', ( #6599, #83821, #1370, #55077, #50998 ) ) ;
#94990 = CARTESIAN_POINT ( 'NONE',  ( 91.35834606489962084, -38.36978471520085776, -3.221837418575325795 ) ) ;
#94991 = SURFACE_SIDE_STYLE ('',( #21640 ) ) ;
#94992 = CARTESIAN_POINT ( 'NONE',  ( -18.92655221378187491, 49.02800889251220440, 62.11188204109627264 ) ) ;
#94993 = CARTESIAN_POINT ( 'NONE',  ( 10.36819426459840265, 43.97404897798725187, 12.90779740156146005 ) ) ;
#94994 = CARTESIAN_POINT ( 'NONE',  ( 6.855074334103434808, 40.29457790742911527, -71.16068745972087584 ) ) ;
#94995 = CARTESIAN_POINT ( 'NONE',  ( -31.61471011888779969, 437.7834120463330692, 21.48349580664253011 ) ) ;
#94996 = CARTESIAN_POINT ( 'NONE',  ( -32.39498043692212548, 435.1520223549252364, 14.91902686226306152 ) ) ;
#94997 = CARTESIAN_POINT ( 'NONE',  ( 10.50000000000000711, -5.000000000000000000, -55.73109925765190553 ) ) ;
#94998 = EDGE_CURVE ( 'NONE', #24767, #91737, #44727, .T. ) ;
#94999 = CARTESIAN_POINT ( 'NONE',  ( 112.1772628306614052, -59.99999999999999289, 169.0755217369682555 ) ) ;
#95000 = DIRECTION ( 'NONE',  ( -1.000000000000000000, -1.224606353822377258E-16, -0.000000000000000000 ) ) ;
#95001 = ORIENTED_EDGE ( 'NONE', *, *, #85532, .T. ) ;
#95002 = DIRECTION ( 'NONE',  ( 0.5735764363510440500, 0.8191520442889932418, 0.000000000000000000 ) ) ;
#95003 = B_SPLINE_CURVE_WITH_KNOTS ( 'NONE', 3,
 ( #49793, #97810, #6679, #74059, #64407, #97280 ),
 .UNSPECIFIED., .F., .F.,
 ( 4, 2, 4 ),
 ( -4.604908129295353508E-06, 0.0003318387708540403657, 0.0006682824498373760849 ),
 .UNSPECIFIED. ) ;
#95004 = VECTOR ( 'NONE', #53662, 1000.000000000000000 ) ;
#95005 = DIRECTION ( 'NONE',  ( 0.000000000000000000, 0.000000000000000000, 1.000000000000000000 ) ) ;
#95006 = ORIENTED_EDGE ( 'NONE', *, *, #70467, .F. ) ;
#95008 = CARTESIAN_POINT ( 'NONE',  ( 5.302285649869180162, 20.37004371428214000, -39.55474687996256478 ) ) ;
#95007 = CARTESIAN_POINT ( 'NONE',  ( -105.5261409709756748, -38.38483589435347199, 196.9266904464792844 ) ) ;
#95009 = CARTESIAN_POINT ( 'NONE',  ( 12.48649638673671802, -3.535767641867485711, -13.71266585591266818 ) ) ;
#95010 = CARTESIAN_POINT ( 'NONE',  ( 44.83349330513380693, -4.000000000000000888, 4.898587196589416773E-16 ) ) ;
#95011 = CARTESIAN_POINT ( 'NONE',  ( 7.188101187500000044, -15.03125000204838457, 0.000000000000000000 ) ) ;
#95012 = CONICAL_SURFACE ( 'NONE', #41543, 3.309500000000001663, 0.9599310885968770357 ) ;
#95013 = CARTESIAN_POINT ( 'NONE',  ( 6.145467200820721843, -5.000000000000002665, -77.00333157708637088 ) ) ;
#95014 = VECTOR ( 'NONE', #18922, 1000.000000000000000 ) ;
#95015 = B_SPLINE_CURVE_WITH_KNOTS ( 'NONE', 3,
 ( #20260, #9980, #86029, #35359, #44493, #77381, #12101, #76839, #19191, #84413, #83869, #92489, #91964, #10509, #42883, #93031, #26743, #27817, #4025, #36952, #69821, #101122, #11030, #34832, #101658, #27283, #60164, #35902 ),
 .UNSPECIFIED., .F., .F.,
 ( 4, 2, 2, 2, 2, 2, 2, 2, 2, 2, 2, 2, 2, 4 ),
 ( 0.0005213801848541129184, 0.0007543876772704475415, 0.0009873951696867831404, 0.001453410154519451519, 0.001919425139352119464, 0.002385440124184787843, 0.003317470093850121132, 0.004249500063515453986, 0.005181530033180787274, 0.006113560002846121430, 0.007045589972511453851, 0.007511604957344118760, 0.007744612449760451649, 0.007977619942176784537 ),
 .UNSPECIFIED. ) ;
#95016 = FACE_OUTER_BOUND ( 'NONE', #34455, .T. ) ;
#95018 = VERTEX_POINT ( 'NONE', #43120 ) ;
#95017 = CARTESIAN_POINT ( 'NONE',  ( 6.394343112843833055, -3.776352960569632433, 6.540835195019756299 ) ) ;
#95019 = CARTESIAN_POINT ( 'NONE',  ( 84.88150630316555123, -25.51212071581490193, 165.4351799496252795 ) ) ;
#95020 = CARTESIAN_POINT ( 'NONE',  ( -44.08684117349997678, 464.4011528862877753, 9.618368244415259838 ) ) ;
#95021 = CARTESIAN_POINT ( 'NONE',  ( 46.08349330513379982, 4.898587196589405926E-16, -4.000000000000001776 ) ) ;
#95022 = ORIENTED_EDGE ( 'NONE', *, *, #100169, .T. ) ;
#95023 = CARTESIAN_POINT ( 'NONE',  ( -28.04142041209776437, 305.7898939697568608, -9.347126562776695735 ) ) ;
#95024 = CARTESIAN_POINT ( 'NONE',  ( -47.50459250088627527, 17.89957706894783840, 14.46754909258801725 ) ) ;
#95025 = CARTESIAN_POINT ( 'NONE',  ( 5.656854249492378806, -29.18749999999999645, 5.656854249492381470 ) ) ;
#95026 = CARTESIAN_POINT ( 'NONE',  ( 69.67238219402268840, 6.975173280561618775E-15, 0.000000000000000000 ) ) ;
#95027 = DIRECTION ( 'NONE',  ( 0.000000000000000000, 0.000000000000000000, 1.000000000000000000 ) ) ;
#95028 = ORIENTED_EDGE ( 'NONE', *, *, #28448, .F. ) ;
#95029 = ADVANCED_FACE ( 'NONE', ( #51188 ), #10206, .T. ) ;
#95030 =( NAMED_UNIT ( * ) PLANE_ANGLE_UNIT ( ) SI_UNIT ( $, .RADIAN. ) );
#95031 = CARTESIAN_POINT ( 'NONE',  ( -76.57718945954728440, -29.99999999999999645, -16.95318723146485951 ) ) ;
#95032 = DIRECTION ( 'NONE',  ( 0.000000000000000000, -1.000000000000000000, 0.000000000000000000 ) ) ;
#95033 = CARTESIAN_POINT ( 'NONE',  ( 14.67692467444030235, 22.45409176455828870, -3.436280814760010571 ) ) ;
#95034 = ADVANCED_FACE ( 'NONE', ( #100808 ), #43622, .T. ) ;
#95036 = PRESENTATION_STYLE_ASSIGNMENT (( #69684 ) ) ;
#95035 = CARTESIAN_POINT ( 'NONE',  ( 33.09999999999999432, 1.533819458162526451E-15, 0.000000000000000000 ) ) ;
#95037 = EDGE_CURVE ( 'NONE', #51548, #79974, #3991, .T. ) ;
#95038 = CARTESIAN_POINT ( 'NONE',  ( 7.188101187500000044, -17.65625000204838457, 0.000000000000000000 ) ) ;
#95039 = CARTESIAN_POINT ( 'NONE',  ( 15.65616503042675767, 294.5586764198427545, -2.062307778642553213 ) ) ;
#95040 = DIRECTION ( 'NONE',  ( 1.000000000000000000, -0.000000000000000000, 1.224646799147353207E-16 ) ) ;
#95041 = EDGE_LOOP ( 'NONE', ( #24355, #9843, #42127, #47200, #48344, #87397 ) ) ;
#95042 = AXIS2_PLACEMENT_3D ( 'NONE', #10093, #50016, #82920 ) ;
#95043 = CARTESIAN_POINT ( 'NONE',  ( 41.96546066671465525, 485.5623541565433356, -4.077117913361723467 ) ) ;
#95044 = EDGE_CURVE ( 'NONE', #86521, #94562, #78569, .T. ) ;
#95045 = CARTESIAN_POINT ( 'NONE',  ( 43.54152132068616510, 464.9591243096638777, 12.86066449444697035 ) ) ;
#95046 = CIRCLE ( 'NONE', #2007, 5.000000000000002665 ) ;
#95047 = CARTESIAN_POINT ( 'NONE',  ( -9.686785446502932828, 8.472505610603299431, -5.000000000000000888 ) ) ;
#95048 = CARTESIAN_POINT ( 'NONE',  ( -6.256238905932293370, -3.000000000000353495, -71.20382035666706599 ) ) ;
#95049 = CARTESIAN_POINT ( 'NONE',  ( -14.84861631010436689, 2.245468665778625361, 2.074511027887800729 ) ) ;
#95050 = ORIENTED_EDGE ( 'NONE', *, *, #56927, .F. ) ;
#95051 = CARTESIAN_POINT ( 'NONE',  ( 35.96984634191181840, 491.2828258641249590, 12.80275614855168342 ) ) ;
#95052 = CARTESIAN_POINT ( 'NONE',  ( -2.354803500934599558, 48.00000000000000000, -100.0000000000000000 ) ) ;
#95054 = VERTEX_POINT ( 'NONE', #4788 ) ;
#95053 = VECTOR ( 'NONE', #74097, 1000.000000000000000 ) ;
#95055 = CIRCLE ( 'NONE', #57137, 0.9999999999999980016 ) ;
#95056 =( NAMED_UNIT ( * ) SI_UNIT ( $, .STERADIAN. ) SOLID_ANGLE_UNIT ( ) );
#95057 = CARTESIAN_POINT ( 'NONE',  ( -42.47818524942086071, 39.50286766178945186, -49.65699901859316867 ) ) ;
#95058 = CARTESIAN_POINT ( 'NONE',  ( -109.8703831905171739, -60.00000000000000000, 191.6706218040895351 ) ) ;
#95059 = DIRECTION ( 'NONE',  ( 1.000000000000000000, 0.000000000000000000, -1.224646799147353207E-16 ) ) ;
#95060 = CARTESIAN_POINT ( 'NONE',  ( -30.00000000000000000, 500.0000000000002274, 0.000000000000000000 ) ) ;
#95061 = FACE_OUTER_BOUND ( 'NONE', #6947, .T. ) ;
#95062 = CARTESIAN_POINT ( 'NONE',  ( 17.83157035608863694, 34.57710935724472279, -22.40747207865632618 ) ) ;
#95063 = CARTESIAN_POINT ( 'NONE',  ( -81.99317651741259283, -57.10874830205603558, 184.9732242174657131 ) ) ;
#95064 = CARTESIAN_POINT ( 'NONE',  ( 30.58918467992911872, 43.16177272848633351, -68.44682372717235808 ) ) ;
#95065 = ORIENTED_EDGE ( 'NONE', *, *, #71814, .F. ) ;
#95066 = DIRECTION ( 'NONE',  ( -1.000000000000000000, -1.224606353822377258E-16, -0.000000000000000000 ) ) ;
#95067 = CARTESIAN_POINT ( 'NONE',  ( 5.856955515201464735, -68.78289058880862683, 1.326217528971463055 ) ) ;
#95068 = CARTESIAN_POINT ( 'NONE',  ( -82.58338653627937731, -37.82595221992723111, 19.55788899699552985 ) ) ;
#95069 = AXIS2_PLACEMENT_3D ( 'NONE', #78215, #62578, #21608 ) ;
#95070 = CARTESIAN_POINT ( 'NONE',  ( -2.152702816552580778, -7.044814775684473673, -13.28738398835509216 ) ) ;
#95071 = STYLED_ITEM ( 'NONE', ( #51694 ), #93400 ) ;
#95072 = CARTESIAN_POINT ( 'NONE',  ( 3.768804542116022116, 132.6332890310193875, -4.999999999999999112 ) ) ;
#95073 = CARTESIAN_POINT ( 'NONE',  ( 40.92692307692308162, 4.172000000000003261, 0.000000000000000000 ) ) ;
#95074 = CARTESIAN_POINT ( 'NONE',  ( 51.76085035121451483, 41.99999999999999289, 29.83308852632746522 ) ) ;
#95075 = CARTESIAN_POINT ( 'NONE',  ( 91.59609553898350498, -30.00000000000011013, 199.7677339052814602 ) ) ;
#95076 = CARTESIAN_POINT ( 'NONE',  ( 0.000000000000000000, 27.55047179872464724, -49.09040922050319011 ) ) ;
#95077 = EDGE_CURVE ( 'NONE', #88114, #61174, #88440, .T. ) ;
#95078 = CARTESIAN_POINT ( 'NONE',  ( -103.3502313461265771, -29.99999999999994671, 116.5677832811329893 ) ) ;
#95079 = STYLED_ITEM ( 'NONE', ( #31646 ), #104567 ) ;
#95080 = CARTESIAN_POINT ( 'NONE',  ( -64.34807526719896487, -29.05564722728329841, 78.93431987242449566 ) ) ;
#95081 = ORIENTED_EDGE ( 'NONE', *, *, #96164, .F. ) ;
#95082 = CARTESIAN_POINT ( 'NONE',  ( 107.5269304809499431, -60.00000000000002132, 200.1385401206229062 ) ) ;
#95083 = CARTESIAN_POINT ( 'NONE',  ( -28.75528690196496839, 39.42481417973143465, 58.36921663661286175 ) ) ;
#95084 = CARTESIAN_POINT ( 'NONE',  ( 68.10881077269327477, -59.99999999992211741, 143.9720702942270805 ) ) ;
#95085 = ORIENTED_EDGE ( 'NONE', *, *, #81492, .T. ) ;
#95086 = CARTESIAN_POINT ( 'NONE',  ( -33.74362713068857289, 463.9326864247045137, 7.533159870298685057 ) ) ;
#95087 = CARTESIAN_POINT ( 'NONE',  ( -2.977408999572650039, -19.06250000204838102, -7.188101187500000933 ) ) ;
#95088 = VERTEX_POINT ( 'NONE', #38759 ) ;
#95089 = CARTESIAN_POINT ( 'NONE',  ( 3.415268766438305459, -49.17042234883166429, 103.8819051289220710 ) ) ;
#95090 = ORIENTED_EDGE ( 'NONE', *, *, #29825, .F. ) ;
#95091 = PLANE ( 'NONE',  #26942 ) ;
#95092 = CARTESIAN_POINT ( 'NONE',  ( -22.28694302522780646, -60.00000000000000000, -41.69514407324499672 ) ) ;
#95093 = DIRECTION ( 'NONE',  ( 0.000000000000000000, -1.000000000000000000, 0.000000000000000000 ) ) ;
#95094 = CARTESIAN_POINT ( 'NONE',  ( -5.082755093536326818, -32.09375000204838813, 5.082755093536325042 ) ) ;
#95095 = CARTESIAN_POINT ( 'NONE',  ( 32.80432905490892637, 485.2968070025902421, 5.900212245013106482 ) ) ;
#95096 = CARTESIAN_POINT ( 'NONE',  ( 20.05453516056601870, -4.285714285714295357, 15.38541618194247462 ) ) ;
#95097 = CARTESIAN_POINT ( 'NONE',  ( -13.00000000000003730, -85.00000000000000000, -4.000000000000001776 ) ) ;
#95098 = FACE_OUTER_BOUND ( 'NONE', #57614, .T. ) ;
#95099 = EDGE_CURVE ( 'NONE', #95526, #64087, #38245, .T. ) ;
#95100 = CARTESIAN_POINT ( 'NONE',  ( -7.986452802927059835, 108.9730975769188461, 0.5332468218996380127 ) ) ;
#95101 = CARTESIAN_POINT ( 'NONE',  ( 38.90208975916642942, 437.7929390081956740, 4.481369775529410404 ) ) ;
#95102 = DIRECTION ( 'NONE',  ( -1.000000000000000000, -0.000000000000000000, -0.000000000000000000 ) ) ;
#95103 = EDGE_LOOP ( 'NONE', ( #88488, #100411, #51233, #79823, #94302 ) ) ;
#95104 = DIRECTION ( 'NONE',  ( -0.5735764363510494901, -0.8191520442889894671, 0.000000000000000000 ) ) ;
#95105 = CARTESIAN_POINT ( 'NONE',  ( 35.58361799548379167, -5.000000000000000888, 6.123233995736769241E-16 ) ) ;
#95106 = CARTESIAN_POINT ( 'NONE',  ( 35.25614048150857371, -29.11149068573612197, 33.41673982746184635 ) ) ;
#95107 = CARTESIAN_POINT ( 'NONE',  ( -22.23822744035697241, -8.673617379884035472E-16, 2.910977163147204116 ) ) ;
#95108 = ORIENTED_EDGE ( 'NONE', *, *, #24161, .T. ) ;
#95109 = CARTESIAN_POINT ( 'NONE',  ( 38.81358894280276672, 485.1131561813238591, -4.191378885298274959 ) ) ;
#95111 = CARTESIAN_POINT ( 'NONE',  ( -23.95564068939877345, 305.6666757346319514, -9.824255363917307804 ) ) ;
#95110 = CARTESIAN_POINT ( 'NONE',  ( 6.539198257602121700, -3.775407874310934719, -6.286450516131051991 ) ) ;
#95112 = DIRECTION ( 'NONE',  ( -0.5735764363510494901, -0.8191520442889894671, 0.000000000000000000 ) ) ;
#95113 = CARTESIAN_POINT ( 'NONE',  ( 4.898587196589412829E-16, -22.81250000409677270, -8.000000000000000000 ) ) ;
#95114 = CARTESIAN_POINT ( 'NONE',  ( -7.500000000000007105, -4.999999999999999112, -52.94236561372731131 ) ) ;
#95115 = DIRECTION ( 'NONE',  ( -0.000000000000000000, 1.000000000000000000, -0.000000000000000000 ) ) ;
#95117 = EDGE_CURVE ( 'NONE', #74794, #94076, #43808, .T. ) ;
#95116 = CARTESIAN_POINT ( 'NONE',  ( 0.000000000000000000, 0.000000000000000000, 0.000000000000000000 ) ) ;
#95118 = CARTESIAN_POINT ( 'NONE',  ( -34.83844953172029335, 463.9146721063430618, 18.82558425661466828 ) ) ;
#95119 = EDGE_LOOP ( 'NONE', ( #64579, #20173, #93260, #31136, #34510, #101525 ) ) ;
#95120 = EDGE_CURVE ( 'NONE', #11929, #62962, #16587, .T. ) ;
#95121 = CARTESIAN_POINT ( 'NONE',  ( 92.42130671373989514, -59.99999999999999289, -0.1412969037266383898 ) ) ;
#95122 = DIRECTION ( 'NONE',  ( -0.000000000000000000, 1.000000000000000000, -0.000000000000000000 ) ) ;
#95124 = CARTESIAN_POINT ( 'NONE',  ( 0.5805565836007605673, -3.752776749732561257, 6.500000000000000000 ) ) ;
#95123 = VECTOR ( 'NONE', #93421, 1000.000000000000000 ) ;
#95125 = AXIS2_PLACEMENT_3D ( 'NONE', #16329, #75082, #7697 ) ;
#95126 = CARTESIAN_POINT ( 'NONE',  ( -5.597109339400236472, 41.52722309069373097, -70.77038831392039242 ) ) ;
#95127 = DIRECTION ( 'NONE',  ( 0.000000000000000000, 0.000000000000000000, -1.000000000000000000 ) ) ;
#95128 = VERTEX_POINT ( 'NONE', #32258 ) ;
#95129 = CARTESIAN_POINT ( 'NONE',  ( -100.6754568013630546, -30.00000000001534417, 198.8498281808039110 ) ) ;
#95130 = ORIENTED_EDGE ( 'NONE', *, *, #102050, .T. ) ;
#95131 = SURFACE_SIDE_STYLE ('',( #54621 ) ) ;
#95132 = CARTESIAN_POINT ( 'NONE',  ( 3.352941176470589646, -48.79941684889505638, 104.5794940929807524 ) ) ;
#95133 = CARTESIAN_POINT ( 'NONE',  ( 16.14327244186471688, 20.71081664948948742, 4.173128809998666533 ) ) ;
#95134 = CONICAL_SURFACE ( 'NONE', #48580, 6.500000000000000000, 1.047197551196600296 ) ;
#95135 = CARTESIAN_POINT ( 'NONE',  ( -7.188101187500000044, -30.78125000204838813, -8.802885111219163269E-16 ) ) ;
#95136 = DIRECTION ( 'NONE',  ( 0.000000000000000000, 0.000000000000000000, 1.000000000000000000 ) ) ;
#95137 = DIRECTION ( 'NONE',  ( -0.000000000000000000, -1.000000000000000000, -0.000000000000000000 ) ) ;
#95138 =( NAMED_UNIT ( * ) PLANE_ANGLE_UNIT ( ) SI_UNIT ( $, .RADIAN. ) );
#95139 = CIRCLE ( 'NONE', #15887, 5.000000000000011546 ) ;
#95140 = ORIENTED_EDGE ( 'NONE', *, *, #79363, .T. ) ;
#95142 = ORIENTED_EDGE ( 'NONE', *, *, #14359, .F. ) ;
#95141 =( NAMED_UNIT ( * ) PLANE_ANGLE_UNIT ( ) SI_UNIT ( $, .RADIAN. ) );
#95143 = CARTESIAN_POINT ( 'NONE',  ( 80.28596508060884673, -22.14989292550031408, 130.4700177602690303 ) ) ;
#95144 =( LENGTH_UNIT ( ) NAMED_UNIT ( * ) SI_UNIT ( .MILLI., .METRE. ) );
#95145 = ORIENTED_EDGE ( 'NONE', *, *, #74402, .T. ) ;
#95146 = CARTESIAN_POINT ( 'NONE',  ( -12.50000000000000533, 27.12381979734430004, -44.66014792738449302 ) ) ;
#95147 = CARTESIAN_POINT ( 'NONE',  ( -2.977408999572650039, -21.68750000204838813, -7.188101187500000933 ) ) ;
#95148 = CARTESIAN_POINT ( 'NONE',  ( -79.30961931381874308, -57.50609382800362823, 198.1725500959836666 ) ) ;
#95149 = ORIENTED_EDGE ( 'NONE', *, *, #29511, .F. ) ;
#95150 = VECTOR ( 'NONE', #33331, 1000.000000000000000 ) ;
#95151 = AXIS2_PLACEMENT_3D ( 'NONE', #35835, #43880, #68716 ) ;
#95152 = CARTESIAN_POINT ( 'NONE',  ( 3.641322288960101350, 22.19827187969977089, 4.999999999999997335 ) ) ;
#95153 = CARTESIAN_POINT ( 'NONE',  ( 6.786616689952412074, 41.72678941544184994, -59.11526159199856068 ) ) ;
#95154 = CIRCLE ( 'NONE', #81331, 12.00000000000000711 ) ;
#95155 = CARTESIAN_POINT ( 'NONE',  ( 48.80564935040053598, 14.82671221252832972, -14.61894534951930069 ) ) ;
#95156 = CARTESIAN_POINT ( 'NONE',  ( -3.313708498984765161, -11.65625000409677092, 7.999999999999998224 ) ) ;
#95157 = CARTESIAN_POINT ( 'NONE',  ( -44.27626259443545109, -28.04480004288071271, 39.31746864059538638 ) ) ;
#95158 = CARTESIAN_POINT ( 'NONE',  ( 9.999999999999996447, 15.00000000000000000, 4.397168787612224072 ) ) ;
#95159 = AXIS2_PLACEMENT_3D ( 'NONE', #54760, #13773, #46685 ) ;
#95160 = CARTESIAN_POINT ( 'NONE',  ( 36.08349330513379982, -4.000000000000000888, 4.898587196589416773E-16 ) ) ;
#95161 = DIRECTION ( 'NONE',  ( 0.000000000000000000, 0.000000000000000000, 1.000000000000000000 ) ) ;
#95162 = CARTESIAN_POINT ( 'NONE',  ( 4.524745413718507692, 51.56500811734601797, 8.282296607710694758 ) ) ;
#95163 = APPLICATION_PROTOCOL_DEFINITION ( 'draft international standard', 'automotive_design', 1998, #67293 ) ;
#95164 = CARTESIAN_POINT ( 'NONE',  ( 38.54676549570872623, 27.49636554353505247, 11.41392474695979864 ) ) ;
#95165 = ORIENTED_EDGE ( 'NONE', *, *, #5066, .T. ) ;
#95166 = CARTESIAN_POINT ( 'NONE',  ( -1.729304526577840617, -50.00420662738919475, 40.95323976638580632 ) ) ;
#95167 = DIRECTION ( 'NONE',  ( 0.000000000000000000, 0.000000000000000000, 1.000000000000000000 ) ) ;
#95168 = EDGE_CURVE ( 'NONE', #37530, #102954, #105599, .T. ) ;
#95169 = DIRECTION ( 'NONE',  ( 0.000000000000000000, 0.000000000000000000, 1.000000000000000000 ) ) ;
#95170 = CARTESIAN_POINT ( 'NONE',  ( 36.34975922649171309, -25.58885759170347285, -36.75400926445155392 ) ) ;
#95171 = CARTESIAN_POINT ( 'NONE',  ( -70.50465783075846105, -30.00000000000000000, 96.95367432551131515 ) ) ;
#95172 = ADVANCED_FACE ( 'NONE', ( #73211 ), #89945, .F. ) ;
#95173 = CARTESIAN_POINT ( 'NONE',  ( 7.500000000000007105, 40.00000000000000000, -58.09827136975972905 ) ) ;
#95174 = B_SPLINE_CURVE_WITH_KNOTS ( 'NONE', 3,
 ( #60985, #102496, #86335, #44261, #28640, #101951, #77153, #44803, #70123, #12931, #77692, #3268, #36209, #69076, #93872, #72756, #87382, #88961, #37795, #30213, #56572, #105663, #21604, #54435, #31799, #23183, #13459, #95999, #5393, #15591, #47946, #97042, #80852, #79800, #48482, #54976 ),
 .UNSPECIFIED., .F., .F.,
 ( 4, 2, 2, 2, 2, 2, 2, 2, 2, 2, 2, 2, 2, 2, 2, 2, 2, 4 ),
 ( 0.000000000000000000, 0.0008074604767267247983, 0.001614920953453449597, 0.002422381430180174395, 0.003229841906906899193, 0.004037302383633624425, 0.004844762860360348790, 0.005652223337087073154, 0.006459683813813798386, 0.007267144290540523618, 0.008074604767267248850, 0.008882065243993972348, 0.009689525720720697580, 0.01049698619744742281, 0.01130444667417414631, 0.01211190715090087154, 0.01251563738926423502, 0.01291936762762759677 ),
 .UNSPECIFIED. ) ;
#95175 = ORIENTED_EDGE ( 'NONE', *, *, #45199, .T. ) ;
#95176 = CARTESIAN_POINT ( 'NONE',  ( -25.91608795999933434, 37.21123558588128333, -8.412246229538014930 ) ) ;
#95177 = CARTESIAN_POINT ( 'NONE',  ( 83.82547419363363872, -57.54511867887681120, 201.6526650243154961 ) ) ;
#95178 = CARTESIAN_POINT ( 'NONE',  ( 66.35709354130753468, -34.58960992778622057, -23.23728143668597212 ) ) ;
#95179 = CARTESIAN_POINT ( 'NONE',  ( -5.589124336233769696, -4.278671059403218457, -6.219623095963493498 ) ) ;
#95180 = CARTESIAN_POINT ( 'NONE',  ( -14.29190075645414737, 21.26710225494818474, 5.626279437268514094 ) ) ;
#95181 = CARTESIAN_POINT ( 'NONE',  ( 10.41054107240687188, 5.000000000000003553, 0.000000000000000000 ) ) ;
#95182 = CARTESIAN_POINT ( 'NONE',  ( -65.73763923497537576, -59.99999999999999289, 121.3057691148710546 ) ) ;
#95183 = CIRCLE ( 'NONE', #98613, 4.000000000000001776 ) ;
#95184 = DIRECTION ( 'NONE',  ( 0.000000000000000000, -1.000000000000000000, 0.000000000000000000 ) ) ;
#95185 = DIRECTION ( 'NONE',  ( 0.000000000000000000, 0.000000000000000000, -1.000000000000000000 ) ) ;
#95186 = CARTESIAN_POINT ( 'NONE',  ( 5.774137037018601148, 50.00000000000000000, 63.00000000000000000 ) ) ;
#95187 = CARTESIAN_POINT ( 'NONE',  ( -85.48259689372021342, -42.91901377629291403, 187.0514599090093668 ) ) ;
#95188 = CONICAL_SURFACE ( 'NONE', #88256, 4.000000000000001776, 0.9599310885968808105 ) ;
#95189 = ORIENTED_EDGE ( 'NONE', *, *, #50449, .T. ) ;
#95190 = CARTESIAN_POINT ( 'NONE',  ( 33.79349388191229053, 321.1166572771793426, -5.792392752899560904 ) ) ;
#95191 = CARTESIAN_POINT ( 'NONE',  ( 43.55923498581227449, 484.2982027343990694, 0.7709916636031838300 ) ) ;
#95192 = CARTESIAN_POINT ( 'NONE',  ( -7.049753390875842740, 41.74264178408463977, -59.69459095116845759 ) ) ;
#95193 = CARTESIAN_POINT ( 'NONE',  ( 12.17614236696284813, -4.623354119923609673, -76.80722648406000985 ) ) ;
#95194 = CARTESIAN_POINT ( 'NONE',  ( -25.49268852105929639, 305.2874338487552563, -9.687155370726696191 ) ) ;
#95195 = CARTESIAN_POINT ( 'NONE',  ( -82.19473257060306537, -37.78714006915895141, -13.37952554880742539 ) ) ;
#95196 = AXIS2_PLACEMENT_3D ( 'NONE', #73868, #106763, #33439 ) ;
#95197 = CARTESIAN_POINT ( 'NONE',  ( 0.9999999999999961142, 0.000000000000000000, 27.00000000000000000 ) ) ;
#95198 = CARTESIAN_POINT ( 'NONE',  ( -44.00534824917842514, 485.4287573672962708, 6.291782489092286212 ) ) ;
#95199 = EDGE_LOOP ( 'NONE', ( #68761, #70916, #18142, #55114 ) ) ;
#95200 = CARTESIAN_POINT ( 'NONE',  ( 18.82548581215701944, 50.00000000000000711, 60.82217600870657748 ) ) ;
#95201 = CARTESIAN_POINT ( 'NONE',  ( 11.08215839935742331, 19.47830716714238974, 8.757826482158389325 ) ) ;
#95202 = CARTESIAN_POINT ( 'NONE',  ( -20.16952962162825358, -4.285714285714285587, -15.50035291838207741 ) ) ;
#95203 = ADVANCED_FACE ( 'NONE', ( #890 ), #33867, .F. ) ;
#95204 = CARTESIAN_POINT ( 'NONE',  ( 81.17508142137076277, -14.21045842199431952, -20.85096179708197184 ) ) ;
#95205 = CARTESIAN_POINT ( 'NONE',  ( -82.19555188958855751, -18.68685282153844440, 137.0995853282088888 ) ) ;
#95206 = VERTEX_POINT ( 'NONE', #99624 ) ;
#95207 = CARTESIAN_POINT ( 'NONE',  ( 43.03265099499984103, 484.2747968070553952, -0.8099405866656324005 ) ) ;
#95208 = DIRECTION ( 'NONE',  ( 3.890967530689355418E-15, -0.2755684261031602356, 0.9612814585411637580 ) ) ;
#95209 = CARTESIAN_POINT ( 'NONE',  ( 68.47697457713316282, -57.68192611185578755, 143.9093171085472136 ) ) ;
#95210 = CARTESIAN_POINT ( 'NONE',  ( -10.00000000000000355, 15.00000000000000000, -10.00000000000000000 ) ) ;
#95211 = UNCERTAINTY_MEASURE_WITH_UNIT (LENGTH_MEASURE( 1.000000000000000082E-05 ), #21106, 'distance_accuracy_value', 'NONE');
#95212 = CARTESIAN_POINT ( 'NONE',  ( 43.06571828467162533, 345.9933190868828774, 10.02031458026529265 ) ) ;
#95213 = CARTESIAN_POINT ( 'NONE',  ( 0.000000000000000000, 44.50000000000000711, 57.21727615095610275 ) ) ;
#95214 = ORIENTED_EDGE ( 'NONE', *, *, #5535, .F. ) ;
#95215 = CARTESIAN_POINT ( 'NONE',  ( 0.000000000000000000, 0.000000000000000000, 0.000000000000000000 ) ) ;
#95216 = CARTESIAN_POINT ( 'NONE',  ( -8.559508646656370345, 51.83514083332403999, 1.531152949374564365 ) ) ;
#95217 = CARTESIAN_POINT ( 'NONE',  ( -1.320432766682874540E-15, -27.03125000204838813, 7.188101187500000044 ) ) ;
#95218 = ORIENTED_EDGE ( 'NONE', *, *, #59964, .T. ) ;
#95219 = CARTESIAN_POINT ( 'NONE',  ( 7.999999999999998224, -20.28125000409677625, 3.313708498984766049 ) ) ;
#95220 =( GEOMETRIC_REPRESENTATION_CONTEXT ( 3 ) GLOBAL_UNCERTAINTY_ASSIGNED_CONTEXT ( ( #67542 ) ) GLOBAL_UNIT_ASSIGNED_CONTEXT ( ( #6910, #32280, #82930 ) ) REPRESENTATION_CONTEXT ( 'NONE', 'WORKASPACE' ) );
#95221 = DIRECTION ( 'NONE',  ( -1.000000000000000000, -0.000000000000000000, -0.000000000000000000 ) ) ;
#95222 = CARTESIAN_POINT ( 'NONE',  ( -44.21445409815639493, 435.3521084850503371, 10.81722560632401731 ) ) ;
#95223 = EDGE_CURVE ( 'NONE', #50155, #10730, #60888, .T. ) ;
#95224 = CARTESIAN_POINT ( 'NONE',  ( -17.26510143360928140, 45.41334515577719344, -6.504361445978008582 ) ) ;
#95225 = CARTESIAN_POINT ( 'NONE',  ( 17.33349330513380693, -4.000000000000000000, 4.898587196589415787E-16 ) ) ;
#95226 = CARTESIAN_POINT ( 'NONE',  ( 17.25418300772434321, 43.52740561176951672, -4.305768132160899597 ) ) ;
#95227 = ORIENTED_EDGE ( 'NONE', *, *, #2307, .F. ) ;
#95228 = CARTESIAN_POINT ( 'NONE',  ( 88.58376342546317517, -59.99999999999997868, -20.95051356008556454 ) ) ;
#95229 = CIRCLE ( 'NONE', #28111, 0.9999999999999993339 ) ;
#95231 = CARTESIAN_POINT ( 'NONE',  ( 24.15507690844725275, -18.60410174432488617, 28.02059554046051204 ) ) ;
#95230 = CARTESIAN_POINT ( 'NONE',  ( -67.93243969554674777, -60.00000000000000711, 143.1807200622937728 ) ) ;
#95232 = CARTESIAN_POINT ( 'NONE',  ( 39.18206537991730443, 57.18445727710330573, -19.59103268995864155 ) ) ;
#95233 = ORIENTED_EDGE ( 'NONE', *, *, #34496, .F. ) ;
#95234 = ORIENTED_EDGE ( 'NONE', *, *, #2698, .F. ) ;
#95235 = DIRECTION ( 'NONE',  ( 0.000000000000000000, -1.000000000000000000, 0.000000000000000000 ) ) ;
#95236 = DIRECTION ( 'NONE',  ( -0.9090909090909090606, 0.000000000000000000, 0.4165977904505314133 ) ) ;
#95237 = SURFACE_SIDE_STYLE ('',( #105439 ) ) ;
#95238 = DIRECTION ( 'NONE',  ( 0.000000000000000000, 0.000000000000000000, -1.000000000000000000 ) ) ;
#95239 = CARTESIAN_POINT ( 'NONE',  ( 11.33125095928769355, 2.319207801596048224, 14.82048394585365791 ) ) ;
#95240 = CARTESIAN_POINT ( 'NONE',  ( -15.72218280906577625, 5.595371698627605639, 6.516822309428270010 ) ) ;
#95241 = ORIENTED_EDGE ( 'NONE', *, *, #103491, .T. ) ;
#95242 = EDGE_CURVE ( 'NONE', #74067, #103934, #35037, .T. ) ;
#95243 = CARTESIAN_POINT ( 'NONE',  ( 90.02747032318434606, -29.99999999999950617, 189.8937112016718913 ) ) ;
#95244 = CARTESIAN_POINT ( 'NONE',  ( -11.89787374881586501, 21.47933664795157327, -7.281391404119607280 ) ) ;
#95245 = CARTESIAN_POINT ( 'NONE',  ( 7.500000000000000888, -3.988190556646206364, -0.8526458641284285767 ) ) ;
#95246 = CARTESIAN_POINT ( 'NONE',  ( 81.42671810001343147, -30.00000000000000355, -2.306699052306097730 ) ) ;
#95247 =( BOUNDED_CURVE ( )  B_SPLINE_CURVE ( 2, ( #17032, #82817, #8916, #73645, #32157, #65036, #24084, #56925, #106549 ),
 .UNSPECIFIED., .F., .F. ) 
 B_SPLINE_CURVE_WITH_KNOTS ( ( 3, 2, 2, 2, 3 ),
 ( 0.6911764705882352811, 0.6985294117647058432, 0.7058823529411765163, 0.7132352941176470784, 0.7205882352941176405 ),
 .UNSPECIFIED. ) 
 CURVE ( )  GEOMETRIC_REPRESENTATION_ITEM ( )  RATIONAL_B_SPLINE_CURVE ( ( 1.000000000000000000, 0.9238795325112867385, 1.000000000000000000, 0.9238795325112867385, 1.000000000000000000, 0.9238795325112867385, 1.000000000000000000, 0.9238795325112867385, 1.000000000000000000 ) ) 
 REPRESENTATION_ITEM ( '' )  );
#95248 = EDGE_CURVE ( 'NONE', #24986, #77591, #36742, .T. ) ;
#95249 = LINE ( 'NONE', #88214, #84619 ) ;
#95250 = VERTEX_POINT ( 'NONE', #50013 ) ;
#95251 = B_SPLINE_CURVE_WITH_KNOTS ( 'NONE', 3,
 ( #87119, #37531, #63380, #46637, #21870, #22403 ),
 .UNSPECIFIED., .F., .F.,
 ( 4, 2, 4 ),
 ( 0.000000000000000000, 0.5000000000000000000, 1.000000000000000000 ),
 .UNSPECIFIED. ) ;
#95252 = ORIENTED_EDGE ( 'NONE', *, *, #29002, .T. ) ;
#95253 = ORIENTED_EDGE ( 'NONE', *, *, #73620, .F. ) ;
#95254 = DIRECTION ( 'NONE',  ( 0.000000000000000000, 0.000000000000000000, -1.000000000000000000 ) ) ;
#95255 = DIRECTION ( 'NONE',  ( 0.5735764363510462704, 0.8191520442889915765, 0.000000000000000000 ) ) ;
#95256 = CARTESIAN_POINT ( 'NONE',  ( 0.000000000000000000, 4.000000000000000000, 3.500000000000000000 ) ) ;
#95257 = CARTESIAN_POINT ( 'NONE',  ( -45.50297956008602540, 391.5886742618069434, 8.004120577752210863 ) ) ;
#95258 =( NAMED_UNIT ( * ) SI_UNIT ( $, .STERADIAN. ) SOLID_ANGLE_UNIT ( ) );
#95259 = ADVANCED_FACE ( 'NONE', ( #99082 ), #83194, .T. ) ;
#95260 = CARTESIAN_POINT ( 'NONE',  ( -7.896571385775229324, -88.78997999345754977, 1.305932416347435732 ) ) ;
#95261 = CYLINDRICAL_SURFACE ( 'NONE', #67324, 4.000000000000000000 ) ;
#95262 = EDGE_LOOP ( 'NONE', ( #54224, #24719, #51583, #73807 ) ) ;
#95263 = CARTESIAN_POINT ( 'NONE',  ( 5.036189802311931807, 48.00000000000000000, -93.73786388412125348 ) ) ;
#95264 = ORIENTED_EDGE ( 'NONE', *, *, #32011, .T. ) ;
#95265 = CARTESIAN_POINT ( 'NONE',  ( -2.450449656239130025, 15.75130202679986269, -9.701736001019305888 ) ) ;
#95266 = CARTESIAN_POINT ( 'NONE',  ( 61.07682198875333768, -38.34186034985221170, 99.84630197542874441 ) ) ;
#95267 = CARTESIAN_POINT ( 'NONE',  ( -40.08499133126677094, 485.6798096563409217, -4.492259481483594996 ) ) ;
#95268 = EDGE_CURVE ( 'NONE', #62970, #1839, #70853, .T. ) ;
#95269 = CARTESIAN_POINT ( 'NONE',  ( -81.20402667235619276, -59.99999999999999289, 183.8840203063076615 ) ) ;
#95270 = CARTESIAN_POINT ( 'NONE',  ( 64.65535091061465778, -18.62627765022782711, 74.52426303803912333 ) ) ;
#95271 = VECTOR ( 'NONE', #33346, 1000.000000000000000 ) ;
#95272 = ADVANCED_FACE ( 'NONE', ( #54114 ), #23296, .F. ) ;
#95273 = ORIENTED_EDGE ( 'NONE', *, *, #2438, .F. ) ;
#95274 = CARTESIAN_POINT ( 'NONE',  ( -7.500000000000007105, 39.99999999999998579, -68.91429205786793943 ) ) ;
#95275 = CARTESIAN_POINT ( 'NONE',  ( 0.000000000000000000, 0.000000000000000000, -10.00000000000000000 ) ) ;
#95276 = VECTOR ( 'NONE', #50972, 1000.000000000000114 ) ;
#95277 = CARTESIAN_POINT ( 'NONE',  ( -6.322210203194782885, 10.35489075027773254, -3.011395388464981338 ) ) ;
#95278 = CARTESIAN_POINT ( 'NONE',  ( -8.717348576474769573, 51.77858947231555220, 1.531152949374564143 ) ) ;
#95279 = B_SPLINE_CURVE_WITH_KNOTS ( 'NONE', 3,
 ( #90929, #17040, #7324, #49376, #48841, #24616, #57464, #105506, #7857, #56400, #82285, #73655, #47783, #98985, #82823, #80685, #23555, #49915, #33767, #8922, #24091, #8396, #65579, #40236, #97395, #56934, #41828, #89334, #15426, #41298, #6805, #72601 ),
 .UNSPECIFIED., .F., .F.,
 ( 4, 2, 2, 2, 2, 2, 2, 2, 2, 2, 2, 2, 2, 2, 2, 4 ),
 ( 0.02274979562923905643, 0.02388451199206677311, 0.02501922835489448979, 0.02615394471772220647, 0.02728866108054992315, 0.02842337744337763983, 0.02955809380620535998, 0.03069281016903307666, 0.03182752653186079334, 0.03296224289468851348, 0.03409695925751622669, 0.03523167562034394684, 0.03636639198317166699, 0.03750110834599938714, 0.03863582470882710729, 0.04090525743448254065 ),
 .UNSPECIFIED. ) ;
#95280 = ORIENTED_EDGE ( 'NONE', *, *, #14830, .T. ) ;
#95281 = CARTESIAN_POINT ( 'NONE',  ( 23.58349330513380337, -4.000000000000000000, 4.898587196589415787E-16 ) ) ;
#95282 = CARTESIAN_POINT ( 'NONE',  ( -67.80574261165853045, -59.99999999999996447, -27.21884045395757923 ) ) ;
#95283 = DIRECTION ( 'NONE',  ( -1.000000000000000000, -0.000000000000000000, -0.000000000000000000 ) ) ;
#95284 = CARTESIAN_POINT ( 'NONE',  ( -28.99999999999998934, 0.000000000000000000, -9.000000000000000000 ) ) ;
#95285 = CARTESIAN_POINT ( 'NONE',  ( 9.701712097384767475, 15.75132464342601146, 2.450541714948253347 ) ) ;
#95286 = CARTESIAN_POINT ( 'NONE',  ( 84.25898199574321268, -61.06033809349827379, 192.6519333314404321 ) ) ;
#95287 = CARTESIAN_POINT ( 'NONE',  ( -5.221476981229875136, 6.992073347021172225, -27.46175062982092996 ) ) ;
#95288 = CARTESIAN_POINT ( 'NONE',  ( -9.999142969094119593, 7.501227345702223381, 0.000000000000000000 ) ) ;
#95289 = CARTESIAN_POINT ( 'NONE',  ( 81.26467260280679739, 1.016364837396684119E-14, 0.000000000000000000 ) ) ;
#95290 = CARTESIAN_POINT ( 'NONE',  ( 13.69901872062297166, -51.35359963483656287, 24.10656755472290769 ) ) ;
#95291 = CARTESIAN_POINT ( 'NONE',  ( 17.61650669486618881, 4.898587196589413815E-16, -4.000000000000000888 ) ) ;
#95292 = AXIS2_PLACEMENT_3D ( 'NONE', #42482, #24734, #75378 ) ;
#95293 = CARTESIAN_POINT ( 'NONE',  ( -97.63826302307023752, -29.99999999999999289, 135.0012949887297964 ) ) ;
#95294 = EDGE_CURVE ( 'NONE', #68089, #96995, #16, .T. ) ;
#95295 =( GEOMETRIC_REPRESENTATION_CONTEXT ( 3 ) GLOBAL_UNCERTAINTY_ASSIGNED_CONTEXT ( ( #27668 ) ) GLOBAL_UNIT_ASSIGNED_CONTEXT ( ( #101104, #59061, #9960 ) ) REPRESENTATION_CONTEXT ( 'NONE', 'WORKASPACE' ) );
#95296 = CIRCLE ( 'NONE', #12589, 4.172000000000001485 ) ;
#95297 = CARTESIAN_POINT ( 'NONE',  ( -2.971071886220395530, -5.790204346174092187, -1.819539708428537912E-14 ) ) ;
#95298 = CARTESIAN_POINT ( 'NONE',  ( 18.63861866008372914, -57.67172055977938072, 42.04919199611194358 ) ) ;
#95299 = EDGE_CURVE ( 'NONE', #77629, #34409, #104809, .T. ) ;
#95301 = DIRECTION ( 'NONE',  ( 0.000000000000000000, 1.000000000000000000, 0.000000000000000000 ) ) ;
#95300 = CARTESIAN_POINT ( 'NONE',  ( 9.077274974099184490, 43.76958732884290271, 14.51298487815000193 ) ) ;
#95302 = CARTESIAN_POINT ( 'NONE',  ( -46.55033485923301129, 41.07609223179107261, -46.50387006460696426 ) ) ;
#95303 = CARTESIAN_POINT ( 'NONE',  ( -17.57798479617512655, 49.99999999999999289, 62.77754979738582364 ) ) ;
#95304 = CARTESIAN_POINT ( 'NONE',  ( 43.00000000000000000, 500.0000000000002274, 0.000000000000000000 ) ) ;
#95305 = CARTESIAN_POINT ( 'NONE',  ( 46.00000000000000000, 488.3725375423282458, 3.127739281032916097 ) ) ;
#95306 = CARTESIAN_POINT ( 'NONE',  ( 8.061685236282825271E-09, -15.39512265162600535, -35.22781471665102515 ) ) ;
#95307 = DIRECTION ( 'NONE',  ( -1.000000000000000000, -1.224606353822377258E-16, -0.000000000000000000 ) ) ;
#95308 = CARTESIAN_POINT ( 'NONE',  ( 43.04469050570450150, 434.7734435962914290, 9.248231035223298591 ) ) ;
#95309 = EDGE_LOOP ( 'NONE', ( #50150, #77254 ) ) ;
#95310 = CARTESIAN_POINT ( 'NONE',  ( 41.46910480218708273, 484.7338956289814860, -3.418960549715457375 ) ) ;
#95311 = DIRECTION ( 'NONE',  ( 0.000000000000000000, 1.000000000000000000, 0.000000000000000000 ) ) ;
#95312 = CARTESIAN_POINT ( 'NONE',  ( -12.26548772233443607, -29.03140120957289483, 28.77903004484144844 ) ) ;
#95314 = DIRECTION ( 'NONE',  ( -0.000000000000000000, 1.000000000000000000, -0.000000000000000000 ) ) ;
#95313 = CARTESIAN_POINT ( 'NONE',  ( -85.18896233714281152, -59.99999999999995737, -15.68185129854840554 ) ) ;
#95315 = ORIENTED_EDGE ( 'NONE', *, *, #58322, .T. ) ;
#95316 = SURFACE_STYLE_FILL_AREA ( #11180 ) ;
#95317 = CARTESIAN_POINT ( 'NONE',  ( 0.5805565836007650082, -3.752776749732574135, -6.500000000000001776 ) ) ;
#95318 = CARTESIAN_POINT ( 'NONE',  ( 16.02369196221434677, 4.084267053693343641, -2.245701149433702692 ) ) ;
#95319 = ADVANCED_FACE ( 'NONE', ( #89694 ), #31485, .F. ) ;
#95320 = CARTESIAN_POINT ( 'NONE',  ( 0.000000000000000000, 6.123233995736767268E-16, -5.000000000000000888 ) ) ;
#95321 = ORIENTED_EDGE ( 'NONE', *, *, #14582, .F. ) ;
#95322 = DIRECTION ( 'NONE',  ( 1.000000000000000000, 0.000000000000000000, -0.000000000000000000 ) ) ;
#95323 = VECTOR ( 'NONE', #94382, 1000.000000000000000 ) ;
#95324 = SURFACE_SIDE_STYLE ('',( #95857 ) ) ;
#95325 = CARTESIAN_POINT ( 'NONE',  ( -6.795502735115863224, 303.7372916219597414, -10.02434238300769032 ) ) ;
#95326 = ORIENTED_EDGE ( 'NONE', *, *, #95372, .F. ) ;
#95327 = AXIS2_PLACEMENT_3D ( 'NONE', #4548, #10505, #94092 ) ;
#95328 = ORIENTED_EDGE ( 'NONE', *, *, #42972, .F. ) ;
#95329 = CARTESIAN_POINT ( 'NONE',  ( -28.84813086497338475, 319.7805192248010258, 12.61644190180718006 ) ) ;
#95330 = ORIENTED_EDGE ( 'NONE', *, *, #22675, .T. ) ;
#95331 = SURFACE_SIDE_STYLE ('',( #30082 ) ) ;
#95332 = DIRECTION ( 'NONE',  ( -1.000000000000000000, -1.224606353822377258E-16, -0.000000000000000000 ) ) ;
#95333 = FACE_OUTER_BOUND ( 'NONE', #13596, .T. ) ;
#95335 = EDGE_CURVE ( 'NONE', #70548, #77591, #55696, .T. ) ;
#95334 = ORIENTED_EDGE ( 'NONE', *, *, #13164, .T. ) ;
#95336 = CARTESIAN_POINT ( 'NONE',  ( 89.06666666666666288, 1.023464760207051730E-14, 0.000000000000000000 ) ) ;
#95337 = CARTESIAN_POINT ( 'NONE',  ( -6.917891564935159998, 41.82074884801031800, -68.91429205806258551 ) ) ;
#95338 = CARTESIAN_POINT ( 'NONE',  ( -81.99131086603355811, -60.00000000001472245, 201.2528149072493591 ) ) ;
#95339 = DIRECTION ( 'NONE',  ( -1.734723475976807094E-16, -0.000000000000000000, -1.000000000000000000 ) ) ;
#95340 = CARTESIAN_POINT ( 'NONE',  ( 27.99111733527702128, -59.99999999998071587, -43.50173535898519361 ) ) ;
#95341 = CARTESIAN_POINT ( 'NONE',  ( 3.302481927409230966, -4.999999999999999112, 16.08827426322715581 ) ) ;
#95342 = CARTESIAN_POINT ( 'NONE',  ( -5.420469775605653240, 41.88321586335170821, -59.04137891894602319 ) ) ;
#95343 = MECHANICAL_DESIGN_GEOMETRIC_PRESENTATION_REPRESENTATION (  '', ( #38538 ), #52284 ) ;
#95345 = CARTESIAN_POINT ( 'NONE',  ( 10.33868530926878293, -46.43477040252509624, 31.64147147909017477 ) ) ;
#95344 = CARTESIAN_POINT ( 'NONE',  ( -93.27866288726950472, -14.21045842199433373, 72.78127944122930160 ) ) ;
#95346 = DIRECTION ( 'NONE',  ( 0.000000000000000000, -1.000000000000000000, 0.000000000000000000 ) ) ;
#95347 = CARTESIAN_POINT ( 'NONE',  ( -48.79702489733374193, -53.36716363833840404, 53.26924858186875156 ) ) ;
#95348 = CARTESIAN_POINT ( 'NONE',  ( -2.455519666312785620, 21.02091283430367241, 6.559096923523866529 ) ) ;
#95349 = ORIENTED_EDGE ( 'NONE', *, *, #57441, .F. ) ;
#95350 = CARTESIAN_POINT ( 'NONE',  ( 1.159632968975068845, 11.84294440633027001, -50.01761517489052267 ) ) ;
#95351 = DIRECTION ( 'NONE',  ( -1.000000000000000000, 0.000000000000000000, 0.000000000000000000 ) ) ;
#95352 = CYLINDRICAL_SURFACE ( 'NONE', #24160, 1.250000000000000222 ) ;
#95353 = ORIENTED_EDGE ( 'NONE', *, *, #32843, .T. ) ;
#95354 = CARTESIAN_POINT ( 'NONE',  ( -11.55112723807207331, -8.861487880012006713, 19.08437505212382845 ) ) ;
#95355 = ORIENTED_EDGE ( 'NONE', *, *, #17216, .F. ) ;
#95356 = CARTESIAN_POINT ( 'NONE',  ( 109.5302677101368971, -30.00000000002007638, 167.0734019624199220 ) ) ;
#95357 = CARTESIAN_POINT ( 'NONE',  ( 43.58349330513380693, 1.593028355512270567E-15, 0.000000000000000000 ) ) ;
#95358 = VECTOR ( 'NONE', #27930, 1000.000000000000000 ) ;
#95359 = CARTESIAN_POINT ( 'NONE',  ( 6.986467729351123701, 41.76526144824654807, -59.56845322044426183 ) ) ;
#95360 = CARTESIAN_POINT ( 'NONE',  ( 15.50526908259248593, 42.00000000004113332, 57.69562748392037577 ) ) ;
#95361 = CARTESIAN_POINT ( 'NONE',  ( 98.45048472303585640, -29.99999999999998934, 189.9226899209341752 ) ) ;
#95362 = AXIS2_PLACEMENT_3D ( 'NONE', #33710, #100010, #75737 ) ;
#95363 = EDGE_CURVE ( 'NONE', #37934, #45434, #105860, .T. ) ;
#95364 = CARTESIAN_POINT ( 'NONE',  ( 28.99999999999999645, 6.123233995736765296E-16, 4.999999999999999112 ) ) ;
#95365 = ORIENTED_EDGE ( 'NONE', *, *, #101410, .F. ) ;
#95366 = STYLED_ITEM ( 'NONE', ( #62658 ), #44833 ) ;
#95367 = AXIS2_PLACEMENT_3D ( 'NONE', #19189, #33217, #9425 ) ;
#95368 = VERTEX_POINT ( 'NONE', #48675 ) ;
#95369 = ORIENTED_EDGE ( 'NONE', *, *, #91017, .F. ) ;
#95370 = DIRECTION ( 'NONE',  ( -0.5735764363510494901, -0.8191520442889894671, 0.000000000000000000 ) ) ;
#95371 = CARTESIAN_POINT ( 'NONE',  ( 0.000000000000000000, -48.79941684889505638, 120.1428571428571388 ) ) ;
#95372 = EDGE_CURVE ( 'NONE', #29177, #100701, #81559, .T. ) ;
#95373 = ORIENTED_EDGE ( 'NONE', *, *, #76816, .F. ) ;
#95374 = DIRECTION ( 'NONE',  ( -1.000000000000000000, -1.224606353822377258E-16, -0.000000000000000000 ) ) ;
#95375 = ORIENTED_EDGE ( 'NONE', *, *, #9834, .T. ) ;
#95376 = CARTESIAN_POINT ( 'NONE',  ( 90.18666349947973515, -38.51691557554957512, 200.6227239373147029 ) ) ;
#95377 = CARTESIAN_POINT ( 'NONE',  ( 11.22265610080591003, 19.85824387651571499, 8.522341943024397182 ) ) ;
#95378 = CARTESIAN_POINT ( 'NONE',  ( 82.58786548269614514, -37.85377812443031331, 19.55393185633859687 ) ) ;
#95379 = CARTESIAN_POINT ( 'NONE',  ( 6.222742520105469133, -3.584500230190538428, 6.791463481567636684 ) ) ;
#95380 = CARTESIAN_POINT ( 'NONE',  ( 32.46537690518270125, 342.4109961635215882, 19.27576733899797645 ) ) ;
#95381 = CARTESIAN_POINT ( 'NONE',  ( 0.000000000000000000, -14.49999999999999822, -9.000000000000000000 ) ) ;
#95382 = DIRECTION ( 'NONE',  ( 0.000000000000000000, 1.000000000000000000, 0.000000000000000000 ) ) ;
#95383 = ADVANCED_FACE ( 'NONE', ( #29889 ), #62774, .F. ) ;
#95384 = CARTESIAN_POINT ( 'NONE',  ( 0.000000000000000000, 48.50000000000000000, 62.00000000000000000 ) ) ;
#95385 = FILL_AREA_STYLE_COLOUR ( '', #2416 ) ;
#95386 = ORIENTED_EDGE ( 'NONE', *, *, #96075, .T. ) ;
#95387 = CARTESIAN_POINT ( 'NONE',  ( -34.39884064632509819, 463.9244153862098301, 5.561476059303757324 ) ) ;
#95388 = VECTOR ( 'NONE', #62717, 1000.000000000000000 ) ;
#95389 = CARTESIAN_POINT ( 'NONE',  ( -3.006276549692158628, 103.2175972223608937, 4.999999999999999112 ) ) ;
#95390 = ORIENTED_EDGE ( 'NONE', *, *, #21862, .T. ) ;
#95391 = CARTESIAN_POINT ( 'NONE',  ( -32.76369084077356320, 322.0407035852106219, -4.798215932636743730 ) ) ;
#95392 = CARTESIAN_POINT ( 'NONE',  ( -24.42128123963413344, 304.1868369482826324, 10.22974940677398692 ) ) ;
#95393 = DIRECTION ( 'NONE',  ( 0.000000000000000000, 0.000000000000000000, 1.000000000000000000 ) ) ;
#95394 = CARTESIAN_POINT ( 'NONE',  ( 7.999999999999998224, -18.59374999999998934, 3.313708498984766493 ) ) ;
#95395 = CARTESIAN_POINT ( 'NONE',  ( 19.80240316827772418, -19.66620075454853023, 35.71518255902564931 ) ) ;
#95396 = DIRECTION ( 'NONE',  ( 0.000000000000000000, 0.7633528697415662423, -0.6459817305909786311 ) ) ;
#95397 = ORIENTED_EDGE ( 'NONE', *, *, #11285, .F. ) ;
#95398 = CARTESIAN_POINT ( 'NONE',  ( 83.08287465949443629, -57.29649053352386545, 188.7195907736446259 ) ) ;
#95399 = CARTESIAN_POINT ( 'NONE',  ( -38.56652002779529909, 27.31830886215414012, 12.97473753426408472 ) ) ;
#95400 = CARTESIAN_POINT ( 'NONE',  ( -5.290067270632268226, 54.20842449845686417, -6.031152949374520844 ) ) ;
#95401 = EDGE_LOOP ( 'NONE', ( #93482, #59473, #68277, #1400 ) ) ;
#95402 = AXIS2_PLACEMENT_3D ( 'NONE', #64666, #71158, #71676 ) ;
#95403 = CARTESIAN_POINT ( 'NONE',  ( 94.19135992194647145, -57.67257302826786258, 22.54914657329851124 ) ) ;
#95404 = CARTESIAN_POINT ( 'NONE',  ( 0.7145311798163270778, 9.237604307034018802, 2.885982852862873934E-16 ) ) ;
#95405 = CARTESIAN_POINT ( 'NONE',  ( -14.73122683063152571, -5.000000000000002665, -81.05502296678268692 ) ) ;
#95406 = CARTESIAN_POINT ( 'NONE',  ( -30.42742517972270377, 7.740625494265014339, 41.86256052107386694 ) ) ;
#95407 = PRESENTATION_STYLE_ASSIGNMENT (( #28582 ) ) ;
#95408 =( GEOMETRIC_REPRESENTATION_CONTEXT ( 3 ) GLOBAL_UNCERTAINTY_ASSIGNED_CONTEXT ( ( #78313 ) ) GLOBAL_UNIT_ASSIGNED_CONTEXT ( ( #35137, #26004, #34081 ) ) REPRESENTATION_CONTEXT ( 'NONE', 'WORKASPACE' ) );
#95409 = EDGE_CURVE ( 'NONE', #22420, #73528, #26492, .T. ) ;
#95410 = CARTESIAN_POINT ( 'NONE',  ( 11.50153144591023135, -20.88508670642358567, 35.51598441719492882 ) ) ;
#95411 = SURFACE_SIDE_STYLE ('',( #36161 ) ) ;
#95412 = CARTESIAN_POINT ( 'NONE',  ( 45.73666261138588851, -28.54726377660503189, 40.86505474274270711 ) ) ;
#95413 = ADVANCED_FACE ( 'NONE', ( #91820, #17407 ), #9812, .T. ) ;
#95415 = CARTESIAN_POINT ( 'NONE',  ( -10.02817096105811778, 14.31193741560988641, 10.49095716857858029 ) ) ;
#95414 = CARTESIAN_POINT ( 'NONE',  ( -19.73463816634111012, 304.7971333121958537, 8.925379062039116462 ) ) ;
#95416 = CARTESIAN_POINT ( 'NONE',  ( 42.08762648273145857, 487.0030674539048050, 9.106351919857864630 ) ) ;
#95417 = CARTESIAN_POINT ( 'NONE',  ( 0.000000000000000000, -78.00000000000000000, 27.00000000000000000 ) ) ;
#95418 = CARTESIAN_POINT ( 'NONE',  ( 43.67632028636852937, 390.4705434914407078, 15.75357519261242167 ) ) ;
#95419 = CARTESIAN_POINT ( 'NONE',  ( -18.91781669292785395, 48.00000000000000000, 62.18610382930904734 ) ) ;
#95420 = ADVANCED_FACE ( 'NONE', ( #42729 ), #83703, .F. ) ;
#95421 = CARTESIAN_POINT ( 'NONE',  ( 46.00000000000000000, 450.0000000000002274, 13.20242257375370976 ) ) ;
#95422 =( GEOMETRIC_REPRESENTATION_CONTEXT ( 3 ) GLOBAL_UNCERTAINTY_ASSIGNED_CONTEXT ( ( #67773 ) ) GLOBAL_UNIT_ASSIGNED_CONTEXT ( ( #35883, #62652, #39441 ) ) REPRESENTATION_CONTEXT ( 'NONE', 'WORKASPACE' ) );
#95423 = ORIENTED_EDGE ( 'NONE', *, *, #73497, .F. ) ;
#95424 = CARTESIAN_POINT ( 'NONE',  ( -11.18613547696531185, 2.364262554124563653, 14.81278392879739947 ) ) ;
#95425 = CARTESIAN_POINT ( 'NONE',  ( 5.093082057083964997, -62.55553793578429378, -3.176439207277723664 ) ) ;
#95426 = VECTOR ( 'NONE', #42997, 1000.000000000000000 ) ;
#95428 = CARTESIAN_POINT ( 'NONE',  ( -9.445484387178764152, -34.58962642155982792, -32.44472896259313188 ) ) ;
#95427 = CARTESIAN_POINT ( 'NONE',  ( 39.56197461363974099, -0.1944580884125578779, 19.78098730681987050 ) ) ;
#95429 = EDGE_CURVE ( 'NONE', #80759, #61174, #38337, .T. ) ;
#95430 = ORIENTED_EDGE ( 'NONE', *, *, #12903, .F. ) ;
#95431 = AXIS2_PLACEMENT_3D ( 'NONE', #42718, #11393, #75612 ) ;
#95432 = CARTESIAN_POINT ( 'NONE',  ( 1.060314165523193353, 8.048081368953958759, -7.659344964962508051 ) ) ;
#95433 = CARTESIAN_POINT ( 'NONE',  ( -52.56483885390523625, -79.93083296558610584, -38.23529411764706509 ) ) ;
#95434 = ORIENTED_EDGE ( 'NONE', *, *, #84280, .F. ) ;
#95435 = FACE_BOUND ( 'NONE', #2896, .T. ) ;
#95436 = CARTESIAN_POINT ( 'NONE',  ( 5.000000000000000000, 0.000000000000000000, 35.66025403784438907 ) ) ;
#95437 = CARTESIAN_POINT ( 'NONE',  ( -92.69104981119035358, -60.00000000000001421, -9.101021654975044228 ) ) ;
#95438 = ORIENTED_EDGE ( 'NONE', *, *, #29544, .T. ) ;
#95439 = CARTESIAN_POINT ( 'NONE',  ( -38.81358894280271699, 485.1131561813180042, -4.191378885296423995 ) ) ;
#95440 = DIRECTION ( 'NONE',  ( -0.5735764363510494901, -0.8191520442889894671, 0.000000000000000000 ) ) ;
#95441 = CARTESIAN_POINT ( 'NONE',  ( -9.843481099141454749, 26.40795443846614532, -1.779148000612201574 ) ) ;
#95443 = CARTESIAN_POINT ( 'NONE',  ( 21.36650669486618881, 1.474610560812782335E-15, 0.000000000000000000 ) ) ;
#95442 = CARTESIAN_POINT ( 'NONE',  ( -1.469576158976823947E-15, -26.37499999999999645, 8.000000000000000000 ) ) ;
#95444 = CARTESIAN_POINT ( 'NONE',  ( -83.15922951428930787, -36.01117145647910434, 165.7727490414225997 ) ) ;
#95445 = ORIENTED_EDGE ( 'NONE', *, *, #17416, .T. ) ;
#95446 = CARTESIAN_POINT ( 'NONE',  ( -12.81923949848597566, -0.000000000000000000, -11.24494283603735667 ) ) ;
#95447 = ORIENTED_EDGE ( 'NONE', *, *, #7508, .F. ) ;
#95448 = EDGE_LOOP ( 'NONE', ( #29672, #6748, #2928, #97370, #32904 ) ) ;
#95449 = CARTESIAN_POINT ( 'NONE',  ( 32.09613187451483896, 439.8906214799515624, 23.54885978596032814 ) ) ;
#95450 = CARTESIAN_POINT ( 'NONE',  ( 29.34999999999999787, 1.533819458162526451E-15, 0.000000000000000000 ) ) ;
#95451 = LINE ( 'NONE', #53919, #65626 ) ;
#95452 = ORIENTED_EDGE ( 'NONE', *, *, #57569, .F. ) ;
#95453 =( GEOMETRIC_REPRESENTATION_CONTEXT ( 3 ) GLOBAL_UNCERTAINTY_ASSIGNED_CONTEXT ( ( #22237 ) ) GLOBAL_UNIT_ASSIGNED_CONTEXT ( ( #98513, #67755, #83396 ) ) REPRESENTATION_CONTEXT ( 'NONE', 'WORKASPACE' ) );
#95455 = CARTESIAN_POINT ( 'NONE',  ( 61.11682663846713837, 6.975173280561618775E-15, 0.000000000000000000 ) ) ;
#95454 = B_SPLINE_CURVE_WITH_KNOTS ( 'NONE', 3,
 ( #94197, #44593, #61306, #54233, #68874, #62375, #20366, #60261, #76939, #53207, #4658, #85587, #36532, #12727, #19821, #61848, #3595, #103352, #86127, #29500, #12199, #11123, #78007, #4124, #27917, #86657, #37053, #60780, #93669, #87173, #102821, #53729, #27381, #70455, #28982, #93129 ),
 .UNSPECIFIED., .F., .F.,
 ( 4, 2, 2, 2, 2, 2, 2, 2, 2, 2, 2, 2, 2, 2, 2, 2, 2, 4 ),
 ( 0.01291936762762759677, 0.01372441420841340881, 0.01452946078919922085, 0.01533450736998503289, 0.01613955395077084493, 0.01694460053155665696, 0.01774964711234246900, 0.01855469369312828104, 0.01935974027391408961, 0.02016478685469990165, 0.02096983343548571369, 0.02177488001627152572, 0.02257992659705733776, 0.02338497317784314633, 0.02419001975862895837, 0.02459254304902186439, 0.02499506633941477041, 0.02580011292020054428 ),
 .UNSPECIFIED. ) ;
#95456 = CARTESIAN_POINT ( 'NONE',  ( 42.33349330513380693, -4.000000000000000888, 4.898587196589416773E-16 ) ) ;
#95457 = CARTESIAN_POINT ( 'NONE',  ( -91.87475470944771416, -57.66094841159801376, -19.53952869114660373 ) ) ;
#95458 = CARTESIAN_POINT ( 'NONE',  ( 0.9999999999999940048, -50.00000000000000000, 101.0455488498966758 ) ) ;
#95459 = CARTESIAN_POINT ( 'NONE',  ( 0.000000000000000000, 0.000000000000000000, 0.000000000000000000 ) ) ;
#95460 = CARTESIAN_POINT ( 'NONE',  ( 31.36650669486618881, 1.474610560812782335E-15, 0.000000000000000000 ) ) ;
#95461 = CARTESIAN_POINT ( 'NONE',  ( -13.87407757772530736, -50.52807032218477445, 25.11348823608586400 ) ) ;
#95462 = CARTESIAN_POINT ( 'NONE',  ( -16.75187969033554936, 37.11970326878314097, -21.80698433968595751 ) ) ;
#95463 = CARTESIAN_POINT ( 'NONE',  ( 88.04031092259528180, -30.00000000000002842, -17.07720529721093072 ) ) ;
#95464 = CARTESIAN_POINT ( 'NONE',  ( -69.27297328317253289, -60.00000000000002132, 151.6304908672517513 ) ) ;
#95465 = CARTESIAN_POINT ( 'NONE',  ( -55.70695580102734112, -39.49968801934875984, 61.84876187497510358 ) ) ;
#95466 = ORIENTED_EDGE ( 'NONE', *, *, #21865, .F. ) ;
#95467 = CARTESIAN_POINT ( 'NONE',  ( 5.888319653649583429, 14.31359841374870712, -3.787045357069728446 ) ) ;
#95468 = ORIENTED_EDGE ( 'NONE', *, *, #2378, .F. ) ;
#95469 = CARTESIAN_POINT ( 'NONE',  ( -103.0193768792050122, -60.17265108286817821, 192.8001605453025888 ) ) ;
#95470 = CIRCLE ( 'NONE', #79986, 5.000000000000001776 ) ;
#95471 = APPLICATION_CONTEXT ( 'automotive_design' ) ;
#95472 = CARTESIAN_POINT ( 'NONE',  ( -1.218060163800027018, 51.81072258316640244, 8.677483100841660857 ) ) ;
#95473 = VERTEX_POINT ( 'NONE', #24977 ) ;
#95474 = CARTESIAN_POINT ( 'NONE',  ( 19.23821838457499922, 49.80979460016762062, 61.48217125059658628 ) ) ;
#95475 = CIRCLE ( 'NONE', #93714, 3.400000000000000355 ) ;
#95476 = PRESENTATION_STYLE_ASSIGNMENT (( #36225 ) ) ;
#95477 = CARTESIAN_POINT ( 'NONE',  ( 7.188101187500000044, -16.53125000204838813, 0.000000000000000000 ) ) ;
#95478 = CARTESIAN_POINT ( 'NONE',  ( -2.119141824078783376, -69.49710365781473342, 12.89375316341194377 ) ) ;
#95479 = PRESENTATION_STYLE_ASSIGNMENT (( #45354 ) ) ;
#95480 = CARTESIAN_POINT ( 'NONE',  ( -40.85254446136673323, 441.7500193615117610, 25.53625856138344474 ) ) ;
#95481 = CARTESIAN_POINT ( 'NONE',  ( -9.882987946621028641, 43.35715013040534416, -15.34374875303372576 ) ) ;
#95482 = DIRECTION ( 'NONE',  ( 0.000000000000000000, -0.7605354461462394688, 0.6492964154799720777 ) ) ;
#95483 = EDGE_CURVE ( 'NONE', #29729, #93035, #20769, .T. ) ;
#95484 = CARTESIAN_POINT ( 'NONE',  ( -38.81358894280271699, 485.1131561813180042, -4.191378885296423995 ) ) ;
#95485 = UNCERTAINTY_MEASURE_WITH_UNIT (LENGTH_MEASURE( 1.000000000000000082E-05 ), #56930, 'distance_accuracy_value', 'NONE');
#95486 = CARTESIAN_POINT ( 'NONE',  ( -28.03643574868016941, -56.86872177355682112, 35.51725734821072678 ) ) ;
#95487 = ADVANCED_FACE ( 'NONE', ( #19033 ), #24780, .T. ) ;
#95488 = ORIENTED_EDGE ( 'NONE', *, *, #98244, .T. ) ;
#95489 = EDGE_LOOP ( 'NONE', ( #97283, #101028, #78960, #69280 ) ) ;
#95490 = CARTESIAN_POINT ( 'NONE',  ( 47.55815791837702022, -60.27279555562992641, 53.32434900433165126 ) ) ;
#95491 = CARTESIAN_POINT ( 'NONE',  ( -0.1549862348970068859, 7.763683557544238667, 51.74239981364938501 ) ) ;
#95492 = CARTESIAN_POINT ( 'NONE',  ( -6.770548583014333488, 16.58437012435219415, -1.794845940801068629 ) ) ;
#95493 = EDGE_CURVE ( 'NONE', #3065, #8034, #38561, .T. ) ;
#95494 = CARTESIAN_POINT ( 'NONE',  ( -108.8780014184540050, -38.35654192929601436, 190.5193283876913881 ) ) ;
#95495 = ORIENTED_EDGE ( 'NONE', *, *, #86848, .F. ) ;
#95496 = CARTESIAN_POINT ( 'NONE',  ( 90.93050292392858580, -38.34431075332760486, 3.015154126244044441 ) ) ;
#95497 = CARTESIAN_POINT ( 'NONE',  ( 12.91023948886108030, 4.515193599548165793, -7.530818612190385508 ) ) ;
#95498 = DIRECTION ( 'NONE',  ( -1.000000000000000000, -1.224606353822377258E-16, -0.000000000000000000 ) ) ;
#95499 = DIRECTION ( 'NONE',  ( -1.000000000000000000, -1.224606353822377258E-16, -0.000000000000000000 ) ) ;
#95500 =( NAMED_UNIT ( * ) PLANE_ANGLE_UNIT ( ) SI_UNIT ( $, .RADIAN. ) );
#95501 = CARTESIAN_POINT ( 'NONE',  ( 5.308064239167483045, 41.67430808361709182, -70.56675995020944470 ) ) ;
#95502 = CARTESIAN_POINT ( 'NONE',  ( -33.72112513506057496, 434.9249801536511768, 12.79203885703619292 ) ) ;
#95503 = CARTESIAN_POINT ( 'NONE',  ( -33.00000000000002842, 489.5971041675260835, 10.80646835458717270 ) ) ;
#95504 = CARTESIAN_POINT ( 'NONE',  ( 12.49999999999999822, -4.999999999999999112, -11.21398294031200216 ) ) ;
#95505 = CARTESIAN_POINT ( 'NONE',  ( 87.01852956366043657, -60.00000000000000711, 201.0108315922142879 ) ) ;
#95506 = AXIS2_PLACEMENT_3D ( 'NONE', #40349, #51625, #34951 ) ;
#95507 = EDGE_CURVE ( 'NONE', #42044, #53428, #52309, .T. ) ;
#95508 = CIRCLE ( 'NONE', #48975, 5.000000000000011546 ) ;
#95509 = CARTESIAN_POINT ( 'NONE',  ( -16.58692244248932468, 34.28951775970666915, 24.30698433968612804 ) ) ;
#95510 = ORIENTED_EDGE ( 'NONE', *, *, #4977, .F. ) ;
#95511 = CARTESIAN_POINT ( 'NONE',  ( -32.16602296798976823, 298.8760903595368177, -9.110068575937141588 ) ) ;
#95512 = CARTESIAN_POINT ( 'NONE',  ( 7.414580834929598296, 32.64656280281481315, 3.010264818013836052 ) ) ;
#95513 = AXIS2_PLACEMENT_3D ( 'NONE', #104289, #29907, #55201 ) ;
#95514 = CIRCLE ( 'NONE', #38705, 5.000000000000010658 ) ;
#95515 = CARTESIAN_POINT ( 'NONE',  ( -7.046357527897572304, 28.69384349398995937, -3.789683693877204718 ) ) ;
#95516 = ORIENTED_EDGE ( 'NONE', *, *, #85584, .T. ) ;
#95518 = CARTESIAN_POINT ( 'NONE',  ( 38.09999999999998721, 0.000000000000000000, 0.000000000000000000 ) ) ;
#95517 = CARTESIAN_POINT ( 'NONE',  ( -103.4331137144314141, -38.42286339601668743, 198.8239305193790472 ) ) ;
#95519 = CARTESIAN_POINT ( 'NONE',  ( 1.224646799147355426E-15, -100.0000000000000000, 10.00000000000001954 ) ) ;
#95520 = CARTESIAN_POINT ( 'NONE',  ( 43.51084452654469459, 465.2903130129626561, 9.421687747985401984 ) ) ;
#95521 = PRESENTATION_STYLE_ASSIGNMENT (( #12460 ) ) ;
#95522 = CARTESIAN_POINT ( 'NONE',  ( 5.082755093536325930, -11.84375000204838635, -5.082755093536325042 ) ) ;
#95523 = CARTESIAN_POINT ( 'NONE',  ( 1.308996937480704670, -3.000000000000002665, -95.00000000000000000 ) ) ;
#95524 = CARTESIAN_POINT ( 'NONE',  ( 30.10126468112042986, 13.03072330106368781, -42.03538192853125111 ) ) ;
#95526 = VERTEX_POINT ( 'NONE', #12467 ) ;
#95525 = DIRECTION ( 'NONE',  ( 0.000000000000000000, 1.000000000000000000, 0.000000000000000000 ) ) ;
#95527 = CARTESIAN_POINT ( 'NONE',  ( 81.72320301993624980, -53.48224605584718461, 179.5177899479337214 ) ) ;
#95528 = CARTESIAN_POINT ( 'NONE',  ( 59.41111111111111143, 3.309500000000014541, 4.052968581778174646E-16 ) ) ;
#95529 = CARTESIAN_POINT ( 'NONE',  ( -36.85885249723667556, 438.9055665639564268, 23.87932036944819814 ) ) ;
#95530 = VERTEX_POINT ( 'NONE', #100959 ) ;
#95531 = CARTESIAN_POINT ( 'NONE',  ( -34.46322806571021147, 319.4038054108495999, -5.983482695349220393 ) ) ;
#95532 = DIRECTION ( 'NONE',  ( 0.000000000000000000, -1.000000000000000000, 0.000000000000000000 ) ) ;
#95533 = CARTESIAN_POINT ( 'NONE',  ( 62.33904886068935980, -1.232595164407830946E-29, 4.000000000000007105 ) ) ;
#95534 = CARTESIAN_POINT ( 'NONE',  ( 32.12566262182734533, 486.1613120233242853, 5.452106427430475577 ) ) ;
#95535 = DIRECTION ( 'NONE',  ( -1.000000000000000000, 0.000000000000000000, 0.000000000000000000 ) ) ;
#95536 = CARTESIAN_POINT ( 'NONE',  ( 0.000000000000000000, 37.86482112153536406, -10.52123582012688274 ) ) ;
#95537 = CONICAL_SURFACE ( 'NONE', #16536, 4.172000000000009479, 0.9599310885968813656 ) ;
#95538 = EDGE_LOOP ( 'NONE', ( #15993, #32509, #59525, #103972, #100687 ) ) ;
#95539 = EDGE_CURVE ( 'NONE', #25389, #11437, #38672, .T. ) ;
#95540 = VECTOR ( 'NONE', #87817, 1000.000000000000227 ) ;
#95541 = CARTESIAN_POINT ( 'NONE',  ( -4.551587301587297851, -48.79941684889506348, 104.4018401814738013 ) ) ;
#95542 = DIRECTION ( 'NONE',  ( 0.5564727496918437932, 0.8308658609248540383, -2.895979027895421214E-16 ) ) ;
#95543 = CARTESIAN_POINT ( 'NONE',  ( 80.97977184163765685, -2.002967142162725287E-29, 5.000000000000011546 ) ) ;
#95544 = EDGE_CURVE ( 'NONE', #56015, #96494, #19567, .T. ) ;
#95545 = EDGE_CURVE ( 'NONE', #11437, #26529, #94069, .T. ) ;
#95547 = CARTESIAN_POINT ( 'NONE',  ( -13.92884988672090607, 2.721025988440579191, -5.537286027112259035 ) ) ;
#95546 = DIRECTION ( 'NONE',  ( -0.000000000000000000, -0.000000000000000000, -1.000000000000000000 ) ) ;
#95548 = CARTESIAN_POINT ( 'NONE',  ( -5.082755093536326818, -19.71875000204838457, 5.082755093536325042 ) ) ;
#95549 = CARTESIAN_POINT ( 'NONE',  ( 9.970195021754619802, 302.6460196488382053, -10.04373974541431380 ) ) ;
#95550 = AXIS2_PLACEMENT_3D ( 'NONE', #53001, #3386, #17987 ) ;
#95551 = FACE_OUTER_BOUND ( 'NONE', #97458, .T. ) ;
#95552 = AXIS2_PLACEMENT_3D ( 'NONE', #59259, #18829, #92671 ) ;
#95553 = B_SPLINE_CURVE_WITH_KNOTS ( 'NONE', 3,
 ( #101581, #27741, #67628, #99974, #17487, #93503, #50350, #51422, #19649, #9897, #11485, #44411, #26145, #3420, #42265, #83262, #75158, #1249, #59001, #77839, #38458, #78885, #54061, #95096, #21755, #36362, #37415, #28801, #12024, #21233, #45486, #29322, #62213, #61683 ),
 .UNSPECIFIED., .F., .F.,
 ( 4, 2, 2, 2, 2, 2, 2, 2, 2, 2, 2, 2, 2, 2, 2, 2, 4 ),
 ( 0.5000000000000000000, 0.5312500000000000000, 0.5625000000000000000, 0.5937500000000000000, 0.6250000000000000000, 0.6562500000000000000, 0.6875000000000000000, 0.7187500000000000000, 0.7500000000000000000, 0.7812500000000000000, 0.8125000000000000000, 0.8437500000000000000, 0.8750000000000000000, 0.9062500000000000000, 0.9375000000000000000, 0.9687500000000000000, 1.000000000000000000 ),
 .UNSPECIFIED. ) ;
#95554 = MECHANICAL_DESIGN_GEOMETRIC_PRESENTATION_REPRESENTATION (  '', ( #55860 ), #83459 ) ;
#95555 = CONTEXT_DEPENDENT_SHAPE_REPRESENTATION ( #441, #29637 ) ;
#95556 = ORIENTED_EDGE ( 'NONE', *, *, #74241, .F. ) ;
#95557 = DIRECTION ( 'NONE',  ( -1.000000000000000000, -0.000000000000000000, -0.000000000000000000 ) ) ;
#95558 = DIRECTION ( 'NONE',  ( 0.000000000000000000, -1.000000000000000000, 0.000000000000000000 ) ) ;
#95559 = CIRCLE ( 'NONE', #5998, 3.400000000000000355 ) ;
#95560 = CARTESIAN_POINT ( 'NONE',  ( -8.240610721218175172, 35.73638292219670376, -5.000000000000000888 ) ) ;
#95561 =( BOUNDED_SURFACE ( )  B_SPLINE_SURFACE ( 3, 2, ( 
 ( #18716, #76372, #10580 ),
 ( #34373, #58618, #99584 ),
 ( #92565, #66160, #90444 ),
 ( #34901, #82347, #90987 ),
 ( #17098, #74772, #75854 ),
 ( #2483, #1948, #91519 ),
 ( #100124, #17635, #41355 ),
 ( #59151, #42962, #57523 ) ),
 .UNSPECIFIED., .F., .F., .T. ) 
 B_SPLINE_SURFACE_WITH_KNOTS ( ( 4, 2, 2, 4 ),
 ( 3, 3 ),
 ( 0.006812271038101275558, 0.007673844606673213380, 0.008535418175245151201, 0.01025856531238902858 ),
 ( 0.000000000000000000, 0.8457923845102014448 ),
 .UNSPECIFIED. ) 
 GEOMETRIC_REPRESENTATION_ITEM ( )  RATIONAL_B_SPLINE_SURFACE ( (
 ( 1.000000000000000000, 0.7678693572792288924, 0.9284073742078311486),
 ( 1.000000000000000000, 0.7757895751984035249, 0.9308500900467820971),
 ( 1.000000000000000000, 0.7815379911777921018, 0.9326229890888320107),
 ( 1.000000000000000000, 0.7881252992655237710, 0.9346546152342435354),
 ( 1.000000000000000000, 0.7889532766692782806, 0.9349099760764683076),
 ( 1.000000000000000000, 0.7842545691361754168, 0.9334608231073407980),
 ( 1.000000000000000000, 0.7715427182228143943, 0.9295402946717183923),
 ( 1.000000000000000000, 0.7522731460529035186, 0.9235972651200572425) ) ) 
 REPRESENTATION_ITEM ( '' )  SURFACE ( )  );
#95562 = CARTESIAN_POINT ( 'NONE',  ( 6.683837171061802529, 3.955946848495962787, 6.851900933636986935 ) ) ;
#95563 = ADVANCED_FACE ( 'NONE', ( #61593 ), #84785, .F. ) ;
#95564 = VERTEX_POINT ( 'NONE', #95021 ) ;
#95565 = CARTESIAN_POINT ( 'NONE',  ( 43.98625509876906392, 435.4996938134206630, 9.950854633800886972 ) ) ;
#95566 = DIRECTION ( 'NONE',  ( -1.000000000000000000, 0.000000000000000000, 0.000000000000000000 ) ) ;
#95567 = ORIENTED_EDGE ( 'NONE', *, *, #86341, .T. ) ;
#95568 = ADVANCED_FACE ( 'NONE', ( #27658, #43788 ), #53483, .F. ) ;
#95569 = CARTESIAN_POINT ( 'NONE',  ( -43.00000000000000000, 500.0000000000002274, -15.00000000000000711 ) ) ;
#95570 = CARTESIAN_POINT ( 'NONE',  ( -2.228836330356652073, -0.1847672526321134656, 102.4817230975930897 ) ) ;
#95571 = CARTESIAN_POINT ( 'NONE',  ( 6.831363830528337289, 41.73171983268898089, -59.17722554277374059 ) ) ;
#95572 = CARTESIAN_POINT ( 'NONE',  ( 18.86650669486618881, 4.000000000000003553, 4.898587196589414801E-16 ) ) ;
#95573 = UNCERTAINTY_MEASURE_WITH_UNIT (LENGTH_MEASURE( 1.000000000000000082E-05 ), #60464, 'distance_accuracy_value', 'NONE');
#95574 = CARTESIAN_POINT ( 'NONE',  ( -109.2006123233502137, -59.99999999999999289, 137.4141054976637975 ) ) ;
#95575 = CARTESIAN_POINT ( 'NONE',  ( 94.26467260280679739, -2.002967142162725287E-29, 5.000000000000011546 ) ) ;
#95576 = CARTESIAN_POINT ( 'NONE',  ( 5.978033218201109555, 4.054134411712192687, -0.5602453477493177791 ) ) ;
#95577 = CARTESIAN_POINT ( 'NONE',  ( 0.000000000000000000, 0.000000000000000000, -8.000000000000000000 ) ) ;
#95578 = EDGE_CURVE ( 'NONE', #57692, #64733, #44330, .T. ) ;
#95579 = CARTESIAN_POINT ( 'NONE',  ( 3.006829104376306210E-15, 38.19193163660327173, -24.55262289886175964 ) ) ;
#95580 = CARTESIAN_POINT ( 'NONE',  ( -82.47186679091046813, -60.82202273473512122, 189.3326345159165953 ) ) ;
#95581 = CARTESIAN_POINT ( 'NONE',  ( 39.05849473363845448, 42.03646466411915839, -56.80344740562036066 ) ) ;
#95582 = COLOUR_RGB ( '', 0.09019608, 0.27058824, 0.51372549) ;
#95583 = ORIENTED_EDGE ( 'NONE', *, *, #70960, .T. ) ;
#95584 = CARTESIAN_POINT ( 'NONE',  ( 4.250000000000000000, 0.000000000000000000, -7.657127082228716297 ) ) ;
#95585 = DIRECTION ( 'NONE',  ( -1.000000000000000000, -1.224606353822377258E-16, -0.000000000000000000 ) ) ;
#95586 = PRODUCT_DEFINITION_FORMATION_WITH_SPECIFIED_SOURCE ( 'ANY', '', #53642, .NOT_KNOWN. ) ;
#95587 = CARTESIAN_POINT ( 'NONE',  ( -83.90290634939050562, -45.26542921300821831, 21.05896802600032913 ) ) ;
#95588 = CARTESIAN_POINT ( 'NONE',  ( -32.28930913497458022, 488.2717154064632723, 9.213726894912692700 ) ) ;
#95589 = CARTESIAN_POINT ( 'NONE',  ( -2.942719846374528547, 97.39685729185900698, -5.000000000000000000 ) ) ;
#95590 = CARTESIAN_POINT ( 'NONE',  ( 8.441095186813715401, 123.9902009031610817, 0.000000000000000000 ) ) ;
#95591 = DIRECTION ( 'NONE',  ( 0.000000000000000000, 0.000000000000000000, 1.000000000000000000 ) ) ;
#95592 = CARTESIAN_POINT ( 'NONE',  ( -5.022013495247517945, 18.64316884711714195, -38.36535705883633085 ) ) ;
#95593 = CARTESIAN_POINT ( 'NONE',  ( 82.63356161194110427, -60.00000000000014921, 201.7055385233423976 ) ) ;
#95594 = CARTESIAN_POINT ( 'NONE',  ( -103.2977232915219048, -14.21045842199428577, 133.3115090881459253 ) ) ;
#95595 = CARTESIAN_POINT ( 'NONE',  ( -63.04233670341422169, -60.34557740310773966, 91.29213200275268036 ) ) ;
#95596 = ORIENTED_EDGE ( 'NONE', *, *, #17815, .T. ) ;
#95597 = CARTESIAN_POINT ( 'NONE',  ( 59.27210092795512253, 39.42463516292936276, 26.84561385324717264 ) ) ;
#95598 = CARTESIAN_POINT ( 'NONE',  ( 99.19415962822883159, -60.00000000000739675, 204.5929917445554338 ) ) ;
#95599 = ORIENTED_EDGE ( 'NONE', *, *, #4590, .F. ) ;
#95600 = DIRECTION ( 'NONE',  ( -0.5735764363510459374, -0.8191520442889919096, 0.000000000000000000 ) ) ;
#95601 = CARTESIAN_POINT ( 'NONE',  ( -7.188101187500000933, -20.37500000204838813, -2.977408999572651371 ) ) ;
#95602 = ORIENTED_EDGE ( 'NONE', *, *, #33990, .F. ) ;
#95603 = CARTESIAN_POINT ( 'NONE',  ( -11.53061943269021050, 45.53913102596384022, 13.95708208482078483 ) ) ;
#95604 = ORIENTED_EDGE ( 'NONE', *, *, #64618, .T. ) ;
#95605 = CARTESIAN_POINT ( 'NONE',  ( 10.45288716919446692, 45.35420570811798058, -15.39944944803840698 ) ) ;
#95606 = CARTESIAN_POINT ( 'NONE',  ( -42.19179521602280403, 485.4956273777414708, -3.824025998168937512 ) ) ;
#95607 = CARTESIAN_POINT ( 'NONE',  ( -63.47509362114410436, -60.00000000000000000, -34.70012741899613218 ) ) ;
#95608 = CARTESIAN_POINT ( 'NONE',  ( 34.94142348598472125, 329.2055239765263650, -3.785525783732882399 ) ) ;
#95609 = CARTESIAN_POINT ( 'NONE',  ( -7.188101187500002709, -32.18750000204838813, 2.977408999572648707 ) ) ;
#95610 = CARTESIAN_POINT ( 'NONE',  ( 32.82264240587376491, 485.2608142494332242, 5.823360857566779458 ) ) ;
#95611 = CARTESIAN_POINT ( 'NONE',  ( 20.11650669486618881, 1.474610560812782335E-15, 0.000000000000000000 ) ) ;
#95612 = CARTESIAN_POINT ( 'NONE',  ( 1.000000000000000000, -63.35320086167136822, 9.447768535959317759 ) ) ;
#95613 = CARTESIAN_POINT ( 'NONE',  ( 8.737863884124120517, 49.99999999999999289, -90.03618980230058355 ) ) ;
#95614 = CARTESIAN_POINT ( 'NONE',  ( -6.928203230275507885, 105.0000000000000000, -4.000000000000001776 ) ) ;
#95615 = DIRECTION ( 'NONE',  ( 0.000000000000000000, 0.000000000000000000, 1.000000000000000000 ) ) ;
#95616 = EDGE_CURVE ( 'NONE', #2324, #103314, #15533, .T. ) ;
#95617 = CIRCLE ( 'NONE', #33642, 4.000000000000001776 ) ;
#95618 = CARTESIAN_POINT ( 'NONE',  ( 101.1017039263183221, -60.00000000000007816, 195.0041137791595531 ) ) ;
#95619 = ORIENTED_EDGE ( 'NONE', *, *, #70232, .T. ) ;
#95620 = CARTESIAN_POINT ( 'NONE',  ( -9.560175649466449599, 53.41719017493603872, -3.548455548004890936 ) ) ;
#95621 = CARTESIAN_POINT ( 'NONE',  ( 35.65037063887645274, -36.04038755283193041, 35.00118258462216403 ) ) ;
#95622 = AXIS2_PLACEMENT_3D ( 'NONE', #32238, #80760, #73184 ) ;
#95623 = CARTESIAN_POINT ( 'NONE',  ( -21.65942590380950605, 4.828984019150144164E-12, 5.820808985950977288 ) ) ;
#95624 = ORIENTED_EDGE ( 'NONE', *, *, #77037, .T. ) ;
#95625 = EDGE_CURVE ( 'NONE', #30642, #44793, #88519, .T. ) ;
#95626 = FACE_OUTER_BOUND ( 'NONE', #8001, .T. ) ;
#95627 = EDGE_CURVE ( 'NONE', #1638, #23889, #84512, .T. ) ;
#95628 = CIRCLE ( 'NONE', #98979, 3.400000000000000355 ) ;
#95629 = ORIENTED_EDGE ( 'NONE', *, *, #78625, .T. ) ;
#95631 = CARTESIAN_POINT ( 'NONE',  ( -35.44563196690202744, 355.0508310518326311, 1.542887188955126110 ) ) ;
#95630 = CARTESIAN_POINT ( 'NONE',  ( 0.000000000000000000, 80.00000000000000000, -10.00000000000000000 ) ) ;
#95632 = DIRECTION ( 'NONE',  ( -0.000000000000000000, -0.000000000000000000, 1.000000000000000000 ) ) ;
#95633 = DIRECTION ( 'NONE',  ( 0.5735764363510440500, 0.8191520442889932418, 0.000000000000000000 ) ) ;
#95634 = AXIS2_PLACEMENT_3D ( 'NONE', #30950, #31995, #13654 ) ;
#95635 = MECHANICAL_DESIGN_GEOMETRIC_PRESENTATION_REPRESENTATION (  '', ( #74965 ), #14686 ) ;
#95636 = DIRECTION ( 'NONE',  ( 0.000000000000000000, 0.000000000000000000, 1.000000000000000000 ) ) ;
#95637 = VECTOR ( 'NONE', #80037, 1000.000000000000000 ) ;
#95638 = CARTESIAN_POINT ( 'NONE',  ( 0.5805565836007616776, 3.752776749732562589, -6.500000000000000888 ) ) ;
#95639 = CARTESIAN_POINT ( 'NONE',  ( 66.00571552735603120, 6.975173280561618775E-15, 0.000000000000000000 ) ) ;
#95640 = EDGE_LOOP ( 'NONE', ( #67674, #51103, #84688, #85089, #54985 ) ) ;
#95641 = CARTESIAN_POINT ( 'NONE',  ( 100.7204764832770536, -60.00000000000001421, 85.25963890312766580 ) ) ;
#95642 = AXIS2_PLACEMENT_3D ( 'NONE', #38333, #23205, #71194 ) ;
#95643 = DIRECTION ( 'NONE',  ( 0.5735764363510468256, 0.8191520442889913545, 0.000000000000000000 ) ) ;
#95644 = ADVANCED_FACE ( 'NONE', ( #29766 ), #79874, .T. ) ;
#95645 = ADVANCED_FACE ( 'NONE', ( #31872 ), #67395, .F. ) ;
#95646 = AXIS2_PLACEMENT_3D ( 'NONE', #72317, #89038, #105737 ) ;
#95647 = DIRECTION ( 'NONE',  ( -1.000000000000000000, -0.000000000000000000, -0.000000000000000000 ) ) ;
#95648 = CARTESIAN_POINT ( 'NONE',  ( -12.25900440697833993, 17.71059303037062449, -8.828067291959920126 ) ) ;
#95649 = VERTEX_POINT ( 'NONE', #33464 ) ;
#95650 = CARTESIAN_POINT ( 'NONE',  ( -90.07223913452511965, -30.00000000002903988, -8.398832610232158657 ) ) ;
#95651 = ORIENTED_EDGE ( 'NONE', *, *, #23726, .F. ) ;
#95652 = DIRECTION ( 'NONE',  ( 0.000000000000000000, 0.000000000000000000, 1.000000000000000000 ) ) ;
#95653 = DIRECTION ( 'NONE',  ( 0.000000000000000000, -0.9221233147934838614, -0.3868961001538753219 ) ) ;
#95654 = CARTESIAN_POINT ( 'NONE',  ( -6.500000000000000888, 0.000000000000000000, 1.734723475976807094E-15 ) ) ;
#95655 = CARTESIAN_POINT ( 'NONE',  ( 2.977408999572650927, -34.25000000204838813, -7.188101187500001821 ) ) ;
#95656 = LINE ( 'NONE', #87568, #17435 ) ;
#95657 = DIRECTION ( 'NONE',  ( -1.000000000000000000, -1.224606353822377258E-16, -0.000000000000000000 ) ) ;
#95658 = CARTESIAN_POINT ( 'NONE',  ( 28.99999999999999645, 0.000000000000000000, -4.999999999999999112 ) ) ;
#95659 = EDGE_LOOP ( 'NONE', ( #8475, #5235, #45050, #14485, #17923, #80115 ) ) ;
#95661 = ORIENTED_EDGE ( 'NONE', *, *, #24679, .F. ) ;
#95660 = CARTESIAN_POINT ( 'NONE',  ( 0.000000000000000000, 0.000000000000000000, -9.274828571428571422 ) ) ;
#95662 = CARTESIAN_POINT ( 'NONE',  ( 80.34687235150721563, -36.02841022270869331, 144.2383497923063658 ) ) ;
#95663 = FILL_AREA_STYLE_COLOUR ( '', #31634 ) ;
#95664 = ORIENTED_EDGE ( 'NONE', *, *, #45147, .T. ) ;
#95665 = CARTESIAN_POINT ( 'NONE',  ( -12.50000000000000711, 39.72072293383548214, -64.90088073866644436 ) ) ;
#95666 = CARTESIAN_POINT ( 'NONE',  ( -5.082755093536326818, -19.71875000204838457, 5.082755093536325042 ) ) ;
#95667 = AXIS2_PLACEMENT_3D ( 'NONE', #645, #51888, #10367 ) ;
#95668 = CARTESIAN_POINT ( 'NONE',  ( -74.02244645645996002, -57.61166141858229395, 187.2311674206319765 ) ) ;
#95669 = CARTESIAN_POINT ( 'NONE',  ( 85.31310517497098544, -5.000000000000000888, 6.123233995736779101E-16 ) ) ;
#95670 = ORIENTED_EDGE ( 'NONE', *, *, #18487, .F. ) ;
#95671 = CARTESIAN_POINT ( 'NONE',  ( -4.903871675326606727, -12.02085807301495457, -3.461400506969853907 ) ) ;
#95672 = CARTESIAN_POINT ( 'NONE',  ( -9.797372177749751998, 81.53490505152436185, 2.014953862275846497 ) ) ;
#95673 = EDGE_CURVE ( 'NONE', #17049, #7599, #41997, .T. ) ;
#95674 = CARTESIAN_POINT ( 'NONE',  ( 0.000000000000000000, 27.68727484027578356, -33.82893434829263413 ) ) ;
#95675 = CARTESIAN_POINT ( 'NONE',  ( -5.656854249492381470, -11.75000000409677092, 5.656854249492379694 ) ) ;
#95676 = DIRECTION ( 'NONE',  ( 0.000000000000000000, 0.000000000000000000, 1.000000000000000000 ) ) ;
#95677 = CARTESIAN_POINT ( 'NONE',  ( -46.00000000000004263, 486.8231468695061039, 5.689692765235337291 ) ) ;
#95678 = EDGE_CURVE ( 'NONE', #66787, #4323, #78404, .T. ) ;
#95679 = CARTESIAN_POINT ( 'NONE',  ( -37.62251730745840916, 437.3427388312646258, 4.535622330043208805 ) ) ;
#95680 = FILL_AREA_STYLE ('',( #30438 ) ) ;
#95681 = AXIS2_PLACEMENT_3D ( 'NONE', #81591, #40104, #96754 ) ;
#95682 = DIRECTION ( 'NONE',  ( 0.3957342950827466566, 0.000000000000000000, 0.9183650514339936066 ) ) ;
#95683 = CARTESIAN_POINT ( 'NONE',  ( 37.88764991246872427, 27.49831504271226734, 13.42506037026353738 ) ) ;
#95684 = ORIENTED_EDGE ( 'NONE', *, *, #36235, .T. ) ;
#95685 = CARTESIAN_POINT ( 'NONE',  ( -1.432938875184908145, -50.02820789671614676, 40.96157042262397852 ) ) ;
#95686 = CARTESIAN_POINT ( 'NONE',  ( -1.544939622599249551, 15.00000000000000000, 9.999999999999998224 ) ) ;
#95687 = CARTESIAN_POINT ( 'NONE',  ( -4.000000000000000000, 17.85270131633358659, -5.744562646538044604 ) ) ;
#95688 = CARTESIAN_POINT ( 'NONE',  ( -27.26849945976038114, -20.79577116979002227, -32.65558008730316431 ) ) ;
#95689 = CARTESIAN_POINT ( 'NONE',  ( -82.88436837210520025, -29.99999999999999645, 152.0600583881144132 ) ) ;
#95690 = DIRECTION ( 'NONE',  ( 0.000000000000000000, -1.000000000000000000, 0.000000000000000000 ) ) ;
#95691 = VECTOR ( 'NONE', #10201, 1000.000000000000000 ) ;
#95692 = ORIENTED_EDGE ( 'NONE', *, *, #83882, .T. ) ;
#95693 = DIRECTION ( 'NONE',  ( -0.5735764363510461594, 0.8191520442889916875, 1.003171929053524870E-16 ) ) ;
#95694 = VECTOR ( 'NONE', #42960, 1000.000000000000000 ) ;
#95695 = CARTESIAN_POINT ( 'NONE',  ( 91.17736083037920025, -57.61337127814945802, 204.2034886438755166 ) ) ;
#95696 = CIRCLE ( 'NONE', #49167, 4.000000000000007105 ) ;
#95697 = CARTESIAN_POINT ( 'NONE',  ( 59.86708669470515787, -21.77003396638972532, -23.08968796104069909 ) ) ;
#95698 = EDGE_CURVE ( 'NONE', #25329, #1155, #100513, .T. ) ;
#95699 = CARTESIAN_POINT ( 'NONE',  ( -10.00000000000000355, 105.0000000000000000, 4.000000000000001776 ) ) ;
#95700 = CARTESIAN_POINT ( 'NONE',  ( -15.79785611713298366, 22.78916061418441075, -0.5147589528978404605 ) ) ;
#95701 = MECHANICAL_DESIGN_GEOMETRIC_PRESENTATION_REPRESENTATION (  '', ( #2601 ), #880 ) ;
#95702 = CARTESIAN_POINT ( 'NONE',  ( 7.996668423981797780, -3.000000000000003109, -78.85453280025085121 ) ) ;
#95703 = CARTESIAN_POINT ( 'NONE',  ( -53.48817481113404426, -59.99999999999999289, 80.99915126202921556 ) ) ;
#95704 = CIRCLE ( 'NONE', #12991, 1.000000000000000000 ) ;
#95705 = AXIS2_PLACEMENT_3D ( 'NONE', #15843, #48725, #81614 ) ;
#95706 = FACE_OUTER_BOUND ( 'NONE', #29711, .T. ) ;
#95707 = DIRECTION ( 'NONE',  ( -0.000000000000000000, -1.000000000000000000, -0.000000000000000000 ) ) ;
#95708 = EDGE_CURVE ( 'NONE', #39859, #55434, #64358, .T. ) ;
#95709 = CARTESIAN_POINT ( 'NONE',  ( -62.59524157943269529, 48.00000000000000000, 18.50207713769755102 ) ) ;
#95710 = CARTESIAN_POINT ( 'NONE',  ( -85.68467769695706693, -39.26620762603923254, 186.0355029637988480 ) ) ;
#95711 = ORIENTED_EDGE ( 'NONE', *, *, #90266, .F. ) ;
#95712 = CARTESIAN_POINT ( 'NONE',  ( 32.40217524501196777, 319.2284543538688126, -6.509870530067201067 ) ) ;
#95713 = CARTESIAN_POINT ( 'NONE',  ( -3.373226601126230406, 304.8518027749948374, -9.000000000275649725 ) ) ;
#95714 = AXIS2_PLACEMENT_3D ( 'NONE', #64890, #97252, #48158 ) ;
#95715 = CARTESIAN_POINT ( 'NONE',  ( 71.14984002819953446, -4.000000000000000000, 0.000000000000000000 ) ) ;
#95716 = B_SPLINE_CURVE_WITH_KNOTS ( 'NONE', 3,
 ( #22940, #63398, #104903, #105423, #21886, #23471, #71991, #39648, #31041, #15344, #63921, #56307, #96809, #40150, #81133, #6180, #55777, #31563 ),
 .UNSPECIFIED., .F., .F.,
 ( 4, 2, 2, 2, 2, 2, 2, 2, 4 ),
 ( 0.002442598131820562096, 0.002946487642774274582, 0.003198432398251129308, 0.003450377153727984467, 0.004458156175635422450, 0.004962045686589144043, 0.005465935197542866504, 0.005969824708496588965, 0.006473714219450311426 ),
 .UNSPECIFIED. ) ;
#95717 = CARTESIAN_POINT ( 'NONE',  ( -30.57762908964539506, 310.6565871460678636, -8.419674958802174203 ) ) ;
#95718 = CARTESIAN_POINT ( 'NONE',  ( -84.35224106894892770, -60.17954417897186659, -17.01416247631696166 ) ) ;
#95719 = CARTESIAN_POINT ( 'NONE',  ( -16.14595037822616419, 12.99999999999999289, 8.749999999999921840 ) ) ;
#95720 = ORIENTED_EDGE ( 'NONE', *, *, #89709, .F. ) ;
#95721 = CARTESIAN_POINT ( 'NONE',  ( 18.79996295430579423, 50.00000000000000711, 60.85687850329983206 ) ) ;
#95722 = CARTESIAN_POINT ( 'NONE',  ( 11.37917810246435657, 20.25992464176842489, 8.251280100175593546 ) ) ;
#95723 = CARTESIAN_POINT ( 'NONE',  ( 3.088855081073062209E-15, -4.285714285714286476, 25.22241582816893413 ) ) ;
#95724 = DIRECTION ( 'NONE',  ( -1.000000000000000000, -1.224606353822377258E-16, -0.000000000000000000 ) ) ;
#95725 = CARTESIAN_POINT ( 'NONE',  ( 86.58362542449755495, -60.00000000000002132, -26.27920600484676683 ) ) ;
#95726 = CARTESIAN_POINT ( 'NONE',  ( -77.55089032165899710, -49.90769110663840991, 141.6289234985631538 ) ) ;
#95727 = PRODUCT_DEFINITION ( 'UNKNOWN', '', #78326, #74761 ) ;
#95728 = VERTEX_POINT ( 'NONE', #25388 ) ;
#95729 = FILL_AREA_STYLE ('',( #36995 ) ) ;
#95730 = CARTESIAN_POINT ( 'NONE',  ( -4.464296094009082339, -13.01099471650159956, -12.88508357975250185 ) ) ;
#95731 = CARTESIAN_POINT ( 'NONE',  ( 79.56404080552624691, -57.50631293715987624, 198.4392659916153150 ) ) ;
#95732 = CARTESIAN_POINT ( 'NONE',  ( 53.14262477155799758, 49.99999999999999289, 33.99861374406009418 ) ) ;
#95733 = CARTESIAN_POINT ( 'NONE',  ( 35.93223276062541061, 303.8771570922352225, 0.07619417529777239295 ) ) ;
#95734 = DIRECTION ( 'NONE',  ( 0.000000000000000000, 0.000000000000000000, 1.000000000000000000 ) ) ;
#95735 = ORIENTED_EDGE ( 'NONE', *, *, #119, .T. ) ;
#95736 = DIRECTION ( 'NONE',  ( 1.000000000000000000, 0.000000000000000000, -0.000000000000000000 ) ) ;
#95737 = CARTESIAN_POINT ( 'NONE',  ( 31.33625191410321875, 438.2398020556285019, 22.62030528329812995 ) ) ;
#95738 = CYLINDRICAL_SURFACE ( 'NONE', #98363, 4.000000000000000000 ) ;
#95739 = CARTESIAN_POINT ( 'NONE',  ( 4.401442555609581635E-16, -23.28125000204838457, -7.188101187500000044 ) ) ;
#95740 = ORIENTED_EDGE ( 'NONE', *, *, #102003, .F. ) ;
#95741 = DIRECTION ( 'NONE',  ( -1.000000000000000000, -1.224606353822377258E-16, -0.000000000000000000 ) ) ;
#95742 = AXIS2_PLACEMENT_3D ( 'NONE', #65170, #96490, #63058 ) ;
#95743 = CARTESIAN_POINT ( 'NONE',  ( -1.469576158976823947E-15, -25.06250000409677270, 8.000000000000000000 ) ) ;
#95744 = DIRECTION ( 'NONE',  ( -0.000000000000000000, -1.000000000000000000, -0.000000000000000000 ) ) ;
#95745 = DIRECTION ( 'NONE',  ( 0.000000000000000000, -1.000000000000000000, 0.000000000000000000 ) ) ;
#95746 = CARTESIAN_POINT ( 'NONE',  ( 0.000000000000000000, 0.000000000000000000, 0.000000000000000000 ) ) ;
#95747 = CARTESIAN_POINT ( 'NONE',  ( 17.58429050390567383, 43.20947028070973772, -6.235027717422475746 ) ) ;
#95748 = VERTEX_POINT ( 'NONE', #58244 ) ;
#95749 = CARTESIAN_POINT ( 'NONE',  ( 43.86555507694461653, 486.1044689237371017, 5.341991804865976690 ) ) ;
#95751 = CARTESIAN_POINT ( 'NONE',  ( 26.10287486467459317, -39.47800315929696779, 32.00527294968382819 ) ) ;
#95750 = CARTESIAN_POINT ( 'NONE',  ( -66.01875947964627755, -14.21045842199442077, 101.7785962432973292 ) ) ;
#95752 = CARTESIAN_POINT ( 'NONE',  ( 24.32770621568436198, 27.33676458719045854, -32.55389746325929679 ) ) ;
#95753 = ORIENTED_EDGE ( 'NONE', *, *, #91531, .T. ) ;
#95754 = EDGE_CURVE ( 'NONE', #24684, #73958, #91693, .T. ) ;
#95755 = B_SPLINE_CURVE_WITH_KNOTS ( 'NONE', 3,
 ( #8648, #26475, #49637, #74436, #43156, #34030, #76038, #515, #99787, #58817, #53373, #79231, #28070, #87341, #45289, #85203, #69038, #78167, #29662, #77650, #61479, #29146, #5357, #27544, #62532, #102985, #4818, #78686, #44220, #53885, #37755, #94372, #101912, #70618, #44761, #3227, #85758, #38277, #28596, #103509, #52292, #77112, #95418, #13417, #21558, #62016, #94912, #71137 ),
 .UNSPECIFIED., .F., .F.,
 ( 4, 2, 2, 2, 2, 2, 2, 2, 2, 2, 2, 2, 2, 2, 2, 2, 2, 2, 2, 2, 2, 2, 2, 4 ),
 ( -5.999999999093525979E-08, 0.002372776880890837756, 0.004745613761781666481, 0.009491287523563323933, 0.01067770596400873830, 0.01186412440445415092, 0.01423696128534487210, 0.01660979816623559674, 0.01898263504712631444, 0.02135547192801703908, 0.02372830880890775679, 0.02610114568979847449, 0.02847398257068919220, 0.03321965633247064148, 0.03796533009425209076, 0.04745667761781514199, 0.05694802514137819321, 0.06643937266494123750, 0.07593072018850428873, 0.08542206771206733995, 0.09491341523563037730, 0.1138961102827564797, 0.1328788053298826100, 0.1518615003770086846 ),
 .UNSPECIFIED. ) ;
#95756 = UNCERTAINTY_MEASURE_WITH_UNIT (LENGTH_MEASURE( 1.000000000000000082E-05 ), #21727, 'distance_accuracy_value', 'NONE');
#95757 = VERTEX_POINT ( 'NONE', #17805 ) ;
#95758 = CARTESIAN_POINT ( 'NONE',  ( -21.88880945939638067, -4.285714285714295357, -12.64023069600375138 ) ) ;
#95759 = CARTESIAN_POINT ( 'NONE',  ( 1.714505518806292863E-15, 60.00000000000000000, -6.999999999999992895 ) ) ;
#95760 =( LENGTH_UNIT ( ) NAMED_UNIT ( * ) SI_UNIT ( .MILLI., .METRE. ) );
#95761 = CARTESIAN_POINT ( 'NONE',  ( -0.08502184264844901695, 51.26930509877139031, -10.25000000000000000 ) ) ;
#95762 = PRESENTATION_STYLE_ASSIGNMENT (( #23489 ) ) ;
#95763 = CARTESIAN_POINT ( 'NONE',  ( 0.1551999952495689006, 18.85523120475384573, -49.25760693525473499 ) ) ;
#95764 = EDGE_LOOP ( 'NONE', ( #53264, #10183, #57416, #72144 ) ) ;
#95765 = B_SPLINE_CURVE_WITH_KNOTS ( 'NONE', 3,
 ( #26520, #57755, #92253, #75552, #50722, #17869, #18408, #90682, #58858, #58306, #33522, #83634, #75003, #1647, #34608, #9209, #43194, #2180, #51263, #84187, #1098, #10282 ),
 .UNSPECIFIED., .F., .F.,
 ( 4, 2, 2, 2, 2, 2, 2, 2, 2, 2, 4 ),
 ( 0.007303875631389625950, 0.007555818938590126363, 0.007807762245790625909, 0.008311648860191622398, 0.008815535474592619755, 0.009319422088993615377, 0.009823308703394612734, 0.01032719531779561009, 0.01083108193219660571, 0.01108302523939710613, 0.01133496854659760480 ),
 .UNSPECIFIED. ) ;
#95766 = SURFACE_SIDE_STYLE ('',( #26420 ) ) ;
#95767 = PRESENTATION_LAYER_ASSIGNMENT (  '', '', ( #42389 ) ) ;
#95768 = CARTESIAN_POINT ( 'NONE',  ( 53.08934989192468379, -29.99999999999999289, 52.21148837440650681 ) ) ;
#95769 = CARTESIAN_POINT ( 'NONE',  ( -13.51397627351688513, 24.63143318842911356, 1.638057307426889597 ) ) ;
#95770 = DIRECTION ( 'NONE',  ( -1.000000000000000000, -0.000000000000000000, -0.000000000000000000 ) ) ;
#95771 = EDGE_CURVE ( 'NONE', #8828, #40203, #7555, .T. ) ;
#95772 = CARTESIAN_POINT ( 'NONE',  ( 81.13063282006866928, -30.00000000000000711, 1.952550465599699470 ) ) ;
#95773 = EDGE_CURVE ( 'NONE', #76782, #85296, #105665, .T. ) ;
#95774 = CARTESIAN_POINT ( 'NONE',  ( 19.00000000000000711, 4.000000000000000000, -2.500000000000000000 ) ) ;
#95775 = ORIENTED_EDGE ( 'NONE', *, *, #95493, .T. ) ;
#95776 = AXIS2_PLACEMENT_3D ( 'NONE', #27924, #85596, #60790 ) ;
#95777 = ORIENTED_EDGE ( 'NONE', *, *, #77722, .T. ) ;
#95778 = ORIENTED_EDGE ( 'NONE', *, *, #15458, .T. ) ;
#95779 = CARTESIAN_POINT ( 'NONE',  ( -20.00000000000000000, 12.99999999999999289, 0.000000000000000000 ) ) ;
#95780 = FILL_AREA_STYLE ('',( #103341 ) ) ;
#95781 = CARTESIAN_POINT ( 'NONE',  ( 1.128077836147720614, 302.8478239976497548, 9.936168295454386623 ) ) ;
#95782 = CIRCLE ( 'NONE', #57617, 5.000000000000001776 ) ;
#95783 = FACE_OUTER_BOUND ( 'NONE', #106230, .T. ) ;
#95784 = CARTESIAN_POINT ( 'NONE',  ( -1.184166769438234956, -69.62625514036700736, 12.78541671988950945 ) ) ;
#95785 = CARTESIAN_POINT ( 'NONE',  ( 0.5805565836007616776, 3.752776749732562589, -6.500000000000000888 ) ) ;
#95786 = ORIENTED_EDGE ( 'NONE', *, *, #29786, .F. ) ;
#95787 = CARTESIAN_POINT ( 'NONE',  ( 7.996668422911924701, 48.00000000000000000, -91.14546720081904141 ) ) ;
#95788 = ORIENTED_EDGE ( 'NONE', *, *, #24359, .F. ) ;
#95789 = CYLINDRICAL_SURFACE ( 'NONE', #36447, 1.250000000000001110 ) ;
#95790 = DIRECTION ( 'NONE',  ( 0.000000000000000000, -1.000000000000000000, 0.000000000000000000 ) ) ;
#95791 = DIRECTION ( 'NONE',  ( 0.8191520442889884679, 0.000000000000000000, 0.5735764363510509334 ) ) ;
#95792 = AXIS2_PLACEMENT_3D ( 'NONE', #60844, #21985, #13851 ) ;
#95793 = CIRCLE ( 'NONE', #28598, 0.5000000000000004441 ) ;
#95794 = AXIS2_PLACEMENT_3D ( 'NONE', #41080, #56163, #89105 ) ;
#95795 = AXIS2_PLACEMENT_3D ( 'NONE', #103932, #68539, #85238 ) ;
#95796 = CARTESIAN_POINT ( 'NONE',  ( 2.289784721614370078, 298.7146547035764570, -10.00340817433579943 ) ) ;
#95798 = CARTESIAN_POINT ( 'NONE',  ( 63.73364275548575364, -22.10444409302240132, 73.75141016224915802 ) ) ;
#95797 = PRODUCT_DEFINITION_SHAPE ( 'NONE', 'NONE',  #17933 ) ;
#95799 = EDGE_LOOP ( 'NONE', ( #24692, #68556, #45759 ) ) ;
#95800 = LINE ( 'NONE', #103870, #84067 ) ;
#95801 = MECHANICAL_DESIGN_GEOMETRIC_PRESENTATION_REPRESENTATION (  '', ( #52733 ), #75122 ) ;
#95802 = CARTESIAN_POINT ( 'NONE',  ( 16.64348903516512834, 45.60392139269950462, -6.657797401561770911 ) ) ;
#95803 = CARTESIAN_POINT ( 'NONE',  ( -5.744562646538031281, 12.73020740600051148, -4.000000000000000888 ) ) ;
#95804 = DIRECTION ( 'NONE',  ( -1.000000000000000000, -0.000000000000000000, -0.000000000000000000 ) ) ;
#95805 = VERTEX_POINT ( 'NONE', #40469 ) ;
#95806 = B_SPLINE_CURVE_WITH_KNOTS ( 'NONE', 3,
 ( #70893, #52571, #3508, #36448, #69315, #12114, #85494, #19734, #103263, #21313, #29925, #102194, #95702, #36968, #2957, #28341, #13702, #62812 ),
 .UNSPECIFIED., .F., .F.,
 ( 4, 2, 2, 2, 2, 2, 2, 2, 4 ),
 ( 0.5000000000000000000, 0.5625000000000000000, 0.6250000000000000000, 0.6875000000000000000, 0.7500000000000000000, 0.8125000000000000000, 0.8750000000000000000, 0.9375000000000000000, 1.000000000000000000 ),
 .UNSPECIFIED. ) ;
#95807 = FILL_AREA_STYLE ('',( #61325 ) ) ;
#95808 = CARTESIAN_POINT ( 'NONE',  ( -19.86162800728182276, 303.8052307878184024, 8.927100233615661296 ) ) ;
#95809 = CARTESIAN_POINT ( 'NONE',  ( 40.03204023273700329, -60.00000000000002842, -33.82007831649015372 ) ) ;
#95810 = AXIS2_PLACEMENT_3D ( 'NONE', #73339, #38884, #24314 ) ;
#95811 = CARTESIAN_POINT ( 'NONE',  ( 41.50669491856072568, 1.482358050883964840E-15, 0.000000000000000000 ) ) ;
#95812 = EDGE_CURVE ( 'NONE', #27254, #101726, #70366, .T. ) ;
#95813 = CARTESIAN_POINT ( 'NONE',  ( 5.656854249492380582, -27.50000000409677270, -5.656854249492379694 ) ) ;
#95814 = CARTESIAN_POINT ( 'NONE',  ( 2.617993873628327250, -5.000000000000000000, 10.00000000000000000 ) ) ;
#95815 = CARTESIAN_POINT ( 'NONE',  ( 86.66175704258623114, -20.68399464850984870, 184.7485519202856210 ) ) ;
#95816 = DIRECTION ( 'NONE',  ( 0.000000000000000000, -1.000000000000000000, 0.000000000000000000 ) ) ;
#95817 = CIRCLE ( 'NONE', #2792, 4.000000000000007105 ) ;
#95818 = CARTESIAN_POINT ( 'NONE',  ( -4.790746215594418267, 7.453269623570716540, 5.000000000000000000 ) ) ;
#95819 = CARTESIAN_POINT ( 'NONE',  ( 6.943926999490789953, -9.466990073738530853, -3.973092371898544251 ) ) ;
#95820 = CARTESIAN_POINT ( 'NONE',  ( 8.572527594031473190E-16, 0.9999999999999970024, -7.000000000000000000 ) ) ;
#95821 = VERTEX_POINT ( 'NONE', #73351 ) ;
#95822 = CARTESIAN_POINT ( 'NONE',  ( 16.58627947206455744, 35.02806585639755355, -21.80698433968624173 ) ) ;
#95823 = CARTESIAN_POINT ( 'NONE',  ( 5.000000000000000000, -13.86855732159281018, 11.25329773914766918 ) ) ;
#95824 = CARTESIAN_POINT ( 'NONE',  ( -99.07703161370366729, -30.00000000000000000, 145.6223805078784324 ) ) ;
#95825 = ADVANCED_FACE ( 'NONE', ( #93903, #32941 ), #65811, .F. ) ;
#95826 = CARTESIAN_POINT ( 'NONE',  ( -2.688402820137723914, -5.953403407568504946, -0.01956314070070124325 ) ) ;
#95827 = CARTESIAN_POINT ( 'NONE',  ( 42.44169098129961526, -57.68683908594360332, 59.94108253702619749 ) ) ;
#95829 =( NAMED_UNIT ( * ) SI_UNIT ( $, .STERADIAN. ) SOLID_ANGLE_UNIT ( ) );
#95828 = CARTESIAN_POINT ( 'NONE',  ( 9.523181975977013991, 43.48366182708068095, 15.16065324379447077 ) ) ;
#95830 = CARTESIAN_POINT ( 'NONE',  ( -16.51907061138358657, 42.00139744608743086, -87.79003255390425409 ) ) ;
#95831 = CARTESIAN_POINT ( 'NONE',  ( -17.97115738240404781, 50.00000000000000711, 61.92613045224233304 ) ) ;
#95832 = CARTESIAN_POINT ( 'NONE',  ( -41.47644945075508360, 477.1143663313983438, -1.041634112212352692 ) ) ;
#95833 = FILL_AREA_STYLE ('',( #71016 ) ) ;
#95834 = EDGE_CURVE ( 'NONE', #83001, #90863, #58918, .T. ) ;
#95835 = MECHANICAL_DESIGN_GEOMETRIC_PRESENTATION_REPRESENTATION (  '', ( #13126 ), #50999 ) ;
#95836 = CARTESIAN_POINT ( 'NONE',  ( -87.15677342750342405, -53.73642251599375896, 193.0054991913189042 ) ) ;
#95837 = VERTEX_POINT ( 'NONE', #19968 ) ;
#95838 = SURFACE_SIDE_STYLE ('',( #20938 ) ) ;
#95839 = CARTESIAN_POINT ( 'NONE',  ( 39.99672247557288784, 437.4320613725466842, 22.45588292425958699 ) ) ;
#95840 = CARTESIAN_POINT ( 'NONE',  ( -11.40776449738530474, -46.43936320564299081, 31.65861530297792825 ) ) ;
#95841 = EDGE_CURVE ( 'NONE', #84725, #51711, #53997, .T. ) ;
#95843 = CARTESIAN_POINT ( 'NONE',  ( 14.85284876471456350, 6.123233995736772199E-16, -5.000000000000001776 ) ) ;
#95842 = CARTESIAN_POINT ( 'NONE',  ( -101.2984257039321818, -59.99999999999997868, 123.3486402982567398 ) ) ;
#95844 = AXIS2_PLACEMENT_3D ( 'NONE', #75366, #1467, #5217 ) ;
#95845 = VERTEX_POINT ( 'NONE', #92741 ) ;
#95846 = CARTESIAN_POINT ( 'NONE',  ( -43.36787761363371629, 463.6242408504509172, 5.358769950476687249 ) ) ;
#95847 = FILL_AREA_STYLE_COLOUR ( '', #82121 ) ;
#95848 = CARTESIAN_POINT ( 'NONE',  ( 33.58349330513379982, -4.000000000000000888, 4.898587196589416773E-16 ) ) ;
#95849 = CARTESIAN_POINT ( 'NONE',  ( 16.04706613565588569, 4.602530725767624453, -3.432994500412984262 ) ) ;
#95850 = CARTESIAN_POINT ( 'NONE',  ( 73.51678032629719439, -60.00000000000000000, 167.3558390227925088 ) ) ;
#95851 = CONICAL_SURFACE ( 'NONE', #21815, 5.000000000000010658, 0.9599310885968697082 ) ;
#95852 = CARTESIAN_POINT ( 'NONE',  ( -0.3374940846666292793, 54.29275678046128206, -7.784862885205691363 ) ) ;
#95853 = EDGE_LOOP ( 'NONE', ( #19552, #26097, #55598, #92973 ) ) ;
#95854 = STYLED_ITEM ( 'NONE', ( #70965 ), #23751 ) ;
#95855 = VECTOR ( 'NONE', #57588, 1000.000000000000000 ) ;
#95856 = VECTOR ( 'NONE', #60062, 1000.000000000000000 ) ;
#95858 = FILL_AREA_STYLE_COLOUR ( '', #99524 ) ;
#95857 = SURFACE_STYLE_FILL_AREA ( #62433 ) ;
#95859 = B_SPLINE_CURVE_WITH_KNOTS ( 'NONE', 3,
 ( #10418, #75145, #1240, #34211, #58992, #91880, #18007, #9884 ),
 .UNSPECIFIED., .F., .F.,
 ( 4, 2, 2, 4 ),
 ( 0.1960348326659903384, 0.3970261244994927607, 0.5980174163329952108, 1.000000000000000000 ),
 .UNSPECIFIED. ) ;
#95860 = CARTESIAN_POINT ( 'NONE',  ( 3.641322288960107567, 129.8017281203003961, -4.999999999999998224 ) ) ;
#95861 = CARTESIAN_POINT ( 'NONE',  ( -5.833333333391548692, -3.737948356783034942, 103.8776713793676834 ) ) ;
#95862 = ORIENTED_EDGE ( 'NONE', *, *, #52312, .F. ) ;
#95863 = EDGE_CURVE ( 'NONE', #54301, #98888, #57543, .T. ) ;
#95864 = EDGE_LOOP ( 'NONE', ( #66050, #65151, #88551, #18859 ) ) ;
#95866 = AXIS2_PLACEMENT_3D ( 'NONE', #78981, #38546, #14231 ) ;
#95865 = CARTESIAN_POINT ( 'NONE',  ( -27.85081853580795297, 315.3923268305527472, 12.51532622124604011 ) ) ;
#95867 = ORIENTED_EDGE ( 'NONE', *, *, #16337, .F. ) ;
#95869 =( BOUNDED_SURFACE ( )  B_SPLINE_SURFACE ( 2, 3, ( 
 ( #6920, #39841, #65160, #87860, #54932, #13944, #15007, #23672, #14464, #106675, #79750, #89450, #5857, #24207, #22626, #55979, #71648, #63594 ),
 ( #16077, #48436, #98056, #105102, #38782, #55458, #15542, #47899, #88913, #104555, #88390, #57057, #89973, #80805, #47379, #40889, #48957, #72714 ),
 ( #7437, #80269, #6382, #39317, #106132, #73775, #81854, #64637, #72197, #31242, #97508, #32823, #105617, #31756, #40354, #73231, #32290, #7977 ) ),
 .UNSPECIFIED., .F., .T., .T. ) 
 B_SPLINE_SURFACE_WITH_KNOTS ( ( 3, 3 ),
 ( 4, 2, 2, 2, 2, 2, 2, 2, 4 ),
 ( 0.000000000000000000, 1.000000000000000000 ),
 ( 0.000000000000000000, 0.7853981633974482790, 1.570796326794896558, 2.356194490192344837, 3.141592653589793116, 3.926990816987241395, 4.712388980384689674, 5.497787143782137953, 6.283185307179586232 ),
 .UNSPECIFIED. ) 
 GEOMETRIC_REPRESENTATION_ITEM ( )  RATIONAL_B_SPLINE_SURFACE ( (
 ( 1.000000000000000000, 1.000000000000000000, 1.000000000000000000, 1.000000000000000000, 1.000000000000000000, 1.000000000000000000, 1.000000000000000000, 1.000000000000000000, 1.000000000000000000, 1.000000000000000000, 1.000000000000000000, 1.000000000000000000, 1.000000000000000000, 1.000000000000000000, 1.000000000000000000, 1.000000000000000000, 1.000000000000000000, 1.000000000000000000),
 ( 1.857142857142858317, 1.857142857142858317, 1.857142857142858317, 1.857142857142858317, 1.857142857142858317, 1.857142857142858317, 1.857142857142858317, 1.857142857142858317, 1.857142857142858317, 1.857142857142858317, 1.857142857142858317, 1.857142857142858317, 1.857142857142858317, 1.857142857142858317, 1.857142857142858317, 1.857142857142858317, 1.857142857142858317, 1.857142857142858317),
 ( 1.000000000000000000, 1.000000000000000000, 1.000000000000000000, 1.000000000000000000, 1.000000000000000000, 1.000000000000000000, 1.000000000000000000, 1.000000000000000000, 1.000000000000000000, 1.000000000000000000, 1.000000000000000000, 1.000000000000000000, 1.000000000000000000, 1.000000000000000000, 1.000000000000000000, 1.000000000000000000, 1.000000000000000000, 1.000000000000000000) ) ) 
 REPRESENTATION_ITEM ( '' )  SURFACE ( )  );
#95868 = FACE_OUTER_BOUND ( 'NONE', #49886, .T. ) ;
#95870 = CARTESIAN_POINT ( 'NONE',  ( -40.56952547639716755, 460.8933045338675925, 2.221423359587606505 ) ) ;
#95871 = FACE_OUTER_BOUND ( 'NONE', #44813, .T. ) ;
#95872 = ORIENTED_EDGE ( 'NONE', *, *, #59348, .T. ) ;
#95873 = FILL_AREA_STYLE_COLOUR ( '', #65184 ) ;
#95874 = CARTESIAN_POINT ( 'NONE',  ( -6.214520335144379182, 41.72338998088525841, -70.49303492603483789 ) ) ;
#95875 = CARTESIAN_POINT ( 'NONE',  ( -94.29423131824410120, -59.99999999999747757, 204.9864844129882044 ) ) ;
#95876 = DIRECTION ( 'NONE',  ( 0.000000000000000000, -1.000000000000000000, 0.000000000000000000 ) ) ;
#95877 = AXIS2_PLACEMENT_3D ( 'NONE', #90739, #35185, #2777 ) ;
#95878 = CARTESIAN_POINT ( 'NONE',  ( 49.62012381316495890, -59.99999999999997868, 70.85806097636194067 ) ) ;
#95879 = CARTESIAN_POINT ( 'NONE',  ( 14.78938945996223886, -5.000000000000000000, 7.149827492542583762 ) ) ;
#95880 = CARTESIAN_POINT ( 'NONE',  ( 0.000000000000000000, 115.0000000000000000, -8.000000000000000000 ) ) ;
#95882 = CARTESIAN_POINT ( 'NONE',  ( 12.44414058928305344, -42.95372205198454196, 31.10491182296270196 ) ) ;
#95881 = CARTESIAN_POINT ( 'NONE',  ( -102.6949714452557885, -14.21045842199446518, 129.2658233771313974 ) ) ;
#95883 = DIRECTION ( 'NONE',  ( 0.000000000000000000, 1.000000000000000000, 0.000000000000000000 ) ) ;
#95884 = CARTESIAN_POINT ( 'NONE',  ( -46.99575457356646524, -18.77608308516024849, 40.16000815951232283 ) ) ;
#95885 = CARTESIAN_POINT ( 'NONE',  ( -7.149999999999890221, 41.65000000000012648, -59.82695526680724640 ) ) ;
#95886 = ORIENTED_EDGE ( 'NONE', *, *, #40212, .F. ) ;
#95887 = DIRECTION ( 'NONE',  ( -1.000000000000000000, -1.224606353822377258E-16, -0.000000000000000000 ) ) ;
#95888 = CARTESIAN_POINT ( 'NONE',  ( 17.99621717127815046, 36.54019273113857480, 22.85642881224868006 ) ) ;
#95890 = VERTEX_POINT ( 'NONE', #36679 ) ;
#95889 = CONICAL_SURFACE ( 'NONE', #40822, 46.94949242731048145, 0.3972631705159501148 ) ;
#95891 = CARTESIAN_POINT ( 'NONE',  ( -5.369327769978998965, -15.91632837477424367, 14.07056384452391029 ) ) ;
#95892 = EDGE_LOOP ( 'NONE', ( #17111, #47838, #104807, #104592, #85691 ) ) ;
#95893 = CARTESIAN_POINT ( 'NONE',  ( 84.89073916653602225, -30.00000000000001776, 197.0696916040373026 ) ) ;
#95894 = CARTESIAN_POINT ( 'NONE',  ( 7.500000000000001776, 0.000000000000000000, 0.000000000000000000 ) ) ;
#95895 = CARTESIAN_POINT ( 'NONE',  ( 6.394717868937521921, 41.92174093517635924, -59.37671486230904350 ) ) ;
#95896 = STYLED_ITEM ( 'NONE', ( #75441 ), #100986 ) ;
#95897 = CARTESIAN_POINT ( 'NONE',  ( 94.82639388037442529, -30.00000000000000355, 191.3365978075416933 ) ) ;
#95898 = EDGE_CURVE ( 'NONE', #74084, #91139, #21331, .T. ) ;
#95899 = DIRECTION ( 'NONE',  ( 0.000000000000000000, 1.000000000000000000, 0.000000000000000000 ) ) ;
#95900 = VERTEX_POINT ( 'NONE', #3748 ) ;
#95901 = ORIENTED_EDGE ( 'NONE', *, *, #63155, .F. ) ;
#95902 = VERTEX_POINT ( 'NONE', #11811 ) ;
#95903 = DIRECTION ( 'NONE',  ( 1.000000000000000000, 1.224606353822377258E-16, 0.000000000000000000 ) ) ;
#95904 = LINE ( 'NONE', #14423, #61135 ) ;
#95905 = ADVANCED_FACE ( 'NONE', ( #10743 ), #43135, .F. ) ;
#95906 = CARTESIAN_POINT ( 'NONE',  ( 6.763850406535977022, 294.7356673863635592, 9.912314076180619438 ) ) ;
#95907 = ADVANCED_FACE ( 'NONE', ( #101893 ), #92196, .T. ) ;
#95908 = ORIENTED_EDGE ( 'NONE', *, *, #5617, .F. ) ;
#95909 = CARTESIAN_POINT ( 'NONE',  ( -76.12537862032631608, -38.35598417008158378, -28.58435412235099804 ) ) ;
#95910 = ORIENTED_EDGE ( 'NONE', *, *, #62587, .T. ) ;
#95911 = DIRECTION ( 'NONE',  ( 0.000000000000000000, -1.000000000000000000, 0.000000000000000000 ) ) ;
#95912 = CARTESIAN_POINT ( 'NONE',  ( 102.3932405693164611, -38.43728085762052160, 199.4716403674687513 ) ) ;
#95913 = CARTESIAN_POINT ( 'NONE',  ( 16.00000000000007461, 4.197692598229727956, 4.745459346021252856 ) ) ;
#95914 = CARTESIAN_POINT ( 'NONE',  ( 83.78544372828790188, -45.28299759132907099, 18.52600201645970657 ) ) ;
#95915 = DIRECTION ( 'NONE',  ( -1.000000000000000000, 0.000000000000000000, 0.000000000000000000 ) ) ;
#95916 = CARTESIAN_POINT ( 'NONE',  ( 40.64097752467004909, 353.9523173779949161, 23.32106799875517567 ) ) ;
#95917 = CARTESIAN_POINT ( 'NONE',  ( 21.36650669486618881, 4.898587196589411843E-16, -4.000000000000000888 ) ) ;
#95918 = TOROIDAL_SURFACE ( 'NONE', #49375, 11.00000000000000000, 1.000000000000000000 ) ;
#95919 = DIRECTION ( 'NONE',  ( -0.000000000000000000, -0.000000000000000000, -1.000000000000000000 ) ) ;
#95920 = STYLED_ITEM ( 'NONE', ( #103223 ), #66649 ) ;
#95921 = CARTESIAN_POINT ( 'NONE',  ( 4.678819457397882964, 143.9212778189118751, 5.000000000000000000 ) ) ;
#95922 = ORIENTED_EDGE ( 'NONE', *, *, #56826, .T. ) ;
#95923 = CARTESIAN_POINT ( 'NONE',  ( -8.000000000000000000, -10.53125000409677092, -3.313708498984762496 ) ) ;
#95924 = CARTESIAN_POINT ( 'NONE',  ( -34.03780482868043578, 462.4848023821838296, 4.882790418534471932 ) ) ;
#95925 = CARTESIAN_POINT ( 'NONE',  ( -3.426400788788944496, 123.5889412327351664, 4.999999999999997335 ) ) ;
#95926 = ORIENTED_EDGE ( 'NONE', *, *, #40887, .F. ) ;
#95927 = DIRECTION ( 'NONE',  ( -0.000000000000000000, 1.000000000000000000, -0.000000000000000000 ) ) ;
#95928 = CARTESIAN_POINT ( 'NONE',  ( -25.65900546945094263, 305.1951251589714502, 10.46195101058732391 ) ) ;
#95929 = CARTESIAN_POINT ( 'NONE',  ( 27.99999999999999645, 0.000000000000000000, 0.000000000000000000 ) ) ;
#95930 = FILL_AREA_STYLE ('',( #104001 ) ) ;
#95931 = CARTESIAN_POINT ( 'NONE',  ( 4.898587196589412829E-16, -12.12499999999999289, -8.000000000000000000 ) ) ;
#95932 = CONICAL_SURFACE ( 'NONE', #11436, 4.000000000000001776, 0.9599310885968808105 ) ;
#95934 = CARTESIAN_POINT ( 'NONE',  ( -36.76540882621739570, -27.25414842009635663, 43.58040692005798888 ) ) ;
#95933 = PRESENTATION_LAYER_ASSIGNMENT (  '', '', ( #68368 ) ) ;
#95935 = ADVANCED_FACE ( 'NONE', ( #35607 ), #94355, .T. ) ;
#95936 = PRESENTATION_LAYER_ASSIGNMENT (  '', '', ( #33902 ) ) ;
#95937 = AXIS2_PLACEMENT_3D ( 'NONE', #105625, #64646, #23683 ) ;
#95938 = CARTESIAN_POINT ( 'NONE',  ( 0.000000000000000000, -15.00000000000000000, -8.500000000000000000 ) ) ;
#95939 = VECTOR ( 'NONE', #23722, 1000.000000000000341 ) ;
#95940 = ORIENTED_EDGE ( 'NONE', *, *, #73180, .F. ) ;
#95941 = CARTESIAN_POINT ( 'NONE',  ( 85.45182810718637256, -39.29543685595842106, 185.3021898051531196 ) ) ;
#95942 = CARTESIAN_POINT ( 'NONE',  ( -38.54883366569859504, 27.49541921524758337, 11.41610407978632402 ) ) ;
#95943 = EDGE_CURVE ( 'NONE', #72232, #77351, #8646, .T. ) ;
#95944 = CARTESIAN_POINT ( 'NONE',  ( -3.400000000000000355, 4.163799117101001052E-16, -6.123524522925831270 ) ) ;
#95945 = EDGE_LOOP ( 'NONE', ( #60848, #14458, #548, #9990, #14675 ) ) ;
#95946 = CARTESIAN_POINT ( 'NONE',  ( 94.01656501709089753, -57.67294275299069284, 19.38523437918474102 ) ) ;
#95947 = VECTOR ( 'NONE', #102760, 1000.000000000000000 ) ;
#95948 = CARTESIAN_POINT ( 'NONE',  ( 35.93056730070288296, 437.9188583894897420, 4.302256410569166967 ) ) ;
#95949 = CARTESIAN_POINT ( 'NONE',  ( 14.82275922442112304, -4.333298119783705715, -10.06958627548034535 ) ) ;
#95950 = VECTOR ( 'NONE', #22241, 1000.000000000000000 ) ;
#95951 =( NAMED_UNIT ( * ) PLANE_ANGLE_UNIT ( ) SI_UNIT ( $, .RADIAN. ) );
#95952 = ADVANCED_FACE ( 'NONE', ( #76019 ), #1181, .F. ) ;
#95953 = CARTESIAN_POINT ( 'NONE',  ( 15.09797279524721425, -22.74424748559674470, 35.94748513521482636 ) ) ;
#95954 = CARTESIAN_POINT ( 'NONE',  ( 48.75403305889158645, -29.43289434049833986, 44.67303107480096003 ) ) ;
#95956 = CARTESIAN_POINT ( 'NONE',  ( -12.30943243785228169, 5.664461549456914824, 8.431530038708269004 ) ) ;
#95955 = CARTESIAN_POINT ( 'NONE',  ( 3.096526599377916078, -6.872473572140724407, -6.510295232596552406E-15 ) ) ;
#95957 = CARTESIAN_POINT ( 'NONE',  ( 4.174999999999998934, 0.000000000000000000, -0.5776712190230098853 ) ) ;
#95958 = CARTESIAN_POINT ( 'NONE',  ( -15.88903491159068082, 43.99850675625265950, -4.407766777241893585 ) ) ;
#95959 = ORIENTED_EDGE ( 'NONE', *, *, #51762, .F. ) ;
#95960 = CARTESIAN_POINT ( 'NONE',  ( -39.51997949802257182, -33.17322444800073811, -29.37170241217619449 ) ) ;
#95961 = CARTESIAN_POINT ( 'NONE',  ( 59.89460441624491693, -4.000000000000000888, 4.898587196589422689E-16 ) ) ;
#95962 = CARTESIAN_POINT ( 'NONE',  ( -95.03937034330597555, -38.00000000000000000, 107.8039155741109738 ) ) ;
#95963 = COLOUR_RGB ( '', 0.72549020, 0.75294118, 0.79215686) ;
#95964 = ORIENTED_EDGE ( 'NONE', *, *, #32326, .T. ) ;
#95965 = CARTESIAN_POINT ( 'NONE',  ( -9.717036974652998538, 2.772147514592163908, 14.74200096892023026 ) ) ;
#95966 = CARTESIAN_POINT ( 'NONE',  ( 104.3757837139179117, 1.016364837396684119E-14, 0.000000000000000000 ) ) ;
#95967 = DIRECTION ( 'NONE',  ( -1.000000000000000000, -0.000000000000000000, -0.000000000000000000 ) ) ;
#95968 = ADVANCED_FACE ( 'NONE', ( #79213 ), #30698, .T. ) ;
#95970 = CARTESIAN_POINT ( 'NONE',  ( -41.98950613031892942, -60.22824704085319780, -33.55409513438841174 ) ) ;
#95969 = PRESENTATION_STYLE_ASSIGNMENT (( #38284 ) ) ;
#95971 = ORIENTED_EDGE ( 'NONE', *, *, #12962, .F. ) ;
#95972 = CARTESIAN_POINT ( 'NONE',  ( -44.14563638416869651, 463.1455159964050381, 6.337363416021459805 ) ) ;
#95973 = VERTEX_POINT ( 'NONE', #95400 ) ;
#95974 = CIRCLE ( 'NONE', #89294, 4.000000000000001776 ) ;
#95975 = CARTESIAN_POINT ( 'NONE',  ( 6.585468679846623985, 7.640532685286893333, -0.2337908078075575935 ) ) ;
#95976 = CARTESIAN_POINT ( 'NONE',  ( -44.14911905790387436, 464.3766534541992996, 9.623404994945699897 ) ) ;
#95977 = CARTESIAN_POINT ( 'NONE',  ( -92.53812791416793004, -60.00000000000000711, -1.816796087269537008 ) ) ;
#95978 = ORIENTED_EDGE ( 'NONE', *, *, #65392, .T. ) ;
#95979 = CARTESIAN_POINT ( 'NONE',  ( 7.232205791931205496, 41.33266196706463802, -58.20097105119658920 ) ) ;
#95980 = CARTESIAN_POINT ( 'NONE',  ( 33.00000000000000000, 463.5362553048592531, 6.739467187734345721 ) ) ;
#95981 = CARTESIAN_POINT ( 'NONE',  ( -9.948688207305192321, 26.12976850509815918, -1.044946705213435134 ) ) ;
#95982 = CONICAL_SURFACE ( 'NONE', #90827, 7.000000000000000000, 0.9599310885968753704 ) ;
#95984 = DIRECTION ( 'NONE',  ( -1.000000000000000000, -0.000000000000000000, -0.000000000000000000 ) ) ;
#95983 = CARTESIAN_POINT ( 'NONE',  ( 63.56127108291158123, 4.898587196589294500E-16, -4.000000000000007105 ) ) ;
#95985 = CARTESIAN_POINT ( 'NONE',  ( -83.63428025110276565, -25.61067944322265433, 154.1989751819577634 ) ) ;
#95986 = STYLED_ITEM ( 'NONE', ( #49747 ), #66973 ) ;
#95987 = ORIENTED_EDGE ( 'NONE', *, *, #89285, .T. ) ;
#95988 = CARTESIAN_POINT ( 'NONE',  ( -16.14668631625900019, -0.000000000000000000, -5.483261958887230669 ) ) ;
#95989 = EDGE_CURVE ( 'NONE', #68935, #30792, #40079, .T. ) ;
#95990 = ORIENTED_EDGE ( 'NONE', *, *, #11178, .T. ) ;
#95991 = EDGE_LOOP ( 'NONE', ( #94603, #51649, #79179, #102398, #85340 ) ) ;
#95992 = CARTESIAN_POINT ( 'NONE',  ( 1.301042606982605321E-15, -5.000000000000000000, -10.00000000000000000 ) ) ;
#95993 = DIRECTION ( 'NONE',  ( 0.000000000000000000, 0.000000000000000000, -1.000000000000000000 ) ) ;
#95994 = FILL_AREA_STYLE ('',( #7478 ) ) ;
#95995 = ORIENTED_EDGE ( 'NONE', *, *, #62542, .T. ) ;
#95997 = B_SPLINE_CURVE_WITH_KNOTS ( 'NONE', 3,
 ( #101573, #93493, #52473, #3412, #11475, #44403 ),
 .UNSPECIFIED., .F., .F.,
 ( 4, 2, 4 ),
 ( 0.000000000000000000, 0.001916782365109703659, 0.003833564730219407319 ),
 .UNSPECIFIED. ) ;
#95996 = CARTESIAN_POINT ( 'NONE',  ( -9.168149550320913832, 15.99999999372935022, -3.997425403568243496 ) ) ;
#95998 = CARTESIAN_POINT ( 'NONE',  ( -94.30950767697063952, -57.61975185784459086, 204.5257163505249309 ) ) ;
#95999 = CARTESIAN_POINT ( 'NONE',  ( -4.905194654929172948, -67.02394395019842932, 3.459476078998854121 ) ) ;
#96000 = CARTESIAN_POINT ( 'NONE',  ( 0.000000000000000000, 0.000000000000000000, 0.000000000000000000 ) ) ;
#96001 = CONICAL_SURFACE ( 'NONE', #37450, 4.172000000000001485, 0.9599310885968750373 ) ;
#96002 = AXIS2_PLACEMENT_3D ( 'NONE', #55619, #65336, #104727 ) ;
#96003 =( NAMED_UNIT ( * ) PLANE_ANGLE_UNIT ( ) SI_UNIT ( $, .RADIAN. ) );
#96004 = CARTESIAN_POINT ( 'NONE',  ( 79.45700042099618088, -60.00000000000000711, -30.99979279722015590 ) ) ;
#96005 = CARTESIAN_POINT ( 'NONE',  ( -61.00210428163805432, -14.21045842199449005, 86.20094954650318186 ) ) ;
#96006 = CARTESIAN_POINT ( 'NONE',  ( -56.92782483176372921, -32.55445101946592246, 61.63125569926470604 ) ) ;
#96007 = ORIENTED_EDGE ( 'NONE', *, *, #84151, .F. ) ;
#96008 = DIRECTION ( 'NONE',  ( -0.000000000000000000, -0.000000000000000000, 1.000000000000000000 ) ) ;
#96010 = ORIENTED_EDGE ( 'NONE', *, *, #89988, .F. ) ;
#96009 = AXIS2_PLACEMENT_3D ( 'NONE', #42225, #10384, #43301 ) ;
#96011 = CARTESIAN_POINT ( 'NONE',  ( -101.3713891769874778, -45.26458131978182564, 190.6351527844882980 ) ) ;
#96012 = CARTESIAN_POINT ( 'NONE',  ( 0.000000000000000000, -30.00000000000000000, 0.000000000000000000 ) ) ;
#96013 = VERTEX_POINT ( 'NONE', #87321 ) ;
#96014 = CARTESIAN_POINT ( 'NONE',  ( 19.23019573275864502, 49.80287270500782171, 61.49929745255238345 ) ) ;
#96015 = CARTESIAN_POINT ( 'NONE',  ( 110.7700795740980197, -38.35618397565083626, 179.7263034240603474 ) ) ;
#96016 = CARTESIAN_POINT ( 'NONE',  ( -42.19179521602280403, 485.4956273777414708, -3.824025998168937512 ) ) ;
#96017 = LINE ( 'NONE', #87926, #90475 ) ;
#96018 =( GEOMETRIC_REPRESENTATION_CONTEXT ( 3 ) GLOBAL_UNCERTAINTY_ASSIGNED_CONTEXT ( ( #1680 ) ) GLOBAL_UNIT_ASSIGNED_CONTEXT ( ( #104797, #13651, #46041 ) ) REPRESENTATION_CONTEXT ( 'NONE', 'WORKASPACE' ) );
#96019 = SURFACE_SIDE_STYLE ('',( #63118 ) ) ;
#96020 = CARTESIAN_POINT ( 'NONE',  ( 7.744991119775235688, -81.53561214574868643, -2.016316005557098112 ) ) ;
#96021 = CARTESIAN_POINT ( 'NONE',  ( -33.08751701378358945, 301.6823158026044780, 11.49690784967660662 ) ) ;
#96022 = AXIS2_PLACEMENT_3D ( 'NONE', #103278, #44518, #37518 ) ;
#96023 = CARTESIAN_POINT ( 'NONE',  ( -9.076720569991527654, 43.77011807854803749, -14.51161200666307849 ) ) ;
#96024 = CARTESIAN_POINT ( 'NONE',  ( 43.00000000000000000, 462.1685671383398244, 2.813679926073844317 ) ) ;
#96025 = EDGE_CURVE ( 'NONE', #98395, #59135, #53854, .T. ) ;
#96026 = CARTESIAN_POINT ( 'NONE',  ( 26.11923076923076792, -4.171999999999999709, 0.000000000000000000 ) ) ;
#96027 = CARTESIAN_POINT ( 'NONE',  ( -28.52589013025375664, -25.58464632904579261, 30.19568687849871935 ) ) ;
#96028 = ORIENTED_EDGE ( 'NONE', *, *, #88113, .T. ) ;
#96029 = ORIENTED_EDGE ( 'NONE', *, *, #65294, .F. ) ;
#96030 = CARTESIAN_POINT ( 'NONE',  ( 48.17486088641305741, -56.81898877664855974, 53.29977222331121567 ) ) ;
#96031 = CARTESIAN_POINT ( 'NONE',  ( 0.000000000000000000, -6.928203230275511437, -3.999999999999997335 ) ) ;
#96032 = EDGE_CURVE ( 'NONE', #10770, #5773, #105093, .T. ) ;
#96033 = CARTESIAN_POINT ( 'NONE',  ( 101.2019940638598854, 1.030564683017419500E-14, 0.000000000000000000 ) ) ;
#96034 = CARTESIAN_POINT ( 'NONE',  ( -110.7787815506858209, -38.35615617498751106, 165.0880282141192765 ) ) ;
#96035 = CONICAL_SURFACE ( 'NONE', #3017, 4.000000000000001776, 0.9599310885968808105 ) ;
#96036 = VERTEX_POINT ( 'NONE', #104010 ) ;
#96037 = CARTESIAN_POINT ( 'NONE',  ( 87.50928707171397036, -38.36873170751620421, -20.25758776273239903 ) ) ;
#96038 = CARTESIAN_POINT ( 'NONE',  ( 11.45536878374885958, 14.80507779433297699, -9.852200945225588313 ) ) ;
#96039 = CARTESIAN_POINT ( 'NONE',  ( -19.42844902724960576, 49.96150201163990801, 60.80087220774903756 ) ) ;
#96040 = CARTESIAN_POINT ( 'NONE',  ( 10.61022379808845351, 43.90722765790382454, 12.94778756132729391 ) ) ;
#96041 = CARTESIAN_POINT ( 'NONE',  ( -31.80699609565019514, 437.1986690746257409, 20.73198424672801465 ) ) ;
#96042 = CARTESIAN_POINT ( 'NONE',  ( -35.74109609218656658, 414.8491554067354059, 5.919296220277036724 ) ) ;
#96043 = CARTESIAN_POINT ( 'NONE',  ( -31.55401502570843419, 436.6824539894687973, 19.27688314274631054 ) ) ;
#96044 = CARTESIAN_POINT ( 'NONE',  ( -30.00000000000000355, 488.6481008951263902, 3.890293910846380321 ) ) ;
#96045 = PRESENTATION_LAYER_ASSIGNMENT (  '', '', ( #92636 ) ) ;
#96046 = CARTESIAN_POINT ( 'NONE',  ( 84.12166230012984158, -60.00000000000000711, 199.5799458206678878 ) ) ;
#96047 = AXIS2_PLACEMENT_3D ( 'NONE', #47611, #72431, #57823 ) ;
#96048 = CARTESIAN_POINT ( 'NONE',  ( -16.42296553627748423, 35.05188915981860731, 21.84814778194889939 ) ) ;
#96049 = ORIENTED_EDGE ( 'NONE', *, *, #87301, .T. ) ;
#96050 = CARTESIAN_POINT ( 'NONE',  ( 55.38483915043129002, -46.43683086870206012, 64.00419006234304220 ) ) ;
#96051 = CARTESIAN_POINT ( 'NONE',  ( -28.50623484390343521, 306.2062397803906606, -9.250652555261318355 ) ) ;
#96052 = CARTESIAN_POINT ( 'NONE',  ( -13.00000000000003730, -85.00000000000000000, 0.000000000000000000 ) ) ;
#96053 = CARTESIAN_POINT ( 'NONE',  ( -7.344361273354515163, 27.55439469411475173, -3.175733139645582792 ) ) ;
#96054 = ORIENTED_EDGE ( 'NONE', *, *, #69423, .T. ) ;
#96056 = FACE_OUTER_BOUND ( 'NONE', #31294, .T. ) ;
#96055 = CARTESIAN_POINT ( 'NONE',  ( -101.6643687224884616, -38.44986872770192576, 199.8638131606589923 ) ) ;
#96057 = DIRECTION ( 'NONE',  ( -1.000000000000000000, -0.000000000000000000, -0.000000000000000000 ) ) ;
#96058 = CARTESIAN_POINT ( 'NONE',  ( -13.00000000000003730, -65.00000000000000000, 0.000000000000000000 ) ) ;
#96059 = CARTESIAN_POINT ( 'NONE',  ( 8.000000000000000000, -34.99999999999999289, 0.000000000000000000 ) ) ;
#96060 = CARTESIAN_POINT ( 'NONE',  ( 9.999999999999994671, -3.000000000000002665, -86.30899693747679180 ) ) ;
#96061 = CARTESIAN_POINT ( 'NONE',  ( 30.87964800539008081, 13.48323453669522465, -41.23000148635505013 ) ) ;
#96063 = VERTEX_POINT ( 'NONE', #63041 ) ;
#96062 = CARTESIAN_POINT ( 'NONE',  ( -7.619135598915500296, 101.8269463221532334, 2.449260492474796713 ) ) ;
#96064 = CARTESIAN_POINT ( 'NONE',  ( 82.08679795893965547, -49.97481940385915067, 177.5961885972273251 ) ) ;
#96065 = CARTESIAN_POINT ( 'NONE',  ( 8.160622567441036423, 39.63602799826242062, -1.301042606982605321E-15 ) ) ;
#96066 = VECTOR ( 'NONE', #15528, 1000.000000000000000 ) ;
#96067 = CARTESIAN_POINT ( 'NONE',  ( -33.00000000000000711, 439.7597899781497404, 24.16317522621305258 ) ) ;
#96068 = VERTEX_POINT ( 'NONE', #95944 ) ;
#96069 = CARTESIAN_POINT ( 'NONE',  ( -30.48212520012076254, 308.5335761172966613, -8.699255827182120981 ) ) ;
#96070 = CARTESIAN_POINT ( 'NONE',  ( 6.108201232855582141, -4.361520614648577876, -16.81796607653726383 ) ) ;
#96071 = CARTESIAN_POINT ( 'NONE',  ( 26.48443586042315445, 34.96036863989223775, -7.709928564565299069 ) ) ;
#96072 = PRESENTATION_STYLE_ASSIGNMENT (( #70198 ) ) ;
#96073 = SURFACE_STYLE_USAGE ( .BOTH. , #13539 ) ;
#96074 = DIRECTION ( 'NONE',  ( 0.000000000000000000, 1.000000000000000000, 0.000000000000000000 ) ) ;
#96075 = EDGE_CURVE ( 'NONE', #52615, #22977, #5847, .T. ) ;
#96076 = EDGE_LOOP ( 'NONE', ( #60098, #89124, #57555, #45431 ) ) ;
#96077 = AXIS2_PLACEMENT_3D ( 'NONE', #72620, #105522, #31662 ) ;
#96078 = CARTESIAN_POINT ( 'NONE',  ( -81.02657573093092935, -30.00000000000000000, 21.43806085364088077 ) ) ;
#96079 = CARTESIAN_POINT ( 'NONE',  ( -5.000000000000000888, -51.24344465340260513, 3.816021516648668843 ) ) ;
#96080 = CARTESIAN_POINT ( 'NONE',  ( -3.325451350920383131E-15, 6.534749472788146107, 4.681481898397001906 ) ) ;
#96082 = CARTESIAN_POINT ( 'NONE',  ( -12.14823058519115939, 17.46151334162848912, -8.967021852677630633 ) ) ;
#96081 = CARTESIAN_POINT ( 'NONE',  ( 34.84618260875170392, 489.9833681528626812, 11.97975507378813731 ) ) ;
#96083 = CARTESIAN_POINT ( 'NONE',  ( -2.977408999572650039, -17.18750000204838813, -7.188101187500001821 ) ) ;
#96084 = CARTESIAN_POINT ( 'NONE',  ( 17.14761585140983158, 294.5838192077795838, -10.05696245189486149 ) ) ;
#96085 = MECHANICAL_DESIGN_GEOMETRIC_PRESENTATION_REPRESENTATION (  '', ( #32354 ), #90928 ) ;
#96086 = CARTESIAN_POINT ( 'NONE',  ( 5.000000000000000000, 6.123233995736766282E-16, -8.553285714285713937 ) ) ;
#96087 = ORIENTED_EDGE ( 'NONE', *, *, #2564, .F. ) ;
#96088 = CARTESIAN_POINT ( 'NONE',  ( 32.33349330513379982, 1.593028355512270567E-15, 0.000000000000000000 ) ) ;
#96089 = CARTESIAN_POINT ( 'NONE',  ( 7.500000000000000000, -3.157198044629119682, -7.642795354506497496 ) ) ;
#96090 = CARTESIAN_POINT ( 'NONE',  ( -9.590509843553020275, 9.008796699642211081, -5.000000000000000888 ) ) ;
#96091 = CARTESIAN_POINT ( 'NONE',  ( -4.852941176470594975, -4.999999999999998224, -70.80672828634229177 ) ) ;
#96092 = ADVANCED_FACE ( 'NONE', ( #64119 ), #74469, .T. ) ;
#96093 = DIRECTION ( 'NONE',  ( 0.000000000000000000, -1.000000000000000000, 0.000000000000000000 ) ) ;
#96094 = ORIENTED_EDGE ( 'NONE', *, *, #29745, .T. ) ;
#96095 = AXIS2_PLACEMENT_3D ( 'NONE', #34036, #43682, #99793 ) ;
#96096 = DIRECTION ( 'NONE',  ( 0.000000000000000000, -1.000000000000000000, 0.000000000000000000 ) ) ;
#96097 = ORIENTED_EDGE ( 'NONE', *, *, #49060, .T. ) ;
#96098 = ADVANCED_FACE ( 'NONE', ( #62001 ), #373, .T. ) ;
#96099 = CARTESIAN_POINT ( 'NONE',  ( 4.699999999999999289, -7.505553499465138501, 0.000000000000000000 ) ) ;
#96100 = CARTESIAN_POINT ( 'NONE',  ( -3.363582653045783299, -1.214734195355907431, 104.5994639297836386 ) ) ;
#96101 = CIRCLE ( 'NONE', #46149, 5.000000000000001776 ) ;
#96102 = CARTESIAN_POINT ( 'NONE',  ( 7.149999999999997691, 41.65000000000000568, -59.82695526683420439 ) ) ;
#96103 = CYLINDRICAL_SURFACE ( 'NONE', #61696, 4.000000000000003553 ) ;
#96104 = CARTESIAN_POINT ( 'NONE',  ( -112.1392827011767537, -60.00000000000000000, 167.2709583566187916 ) ) ;
#96105 = DIRECTION ( 'NONE',  ( 1.000000000000000000, 0.000000000000000000, 0.000000000000000000 ) ) ;
#96106 = CARTESIAN_POINT ( 'NONE',  ( 6.562874270078295602, 3.301808241302743863, 6.845811579416823278 ) ) ;
#96107 = CYLINDRICAL_SURFACE ( 'NONE', #102869, 1.250000000000001110 ) ;
#96108 = DIRECTION ( 'NONE',  ( 0.000000000000000000, 0.8660254037844377084, -0.5000000000000017764 ) ) ;
#96109 = CONICAL_SURFACE ( 'NONE', #8327, 4.000000000000001776, 0.9599310885968808105 ) ;
#96110 = CARTESIAN_POINT ( 'NONE',  ( -85.66377476482907127, -25.20926228141058800, 174.6162987478353728 ) ) ;
#96111 = ORIENTED_EDGE ( 'NONE', *, *, #83164, .T. ) ;
#96112 = CARTESIAN_POINT ( 'NONE',  ( 43.55231887857613771, 41.43784824290622026, -50.62546061442120759 ) ) ;
#96113 = EDGE_CURVE ( 'NONE', #26304, #62818, #77962, .T. ) ;
#96114 = ORIENTED_EDGE ( 'NONE', *, *, #37418, .F. ) ;
#96115 = DIRECTION ( 'NONE',  ( 1.000000000000000000, 0.000000000000000000, -0.000000000000000000 ) ) ;
#96116 = SURFACE_SIDE_STYLE ('',( #102613 ) ) ;
#96117 = B_SPLINE_CURVE_WITH_KNOTS ( 'NONE', 3,
 ( #87189, #13268, #46190, #85604, #36016, #28998 ),
 .UNSPECIFIED., .F., .F.,
 ( 4, 2, 4 ),
 ( 0.01067228061038543591, 0.01257272967564228294, 0.01447317874089912824 ),
 .UNSPECIFIED. ) ;
#96118 = CARTESIAN_POINT ( 'NONE',  ( -86.12765991300337021, -60.14013167474347199, 11.25586421641007284 ) ) ;
#96119 = CARTESIAN_POINT ( 'NONE',  ( -6.632175269158647524, 303.7449820775430567, 9.914291074352707511 ) ) ;
#96120 = CIRCLE ( 'NONE', #73698, 6.999999999999999112 ) ;
#96121 = DIRECTION ( 'NONE',  ( 0.000000000000000000, 0.000000000000000000, 1.000000000000000000 ) ) ;
#96122 = CARTESIAN_POINT ( 'NONE',  ( 7.955551520415933275, 53.39349112219682070, -5.000000000000000888 ) ) ;
#96123 = CARTESIAN_POINT ( 'NONE',  ( 5.193195059372482212E-16, -7.895640089090903757, -6.564402953523731377 ) ) ;
#96124 = CARTESIAN_POINT ( 'NONE',  ( 30.67950393665801556, 18.64316884713159794, -23.57730434125293328 ) ) ;
#96125 = CIRCLE ( 'NONE', #87589, 4.000000000000007105 ) ;
#96126 = CARTESIAN_POINT ( 'NONE',  ( 78.95048871113250755, -29.99999999999999645, 188.4614743794136871 ) ) ;
#96127 = CARTESIAN_POINT ( 'NONE',  ( -108.2372990039095271, -60.00000000000000000, 115.4700740038245499 ) ) ;
#96128 = CARTESIAN_POINT ( 'NONE',  ( -62.81791404775724175, -53.39247542489125919, 86.98738384603005613 ) ) ;
#96129 = ORIENTED_EDGE ( 'NONE', *, *, #12202, .F. ) ;
#96130 = CARTESIAN_POINT ( 'NONE',  ( -63.38584389458259949, 38.95340125770254502, 6.668509187926899173 ) ) ;
#96131 = CARTESIAN_POINT ( 'NONE',  ( 80.31347780062725406, -60.00000000002691536, 200.0034699237392601 ) ) ;
#96132 = ORIENTED_EDGE ( 'NONE', *, *, #84912, .F. ) ;
#96133 = CARTESIAN_POINT ( 'NONE',  ( -16.75187969033554936, 36.38380281757302015, -24.30698433968596106 ) ) ;
#96134 = CARTESIAN_POINT ( 'NONE',  ( -5.082755093536326818, -17.09375000204838813, 5.082755093536325042 ) ) ;
#96135 = CONICAL_SURFACE ( 'NONE', #66878, 4.000000000000001776, 0.9599310885968808105 ) ;
#96136 = CARTESIAN_POINT ( 'NONE',  ( -1.469576158976823947E-15, -11.56250000409677092, 8.000000000000000000 ) ) ;
#96137 = ORIENTED_EDGE ( 'NONE', *, *, #65048, .F. ) ;
#96139 = DIRECTION ( 'NONE',  ( 0.000000000000000000, -1.000000000000000000, 0.000000000000000000 ) ) ;
#96138 = AXIS2_PLACEMENT_3D ( 'NONE', #92752, #91703, #30164 ) ;
#96140 = ORIENTED_EDGE ( 'NONE', *, *, #64416, .T. ) ;
#96141 = DIRECTION ( 'NONE',  ( -0.000000000000000000, 1.000000000000000000, -0.000000000000000000 ) ) ;
#96142 = CARTESIAN_POINT ( 'NONE',  ( -38.79830821498207172, 485.8176106091539737, -4.884814968349580511 ) ) ;
#96143 = CARTESIAN_POINT ( 'NONE',  ( -86.98208477778736381, -60.00000000000001421, -22.74275743632538749 ) ) ;
#96144 = DIRECTION ( 'NONE',  ( 0.000000000000000000, -0.5000000000000004441, 0.8660254037844383745 ) ) ;
#96145 = CARTESIAN_POINT ( 'NONE',  ( -7.188101187500002709, -26.18750000204838813, 2.977408999572648707 ) ) ;
#96146 = DIRECTION ( 'NONE',  ( -0.000000000000000000, -0.000000000000000000, -1.000000000000000000 ) ) ;
#96147 = CARTESIAN_POINT ( 'NONE',  ( -32.42271565838826319, 438.8719799267125268, 23.74906467565554991 ) ) ;
#96148 = DIRECTION ( 'NONE',  ( 0.000000000000000000, 0.000000000000000000, -1.000000000000000000 ) ) ;
#96149 = CARTESIAN_POINT ( 'NONE',  ( 9.739726766101595601, 49.99999999999999289, -87.61747884500120165 ) ) ;
#96150 = CARTESIAN_POINT ( 'NONE',  ( -4.250000000000000000, 5.204748896376250699E-16, -0.5505556536572887572 ) ) ;
#96151 = CARTESIAN_POINT ( 'NONE',  ( -37.15025629407706020, 306.0170503793525540, 0.5993149417967529313 ) ) ;
#96152 = EDGE_CURVE ( 'NONE', #14501, #39221, #57304, .T. ) ;
#96153 = CARTESIAN_POINT ( 'NONE',  ( 28.86106494938684364, 306.5463937303920261, -9.171402789936776045 ) ) ;
#96154 = CARTESIAN_POINT ( 'NONE',  ( -38.12989804336692146, -18.75727802424759361, 32.82810357043974392 ) ) ;
#96155 = EDGE_LOOP ( 'NONE', ( #3729, #53318, #76355, #106562, #22733, #43641, #33118, #95987, #3467 ) ) ;
#96156 = CARTESIAN_POINT ( 'NONE',  ( -9.655545083697493425, 53.40239499979105631, -3.405056376145797703 ) ) ;
#96157 = SURFACE_STYLE_FILL_AREA ( #72910 ) ;
#96158 = AXIS2_PLACEMENT_3D ( 'NONE', #95455, #72752, #46377 ) ;
#96159 = COLOUR_RGB ( '', 0.09019608, 0.27058824, 0.51372549) ;
#96160 = CARTESIAN_POINT ( 'NONE',  ( 35.82070543335183288, -18.72939031532795440, 31.62416683920327287 ) ) ;
#96162 = CIRCLE ( 'NONE', #20451, 4.000000000000001776 ) ;
#96161 = CARTESIAN_POINT ( 'NONE',  ( 21.65942590380565491, 2.899645552008857721E-12, 5.820808985964478488 ) ) ;
#96163 = EDGE_LOOP ( 'NONE', ( #14542, #45494, #26593, #46573 ) ) ;
#96164 = EDGE_CURVE ( 'NONE', #7054, #59047, #96167, .T. ) ;
#96165 = ADVANCED_FACE ( 'NONE', ( #40345 ), #9034, .T. ) ;
#96166 = DIRECTION ( 'NONE',  ( 0.000000000000000000, 0.000000000000000000, -1.000000000000000000 ) ) ;
#96167 = B_SPLINE_CURVE_WITH_KNOTS ( 'NONE', 3,
 ( #9558, #98049, #33880, #16067, #82400, #99641 ),
 .UNSPECIFIED., .F., .F.,
 ( 4, 1, 1, 4 ),
 ( 0.000000000000000000, 0.4213833399777465738, 0.5213833399777465516, 0.9843640123765010630 ),
 .UNSPECIFIED. ) ;
#96168 = ORIENTED_EDGE ( 'NONE', *, *, #82254, .F. ) ;
#96170 = CARTESIAN_POINT ( 'NONE',  ( -31.03867016165222026, 468.3124986733989772, 18.90871194958903345 ) ) ;
#96169 = DIRECTION ( 'NONE',  ( 0.000000000000000000, 0.000000000000000000, 1.000000000000000000 ) ) ;
#96171 = CARTESIAN_POINT ( 'NONE',  ( 16.58646281676601575, 37.15392203743714816, 21.81520449073893531 ) ) ;
#96172 = CARTESIAN_POINT ( 'NONE',  ( 6.575918192882433289, -3.850883087735915922, -6.669925161966309801 ) ) ;
#96173 = CIRCLE ( 'NONE', #49638, 4.000000000000000888 ) ;
#96174 = CARTESIAN_POINT ( 'NONE',  ( 0.7842477567516482617, 43.26537946031525195, -18.48697474366874616 ) ) ;
#96175 = CARTESIAN_POINT ( 'NONE',  ( -40.79885302902677324, 436.7553892629194365, 6.138960499427065010 ) ) ;
#96176 = CARTESIAN_POINT ( 'NONE',  ( 4.904566723942682671, -87.02242702470746849, 3.460360782932704549 ) ) ;
#96177 = CARTESIAN_POINT ( 'NONE',  ( 14.85284876471456350, 3.851859888774471706E-31, 5.000000000000001776 ) ) ;
#96178 = CARTESIAN_POINT ( 'NONE',  ( 94.32096871168523933, -60.00000000000000711, 43.89811362915176574 ) ) ;
#96179 = DIRECTION ( 'NONE',  ( 1.000000000000000000, 0.000000000000000000, -0.000000000000000000 ) ) ;
#96180 = CARTESIAN_POINT ( 'NONE',  ( 22.57792046605466041, 1.340359594676612611E-15, 0.000000000000000000 ) ) ;
#96181 = CARTESIAN_POINT ( 'NONE',  ( -43.00000000000000000, 450.0000000000002274, 13.20242257375370976 ) ) ;
#96182 = ORIENTED_EDGE ( 'NONE', *, *, #30939, .F. ) ;
#96183 = ADVANCED_FACE ( 'NONE', ( #65150 ), #86627, .T. ) ;
#96184 = STYLED_ITEM ( 'NONE', ( #69190 ), #44483 ) ;
#96185 = CARTESIAN_POINT ( 'NONE',  ( -89.94601218680125498, -30.00000000001251266, -10.37167675054645066 ) ) ;
#96186 = VERTEX_POINT ( 'NONE', #66084 ) ;
#96187 = CARTESIAN_POINT ( 'NONE',  ( 1.224646799147353256E-15, -2.000000000000000000, -10.00000000000000000 ) ) ;
#96188 = CARTESIAN_POINT ( 'NONE',  ( -16.02800152098323139, 4.194749798104338900, 2.552193233508346371 ) ) ;
#96189 = CARTESIAN_POINT ( 'NONE',  ( 3.363266691729805746, 30.68916429454045058, 5.000000000000000888 ) ) ;
#96190 = CARTESIAN_POINT ( 'NONE',  ( 32.11723263399798611, 433.0682605266380278, 24.32175648712328453 ) ) ;
#96191 = SURFACE_STYLE_USAGE ( .BOTH. , #29881 ) ;
#96192 = CARTESIAN_POINT ( 'NONE',  ( 4.401442555609581635E-16, -34.15625000204838813, -7.188101187500000044 ) ) ;
#96193 = CARTESIAN_POINT ( 'NONE',  ( -1.344569080228518650E-17, 21.85270131633358304, -7.000000000000011546 ) ) ;
#96194 = DIRECTION ( 'NONE',  ( 0.000000000000000000, 0.000000000000000000, 1.000000000000000000 ) ) ;
#96195 = EDGE_CURVE ( 'NONE', #48348, #71070, #53747, .T. ) ;
#96196 = LINE ( 'NONE', #79982, #101120 ) ;
#96197 = ORIENTED_EDGE ( 'NONE', *, *, #86941, .T. ) ;
#96198 = AXIS2_PLACEMENT_3D ( 'NONE', #20055, #53441, #36764 ) ;
#96199 = VECTOR ( 'NONE', #2624, 1000.000000000000227 ) ;
#96201 = VERTEX_POINT ( 'NONE', #1323 ) ;
#96200 = DIRECTION ( 'NONE',  ( -1.000000000000000000, -1.224606353822377258E-16, -0.000000000000000000 ) ) ;
#96202 = CARTESIAN_POINT ( 'NONE',  ( 78.40831120363421292, -56.84011713593565673, 154.9006849491204036 ) ) ;
#96203 = CARTESIAN_POINT ( 'NONE',  ( 0.000000000000000000, 0.000000000000000000, -13.00000000000000000 ) ) ;
#96204 = ORIENTED_EDGE ( 'NONE', *, *, #78132, .T. ) ;
#96205 = CARTESIAN_POINT ( 'NONE',  ( -12.50000000000000711, 39.71451000310032953, -64.87831219546262673 ) ) ;
#96206 = DIRECTION ( 'NONE',  ( 1.000000000000000000, 0.000000000000000000, 0.000000000000000000 ) ) ;
#96207 = CARTESIAN_POINT ( 'NONE',  ( 4.401442555609581635E-16, -18.78125000204838457, -7.188101187500000044 ) ) ;
#96208 =( BOUNDED_SURFACE ( )  B_SPLINE_SURFACE ( 3, 2, ( 
 ( #48135, #98291, #72937 ),
 ( #23371, #56754, #55163 ),
 ( #105845, #80500, #7148 ),
 ( #97746, #81546, #72424 ),
 ( #30944, #15248, #57282 ),
 ( #32529, #81032, #64863 ),
 ( #65400, #24449, #104794 ),
 ( #23913, #105328, #89681 ),
 ( #90205, #8215, #63288 ),
 ( #30401, #41124, #40587 ),
 ( #64354, #16305, #6621 ),
 ( #39548, #71890, #106364 ),
 ( #14172, #49196, #63821 ),
 ( #22318, #15779, #73469 ),
 ( #56209, #82096, #104255 ),
 ( #96711, #39011, #96188 ),
 ( #47076, #55681, #88614 ),
 ( #14704, #89147, #47605 ),
 ( #31471, #97222, #75064 ),
 ( #57817, #74539, #33059 ) ),
 .UNSPECIFIED., .F., .F., .F. ) 
 B_SPLINE_SURFACE_WITH_KNOTS ( ( 4, 2, 2, 2, 2, 2, 2, 2, 2, 4 ),
 ( 3, 3 ),
 ( 0.001112359326657399528, 0.002061628542460812626, 0.003010897758264225940, 0.003960166974067639255, 0.004909436189871052569, 0.005858705405674465884, 0.006807974621477879199, 0.007282609229379585422, 0.007757243837281292513, 0.008706513053084705828 ),
 ( 0.000000000000000000, 1.000000000000000000 ),
 .UNSPECIFIED. ) 
 GEOMETRIC_REPRESENTATION_ITEM ( )  RATIONAL_B_SPLINE_SURFACE ( (
 ( 1.000000000000000000, 0.9115707425106666095, 1.000000000000000000),
 ( 1.000000000000000000, 0.9186010707724077129, 1.000000000000000000),
 ( 1.000000000000000000, 0.9248333139229367728, 1.000000000000000000),
 ( 1.000000000000000000, 0.9351156329915113474, 1.000000000000000000),
 ( 1.000000000000000000, 0.9392288573274951702, 1.000000000000000000),
 ( 1.000000000000000000, 0.9457209207427998976, 1.000000000000000000),
 ( 1.000000000000000000, 0.9480998420263311299, 1.000000000000000000),
 ( 1.000000000000000000, 0.9511999291517323485, 1.000000000000000000),
 ( 1.000000000000000000, 0.9519548416862445572, 1.000000000000000000),
 ( 1.000000000000000000, 0.9519314736513598829, 1.000000000000000000),
 ( 1.000000000000000000, 0.9511539719350848854, 1.000000000000000000),
 ( 1.000000000000000000, 0.9480480161103058689, 1.000000000000000000),
 ( 1.000000000000000000, 0.9457194361326417553, 1.000000000000000000),
 ( 1.000000000000000000, 0.9408176163898155364, 1.000000000000000000),
 ( 1.000000000000000000, 0.9389456878144246676, 1.000000000000000000),
 ( 1.000000000000000000, 0.9347647373043734831, 1.000000000000000000),
 ( 1.000000000000000000, 0.9324473665771305653, 1.000000000000000000),
 ( 1.000000000000000000, 0.9247734139709412604, 1.000000000000000000),
 ( 1.000000000000000000, 0.9186884142190029356, 1.000000000000000000),
 ( 1.000000000000000000, 0.9115707425101438055, 1.000000000000000000) ) ) 
 REPRESENTATION_ITEM ( '' )  SURFACE ( )  );
#96209 = CARTESIAN_POINT ( 'NONE',  ( -29.91071955673133687, -57.68399870184025247, 45.22199076326395328 ) ) ;
#96210 = CARTESIAN_POINT ( 'NONE',  ( 12.03681039759596239, 294.5862353579262276, 9.880551326283205427 ) ) ;
#96211 = EDGE_LOOP ( 'NONE', ( #73943, #22729, #85459, #31708, #94597 ) ) ;
#96212 =( LENGTH_UNIT ( ) NAMED_UNIT ( * ) SI_UNIT ( .MILLI., .METRE. ) );
#96213 = VECTOR ( 'NONE', #530, 1000.000000000000227 ) ;
#96214 = CARTESIAN_POINT ( 'NONE',  ( 41.85000000000000142, 3.309500000000003439, 0.000000000000000000 ) ) ;
#96215 = CARTESIAN_POINT ( 'NONE',  ( -5.999511540169428336, -13.99926730885433557, -0.2833228702578364788 ) ) ;
#96216 = PRESENTATION_LAYER_ASSIGNMENT (  '', '', ( #101367 ) ) ;
#96217 = CARTESIAN_POINT ( 'NONE',  ( 6.738100180926640093, 41.71798714554645215, -59.05424661244425266 ) ) ;
#96218 = DIRECTION ( 'NONE',  ( 0.000000000000000000, 0.000000000000000000, 1.000000000000000000 ) ) ;
#96219 = CARTESIAN_POINT ( 'NONE',  ( 8.000000000000000000, -9.687500004096769146, 0.000000000000000000 ) ) ;
#96221 = B_SPLINE_CURVE_WITH_KNOTS ( 'NONE', 3,
 ( #2094, #25914, #93252, #33985, #58770, #92173, #51176, #99196 ),
 .UNSPECIFIED., .F., .F.,
 ( 4, 2, 2, 4 ),
 ( 0.000000000000000000, 0.001013125157727799708, 0.002026250315455599416, 0.004052500630911192760 ),
 .UNSPECIFIED. ) ;
#96220 = CARTESIAN_POINT ( 'NONE',  ( -10.70060044141619215, -13.94213797727864623, 31.85821448878728290 ) ) ;
#96222 = DIRECTION ( 'NONE',  ( -1.000000000000000000, -1.224606353822377258E-16, -0.000000000000000000 ) ) ;
#96223 = CIRCLE ( 'NONE', #2954, 5.000000000000002665 ) ;
#96224 = DIRECTION ( 'NONE',  ( -1.000000000000000000, -1.224606353822377258E-16, -0.000000000000000000 ) ) ;
#96225 = PRESENTATION_LAYER_ASSIGNMENT (  '', '', ( #8360 ) ) ;
#96226 = CARTESIAN_POINT ( 'NONE',  ( 7.141975279388227626, -3.000000000000119016, -70.98863559356006192 ) ) ;
#96227 = FACE_OUTER_BOUND ( 'NONE', #77994, .T. ) ;
#96228 = APPLICATION_PROTOCOL_DEFINITION ( 'draft international standard', 'automotive_design', 1998, #76878 ) ;
#96229 = CARTESIAN_POINT ( 'NONE',  ( -9.645512969475854348, 33.01103150675724152, -2.645801731561393311 ) ) ;
#96230 = ORIENTED_EDGE ( 'NONE', *, *, #65217, .T. ) ;
#96231 = CARTESIAN_POINT ( 'NONE',  ( 11.53817350584529144, 43.34042535094782522, 14.20050555370484169 ) ) ;
#96232 = CARTESIAN_POINT ( 'NONE',  ( -3.316968746324298500, 15.92795519102023860, 9.435590127032945418 ) ) ;
#96233 = CARTESIAN_POINT ( 'NONE',  ( -37.62251730745840916, 437.3427388312646258, 4.535622330043208805 ) ) ;
#96234 = CARTESIAN_POINT ( 'NONE',  ( 60.33857676659169300, -29.90340425700747673, -32.82934671700747487 ) ) ;
#96235 = CARTESIAN_POINT ( 'NONE',  ( -81.32146438466961058, -29.99999999999999645, 141.8559041851008828 ) ) ;
#96236 = CARTESIAN_POINT ( 'NONE',  ( 7.500000000000008882, 42.00000000000000711, -72.67206406577979294 ) ) ;
#96237 = EDGE_CURVE ( 'NONE', #35664, #90336, #46919, .T. ) ;
#96238 = VERTEX_POINT ( 'NONE', #42340 ) ;
#96239 = AXIS2_PLACEMENT_3D ( 'NONE', #53685, #103311, #95745 ) ;
#96240 = CARTESIAN_POINT ( 'NONE',  ( 0.08285530294364995552, 1.570896314703521091, -8.000000000000000000 ) ) ;
#96241 = CARTESIAN_POINT ( 'NONE',  ( 96.78308981908668329, -57.62245937922295980, 204.4637576706275581 ) ) ;
#96242 = AXIS2_PLACEMENT_3D ( 'NONE', #94549, #70256, #68124 ) ;
#96243 = CARTESIAN_POINT ( 'NONE',  ( 66.87521826036821437, -21.77028756581515623, -20.76402545033162284 ) ) ;
#96244 = ADVANCED_FACE ( 'NONE', ( #50947 ), #34825, .T. ) ;
#96245 = MECHANICAL_DESIGN_GEOMETRIC_PRESENTATION_REPRESENTATION (  '', ( #1497 ), #70449 ) ;
#96246 = ADVANCED_FACE ( 'NONE', ( #67161 ), #67383, .F. ) ;
#96247 = ADVANCED_FACE ( 'NONE', ( #83327 ), #64194, .T. ) ;
#96248 = CARTESIAN_POINT ( 'NONE',  ( 37.67124221001551376, 463.6239404278543361, 19.49545380201367450 ) ) ;
#96249 = CARTESIAN_POINT ( 'NONE',  ( -15.79792377994584029, 22.78987439203835308, 0.2434392984178747332 ) ) ;
#96250 = CARTESIAN_POINT ( 'NONE',  ( 0.08224679563971126761, -6.145890662064649845, 5.355005115540901528 ) ) ;
#96251 = CARTESIAN_POINT ( 'NONE',  ( -72.04520221236295185, -60.00000000000000711, 154.6154111227524766 ) ) ;
#96252 = MECHANICAL_DESIGN_GEOMETRIC_PRESENTATION_REPRESENTATION (  '', ( #106612 ), #87620 ) ;
#96253 = FACE_BOUND ( 'NONE', #44796, .T. ) ;
#96254 = CARTESIAN_POINT ( 'NONE',  ( 93.97977184163765685, 5.000000000000020428, 0.000000000000000000 ) ) ;
#96255 = EDGE_CURVE ( 'NONE', #85724, #23116, #50417, .T. ) ;
#96256 = CARTESIAN_POINT ( 'NONE',  ( 62.91825180719526145, 50.00000000000000000, 6.605622457241173251 ) ) ;
#96257 = CARTESIAN_POINT ( 'NONE',  ( -85.04220142028198381, -50.19910149378929276, 189.2836192048938244 ) ) ;
#96258 = VERTEX_POINT ( 'NONE', #2407 ) ;
#96259 = CARTESIAN_POINT ( 'NONE',  ( 35.53901217317436334, 397.0550940254831289, 6.925270274446173602 ) ) ;
#96260 = ADVANCED_FACE ( 'NONE', ( #42875 ), #68003, .T. ) ;
#96261 = CARTESIAN_POINT ( 'NONE',  ( -7.801339272325197527, -13.58731471959700521, -1.788609912539669944 ) ) ;
#96262 = SURFACE_SIDE_STYLE ('',( #5633 ) ) ;
#96263 = CARTESIAN_POINT ( 'NONE',  ( 0.000000000000000000, 0.000000000000000000, -1.876475477074182940 ) ) ;
#96264 = DIRECTION ( 'NONE',  ( -1.000000000000000000, -1.224606353822377258E-16, -0.000000000000000000 ) ) ;
#96265 = AXIS2_PLACEMENT_3D ( 'NONE', #55459, #105618, #15008 ) ;
#96266 = ORIENTED_EDGE ( 'NONE', *, *, #74293, .T. ) ;
#96267 = DIRECTION ( 'NONE',  ( 0.000000000000000000, -1.000000000000000000, 0.000000000000000000 ) ) ;
#96268 = CARTESIAN_POINT ( 'NONE',  ( 0.000000000000000000, 195.0000000000000000, -7.000000000000011546 ) ) ;
#96269 = CARTESIAN_POINT ( 'NONE',  ( -24.56594385547996140, -4.285714285713227767, 6.601913983196856073 ) ) ;
#96270 = AXIS2_PLACEMENT_3D ( 'NONE', #46546, #12043, #30387 ) ;
#96271 = CARTESIAN_POINT ( 'NONE',  ( 21.36650669486618881, 1.474610560812782335E-15, 0.000000000000000000 ) ) ;
#96272 = CIRCLE ( 'NONE', #58373, 10.00000000000000178 ) ;
#96273 = CARTESIAN_POINT ( 'NONE',  ( 84.17695284478443796, -14.21045842199441367, -18.06956050794424584 ) ) ;
#96274 = CARTESIAN_POINT ( 'NONE',  ( -78.12100248001522118, -56.84623792800805120, 152.8030804558065938 ) ) ;
#96275 = ORIENTED_EDGE ( 'NONE', *, *, #79657, .F. ) ;
#96276 = CARTESIAN_POINT ( 'NONE',  ( 24.48575568784926304, -14.21045842199439946, 35.52093559979998361 ) ) ;
#96277 = DIRECTION ( 'NONE',  ( -1.000000000000000000, -1.224606353822377258E-16, -0.000000000000000000 ) ) ;
#96278 = CARTESIAN_POINT ( 'NONE',  ( 106.0311746394521037, -57.64931060779116478, 200.9292066482266534 ) ) ;
#96279 =( REPRESENTATION_RELATIONSHIP ('NONE','NONE', #69581, #70207 ) REPRESENTATION_RELATIONSHIP_WITH_TRANSFORMATION ( #35221 )SHAPE_REPRESENTATION_RELATIONSHIP( ) );
#96280 = CARTESIAN_POINT ( 'NONE',  ( 50.32385735845999619, 50.00000000000000711, 38.04681602700239296 ) ) ;
#96282 = AXIS2_PLACEMENT_3D ( 'NONE', #95460, #69079, #20580 ) ;
#96281 = CARTESIAN_POINT ( 'NONE',  ( 40.07510820939334906, 310.1680218437383019, -6.385417175660951905 ) ) ;
#96283 = CARTESIAN_POINT ( 'NONE',  ( 0.5805565836007643421, -3.752776749732575468, -6.499999999999999112 ) ) ;
#96284 = ORIENTED_EDGE ( 'NONE', *, *, #46803, .T. ) ;
#96285 = FACE_OUTER_BOUND ( 'NONE', #73726, .T. ) ;
#96287 = CARTESIAN_POINT ( 'NONE',  ( -103.3976274097190071, -52.71035023079828363, 146.8235736524452193 ) ) ;
#96286 = CARTESIAN_POINT ( 'NONE',  ( -16.41900535493362412, 37.18348077072296576, 21.84048156162998922 ) ) ;
#96288 = CARTESIAN_POINT ( 'NONE',  ( -7.188101187500002709, -22.81250000204838813, 2.977408999572648707 ) ) ;
#96289 = CARTESIAN_POINT ( 'NONE',  ( -30.00000000000000000, -54.00000000000000711, 31.11721482942554928 ) ) ;
#96290 = DIRECTION ( 'NONE',  ( -1.000000000000000000, -0.000000000000000000, -0.000000000000000000 ) ) ;
#96291 = CARTESIAN_POINT ( 'NONE',  ( 6.916165809215955917, 41.81554757990602411, -59.83173451229081508 ) ) ;
#96292 = CARTESIAN_POINT ( 'NONE',  ( -5.412925220531727533, 41.84428781238603534, -58.95471249783204115 ) ) ;
#96293 = CARTESIAN_POINT ( 'NONE',  ( 0.000000000000000000, 0.000000000000000000, -8.900000000000000355 ) ) ;
#96295 = CARTESIAN_POINT ( 'NONE',  ( 17.81883034442599012, 43.26653065284484256, -4.974467122015703069 ) ) ;
#96294 = CIRCLE ( 'NONE', #85987, 12.50000000000000000 ) ;
#96296 = ORIENTED_EDGE ( 'NONE', *, *, #64504, .F. ) ;
#96297 = DIRECTION ( 'NONE',  ( 0.000000000000000000, 1.000000000000000000, 0.000000000000000000 ) ) ;
#96299 = CARTESIAN_POINT ( 'NONE',  ( 24.76367760800922113, -35.99787462728398424, 31.10278417371337767 ) ) ;
#96298 = CARTESIAN_POINT ( 'NONE',  ( 0.1306530452038101031, 7.903938623646867612, 2.309976723937613663 ) ) ;
#96300 = CARTESIAN_POINT ( 'NONE',  ( -23.55017320447252871, 25.19299454758883527, 33.17279571835358354 ) ) ;
#96301 = EDGE_LOOP ( 'NONE', ( #58716, #50223, #46345, #72535, #89655 ) ) ;
#96302 = EDGE_CURVE ( 'NONE', #61410, #25935, #99958, .T. ) ;
#96303 = ORIENTED_EDGE ( 'NONE', *, *, #3212, .F. ) ;
#96304 = FACE_BOUND ( 'NONE', #70330, .T. ) ;
#96305 = CARTESIAN_POINT ( 'NONE',  ( 7.343811558498933856, 40.90986947426189602, -58.79603989316886725 ) ) ;
#96306 =( NAMED_UNIT ( * ) PLANE_ANGLE_UNIT ( ) SI_UNIT ( $, .RADIAN. ) );
#96307 = CARTESIAN_POINT ( 'NONE',  ( 0.000000000000000000, 0.000000000000000000, 0.000000000000000000 ) ) ;
#96308 = DIRECTION ( 'NONE',  ( 0.000000000000000000, 1.000000000000000000, 0.000000000000000000 ) ) ;
#96309 = ORIENTED_EDGE ( 'NONE', *, *, #43375, .T. ) ;
#96310 = CONICAL_SURFACE ( 'NONE', #86005, 4.172000000000009479, 0.9599310885968813656 ) ;
#96311 = CARTESIAN_POINT ( 'NONE',  ( 49.72939441809057115, -60.00000000000001421, -37.95769542429952281 ) ) ;
#96312 = CARTESIAN_POINT ( 'NONE',  ( 22.59032126178805200, 25.42946310086070483, -33.04941538723348060 ) ) ;
#96313 = CARTESIAN_POINT ( 'NONE',  ( -10.28098872167596056, 16.62144220248768534, -10.01918470399412797 ) ) ;
#96314 = CARTESIAN_POINT ( 'NONE',  ( 28.86650669486618881, 1.474610560812782335E-15, 0.000000000000000000 ) ) ;
#96315 = CARTESIAN_POINT ( 'NONE',  ( -12.00013170160833731, -5.000000000000000000, -83.40936345630457538 ) ) ;
#96316 = EDGE_CURVE ( 'NONE', #11400, #696, #102657, .T. ) ;
#96317 = DIRECTION ( 'NONE',  ( -1.000000000000000000, -0.000000000000000000, -0.000000000000000000 ) ) ;
#96318 = VERTEX_POINT ( 'NONE', #69812 ) ;
#96319 = ORIENTED_EDGE ( 'NONE', *, *, #7549, .T. ) ;
#96320 = ORIENTED_EDGE ( 'NONE', *, *, #20879, .T. ) ;
#96321 = LINE ( 'NONE', #38619, #15923 ) ;
#96322 = DIRECTION ( 'NONE',  ( 0.000000000000000000, 0.5000000000000007772, -0.8660254037844381525 ) ) ;
#96323 = CARTESIAN_POINT ( 'NONE',  ( -36.47142920048730019, 28.20086854896861084, 11.58052048957462965 ) ) ;
#96324 = CARTESIAN_POINT ( 'NONE',  ( 64.78349330513380266, -1.232595164407830946E-29, 4.000000000000007105 ) ) ;
#96325 = CARTESIAN_POINT ( 'NONE',  ( 0.000000000000000000, 0.000000000000000000, -8.500000000000000000 ) ) ;
#96327 = CARTESIAN_POINT ( 'NONE',  ( -44.07637885077937057, 485.1585573880434481, 0.4493611555661314871 ) ) ;
#96326 = AXIS2_PLACEMENT_3D ( 'NONE', #4670, #54784, #29510 ) ;
#96328 = DIRECTION ( 'NONE',  ( -1.000000000000000000, 0.000000000000000000, 0.000000000000000000 ) ) ;
#96329 = ORIENTED_EDGE ( 'NONE', *, *, #105947, .F. ) ;
#96330 = CARTESIAN_POINT ( 'NONE',  ( 9.999999999999994671, 48.00000000000000000, -83.69100306252322241 ) ) ;
#96331 = VERTEX_POINT ( 'NONE', #94643 ) ;
#96332 = DIRECTION ( 'NONE',  ( -0.000000000000000000, -0.000000000000000000, -1.000000000000000000 ) ) ;
#96333 = CARTESIAN_POINT ( 'NONE',  ( 32.89533925684071392, 465.6911419323517975, 10.83014164272718638 ) ) ;
#96334 = CARTESIAN_POINT ( 'NONE',  ( -40.98863139543954048, 485.5630605922909808, -4.100416933089532812 ) ) ;
#96335 = AXIS2_PLACEMENT_3D ( 'NONE', #84686, #36183, #3778 ) ;
#96336 = AXIS2_PLACEMENT_3D ( 'NONE', #11347, #12418, #61006 ) ;
#96337 = ADVANCED_FACE ( 'NONE', ( #22355 ), #53621, .T. ) ;
#96338 = CARTESIAN_POINT ( 'NONE',  ( -80.12203077669109064, -60.00000000000006395, 175.6696548227984351 ) ) ;
#96339 = CARTESIAN_POINT ( 'NONE',  ( 62.81860187692696229, -53.38668648289181107, 86.98641772761070001 ) ) ;
#96340 = ORIENTED_EDGE ( 'NONE', *, *, #104047, .F. ) ;
#96341 = CARTESIAN_POINT ( 'NONE',  ( 37.54559764570580427, 464.1143081516195821, 19.43664670202559464 ) ) ;
#96342 = FACE_OUTER_BOUND ( 'NONE', #28076, .T. ) ;
#96343 = DIRECTION ( 'NONE',  ( -0.000000000000000000, -1.000000000000000000, -0.000000000000000000 ) ) ;
#96344 = CYLINDRICAL_SURFACE ( 'NONE', #91167, 2.000000000000001776 ) ;
#96345 = ORIENTED_EDGE ( 'NONE', *, *, #17173, .F. ) ;
#96346 = SURFACE_STYLE_USAGE ( .BOTH. , #54786 ) ;
#96347 = CARTESIAN_POINT ( 'NONE',  ( 46.83658167332238520, 18.87978240383752748, 15.22028160905541228 ) ) ;
#96348 = CARTESIAN_POINT ( 'NONE',  ( 72.07940662483305516, -59.99999999999998579, -25.51851818892304635 ) ) ;
#96349 = DIRECTION ( 'NONE',  ( 0.000000000000000000, 0.000000000000000000, 1.000000000000000000 ) ) ;
#96350 = CARTESIAN_POINT ( 'NONE',  ( -8.000000000000001776, -31.34375000409677270, 3.313708498984758943 ) ) ;
#96351 = CARTESIAN_POINT ( 'NONE',  ( 8.922269033010996608, -5.000000000000000000, -5.219866590717683330 ) ) ;
#96352 = CARTESIAN_POINT ( 'NONE',  ( 86.50032125490628232, -17.01892177610816859, 184.1023120340136359 ) ) ;
#96353 = STYLED_ITEM ( 'NONE', ( #64444 ), #31924 ) ;
#96354 = CARTESIAN_POINT ( 'NONE',  ( -5.288744022479204610, 17.47836613358154878, -36.94789734229802747 ) ) ;
#96355 = UNCERTAINTY_MEASURE_WITH_UNIT (LENGTH_MEASURE( 1.000000000000000082E-05 ), #38133, 'distance_accuracy_value', 'NONE');
#96356 = CARTESIAN_POINT ( 'NONE',  ( -3.574667317769504749, 23.87472662520894318, 5.000000000000000888 ) ) ;
#96357 = CARTESIAN_POINT ( 'NONE',  ( -3.220999722221654600E-16, 7.895640089090876224, -6.564402953523721607 ) ) ;
#96358 =( LENGTH_UNIT ( ) NAMED_UNIT ( * ) SI_UNIT ( .MILLI., .METRE. ) );
#96359 = SURFACE_STYLE_USAGE ( .BOTH. , #31624 ) ;
#96360 = DIRECTION ( 'NONE',  ( -1.000000000000000000, -1.224606353822377258E-16, -0.000000000000000000 ) ) ;
#96361 = CARTESIAN_POINT ( 'NONE',  ( 0.000000000000000000, 5.629165124598842773, -3.250000000000011990 ) ) ;
#96362 = CARTESIAN_POINT ( 'NONE',  ( 29.59573307755961480, -59.99999999999998579, 42.83999512026873902 ) ) ;
#96363 = CARTESIAN_POINT ( 'NONE',  ( -99.16875731687827056, -30.00000000000000000, 146.3660697992883968 ) ) ;
#96364 = PRESENTATION_LAYER_ASSIGNMENT (  '', '', ( #75706 ) ) ;
#96365 = EDGE_CURVE ( 'NONE', #8358, #61384, #48750, .T. ) ;
#96366 = DIRECTION ( 'NONE',  ( -0.000000000000000000, -1.000000000000000000, -0.000000000000000000 ) ) ;
#96367 = CARTESIAN_POINT ( 'NONE',  ( 44.76088533861224761, -57.68343184253352263, 64.64529994903629984 ) ) ;
#96369 = DIRECTION ( 'NONE',  ( 0.000000000000000000, 1.000000000000000000, 0.000000000000000000 ) ) ;
#96368 = CARTESIAN_POINT ( 'NONE',  ( -1.007187577324624161, 25.34754566897618133, -40.24471185633667147 ) ) ;
#96370 = EDGE_CURVE ( 'NONE', #95728, #56342, #29873, .T. ) ;
#96371 = EDGE_CURVE ( 'NONE', #54845, #15011, #29338, .T. ) ;
#96373 = CARTESIAN_POINT ( 'NONE',  ( -41.31850805822637085, 460.1795573263363508, 2.184907985914082307 ) ) ;
#96372 = CIRCLE ( 'NONE', #43008, 5.000000000000001776 ) ;
#96374 = CARTESIAN_POINT ( 'NONE',  ( -17.60285536070160717, 50.00000000000000000, 62.67515953917209259 ) ) ;
#96375 = FACE_OUTER_BOUND ( 'NONE', #85328, .T. ) ;
#96376 = CARTESIAN_POINT ( 'NONE',  ( -15.78091564468949848, -59.99999999999999289, 39.83881286635372732 ) ) ;
#96377 = DIRECTION ( 'NONE',  ( -1.000000000000000000, -1.224606353822377258E-16, -0.000000000000000000 ) ) ;
#96378 = CARTESIAN_POINT ( 'NONE',  ( -87.07081158247649455, -24.31846254880739266, 186.7358293699816727 ) ) ;
#96379 = VERTEX_POINT ( 'NONE', #40097 ) ;
#96380 = CARTESIAN_POINT ( 'NONE',  ( 17.50000000000003197, 50.00117660290610644, 59.93398959461712394 ) ) ;
#96381 =( LENGTH_UNIT ( ) NAMED_UNIT ( * ) SI_UNIT ( .MILLI., .METRE. ) );
#96382 = CARTESIAN_POINT ( 'NONE',  ( -15.83958888108630703, -49.92074823066483447, 32.40208527561495089 ) ) ;
#96383 = ADVANCED_FACE ( 'NONE', ( #9698 ), #31561, .T. ) ;
#96385 = CARTESIAN_POINT ( 'NONE',  ( 0.000000000000000000, 0.000000000000000000, -4.567799999999999194 ) ) ;
#96384 = CARTESIAN_POINT ( 'NONE',  ( -87.01178792140694895, -60.00000000000005684, -6.909150771205774255 ) ) ;
#96386 = VERTEX_POINT ( 'NONE', #75506 ) ;
#96387 = CARTESIAN_POINT ( 'NONE',  ( 0.000000000000000000, 0.000000000000000000, 4.000000000000000000 ) ) ;
#96388 = CARTESIAN_POINT ( 'NONE',  ( 14.83882035797308419, 4.620392632310701408, -5.701545570399354723 ) ) ;
#96389 = CARTESIAN_POINT ( 'NONE',  ( -13.43923917260470802, 42.84657065243760599, -92.02410076267699424 ) ) ;
#96390 = CARTESIAN_POINT ( 'NONE',  ( 15.46466052604960595, 2.715844537110140955, -1.564829471087903379 ) ) ;
#96391 = CARTESIAN_POINT ( 'NONE',  ( 72.07854270695700905, -60.00000000000000000, 154.8658330893785546 ) ) ;
#96392 = FACE_OUTER_BOUND ( 'NONE', #13043, .T. ) ;
#96393 = EDGE_LOOP ( 'NONE', ( #65859, #44401, #78698, #95661 ) ) ;
#96394 = CARTESIAN_POINT ( 'NONE',  ( -4.931706463495239667, -29.99999999999998579, 5.709552341500299555 ) ) ;
#96395 = DIRECTION ( 'NONE',  ( 0.000000000000000000, 1.000000000000000000, 0.000000000000000000 ) ) ;
#96397 = CARTESIAN_POINT ( 'NONE',  ( 6.821510612526563655, 41.53001914900257674, -70.37925568709802349 ) ) ;
#96396 = CARTESIAN_POINT ( 'NONE',  ( 48.80991865481109215, -14.21045842199436215, 55.83985330155353921 ) ) ;
#96398 = PRESENTATION_STYLE_ASSIGNMENT (( #30610 ) ) ;
#96399 = SURFACE_SIDE_STYLE ('',( #63500 ) ) ;
#96400 = EDGE_LOOP ( 'NONE', ( #16851, #20891, #99513, #31777, #55420 ) ) ;
#96401 = VERTEX_POINT ( 'NONE', #34563 ) ;
#96402 = CARTESIAN_POINT ( 'NONE',  ( -29.57905231772367216, 319.3810052452713535, 13.75938574405086179 ) ) ;
#96403 = ORIENTED_EDGE ( 'NONE', *, *, #16924, .T. ) ;
#96404 = DIRECTION ( 'NONE',  ( 0.5735764363510470476, -0.8191520442889911324, 1.003171929053524007E-16 ) ) ;
#96405 = DIRECTION ( 'NONE',  ( 0.000000000000000000, -1.000000000000000000, 0.000000000000000000 ) ) ;
#96406 = ORIENTED_EDGE ( 'NONE', *, *, #19204, .F. ) ;
#96407 = FILL_AREA_STYLE ('',( #20966 ) ) ;
#96408 = CARTESIAN_POINT ( 'NONE',  ( 4.999999999999999112, -12.54465221550629472, 8.223849511754998787 ) ) ;
#96409 = MECHANICAL_DESIGN_GEOMETRIC_PRESENTATION_REPRESENTATION (  '', ( #36157 ), #58528 ) ;
#96410 = CARTESIAN_POINT ( 'NONE',  ( -109.0008218237458379, -59.99999999999387512, 198.3904110863214498 ) ) ;
#96411 = CARTESIAN_POINT ( 'NONE',  ( 46.00000000000568434, 486.1435775019263019, 2.115062948001753984 ) ) ;
#96412 = VECTOR ( 'NONE', #67163, 1000.000000000000000 ) ;
#96413 = CARTESIAN_POINT ( 'NONE',  ( 42.98998915891669981, -59.99999999999998579, 56.82525478121357310 ) ) ;
#96414 = CARTESIAN_POINT ( 'NONE',  ( -10.00000000000000355, 105.0000000000000000, -4.000000000000001776 ) ) ;
#96415 = CARTESIAN_POINT ( 'NONE',  ( 1.249985938038163935, 25.55829499317779607, -39.65856465433250122 ) ) ;
#96417 = CARTESIAN_POINT ( 'NONE',  ( 12.26502348511670171, -29.02967927662671599, 28.77873360239995648 ) ) ;
#96416 = CARTESIAN_POINT ( 'NONE',  ( -109.0818456041877766, -30.00000000000003908, 182.6288557207085148 ) ) ;
#96418 = CARTESIAN_POINT ( 'NONE',  ( 84.67820983338387464, -37.99999999999997158, 42.84007939968466161 ) ) ;
#96419 = CARTESIAN_POINT ( 'NONE',  ( -7.350717716529898027, 52.09114849985863316, 3.138633237920497088 ) ) ;
#96420 = ADVANCED_FACE ( 'NONE', ( #88647 ), #26418, .T. ) ;
#96421 = CARTESIAN_POINT ( 'NONE',  ( -45.65210561564843772, -53.35409427601360477, 48.30568668782035502 ) ) ;
#96422 = CARTESIAN_POINT ( 'NONE',  ( -1.101843165701975602, 34.39665841235530053, -29.11167040375564952 ) ) ;
#96423 = ORIENTED_EDGE ( 'NONE', *, *, #73428, .T. ) ;
#96424 = CARTESIAN_POINT ( 'NONE',  ( 0.8429065489285075818, 8.500928503492241717, -51.42638058623190744 ) ) ;
#96425 = PRESENTATION_STYLE_ASSIGNMENT (( #63527 ) ) ;
#96426 = CARTESIAN_POINT ( 'NONE',  ( 4.658465013329191606, -8.676361203269085109, 3.783534922165391112 ) ) ;
#96427 = CARTESIAN_POINT ( 'NONE',  ( 20.24579557674108088, 304.8297271373347144, -10.00469232190996749 ) ) ;
#96428 = ORIENTED_EDGE ( 'NONE', *, *, #31487, .T. ) ;
#96429 = CARTESIAN_POINT ( 'NONE',  ( -14.61009150661556255, -7.492150338152962163, 13.00688103712339050 ) ) ;
#96430 = EDGE_LOOP ( 'NONE', ( #60564, #32276, #73317, #48536 ) ) ;
#96431 = CARTESIAN_POINT ( 'NONE',  ( 79.03822195096249459, -29.99999999999494804, 187.3972024871379176 ) ) ;
#96432 = CARTESIAN_POINT ( 'NONE',  ( 5.682852296829431715, 41.94661659677129961, -59.19459671036732118 ) ) ;
#96433 = CARTESIAN_POINT ( 'NONE',  ( 100.3334076089338112, -30.00000000000000000, 183.9054159315834909 ) ) ;
#96434 = EDGE_CURVE ( 'NONE', #54191, #30765, #12865, .T. ) ;
#96435 = CARTESIAN_POINT ( 'NONE',  ( -1.093036222098963561, 36.52507611590718284, 29.11179518116718512 ) ) ;
#96436 = VERTEX_POINT ( 'NONE', #47639 ) ;
#96437 = CIRCLE ( 'NONE', #31014, 4.172000000000001485 ) ;
#96438 = ORIENTED_EDGE ( 'NONE', *, *, #99267, .F. ) ;
#96439 = ORIENTED_EDGE ( 'NONE', *, *, #36645, .T. ) ;
#96440 = CARTESIAN_POINT ( 'NONE',  ( -27.10511071441182906, 36.60571256639526894, 10.05698433968618488 ) ) ;
#96441 = CARTESIAN_POINT ( 'NONE',  ( 21.67692307692307452, 4.172000000000003261, 5.109226446042759579E-16 ) ) ;
#96442 = CARTESIAN_POINT ( 'NONE',  ( 11.93255308427328565, 294.5886021379643580, 9.881054392645332030 ) ) ;
#96443 = ORIENTED_EDGE ( 'NONE', *, *, #83243, .T. ) ;
#96444 = CARTESIAN_POINT ( 'NONE',  ( 0.000000000000000000, 45.50000000000000711, 0.000000000000000000 ) ) ;
#96445 = AXIS2_PLACEMENT_3D ( 'NONE', #66968, #34628, #68569 ) ;
#96446 = EDGE_LOOP ( 'NONE', ( #15582, #70443, #100175, #55630, #83700 ) ) ;
#96447 = FACE_OUTER_BOUND ( 'NONE', #10247, .T. ) ;
#96448 = CARTESIAN_POINT ( 'NONE',  ( 100.3166457666017237, -38.46339582723162920, 200.4016571423995856 ) ) ;
#96449 = DIRECTION ( 'NONE',  ( 0.000000000000000000, 0.000000000000000000, 1.000000000000000000 ) ) ;
#96450 = CARTESIAN_POINT ( 'NONE',  ( 84.45185607837281339, -45.28786482119996748, -4.595507990911970708 ) ) ;
#96451 = CARTESIAN_POINT ( 'NONE',  ( 61.29076810083007842, -38.00000000000000711, 74.90883847999660361 ) ) ;
#96452 = CARTESIAN_POINT ( 'NONE',  ( 28.40426897693866692, 310.0622289480394898, 11.65337055426186907 ) ) ;
#96453 = EDGE_CURVE ( 'NONE', #64087, #106581, #100311, .T. ) ;
#96454 = STYLED_ITEM ( 'NONE', ( #82167 ), #70542 ) ;
#96455 = CARTESIAN_POINT ( 'NONE',  ( -42.57704743493907529, 486.1612337113410831, 7.852296464539637810 ) ) ;
#96456 = B_SPLINE_CURVE_WITH_KNOTS ( 'NONE', 3,
 ( #52030, #69820, #84940, #5086, #27282, #68777, #11029, #87078, #45558, #43947, #102179, #45030, #86028, #4553, #27816, #77914, #38019, #12099, #20794, #94649, #60685, #76837, #61205, #93573, #20258, #12621, #44492, #4024, #2946 ),
 .UNSPECIFIED., .F., .F.,
 ( 4, 2, 2, 2, 2, 1, 2, 2, 2, 2, 2, 1, 1, 2, 2, 4 ),
 ( 0.000000000000000000, 0.2500000000000769385, 0.3750000000001154077, 0.4375000000001358358, 0.4687500000001451061, 0.4843750000001488809, 0.4921875000001501577, 0.5000000000001513234, 0.6250000000001735279, 0.6875000000001847411, 0.7187500000001917355, 0.7343750000001952882, 0.7421875000001948441, 0.7460937500001922906, 0.7500000000001897371, 1.000000000000000000 ),
 .UNSPECIFIED. ) ;
#96457 =( NAMED_UNIT ( * ) SI_UNIT ( $, .STERADIAN. ) SOLID_ANGLE_UNIT ( ) );
#96458 = CARTESIAN_POINT ( 'NONE',  ( 58.18888888888888999, -3.309500000000000774, 4.475777889183797681E-16 ) ) ;
#96459 = ORIENTED_EDGE ( 'NONE', *, *, #8144, .F. ) ;
#96460 = EDGE_CURVE ( 'NONE', #31698, #4323, #34963, .T. ) ;
#96461 = CARTESIAN_POINT ( 'NONE',  ( -5.000000000000000000, 0.000000000000000000, -5.710657142857142432 ) ) ;
#96462 = DIRECTION ( 'NONE',  ( -1.000000000000000000, -0.000000000000000000, -0.000000000000000000 ) ) ;
#96463 = DIRECTION ( 'NONE',  ( 1.000000000000000000, 1.224606353822377258E-16, 0.000000000000000000 ) ) ;
#96464 = VERTEX_POINT ( 'NONE', #25956 ) ;
#96465 = FACE_OUTER_BOUND ( 'NONE', #70375, .T. ) ;
#96466 = CARTESIAN_POINT ( 'NONE',  ( -25.39099590404848428, 304.9312849039644107, 10.40030929671710069 ) ) ;
#96467 = DIRECTION ( 'NONE',  ( 0.000000000000000000, -1.000000000000000000, 0.000000000000000000 ) ) ;
#96468 = CARTESIAN_POINT ( 'NONE',  ( -1.469576158976823947E-15, -14.37499999999999112, 8.000000000000000000 ) ) ;
#96469 = CARTESIAN_POINT ( 'NONE',  ( -41.97394556256499953, -29.24123356747789160, 50.03082711761693702 ) ) ;
#96470 = VECTOR ( 'NONE', #1189, 1000.000000000000000 ) ;
#96471 = FILL_AREA_STYLE_COLOUR ( '', #36423 ) ;
#96472 = ORIENTED_EDGE ( 'NONE', *, *, #69354, .F. ) ;
#96473 = CARTESIAN_POINT ( 'NONE',  ( 84.97747700260335080, -42.94964189027161439, 185.6624707830199554 ) ) ;
#96474 = LINE ( 'NONE', #102431, #60193 ) ;
#96475 = CARTESIAN_POINT ( 'NONE',  ( 3.714954396655703928, -1.055462661311022288, 103.2971887958214836 ) ) ;
#96476 = VERTEX_POINT ( 'NONE', #91707 ) ;
#96477 = CARTESIAN_POINT ( 'NONE',  ( 94.40184081913845660, -57.67114072026561900, -0.1777694819485469147 ) ) ;
#96478 = CARTESIAN_POINT ( 'NONE',  ( 36.74148664940358344, 437.9559008978175143, 4.252305828303436286 ) ) ;
#96479 = CARTESIAN_POINT ( 'NONE',  ( 1.757245493114544477, -4.333298119783830060, 17.83319508841386281 ) ) ;
#96480 = CARTESIAN_POINT ( 'NONE',  ( 51.48757442383973881, 38.95383793068620548, -37.45149417477089315 ) ) ;
#96481 = CIRCLE ( 'NONE', #3477, 12.00000000000001066 ) ;
#96482 = DIRECTION ( 'NONE',  ( 0.000000000000000000, 0.000000000000000000, 1.000000000000000000 ) ) ;
#96483 = CARTESIAN_POINT ( 'NONE',  ( 58.67238219402268840, 4.000000000000013323, 0.000000000000000000 ) ) ;
#96486 = CARTESIAN_POINT ( 'NONE',  ( -14.21654614743226652, 4.166308247385542174, 4.746652844242380098 ) ) ;
#96485 = CIRCLE ( 'NONE', #5246, 13.99700487351915612 ) ;
#96484 = CARTESIAN_POINT ( 'NONE',  ( 42.59877891056748922, 471.6664475130272081, 11.88903271301921727 ) ) ;
#96487 = FACE_OUTER_BOUND ( 'NONE', #2214, .T. ) ;
#96488 = CARTESIAN_POINT ( 'NONE',  ( 40.77380256327629837, 468.8478597483947965, 21.13608272249925690 ) ) ;
#96489 = CARTESIAN_POINT ( 'NONE',  ( 12.00013170160833909, -5.000000000000000000, -86.59063654373593977 ) ) ;
#96490 = DIRECTION ( 'NONE',  ( -1.000000000000000000, -1.224606353822377258E-16, -0.000000000000000000 ) ) ;
#96491 = CARTESIAN_POINT ( 'NONE',  ( 40.59999999999999432, 3.309500000000003439, 0.000000000000000000 ) ) ;
#96492 = CARTESIAN_POINT ( 'NONE',  ( -90.58776433791602756, -37.99999999999997158, 81.87422108073580773 ) ) ;
#96493 = AXIS2_PLACEMENT_3D ( 'NONE', #44583, #68865, #26308 ) ;
#96494 = VERTEX_POINT ( 'NONE', #17825 ) ;
#96495 = DIRECTION ( 'NONE',  ( -0.000000000000000000, 0.000000000000000000, 1.000000000000000000 ) ) ;
#96496 = FILL_AREA_STYLE_COLOUR ( '', #9077 ) ;
#96497 = ADVANCED_FACE ( 'NONE', ( #50675 ), #7182, .F. ) ;
#96498 = CARTESIAN_POINT ( 'NONE',  ( 4.521127550501229386, -64.32389759472336266, 3.944701057164355706 ) ) ;
#96499 =( BOUNDED_SURFACE ( )  B_SPLINE_SURFACE ( 3, 2, ( 
 ( #82031, #48602, #98226 ),
 ( #24381, #38434, #90142 ),
 ( #89618, #16244, #96119 ),
 ( #14110, #96648, #6024 ),
 ( #38948, #71825, #22782 ),
 ( #80442, #6550, #105265 ),
 ( #99270, #83108, #24898 ),
 ( #25993, #58854, #25449 ),
 ( #57751, #26, #26516 ),
 ( #9205, #2175, #91228 ) ),
 .UNSPECIFIED., .F., .F., .F. ) 
 B_SPLINE_SURFACE_WITH_KNOTS ( ( 4, 2, 2, 2, 4 ),
 ( 3, 3 ),
 ( 0.009739192996185006695, 0.01968048317401947800, 0.02465112826293671539, 0.02713645080739533408, 0.02962177335185395277 ),
 ( 0.000000000000000000, 1.000000000000000000 ),
 .UNSPECIFIED. ) 
 GEOMETRIC_REPRESENTATION_ITEM ( )  RATIONAL_B_SPLINE_SURFACE ( (
 ( 1.000000000000000000, 0.7071067811865475727, 1.000000000000000000),
 ( 1.000000000000000000, 0.7071067811865475727, 1.000000000000000000),
 ( 1.000000000000000000, 0.7071032136392382261, 1.000000000000000000),
 ( 1.000000000000000000, 0.7071081508940738614, 1.000000000000000000),
 ( 1.000000000000000000, 0.7071048030622038016, 1.000000000000000000),
 ( 1.000000000000000000, 0.7071073475187125146, 1.000000000000000000),
 ( 1.000000000000000000, 0.7070920501327951913, 1.000000000000000000),
 ( 1.000000000000000000, 0.7070828652041093454, 1.000000000000000000),
 ( 1.000000000000000000, 0.7071010096815192325, 1.000000000000000000),
 ( 1.000000000000000000, 0.7071067811865493491, 1.000000000000000000) ) ) 
 REPRESENTATION_ITEM ( '' )  SURFACE ( )  );
#96500 = AXIS2_PLACEMENT_3D ( 'NONE', #18582, #2357, #67646 ) ;
#96501 = ADVANCED_FACE ( 'NONE', ( #96748 ), #71460, .T. ) ;
#96503 = CARTESIAN_POINT ( 'NONE',  ( -58.42930312626833711, -21.77003758643937203, -23.50835556100766510 ) ) ;
#96502 = CARTESIAN_POINT ( 'NONE',  ( 0.000000000000000000, -18.92596047533412573, -20.36976895023282097 ) ) ;
#96504 = ORIENTED_EDGE ( 'NONE', *, *, #15815, .F. ) ;
#96505 = MECHANICAL_DESIGN_GEOMETRIC_PRESENTATION_REPRESENTATION (  '', ( #31100 ), #44859 ) ;
#96506 = DIRECTION ( 'NONE',  ( -0.000000000000000000, -0.000000000000000000, -1.000000000000000000 ) ) ;
#96507 = EDGE_LOOP ( 'NONE', ( #97327, #69593, #35568, #102276 ) ) ;
#96508 = ADVANCED_FACE ( 'NONE', ( #13950, #96487, #104560, #22630 ), #64136, .F. ) ;
#96509 = CARTESIAN_POINT ( 'NONE',  ( 5.975663821520835306, 7.000939006314205848, 0.8740179403730332641 ) ) ;
#96510 = VECTOR ( 'NONE', #36275, 1000.000000000000114 ) ;
#96511 = CARTESIAN_POINT ( 'NONE',  ( 37.38561277374697056, -5.000000000000000000, 0.000000000000000000 ) ) ;
#96512 = CARTESIAN_POINT ( 'NONE',  ( -92.62061861149213371, -60.00000000000000711, -10.08911953426519403 ) ) ;
#96513 = EDGE_LOOP ( 'NONE', ( #35530, #27877, #33778 ) ) ;
#96514 = CARTESIAN_POINT ( 'NONE',  ( 8.000000000000000000, -27.59375000409677270, -3.313708498984761164 ) ) ;
#96515 = CARTESIAN_POINT ( 'NONE',  ( -9.907647895771706459, 15.45478884909084272, 1.400734872026643041 ) ) ;
#96516 = CARTESIAN_POINT ( 'NONE',  ( 99.29740484581111559, -45.26881857393725994, 193.1476703519705893 ) ) ;
#96518 = LINE ( 'NONE', #55485, #47781 ) ;
#96517 = LINE ( 'NONE', #80837, #69833 ) ;
#96519 = AXIS2_PLACEMENT_3D ( 'NONE', #75287, #8431, #15456 ) ;
#96520 = CARTESIAN_POINT ( 'NONE',  ( -83.37668499989145232, -32.53985942674935927, 162.2598532935533626 ) ) ;
#96521 = ORIENTED_EDGE ( 'NONE', *, *, #86571, .F. ) ;
#96522 = ORIENTED_EDGE ( 'NONE', *, *, #14632, .T. ) ;
#96523 = EDGE_LOOP ( 'NONE', ( #75520, #15573, #47049, #16780 ) ) ;
#96524 = DIRECTION ( 'NONE',  ( 0.000000000000000000, 0.000000000000000000, 1.000000000000000000 ) ) ;
#96525 = FILL_AREA_STYLE_COLOUR ( '', #23272 ) ;
#96526 = DIRECTION ( 'NONE',  ( -1.000000000000000000, -0.000000000000000000, -0.000000000000000000 ) ) ;
#96527 = EDGE_LOOP ( 'NONE', ( #50072, #48899, #23367, #85422 ) ) ;
#96528 = SURFACE_STYLE_USAGE ( .BOTH. , #62570 ) ;
#96529 = CARTESIAN_POINT ( 'NONE',  ( -82.98668029349501296, -57.53378708018315280, 201.1759417985833238 ) ) ;
#96530 = CARTESIAN_POINT ( 'NONE',  ( 6.162888688655344005, 3.752776749732565253, 6.499999999999997335 ) ) ;
#96531 = CARTESIAN_POINT ( 'NONE',  ( -55.59873597034283677, 48.00000000000001421, -34.06437516161200563 ) ) ;
#96532 = CARTESIAN_POINT ( 'NONE',  ( -1.100033992246165715, 25.39386148385951358, 40.11500734754208963 ) ) ;
#96533 = CARTESIAN_POINT ( 'NONE',  ( 0.3379642130336351080, 27.30892935218310313, -40.71492746916538863 ) ) ;
#96534 = CIRCLE ( 'NONE', #75894, 4.000000000000001776 ) ;
#96535 = CARTESIAN_POINT ( 'NONE',  ( 94.49477393579812201, -60.00000000000003553, -13.88944369105108301 ) ) ;
#96536 = CARTESIAN_POINT ( 'NONE',  ( -69.92584042677506773, -30.00000000000002842, 127.5397447585766599 ) ) ;
#96537 = ADVANCED_FACE ( 'NONE', ( #97513 ), #85996, .F. ) ;
#96538 = CARTESIAN_POINT ( 'NONE',  ( -54.56892480951270841, -22.15834078237627480, 52.62495691221676708 ) ) ;
#96539 = CONICAL_SURFACE ( 'NONE', #10443, 5.000000000000010658, 0.9599310885968697082 ) ;
#96540 = VERTEX_POINT ( 'NONE', #87338 ) ;
#96541 = ORIENTED_EDGE ( 'NONE', *, *, #44063, .F. ) ;
#96542 = CARTESIAN_POINT ( 'NONE',  ( -102.9241234416141282, -60.17493127080694393, 192.9570147602996144 ) ) ;
#96543 = LINE ( 'NONE', #78741, #8173 ) ;
#96544 = VERTEX_POINT ( 'NONE', #30169 ) ;
#96545 = CARTESIAN_POINT ( 'NONE',  ( 19.36667751815805971, 49.91424520787322194, 61.11596122090848127 ) ) ;
#96546 = CARTESIAN_POINT ( 'NONE',  ( 110.9944082960603140, -38.35619069247599100, 173.2626205915072717 ) ) ;
#96547 = CARTESIAN_POINT ( 'NONE',  ( 31.84999999999999787, 1.533819458162526451E-15, 0.000000000000000000 ) ) ;
#96548 = CARTESIAN_POINT ( 'NONE',  ( -5.082755093536326818, -11.09375000204838457, 5.082755093536325042 ) ) ;
#96549 = CARTESIAN_POINT ( 'NONE',  ( -6.379201817708943345, 294.7476909954166331, 1.915027666297735021 ) ) ;
#96550 = CARTESIAN_POINT ( 'NONE',  ( 98.31310517497099966, 1.030564683017419500E-14, 0.000000000000000000 ) ) ;
#96551 = CARTESIAN_POINT ( 'NONE',  ( 54.58541135956112100, -30.00000000000001066, 54.90165979975594013 ) ) ;
#96552 = DIRECTION ( 'NONE',  ( 0.000000000000000000, -1.000000000000000000, 0.000000000000000000 ) ) ;
#96553 = CARTESIAN_POINT ( 'NONE',  ( -3.355892750373183020, -49.00480196350172690, 104.3125661743345916 ) ) ;
#96554 = EDGE_CURVE ( 'NONE', #69179, #22401, #13415, .T. ) ;
#96555 = CARTESIAN_POINT ( 'NONE',  ( -0.5680898101815228252, 34.21849481828488848, 29.61659561779407568 ) ) ;
#96556 = DIRECTION ( 'NONE',  ( 0.000000000000000000, -1.000000000000000000, 0.000000000000000000 ) ) ;
#96557 = UNCERTAINTY_MEASURE_WITH_UNIT (LENGTH_MEASURE( 1.000000000000000082E-05 ), #29563, 'distance_accuracy_value', 'NONE');
#96558 = CIRCLE ( 'NONE', #74128, 4.000000000000000888 ) ;
#96559 = EDGE_LOOP ( 'NONE', ( #30199, #18182, #82883, #21995, #46797, #96439, #90006 ) ) ;
#96560 = ORIENTED_EDGE ( 'NONE', *, *, #3541, .T. ) ;
#96561 = CARTESIAN_POINT ( 'NONE',  ( 48.92534730531904330, -18.75215370966537520, 42.51723731469244427 ) ) ;
#96562 = FACE_OUTER_BOUND ( 'NONE', #74976, .T. ) ;
#96563 = CARTESIAN_POINT ( 'NONE',  ( -6.239948093757999636, 15.44474749025929228, -3.176436098724914281 ) ) ;
#96564 = CARTESIAN_POINT ( 'NONE',  ( -104.4412629575702738, -38.40429514389773402, 198.0193396095312437 ) ) ;
#96565 = ORIENTED_EDGE ( 'NONE', *, *, #26899, .F. ) ;
#96566 = CARTESIAN_POINT ( 'NONE',  ( 88.37099315902020180, -38.37563564094526214, -19.06208899794795997 ) ) ;
#96567 = CARTESIAN_POINT ( 'NONE',  ( 11.68626183382240136, 18.93463063567243410, -8.061502991394757345 ) ) ;
#96568 = CARTESIAN_POINT ( 'NONE',  ( -19.45839315690574622, 49.98279635927520559, 60.54808333947917021 ) ) ;
#96569 = CARTESIAN_POINT ( 'NONE',  ( 0.000000000000000000, 48.00000000000000000, 0.000000000000000000 ) ) ;
#96570 = CARTESIAN_POINT ( 'NONE',  ( 94.36110561261105545, -45.28273083012499001, 96.73308552606165733 ) ) ;
#96571 = CARTESIAN_POINT ( 'NONE',  ( -31.23453009850055651, 439.6107769536124579, 23.21210983230010783 ) ) ;
#96572 = SURFACE_SIDE_STYLE ('',( #8603 ) ) ;
#96573 = CARTESIAN_POINT ( 'NONE',  ( -31.03678703374875880, 438.6650838204938054, 21.86890379898545334 ) ) ;
#96574 = CARTESIAN_POINT ( 'NONE',  ( 10.50000000000000000, -5.000000000000000000, -11.21398294031086706 ) ) ;
#96575 = CARTESIAN_POINT ( 'NONE',  ( 99.43937970958685924, -59.99999999999999289, 202.0376968176740888 ) ) ;
#96576 = EDGE_CURVE ( 'NONE', #89019, #103730, #81992, .T. ) ;
#96577 = CIRCLE ( 'NONE', #10392, 3.309500000000001663 ) ;
#96578 = CARTESIAN_POINT ( 'NONE',  ( -15.51141066637804400, 34.77717015103064568, 23.41592087525514643 ) ) ;
#96579 = ORIENTED_EDGE ( 'NONE', *, *, #31336, .T. ) ;
#96580 = CARTESIAN_POINT ( 'NONE',  ( 56.69983827852902891, -53.38006274212794722, 70.12899238981250960 ) ) ;
#96581 = EDGE_CURVE ( 'NONE', #74647, #67680, #92324, .T. ) ;
#96582 = CARTESIAN_POINT ( 'NONE',  ( -29.09465867093638636, 306.7984205571843290, -9.112160268181819234 ) ) ;
#96583 = CARTESIAN_POINT ( 'NONE',  ( 7.999885325681426629, 33.99977065129937159, 0.2682325777720087623 ) ) ;
#96584 = CARTESIAN_POINT ( 'NONE',  ( -7.999885325681428405, 26.00022934870063551, 0.2682325777720080962 ) ) ;
#96585 = ORIENTED_EDGE ( 'NONE', *, *, #63092, .F. ) ;
#96587 = DIRECTION ( 'NONE',  ( 0.000000000000000000, 0.000000000000000000, 1.000000000000000000 ) ) ;
#96586 = CARTESIAN_POINT ( 'NONE',  ( -106.7662800213460628, -38.36637556396474480, 195.2415563008339348 ) ) ;
#96588 = CARTESIAN_POINT ( 'NONE',  ( 2.093983074874241623, -3.000000000000000444, 7.791781413346523522 ) ) ;
#96589 = CARTESIAN_POINT ( 'NONE',  ( 29.78761703785879433, 327.5675123215826261, 14.51873336366982059 ) ) ;
#96590 = CARTESIAN_POINT ( 'NONE',  ( 8.000000000000000000, -33.49999999999999289, 0.000000000000000000 ) ) ;
#96591 = CARTESIAN_POINT ( 'NONE',  ( 9.999999999999996447, -5.000000000000002665, -83.69100306251233690 ) ) ;
#96592 = EDGE_CURVE ( 'NONE', #77164, #100664, #38485, .T. ) ;
#96593 = CIRCLE ( 'NONE', #41442, 4.000000000000007105 ) ;
#96594 = EDGE_CURVE ( 'NONE', #75282, #32993, #98589, .T. ) ;
#96595 = DIRECTION ( 'NONE',  ( 0.000000000000000000, -1.000000000000000000, 0.000000000000000000 ) ) ;
#96596 = ORIENTED_EDGE ( 'NONE', *, *, #79096, .F. ) ;
#96597 = CARTESIAN_POINT ( 'NONE',  ( 84.83629015364854808, -28.93020097267356050, 170.9427086118279817 ) ) ;
#96598 = CIRCLE ( 'NONE', #91208, 3.309500000000007880 ) ;
#96599 = CARTESIAN_POINT ( 'NONE',  ( 7.953367043448346330, 98.37964251781980352, -0.000000000000000000 ) ) ;
#96600 = CARTESIAN_POINT ( 'NONE',  ( -37.85695620536581885, 439.1124626137719247, 23.53257295012781469 ) ) ;
#96601 = ORIENTED_EDGE ( 'NONE', *, *, #55340, .F. ) ;
#96602 = CARTESIAN_POINT ( 'NONE',  ( 63.81650669486618455, -1.232595164407830946E-29, 4.000000000000007105 ) ) ;
#96603 = EDGE_CURVE ( 'NONE', #98133, #64587, #50555, .T. ) ;
#96604 = CARTESIAN_POINT ( 'NONE',  ( 7.022229286271609361, -4.221542269094411992, -17.11103215588190807 ) ) ;
#96605 = CARTESIAN_POINT ( 'NONE',  ( 26.49069557787568385, 34.70594681385026092, -9.907218389797451508 ) ) ;
#96606 = CARTESIAN_POINT ( 'NONE',  ( 0.000000000000000000, 6.123233995736767268E-16, -5.000000000000000888 ) ) ;
#96607 = VERTEX_POINT ( 'NONE', #9572 ) ;
#96608 = CONICAL_SURFACE ( 'NONE', #50089, 23.23666318551310539, 1.221730476396026388 ) ;
#96609 = CARTESIAN_POINT ( 'NONE',  ( 6.499999999999403144, 1.333904739168199960, -6.094327662196310946 ) ) ;
#96610 = CARTESIAN_POINT ( 'NONE',  ( -4.861072549008415677, -47.07915654916947545, 102.3606070684416665 ) ) ;
#96612 = CARTESIAN_POINT ( 'NONE',  ( -12.98756968922270438, 8.529146807383854778, -8.948902651470408642 ) ) ;
#96611 = CARTESIAN_POINT ( 'NONE',  ( 42.93430011342386621, 435.4574193743733872, 17.27214342660671065 ) ) ;
#96613 = CIRCLE ( 'NONE', #72499, 4.000000000000000888 ) ;
#96614 = CARTESIAN_POINT ( 'NONE',  ( 4.401442555609581635E-16, -21.78125000204838457, -7.188101187500000044 ) ) ;
#96615 = CARTESIAN_POINT ( 'NONE',  ( -28.79546424415106998, 15.38851513919402869, -41.74402054108289661 ) ) ;
#96616 = FILL_AREA_STYLE_COLOUR ( '', #1805 ) ;
#96617 = EDGE_LOOP ( 'NONE', ( #35635, #61914, #4113, #12464, #904, #71835 ) ) ;
#96618 = DIRECTION ( 'NONE',  ( -1.000000000000000000, -0.000000000000000000, -0.000000000000000000 ) ) ;
#96619 = CARTESIAN_POINT ( 'NONE',  ( -8.203969886189964811, 114.5837526205014285, -5.000000000002539302 ) ) ;
#96620 = CARTESIAN_POINT ( 'NONE',  ( -6.256238905642391934, -5.000000000004484413, -71.20382033075676986 ) ) ;
#96621 = ADVANCED_FACE ( 'NONE', ( #26357 ), #86686, .F. ) ;
#96622 = CARTESIAN_POINT ( 'NONE',  ( 20.00000000000000711, 4.000000000000000888, 25.00000000000000000 ) ) ;
#96623 = CIRCLE ( 'NONE', #32898, 8.000000000000000000 ) ;
#96624 = VERTEX_POINT ( 'NONE', #34441 ) ;
#96625 = DIRECTION ( 'NONE',  ( -0.5735764363510497121, 0.8191520442889892450, 1.003171929053521665E-16 ) ) ;
#96626 = FACE_OUTER_BOUND ( 'NONE', #83124, .T. ) ;
#96627 = ORIENTED_EDGE ( 'NONE', *, *, #55340, .T. ) ;
#96628 = ADVANCED_FACE ( 'NONE', ( #57063 ), #60809, .T. ) ;
#96629 = DIRECTION ( 'NONE',  ( 0.000000000000000000, -1.000000000000000000, 0.000000000000000000 ) ) ;
#96630 = SURFACE_SIDE_STYLE ('',( #88540 ) ) ;
#96631 = FILL_AREA_STYLE ('',( #72348 ) ) ;
#96632 = UNCERTAINTY_MEASURE_WITH_UNIT (LENGTH_MEASURE( 1.000000000000000082E-05 ), #57067, 'distance_accuracy_value', 'NONE');
#96633 = CARTESIAN_POINT ( 'NONE',  ( -108.0975085614644513, -60.00000000000000000, 129.7140120509529595 ) ) ;
#96634 = DIRECTION ( 'NONE',  ( 1.000000000000000000, 0.000000000000000000, 0.000000000000000000 ) ) ;
#96635 = CARTESIAN_POINT ( 'NONE',  ( 20.52350613252515643, 304.8999024697870937, 9.947223320822450532 ) ) ;
#96636 = CARTESIAN_POINT ( 'NONE',  ( 6.400292240292954737, 53.43402837650388904, -7.879178544242287252 ) ) ;
#96637 = CARTESIAN_POINT ( 'NONE',  ( 17.95946743641316345, 34.46552302443144100, -22.69735960963333454 ) ) ;
#96638 = CARTESIAN_POINT ( 'NONE',  ( -86.25780443371026251, -18.23629696712657022, 169.8396338056661534 ) ) ;
#96639 = ORIENTED_EDGE ( 'NONE', *, *, #31787, .T. ) ;
#96640 = CARTESIAN_POINT ( 'NONE',  ( 41.82792046605465686, 6.123233995736770227E-16, -5.000000000000002665 ) ) ;
#96641 = CIRCLE ( 'NONE', #72538, 2.000000000000000000 ) ;
#96642 = CONICAL_SURFACE ( 'NONE', #34698, 3.309500000000007880, 0.9599310885968770357 ) ;
#96643 = AXIS2_PLACEMENT_3D ( 'NONE', #90745, #8751, #83177 ) ;
#96644 = VERTEX_POINT ( 'NONE', #57584 ) ;
#96645 = DIRECTION ( 'NONE',  ( -1.000000000000000000, -1.224606353822377258E-16, -0.000000000000000000 ) ) ;
#96646 = CARTESIAN_POINT ( 'NONE',  ( -83.66830488457027570, -45.26507799069083404, 12.12265221865681042 ) ) ;
#96647 = AXIS2_PLACEMENT_3D ( 'NONE', #1491, #40907, #930 ) ;
#96648 = CARTESIAN_POINT ( 'NONE',  ( -11.62661342925168384, 304.6006127265920327, 9.883607322378615834 ) ) ;
#96649 = CARTESIAN_POINT ( 'NONE',  ( 88.48689482502902592, 5.000000000000023093, 6.123233995736781074E-16 ) ) ;
#96650 = CARTESIAN_POINT ( 'NONE',  ( 8.588478090849999802, 23.79665183991622257, 6.142597166387020528E-13 ) ) ;
#96651 = LINE ( 'NONE', #32470, #86460 ) ;
#96652 = CARTESIAN_POINT ( 'NONE',  ( 88.35660587733796945, -14.21045842199459486, 197.0604887900697122 ) ) ;
#96653 = AXIS2_PLACEMENT_3D ( 'NONE', #68352, #41403, #99638 ) ;
#96654 = CARTESIAN_POINT ( 'NONE',  ( -91.50803816462422446, -30.00000000000001776, 42.72771024551138908 ) ) ;
#96655 = ADVANCED_FACE ( 'NONE', ( #101271 ), #36041, .T. ) ;
#96656 = CARTESIAN_POINT ( 'NONE',  ( -61.11614492808612908, -53.39328282429821826, 82.02358402482038002 ) ) ;
#96657 = VERTEX_POINT ( 'NONE', #92631 ) ;
#96658 = CARTESIAN_POINT ( 'NONE',  ( -2.958297520906366884, 39.42457334331769658, 65.00031284538987109 ) ) ;
#96659 = CARTESIAN_POINT ( 'NONE',  ( 96.79493678139994017, -59.99999999999132427, 204.9247966883611980 ) ) ;
#96660 = ORIENTED_EDGE ( 'NONE', *, *, #35280, .F. ) ;
#96661 = CARTESIAN_POINT ( 'NONE',  ( 3.081314264678424397, -56.87780286871037561, 33.36400653726988708 ) ) ;
#96662 = CARTESIAN_POINT ( 'NONE',  ( -5.082755093536325042, -20.46875000204838813, -5.082755093536325930 ) ) ;
#96663 = FILL_AREA_STYLE ('',( #63776 ) ) ;
#96664 = VERTEX_POINT ( 'NONE', #100719 ) ;
#96665 = CARTESIAN_POINT ( 'NONE',  ( -10.91152070480441871, 45.93327767897820735, 13.06343554040036459 ) ) ;
#96666 = ORIENTED_EDGE ( 'NONE', *, *, #54688, .T. ) ;
#96667 = CARTESIAN_POINT ( 'NONE',  ( 11.53061943269010392, 45.53913102596383311, -13.95708208482086121 ) ) ;
#96668 = DIRECTION ( 'NONE',  ( 0.000000000000000000, -1.000000000000000000, 0.000000000000000000 ) ) ;
#96669 = CARTESIAN_POINT ( 'NONE',  ( -93.08565485029603792, -60.00000000000000000, 33.23478458921270828 ) ) ;
#96670 = CARTESIAN_POINT ( 'NONE',  ( 36.69193770976632152, 378.6360570424787966, 4.935504223416926628 ) ) ;
#96671 = CARTESIAN_POINT ( 'NONE',  ( 7.188101187499999156, -25.62500000204838813, 2.977408999572654924 ) ) ;
#96672 = CARTESIAN_POINT ( 'NONE',  ( 32.82325442954073225, 485.9854176254823983, 5.594246714727905356 ) ) ;
#96673 = CARTESIAN_POINT ( 'NONE',  ( -3.175336665761835597, 20.29878287605892595, -6.240496478724519847 ) ) ;
#96674 = LINE ( 'NONE', #95097, #71904 ) ;
#96675 = CARTESIAN_POINT ( 'NONE',  ( -9.739726766104285005, 48.00000000000000000, -82.38252115500968387 ) ) ;
#96676 = EDGE_CURVE ( 'NONE', #90844, #86309, #105589, .T. ) ;
#96677 = CARTESIAN_POINT ( 'NONE',  ( -48.02835407290516656, -1.200000000000000030E-05, 15.60535821593516737 ) ) ;
#96678 = CARTESIAN_POINT ( 'NONE',  ( 20.59177611987304957, 302.8577050849145280, -9.998745446473192189 ) ) ;
#96679 = CARTESIAN_POINT ( 'NONE',  ( -34.85857064921750492, -22.18165287194634416, 31.84054876490759156 ) ) ;
#96680 = STYLED_ITEM ( 'NONE', ( #36337 ), #105888 ) ;
#96681 = EDGE_LOOP ( 'NONE', ( #104118, #66469, #67919 ) ) ;
#96682 = DIRECTION ( 'NONE',  ( 0.000000000000000000, -1.000000000000000000, 0.000000000000000000 ) ) ;
#96683 = CARTESIAN_POINT ( 'NONE',  ( 40.48137601666525853, -22.23684450456674710, 35.13079649809134963 ) ) ;
#96684 = AXIS2_PLACEMENT_3D ( 'NONE', #103175, #87525, #95093 ) ;
#96685 = CARTESIAN_POINT ( 'NONE',  ( -14.86825985027621755, -1.734723475976807094E-15, 8.569529079659670145 ) ) ;
#96686 = ORIENTED_EDGE ( 'NONE', *, *, #94664, .T. ) ;
#96687 = CARTESIAN_POINT ( 'NONE',  ( 34.49820706013684912, 464.8461132933183535, 18.22442427699395395 ) ) ;
#96688 = AXIS2_PLACEMENT_3D ( 'NONE', #41786, #8353, #83306 ) ;
#96689 = CARTESIAN_POINT ( 'NONE',  ( -75.45914410051923937, -38.35135203049976838, 173.8682629998443758 ) ) ;
#96690 = B_SPLINE_CURVE_WITH_KNOTS ( 'NONE', 3,
 ( #90359, #8372, #1320, #43414, #16470, #41801, #82259, #33209 ),
 .UNSPECIFIED., .F., .F.,
 ( 4, 2, 2, 4 ),
 ( 0.003797433802554435033, 0.004743183970586232687, 0.005688934138618029906, 0.007580434474681625213 ),
 .UNSPECIFIED. ) ;
#96691 = ORIENTED_EDGE ( 'NONE', *, *, #14814, .T. ) ;
#96693 = CARTESIAN_POINT ( 'NONE',  ( -22.42417502586373246, 305.3961751430792333, 10.05444931189341773 ) ) ;
#96692 = DIRECTION ( 'NONE',  ( 0.000000000000000000, -1.000000000000000000, 0.000000000000000000 ) ) ;
#96694 = DIRECTION ( 'NONE',  ( 0.000000000000000000, 0.000000000000000000, 1.000000000000000000 ) ) ;
#96695 = DIRECTION ( 'NONE',  ( 0.000000000000000000, -1.000000000000000000, 0.000000000000000000 ) ) ;
#96696 = DIRECTION ( 'NONE',  ( -0.000000000000000000, -0.000000000000000000, -1.000000000000000000 ) ) ;
#96697 = PRESENTATION_STYLE_ASSIGNMENT (( #71875 ) ) ;
#96698 = CARTESIAN_POINT ( 'NONE',  ( -48.91605700228340936, 13.22299455560985315, -16.49079035033054197 ) ) ;
#96699 = CARTESIAN_POINT ( 'NONE',  ( 0.000000000000000000, -6.928203230275503444, 4.000000000000010658 ) ) ;
#96700 = CARTESIAN_POINT ( 'NONE',  ( 95.10565317760159587, -60.00000000000000711, 49.79938089396723200 ) ) ;
#96701 = FACE_OUTER_BOUND ( 'NONE', #30699, .T. ) ;
#96702 = CARTESIAN_POINT ( 'NONE',  ( 0.000000000000000000, 1.502314598737161398E-15, 6.499999999999999112 ) ) ;
#96703 = CARTESIAN_POINT ( 'NONE',  ( 7.758748231342716295, -5.000000000000001776, -73.00623724565090811 ) ) ;
#96704 = ORIENTED_EDGE ( 'NONE', *, *, #44073, .T. ) ;
#96705 = EDGE_CURVE ( 'NONE', #45904, #102350, #47234, .T. ) ;
#96706 = MECHANICAL_DESIGN_GEOMETRIC_PRESENTATION_REPRESENTATION (  '', ( #19224 ), #57029 ) ;
#96707 = B_SPLINE_CURVE_WITH_KNOTS ( 'NONE', 3,
 ( #47804, #46241, #87768, #54292, #105527, #79656, #104460, #71037 ),
 .UNSPECIFIED., .F., .F.,
 ( 4, 2, 2, 4 ),
 ( 8.156951321262543387E-15, 0.003573501338921054610, 0.005360252008377505532, 0.007147002677833957755 ),
 .UNSPECIFIED. ) ;
#96708 = CARTESIAN_POINT ( 'NONE',  ( -88.42496338177498671, -30.00000000000168399, -16.19662829210094301 ) ) ;
#96709 = ORIENTED_EDGE ( 'NONE', *, *, #49927, .F. ) ;
#96710 = CARTESIAN_POINT ( 'NONE',  ( -3.386172510860506968, -49.13793332017446147, 104.0372841442787006 ) ) ;
#96711 = CARTESIAN_POINT ( 'NONE',  ( -15.31219705631699313, 3.104419271460729490, 3.118400172730193542 ) ) ;
#96712 = CARTESIAN_POINT ( 'NONE',  ( 8.224453817209493423, 36.45934599358590589, 0.000000000000000000 ) ) ;
#96713 = CARTESIAN_POINT ( 'NONE',  ( 32.19491124036529328, 391.9745737642126642, 25.40000947286657507 ) ) ;
#96714 = CARTESIAN_POINT ( 'NONE',  ( -1.320432766682874540E-15, -22.90625000204838457, 7.188101187500000044 ) ) ;
#96715 = EDGE_CURVE ( 'NONE', #100006, #77685, #102320, .T. ) ;
#96716 = FACE_OUTER_BOUND ( 'NONE', #43528, .T. ) ;
#96717 = DIRECTION ( 'NONE',  ( 0.000000000000000000, 1.000000000000000000, 0.000000000000000000 ) ) ;
#96719 = ADVANCED_FACE ( 'NONE', ( #35496 ), #68372, .F. ) ;
#96718 = CARTESIAN_POINT ( 'NONE',  ( 6.757705285491359071, 41.35007050631321590, -70.67351639401239538 ) ) ;
#96720 = ORIENTED_EDGE ( 'NONE', *, *, #35342, .F. ) ;
#96722 = ORIENTED_EDGE ( 'NONE', *, *, #43163, .F. ) ;
#96721 = FACE_OUTER_BOUND ( 'NONE', #95401, .T. ) ;
#96723 = CARTESIAN_POINT ( 'NONE',  ( 80.44587350599928754, -49.90936352864175518, 162.4342867686268903 ) ) ;
#96724 = PRESENTATION_LAYER_ASSIGNMENT (  '', '', ( #57119 ) ) ;
#96725 = CARTESIAN_POINT ( 'NONE',  ( 15.36579003345834771, 3.191525062043596872, -3.226546488143007707 ) ) ;
#96726 = ORIENTED_EDGE ( 'NONE', *, *, #99922, .F. ) ;
#96728 = EDGE_CURVE ( 'NONE', #18315, #44795, #90110, .T. ) ;
#96727 = AXIS2_PLACEMENT_3D ( 'NONE', #95929, #87840, #106112 ) ;
#96729 = CARTESIAN_POINT ( 'NONE',  ( 9.797174393178825657E-16, 0.000000000000000000, -8.000000000000000000 ) ) ;
#96730 = CARTESIAN_POINT ( 'NONE',  ( -1.167655683674313938, 14.75960163002330994, -50.96284648200735745 ) ) ;
#96731 = CARTESIAN_POINT ( 'NONE',  ( 2.977408999572652260, -11.93750000204838635, 7.188101187500000044 ) ) ;
#96732 = DIRECTION ( 'NONE',  ( 1.150791560227848544E-16, -0.3420201433256727652, 0.9396926207859068736 ) ) ;
#96733 = MECHANICAL_DESIGN_GEOMETRIC_PRESENTATION_REPRESENTATION (  '', ( #21011 ), #51977 ) ;
#96734 = CARTESIAN_POINT ( 'NONE',  ( -23.49283269198559765, -57.67355083020559192, 42.82390242447587525 ) ) ;
#96735 = CARTESIAN_POINT ( 'NONE',  ( 6.683837171061806970, -7.911893696991936231, 5.688671339918660213E-17 ) ) ;
#96736 = ORIENTED_EDGE ( 'NONE', *, *, #12792, .F. ) ;
#96737 = B_SPLINE_CURVE_WITH_KNOTS ( 'NONE', 3,
 ( #75299, #74237, #82871, #9493, #41873, #58606, #841, #34360, #17087, #84473 ),
 .UNSPECIFIED., .F., .F.,
 ( 4, 2, 2, 2, 4 ),
 ( 4.768881061110644471E-15, 0.001938799274764216535, 0.003877598549523663882, 0.005816397824283111445, 0.007755197099042559009 ),
 .UNSPECIFIED. ) ;
#96738 = CYLINDRICAL_SURFACE ( 'NONE', #40697, 8.000000000000000000 ) ;
#96740 = CARTESIAN_POINT ( 'NONE',  ( 3.757222014067413518, 132.6327721420962575, 4.999999999999999112 ) ) ;
#96739 = CIRCLE ( 'NONE', #50215, 3.309500000000001663 ) ;
#96741 = CARTESIAN_POINT ( 'NONE',  ( 86.75754961941542831, -5.000000000000000000, 6.123233995736778115E-16 ) ) ;
#96742 = MECHANICAL_DESIGN_GEOMETRIC_PRESENTATION_REPRESENTATION (  '', ( #69184 ), #93275 ) ;
#96743 = ORIENTED_EDGE ( 'NONE', *, *, #49034, .T. ) ;
#96744 = CARTESIAN_POINT ( 'NONE',  ( -3.313708498984760720, -12.21875000409676737, -8.000000000000000000 ) ) ;
#96745 = CARTESIAN_POINT ( 'NONE',  ( -7.127421841361177179, -13.18528672947971891, 32.02679007952325918 ) ) ;
#96746 = CARTESIAN_POINT ( 'NONE',  ( -41.34887590656642686, 489.6219161921864043, 10.83929645669275565 ) ) ;
#96747 = CYLINDRICAL_SURFACE ( 'NONE', #20759, 1.250000000000001110 ) ;
#96748 = FACE_OUTER_BOUND ( 'NONE', #43183, .T. ) ;
#96749 = SURFACE_STYLE_FILL_AREA ( #95680 ) ;
#96750 = ITEM_DEFINED_TRANSFORMATION ( 'NONE', 'NONE', #92047,  #10728 ) ;
#96751 = CARTESIAN_POINT ( 'NONE',  ( 37.56673239365873940, 27.88554838446218653, 10.95617127780822564 ) ) ;
#96752 = ORIENTED_EDGE ( 'NONE', *, *, #50152, .T. ) ;
#96753 = CARTESIAN_POINT ( 'NONE',  ( 11.39584891955474433, 43.21406130090534958, 14.75674298142433827 ) ) ;
#96754 = DIRECTION ( 'NONE',  ( 0.000000000000000000, -1.000000000000000000, 0.000000000000000000 ) ) ;
#96755 = CARTESIAN_POINT ( 'NONE',  ( 0.9999999999999954481, -50.00000000000000000, 44.97220075561143204 ) ) ;
#96756 = CARTESIAN_POINT ( 'NONE',  ( -57.63211173758740813, -37.00413535841546775, -34.72254536230725819 ) ) ;
#96757 = DIRECTION ( 'NONE',  ( -1.000000000000000000, -1.224606353822377258E-16, -0.000000000000000000 ) ) ;
#96758 = CARTESIAN_POINT ( 'NONE',  ( 7.500000000000007105, 42.00000000000000711, -58.09827136975972195 ) ) ;
#96759 = EDGE_CURVE ( 'NONE', #77575, #32538, #99462, .T. ) ;
#96760 = CIRCLE ( 'NONE', #33032, 7.500000000000000000 ) ;
#96761 = ORIENTED_EDGE ( 'NONE', *, *, #21027, .T. ) ;
#96762 = CARTESIAN_POINT ( 'NONE',  ( 7.500000000000001776, 1.028703311283776783E-15, -8.400000000000000355 ) ) ;
#96763 = CARTESIAN_POINT ( 'NONE',  ( 100.5645707510053626, -57.62842971074093157, 203.7695601258284057 ) ) ;
#96764 = CIRCLE ( 'NONE', #58891, 60.00000000000000000 ) ;
#96765 = CARTESIAN_POINT ( 'NONE',  ( 58.43705451886171431, -47.40890191778955653, -27.93287016854851501 ) ) ;
#96766 = EDGE_CURVE ( 'NONE', #103314, #44580, #22826, .T. ) ;
#96767 = AXIS2_PLACEMENT_3D ( 'NONE', #78449, #29415, #5624 ) ;
#96768 = CARTESIAN_POINT ( 'NONE',  ( 0.000000000000000000, 0.000000000000000000, 0.000000000000000000 ) ) ;
#96769 = CARTESIAN_POINT ( 'NONE',  ( 43.69716417780046669, 40.83906611472173864, 48.48761666258860714 ) ) ;
#96770 = CARTESIAN_POINT ( 'NONE',  ( -73.50277685114647852, -59.99999999999999289, 167.2174948213626351 ) ) ;
#96771 = CARTESIAN_POINT ( 'NONE',  ( -37.04388863813380794, 311.3287000699716032, 13.89786840526617517 ) ) ;
#96772 = DIRECTION ( 'NONE',  ( 0.000000000000000000, 0.000000000000000000, 1.000000000000000000 ) ) ;
#96773 = EDGE_CURVE ( 'NONE', #52464, #85320, #49317, .T. ) ;
#96774 = CARTESIAN_POINT ( 'NONE',  ( -64.91565662645538737, 49.99999999999999289, 6.815324757469617190 ) ) ;
#96775 = CARTESIAN_POINT ( 'NONE',  ( -85.72959342069100330, -35.64893082154279824, 184.4343426154862584 ) ) ;
#96776 = EDGE_LOOP ( 'NONE', ( #24424, #62056, #13124, #2499, #41773 ) ) ;
#96777 = CARTESIAN_POINT ( 'NONE',  ( 34.80740166408775593, 344.0579031421361833, 0.3694569702644521225 ) ) ;
#96778 = VERTEX_POINT ( 'NONE', #25637 ) ;
#96779 = CARTESIAN_POINT ( 'NONE',  ( 12.19670133565572101, -4.599518202331234207, -76.80113241245393851 ) ) ;
#96780 = CARTESIAN_POINT ( 'NONE',  ( -23.36542799780119495, 304.4283958914435857, -9.876218974521238536 ) ) ;
#96781 = CARTESIAN_POINT ( 'NONE',  ( 41.59240229034593028, 487.6847433724397547, 9.907832703287217768 ) ) ;
#96782 = B_SPLINE_CURVE_WITH_KNOTS ( 'NONE', 3,
 ( #78398, #3993, #53072, #69788, #94612, #37454, #35323, #43911, #69271, #3459, #102144, #102682, #59581, #26708, #92447, #93541, #84379, #94058 ),
 .UNSPECIFIED., .F., .F.,
 ( 4, 2, 2, 2, 2, 2, 2, 2, 4 ),
 ( 0.006884628567306551837, 0.007891832553332813263, 0.008899036539359075557, 0.009150837535865643732, 0.009402638532372210173, 0.009906240525385343054, 0.01015804152189190776, 0.01040984251839847420, 0.01091344451141159320 ),
 .UNSPECIFIED. ) ;
#96783 = FACE_OUTER_BOUND ( 'NONE', #33939, .T. ) ;
#96784 = CARTESIAN_POINT ( 'NONE',  ( -43.00000000000000000, 487.9285348210879647, 8.903916466045071587 ) ) ;
#96785 = ORIENTED_EDGE ( 'NONE', *, *, #84078, .F. ) ;
#96786 = CARTESIAN_POINT ( 'NONE',  ( 17.95249423762719232, 50.00000000000002132, 61.95147677239601336 ) ) ;
#96787 = CARTESIAN_POINT ( 'NONE',  ( 12.29374883903973270, 22.31972738609956153, 6.413658937279785199 ) ) ;
#96788 = CARTESIAN_POINT ( 'NONE',  ( 2.723397405354400211E-15, -8.673617379884035472E-16, 22.23822744035697241 ) ) ;
#96789 = FACE_OUTER_BOUND ( 'NONE', #66431, .T. ) ;
#96790 = CARTESIAN_POINT ( 'NONE',  ( 95.02194560458454475, -59.99999999999987210, -3.233414228271875857 ) ) ;
#96791 = CARTESIAN_POINT ( 'NONE',  ( -77.83469039265052913, -56.84582962964739750, 150.7048350401225889 ) ) ;
#96792 = ORIENTED_EDGE ( 'NONE', *, *, #101942, .T. ) ;
#96793 = CARTESIAN_POINT ( 'NONE',  ( 41.69321614992608716, -29.99999999999995737, 49.76314934024226488 ) ) ;
#96794 = CARTESIAN_POINT ( 'NONE',  ( 36.48461538461538822, -4.171999999999999709, 5.616230220889763424E-16 ) ) ;
#96795 = CARTESIAN_POINT ( 'NONE',  ( 72.54833963118097984, -57.66457796962676952, 177.4209049984457636 ) ) ;
#96796 = LINE ( 'NONE', #22928, #61316 ) ;
#96797 = CARTESIAN_POINT ( 'NONE',  ( 39.12236032760809223, 311.3937239336017342, 1.944237020743172284 ) ) ;
#96798 = DIRECTION ( 'NONE',  ( 0.000000000000000000, 0.000000000000000000, -1.000000000000000000 ) ) ;
#96799 = ORIENTED_EDGE ( 'NONE', *, *, #83544, .T. ) ;
#96800 = DIRECTION ( 'NONE',  ( 0.000000000000000000, -1.000000000000000000, 0.000000000000000000 ) ) ;
#96801 = CIRCLE ( 'NONE', #5480, 2.000000000000000888 ) ;
#96802 = CARTESIAN_POINT ( 'NONE',  ( 51.01037695545453232, 450.0000000000002274, 13.20242257375370976 ) ) ;
#96804 = CARTESIAN_POINT ( 'NONE',  ( -101.6938598978349262, -37.82055728416436580, 153.9927469340554183 ) ) ;
#96803 = CARTESIAN_POINT ( 'NONE',  ( -15.76193534935225671, 36.72733462479576616, 23.83658602074646637 ) ) ;
#96805 = CARTESIAN_POINT ( 'NONE',  ( -2.977408999572654480, -21.12500000204838813, 7.188101187499999156 ) ) ;
#96806 = CARTESIAN_POINT ( 'NONE',  ( 43.39367449914676200, 484.9145775485792456, -0.08602995335240110064 ) ) ;
#96807 = AXIS2_PLACEMENT_3D ( 'NONE', #52674, #18218, #51069 ) ;
#96808 = CARTESIAN_POINT ( 'NONE',  ( 9.948561005166130400, 81.13009726251802078, -1.045755304005129505 ) ) ;
#96809 = CARTESIAN_POINT ( 'NONE',  ( 1.009401082359720370, 34.89502620709782121, 27.74504690791027528 ) ) ;
#96810 = DIRECTION ( 'NONE',  ( 0.000000000000000000, 1.000000000000000000, 0.000000000000000000 ) ) ;
#96811 = CARTESIAN_POINT ( 'NONE',  ( -5.656854249492379694, -13.62500000409676915, -5.656854249492380582 ) ) ;
#96812 = ORIENTED_EDGE ( 'NONE', *, *, #50019, .F. ) ;
#96813 = DIRECTION ( 'NONE',  ( -1.000000000000000000, -0.000000000000000000, 0.000000000000000000 ) ) ;
#96814 = MECHANICAL_DESIGN_GEOMETRIC_PRESENTATION_REPRESENTATION (  '', ( #103650 ), #105429 ) ;
#96816 = CARTESIAN_POINT ( 'NONE',  ( 26.23477066092984700, -42.95572057826144885, 32.63390350353837022 ) ) ;
#96815 = LINE ( 'NONE', #105430, #14757 ) ;
#96817 = CARTESIAN_POINT ( 'NONE',  ( -5.208114383187426810, 52.09973805833581650, -6.031152949374310346 ) ) ;
#96818 = ORIENTED_EDGE ( 'NONE', *, *, #53495, .T. ) ;
#96819 = VECTOR ( 'NONE', #29021, 1000.000000000000000 ) ;
#96820 = UNCERTAINTY_MEASURE_WITH_UNIT (LENGTH_MEASURE( 1.000000000000000082E-05 ), #8415, 'distance_accuracy_value', 'NONE');
#96821 = ORIENTED_EDGE ( 'NONE', *, *, #35676, .T. ) ;
#96823 = CARTESIAN_POINT ( 'NONE',  ( -1.220780421567363883, 43.50148743144289654, -17.81286546842412832 ) ) ;
#96822 = CYLINDRICAL_SURFACE ( 'NONE', #103674, 5.000000000000000888 ) ;
#96824 = FACE_OUTER_BOUND ( 'NONE', #96400, .T. ) ;
#96825 = SURFACE_STYLE_USAGE ( .BOTH. , #95237 ) ;
#96826 = CARTESIAN_POINT ( 'NONE',  ( 16.33361799548379523, 1.482358050883964840E-15, 0.000000000000000000 ) ) ;
#96827 = CARTESIAN_POINT ( 'NONE',  ( 14.78075358320714905, 0.1660929298666962151, 15.00000000000000178 ) ) ;
#96828 = CARTESIAN_POINT ( 'NONE',  ( -7.500000000000000000, 1.854554393013820190, -0.1880126015361690550 ) ) ;
#96829 = ORIENTED_EDGE ( 'NONE', *, *, #41539, .F. ) ;
#96830 = CARTESIAN_POINT ( 'NONE',  ( 15.26350624587492000, -59.99999999999998579, -42.14653362384034807 ) ) ;
#96831 = CARTESIAN_POINT ( 'NONE',  ( 54.95194601437927417, -29.99999999999999289, 55.56075107115263734 ) ) ;
#96832 = CARTESIAN_POINT ( 'NONE',  ( -0.000000000000000000, 7.666536031838887766, -59.53359981990485750 ) ) ;
#96833 = CARTESIAN_POINT ( 'NONE',  ( 8.099999999999999645, 7.505553499465140277, 3.755786496842903002E-16 ) ) ;
#96834 =( BOUNDED_CURVE ( )  B_SPLINE_CURVE ( 2, ( #32317, #24232, #89994, #81882, #8003, #40913, #73804, #84970, #43978 ),
 .UNSPECIFIED., .F., .F. ) 
 B_SPLINE_CURVE_WITH_KNOTS ( ( 3, 2, 2, 2, 3 ),
 ( 0.1960366238535917460, 0.1985294117647058709, 0.2058823529411764885, 0.2132352941176470784, 0.2205882352941176960 ),
 .UNSPECIFIED. ) 
 CURVE ( )  GEOMETRIC_REPRESENTATION_ITEM ( )  RATIONAL_B_SPLINE_CURVE ( ( 0.9658850645339884800, 0.9741937033643860433, 1.000000000000000000, 0.9238795325112867385, 1.000000000000000000, 0.9238795325112867385, 1.000000000000000000, 0.9238795325112861834, 1.000000000000000666 ) ) 
 REPRESENTATION_ITEM ( '' )  );
#96835 = CARTESIAN_POINT ( 'NONE',  ( -48.02835407290534420, 16.78162100668604495, -14.35535821593460248 ) ) ;
#96836 = ORIENTED_EDGE ( 'NONE', *, *, #48836, .T. ) ;
#96837 = EDGE_CURVE ( 'NONE', #55179, #75948, #8336, .T. ) ;
#96838 = VERTEX_POINT ( 'NONE', #82224 ) ;
#96839 = ORIENTED_EDGE ( 'NONE', *, *, #86640, .F. ) ;
#96840 = DIRECTION ( 'NONE',  ( -1.000000000000000000, -0.000000000000000000, -0.000000000000000000 ) ) ;
#96841 = CARTESIAN_POINT ( 'NONE',  ( 14.91338090413177397, 41.98696021714862781, -86.62221405687444076 ) ) ;
#96842 = CARTESIAN_POINT ( 'NONE',  ( -41.18714086166914967, 436.5287100296065432, 21.33940902914881477 ) ) ;
#96843 = CARTESIAN_POINT ( 'NONE',  ( 33.09674748210675688, 373.8214981666397421, 24.18330061219716853 ) ) ;
#96844 = CIRCLE ( 'NONE', #17619, 3.309500000000001663 ) ;
#96845 = CARTESIAN_POINT ( 'NONE',  ( -45.18761087313401958, 356.2647831403982650, 4.028119660265046420 ) ) ;
#96846 = CARTESIAN_POINT ( 'NONE',  ( -3.558726380635282016, -68.96874620124219746, 13.45354069684906229 ) ) ;
#96847 = CARTESIAN_POINT ( 'NONE',  ( -45.99999999998584599, 486.3339417046910853, 3.364639354305617225 ) ) ;
#96848 = CARTESIAN_POINT ( 'NONE',  ( 2.449293598294706907E-16, 0.000000000000000000, 2.000000000000000444 ) ) ;
#96849 = ORIENTED_EDGE ( 'NONE', *, *, #511, .T. ) ;
#96851 = EDGE_CURVE ( 'NONE', #50026, #95748, #40705, .T. ) ;
#96850 = CARTESIAN_POINT ( 'NONE',  ( 6.980486755139912911E-15, 47.00000000000000000, -56.99999999999999289 ) ) ;
#96852 = AXIS2_PLACEMENT_3D ( 'NONE', #28761, #52992, #62170 ) ;
#96853 = EDGE_LOOP ( 'NONE', ( #55411, #61512, #98654, #56318, #84417, #35962 ) ) ;
#96854 = DIRECTION ( 'NONE',  ( -0.5735764363510497121, 0.8191520442889892450, 1.003171929053521665E-16 ) ) ;
#96855 =( NAMED_UNIT ( * ) SI_UNIT ( $, .STERADIAN. ) SOLID_ANGLE_UNIT ( ) );
#96856 = CARTESIAN_POINT ( 'NONE',  ( 8.099999999999999645, 0.000000000000000000, 0.000000000000000000 ) ) ;
#96857 = CARTESIAN_POINT ( 'NONE',  ( 53.29999999999999716, -3.309500000000000774, 4.475777889183797681E-16 ) ) ;
#96858 = CARTESIAN_POINT ( 'NONE',  ( 63.00956775988831993, -39.48292126951590575, 80.42806493650408584 ) ) ;
#96859 = ORIENTED_EDGE ( 'NONE', *, *, #72149, .T. ) ;
#96860 = ADVANCED_FACE ( 'NONE', ( #83292 ), #19577, .T. ) ;
#96861 = CARTESIAN_POINT ( 'NONE',  ( -7.500000000000006217, 40.28748324523081692, -68.91429205787007106 ) ) ;
#96862 = CARTESIAN_POINT ( 'NONE',  ( 7.188101187500000044, -28.15625000204838813, 0.000000000000000000 ) ) ;
#96863 = SURFACE_STYLE_USAGE ( .BOTH. , #72569 ) ;
#96864 = ORIENTED_EDGE ( 'NONE', *, *, #63933, .T. ) ;
#96865 = CARTESIAN_POINT ( 'NONE',  ( 46.77759138928176696, 18.69812886098186411, 15.64253076101912399 ) ) ;
#96866 = CARTESIAN_POINT ( 'NONE',  ( 85.59800593614014019, 1.016364837396684119E-14, 0.000000000000000000 ) ) ;
#96867 = CARTESIAN_POINT ( 'NONE',  ( -8.000000000000000000, -26.93750000409677625, -9.797174393178825657E-16 ) ) ;
#96868 = CARTESIAN_POINT ( 'NONE',  ( 86.83143111513136603, -35.42916943998449142, 187.7786419653708094 ) ) ;
#96869 = FILL_AREA_STYLE ('',( #56913 ) ) ;
#96870 = CARTESIAN_POINT ( 'NONE',  ( -9.426441968457679010, 10.21013571248348839, 1.586979446726977284E-13 ) ) ;
#96871 = CARTESIAN_POINT ( 'NONE',  ( 7.619701877737481865, -6.825578404672334898, -2.447562251315978710 ) ) ;
#96872 = PRESENTATION_LAYER_ASSIGNMENT (  '', '', ( #102020 ) ) ;
#96873 = CARTESIAN_POINT ( 'NONE',  ( -42.36162206505708383, 485.1874691988857080, -2.398526663485941235 ) ) ;
#96874 = ORIENTED_EDGE ( 'NONE', *, *, #105938, .T. ) ;
#96875 = CIRCLE ( 'NONE', #3878, 4.000000000000007105 ) ;
#96876 = CARTESIAN_POINT ( 'NONE',  ( 25.76161585170470403, -60.00000000000001421, 41.38317439764583128 ) ) ;
#96877 = CARTESIAN_POINT ( 'NONE',  ( -98.98182216182540571, -30.00000000000000711, 144.8605357131832534 ) ) ;
#96878 = EDGE_CURVE ( 'NONE', #35979, #59308, #59571, .T. ) ;
#96879 = CARTESIAN_POINT ( 'NONE',  ( -4.000000000000000000, 0.000000000000000000, -5.703399999999999359 ) ) ;
#96880 = CIRCLE ( 'NONE', #91722, 33.82893434829263413 ) ;
#96881 = CARTESIAN_POINT ( 'NONE',  ( 52.17267667566792255, -57.67659005738761380, 83.18092912029068486 ) ) ;
#96883 = PRESENTATION_STYLE_ASSIGNMENT (( #22500 ) ) ;
#96882 = CARTESIAN_POINT ( 'NONE',  ( -1.249563713075066307, 25.67532180842502854, -39.33688851605202075 ) ) ;
#96884 = EDGE_CURVE ( 'NONE', #94312, #699, #57380, .T. ) ;
#96885 = ADVANCED_FACE ( 'NONE', ( #83819 ), #45322, .T. ) ;
#96886 = CARTESIAN_POINT ( 'NONE',  ( -37.47001784820132286, 40.63832974404387244, -58.98724207561210164 ) ) ;
#96887 = CARTESIAN_POINT ( 'NONE',  ( -30.00000000000004619, 464.1532935782769869, 11.21093587219735355 ) ) ;
#96888 = CARTESIAN_POINT ( 'NONE',  ( -9.435590127033082197, 15.92795519102023860, 3.316968746323895267 ) ) ;
#96889 = DIRECTION ( 'NONE',  ( -1.000000000000000000, -1.224606353822377258E-16, -0.000000000000000000 ) ) ;
#96890 = CARTESIAN_POINT ( 'NONE',  ( -8.202091538805017734, -59.99999999999997868, 39.63445737841648508 ) ) ;
#96891 =( REPRESENTATION_RELATIONSHIP ('NONE','NONE', #69581, #38413 ) REPRESENTATION_RELATIONSHIP_WITH_TRANSFORMATION ( #66488 )SHAPE_REPRESENTATION_RELATIONSHIP( ) );
#96892 = CARTESIAN_POINT ( 'NONE',  ( 1.911035399909858157, -15.42382690385200306, -35.21246151727765294 ) ) ;
#96893 = DIRECTION ( 'NONE',  ( -0.000000000000000000, -1.000000000000000000, -0.000000000000000000 ) ) ;
#96894 = ORIENTED_EDGE ( 'NONE', *, *, #55803, .F. ) ;
#96895 = CARTESIAN_POINT ( 'NONE',  ( 17.50000000000007105, 48.29516379690422667, 64.09945637124668849 ) ) ;
#96896 = CARTESIAN_POINT ( 'NONE',  ( 27.59999999999999787, -4.171999999999999709, 0.000000000000000000 ) ) ;
#96897 = CARTESIAN_POINT ( 'NONE',  ( -11.44799901505533946, -49.92097670987179470, 32.23970761380233796 ) ) ;
#96898 = PRESENTATION_LAYER_ASSIGNMENT (  '', '', ( #15971 ) ) ;
#96900 = PRESENTATION_STYLE_ASSIGNMENT (( #80166 ) ) ;
#96899 = CARTESIAN_POINT ( 'NONE',  ( -88.95083730581535519, -60.00000000000000711, 47.31616727603900330 ) ) ;
#96901 = VERTEX_POINT ( 'NONE', #75186 ) ;
#96902 = EDGE_CURVE ( 'NONE', #21459, #101293, #59102, .T. ) ;
#96903 = CARTESIAN_POINT ( 'NONE',  ( -9.537140126497302361, -5.000000000000002665, -20.99850997557460985 ) ) ;
#96904 = DIRECTION ( 'NONE',  ( -1.000000000000000000, -1.224606353822377258E-16, -0.000000000000000000 ) ) ;
#96905 = COLOUR_RGB ( '', 0.72549020, 0.75294118, 0.79215686) ;
#96906 = DIRECTION ( 'NONE',  ( 0.000000000000000000, 1.000000000000000000, 0.000000000000000000 ) ) ;
#96907 = EDGE_CURVE ( 'NONE', #27202, #77668, #79794, .T. ) ;
#96908 = CARTESIAN_POINT ( 'NONE',  ( -6.928203230275508773, -85.00000000000000000, 4.000000000000001776 ) ) ;
#96909 = CARTESIAN_POINT ( 'NONE',  ( 72.66458305811862317, -60.00000000000000711, 159.4996536347722156 ) ) ;
#96910 = CARTESIAN_POINT ( 'NONE',  ( 0.000000000000000000, 115.0000000000000000, 0.000000000000000000 ) ) ;
#96911 = ORIENTED_EDGE ( 'NONE', *, *, #61270, .F. ) ;
#96912 = DIRECTION ( 'NONE',  ( -0.000000000000000000, -0.000000000000000000, -1.000000000000000000 ) ) ;
#96913 = DIRECTION ( 'NONE',  ( -0.000000000000000000, -0.000000000000000000, -1.000000000000000000 ) ) ;
#96914 = EDGE_CURVE ( 'NONE', #72376, #77950, #19489, .T. ) ;
#96915 = FACE_OUTER_BOUND ( 'NONE', #59248, .T. ) ;
#96916 = CARTESIAN_POINT ( 'NONE',  ( -4.725902370230324223, -2.526352736915706387, 103.4500010546506275 ) ) ;
#96917 = ORIENTED_EDGE ( 'NONE', *, *, #86906, .T. ) ;
#96918 = CARTESIAN_POINT ( 'NONE',  ( -29.85348551950092855, 328.3076999754412100, 14.69459570409856219 ) ) ;
#96919 = ORIENTED_EDGE ( 'NONE', *, *, #92820, .F. ) ;
#96920 = FACE_OUTER_BOUND ( 'NONE', #86305, .T. ) ;
#96921 = VERTEX_POINT ( 'NONE', #32653 ) ;
#96922 = CARTESIAN_POINT ( 'NONE',  ( 6.846801517543655180, -12.21872792266575658, 8.794481130080901821 ) ) ;
#96923 = CARTESIAN_POINT ( 'NONE',  ( -104.7668148436344495, -60.00000000001475797, 202.3575108280591337 ) ) ;
#96924 = CARTESIAN_POINT ( 'NONE',  ( 46.00000000000000000, 488.0078051103527059, -0.5538049991179438969 ) ) ;
#96925 = CARTESIAN_POINT ( 'NONE',  ( 76.75507714372903934, -60.00000000000002132, 189.7492337977039654 ) ) ;
#96926 = CARTESIAN_POINT ( 'NONE',  ( 106.4000000000000057, 0.000000000000000000, 0.000000000000000000 ) ) ;
#96927 = DIRECTION ( 'NONE',  ( 0.000000000000000000, 1.000000000000000000, 0.000000000000000000 ) ) ;
#96929 = CARTESIAN_POINT ( 'NONE',  ( 13.71723278984751815, -56.87769479953498575, 33.46138947822615251 ) ) ;
#96928 = CARTESIAN_POINT ( 'NONE',  ( -108.5047409391136455, -30.00000000000001776, 153.5997188701533105 ) ) ;
#96930 = CARTESIAN_POINT ( 'NONE',  ( 82.72479378746378131, -37.99999999999997868, 3.475805411804568923 ) ) ;
#96931 = CARTESIAN_POINT ( 'NONE',  ( 0.1685780251646490369, 54.30395748168558612, -7.758569535635805536 ) ) ;
#96932 = CARTESIAN_POINT ( 'NONE',  ( -46.36168458591362196, -60.26899542073847726, 51.31494294901810349 ) ) ;
#96933 = FACE_OUTER_BOUND ( 'NONE', #8660, .T. ) ;
#96934 = B_SPLINE_CURVE_WITH_KNOTS ( 'NONE', 3,
 ( #57405, #90321, #15900, #97878 ),
 .UNSPECIFIED., .F., .F.,
 ( 4, 4 ),
 ( 0.000000000000000000, 0.001874406674510234461 ),
 .UNSPECIFIED. ) ;
#96935 = ORIENTED_EDGE ( 'NONE', *, *, #23903, .T. ) ;
#96936 = DIRECTION ( 'NONE',  ( 0.000000000000000000, 0.000000000000000000, 1.000000000000000000 ) ) ;
#96937 = CARTESIAN_POINT ( 'NONE',  ( -43.72966438978023973, 434.3041953058478839, 13.93761445528323861 ) ) ;
#96938 = CIRCLE ( 'NONE', #17720, 59.50000000000000000 ) ;
#96939 = FILL_AREA_STYLE ('',( #50891 ) ) ;
#96940 = DIRECTION ( 'NONE',  ( -1.000000000000000000, -1.224606353822377258E-16, -0.000000000000000000 ) ) ;
#96941 = DIRECTION ( 'NONE',  ( 0.000000000000000000, 0.000000000000000000, 1.000000000000000000 ) ) ;
#96942 = CARTESIAN_POINT ( 'NONE',  ( 33.63427961064055438, 325.9154870834976236, -4.827994974213513757 ) ) ;
#96943 = ORIENTED_EDGE ( 'NONE', *, *, #17873, .T. ) ;
#96944 = DIRECTION ( 'NONE',  ( -0.000000000000000000, -0.000000000000000000, -1.000000000000000000 ) ) ;
#96945 = EDGE_LOOP ( 'NONE', ( #3918, #73476, #16366 ) ) ;
#96946 = CARTESIAN_POINT ( 'NONE',  ( 91.10875621309618566, -29.99999999996073896, 199.5150240557169354 ) ) ;
#96947 = CARTESIAN_POINT ( 'NONE',  ( 46.00000000000000000, 461.6622277975422435, 10.18145404766785589 ) ) ;
#96948 = CARTESIAN_POINT ( 'NONE',  ( 5.425084639653764640, 41.91238126396859798, -59.10640578674440349 ) ) ;
#96949 = CARTESIAN_POINT ( 'NONE',  ( 5.022013495247499293, 18.64316884711714195, -38.36535705883633085 ) ) ;
#96950 = CARTESIAN_POINT ( 'NONE',  ( 99.76087090034495475, -30.00000000000000355, 151.2002837684392489 ) ) ;
#96951 = AXIS2_PLACEMENT_3D ( 'NONE', #21970, #53774, #71022 ) ;
#96952 = CARTESIAN_POINT ( 'NONE',  ( 0.01678220609565910307, 0.7854258609844483319, 8.000000000000001776 ) ) ;
#96953 = ORIENTED_EDGE ( 'NONE', *, *, #35503, .F. ) ;
#96954 = EDGE_CURVE ( 'NONE', #20871, #55395, #96977, .T. ) ;
#96955 = VERTEX_POINT ( 'NONE', #26174 ) ;
#96956 = ORIENTED_EDGE ( 'NONE', *, *, #71716, .T. ) ;
#96957 = FACE_OUTER_BOUND ( 'NONE', #41027, .T. ) ;
#96958 = CARTESIAN_POINT ( 'NONE',  ( 43.59756234217347526, 434.3244621007142996, 14.55946156040239003 ) ) ;
#96959 = CARTESIAN_POINT ( 'NONE',  ( 0.000000000000000000, 0.000000000000000000, -0.02540000000000007530 ) ) ;
#96960 = EDGE_CURVE ( 'NONE', #101, #79036, #91920, .T. ) ;
#96961 = ORIENTED_EDGE ( 'NONE', *, *, #67743, .F. ) ;
#96963 = EDGE_CURVE ( 'NONE', #73917, #741, #81784, .T. ) ;
#96962 = CARTESIAN_POINT ( 'NONE',  ( -16.02336867590704728, 4.077607736808446681, 2.243736929358616461 ) ) ;
#96964 = EDGE_LOOP ( 'NONE', ( #24130, #11083, #22884, #71244 ) ) ;
#96965 = DIRECTION ( 'NONE',  ( 0.5735764363510466035, -0.8191520442889914655, 1.003171929053524500E-16 ) ) ;
#96966 = CARTESIAN_POINT ( 'NONE',  ( 79.25291760674103614, -38.71628596270740985, 191.5093671535432520 ) ) ;
#96967 = CARTESIAN_POINT ( 'NONE',  ( 12.35959284188919938, 9.760562649644960231, 9.476716774057315718 ) ) ;
#96968 = CARTESIAN_POINT ( 'NONE',  ( 82.98893668538087809, -37.84625678214262479, -0.6931496944285937545 ) ) ;
#96969 = CARTESIAN_POINT ( 'NONE',  ( 80.69144941626747425, -37.99999999999993605, 148.5548834094500137 ) ) ;
#96970 = CARTESIAN_POINT ( 'NONE',  ( 38.19591848881191964, 317.3555448089408060, 15.41710542503021131 ) ) ;
#96971 = CARTESIAN_POINT ( 'NONE',  ( 42.75230560876955366, 485.3312079086152266, -3.156031357493472189 ) ) ;
#96972 = CARTESIAN_POINT ( 'NONE',  ( -42.45811724857414049, 486.4202366696187596, 8.302074271984052345 ) ) ;
#96973 = EDGE_CURVE ( 'NONE', #86927, #70548, #93527, .T. ) ;
#96974 = DIRECTION ( 'NONE',  ( 0.000000000000000000, 0.000000000000000000, 1.000000000000000000 ) ) ;
#96975 = CARTESIAN_POINT ( 'NONE',  ( 42.23213459610285980, 347.2701562730458704, 14.17138388578061381 ) ) ;
#96976 = ORIENTED_EDGE ( 'NONE', *, *, #38528, .F. ) ;
#96977 = CIRCLE ( 'NONE', #33240, 5.000000000000001776 ) ;
#96978 =( NAMED_UNIT ( * ) PLANE_ANGLE_UNIT ( ) SI_UNIT ( $, .RADIAN. ) );
#96979 = CARTESIAN_POINT ( 'NONE',  ( -38.11704196078224527, 460.5925777724487489, 2.566592005033819568 ) ) ;
#96980 = MECHANICAL_DESIGN_GEOMETRIC_PRESENTATION_REPRESENTATION (  '', ( #102134 ), #62569 ) ;
#96981 = CARTESIAN_POINT ( 'NONE',  ( -27.10511071441182906, 36.60571256639526894, 10.05698433968618488 ) ) ;
#96982 = ORIENTED_EDGE ( 'NONE', *, *, #15652, .T. ) ;
#96983 = CARTESIAN_POINT ( 'NONE',  ( -18.99999999999999289, -4.000000000000000000, -1.500000000000001332 ) ) ;
#96984 = CARTESIAN_POINT ( 'NONE',  ( -25.67144724221197905, 305.2079960181984006, 10.46496832936455412 ) ) ;
#96985 = CARTESIAN_POINT ( 'NONE',  ( -12.48044894998514742, -3.649665456917388973, -76.71620004746266375 ) ) ;
#96986 = UNCERTAINTY_MEASURE_WITH_UNIT (LENGTH_MEASURE( 1.000000000000000082E-05 ), #12661, 'distance_accuracy_value', 'NONE');
#96987 = CARTESIAN_POINT ( 'NONE',  ( 5.656854249492380582, -15.31249999999999289, -5.656854249492379694 ) ) ;
#96988 = VECTOR ( 'NONE', #11257, 1000.000000000000000 ) ;
#96989 = CARTESIAN_POINT ( 'NONE',  ( -44.45120377230485786, 484.8901964262616389, 4.471885531209228937 ) ) ;
#96990 =( NAMED_UNIT ( * ) SI_UNIT ( $, .STERADIAN. ) SOLID_ANGLE_UNIT ( ) );
#96992 = ORIENTED_EDGE ( 'NONE', *, *, #30920, .F. ) ;
#96991 =( BOUNDED_SURFACE ( )  B_SPLINE_SURFACE ( 3, 2, ( 
 ( #59989, #68046, #102004 ),
 ( #84768, #19014, #49325 ),
 ( #61038, #76661, #51856 ),
 ( #43771, #67532, #93925 ),
 ( #82232, #100412, #101484 ),
 ( #20084, #98421, #26575 ),
 ( #27637, #60515, #8345 ),
 ( #93401, #59444, #19550 ),
 ( #86907, #55030, #70710 ),
 ( #45382, #61576, #104121 ) ),
 .UNSPECIFIED., .F., .F., .T. ) 
 B_SPLINE_SURFACE_WITH_KNOTS ( ( 4, 2, 2, 2, 4 ),
 ( 3, 3 ),
 ( -1.185673698478311820E-05, 0.001059589481406181949, 0.002131035699797147187, 0.003202481918188112425, 0.004273928136579077663 ),
 ( 0.000000000000000000, 1.000000000000000000 ),
 .UNSPECIFIED. ) 
 GEOMETRIC_REPRESENTATION_ITEM ( )  RATIONAL_B_SPLINE_SURFACE ( (
 ( 1.000000000000000000, 1.000000000000000000, 1.000000000000000000),
 ( 1.000000000000000000, 0.9999922502423410631, 1.000000000000000000),
 ( 1.000000000000000000, 0.9961090584666346670, 1.000000000000000000),
 ( 1.000000000000000000, 0.9800114100223730196, 1.000000000000000000),
 ( 1.000000000000000000, 0.9677016975220472661, 1.000000000000000000),
 ( 1.000000000000000000, 0.9345728642045315615, 1.000000000000000000),
 ( 1.000000000000000000, 0.9137480076090285230, 1.000000000000000000),
 ( 1.000000000000000000, 0.8628371017890346106, 1.000000000000000000),
 ( 1.000000000000000000, 0.8327438998408613902, 1.000000000000000000),
 ( 1.000000000000000000, 0.7973879088788907721, 1.000000000000000000) ) ) 
 REPRESENTATION_ITEM ( '' )  SURFACE ( )  );
#96993 = CARTESIAN_POINT ( 'NONE',  ( 85.70847550465963138, -32.07071322668284807, 182.3195111745817769 ) ) ;
#96994 = SURFACE_STYLE_FILL_AREA ( #22067 ) ;
#96995 = VERTEX_POINT ( 'NONE', #74133 ) ;
#96996 = CARTESIAN_POINT ( 'NONE',  ( 94.76232204274911908, -57.67206613426113648, 30.20201912920926901 ) ) ;
#96997 = FACE_OUTER_BOUND ( 'NONE', #51364, .T. ) ;
#96998 = LINE ( 'NONE', #15004, #93735 ) ;
#96999 =( NAMED_UNIT ( * ) PLANE_ANGLE_UNIT ( ) SI_UNIT ( $, .RADIAN. ) );
#97000 = CARTESIAN_POINT ( 'NONE',  ( 28.71549002649010518, 15.67055689680115016, 41.65541077617245946 ) ) ;
#97001 = CARTESIAN_POINT ( 'NONE',  ( -0.5974722283283669944, 8.315303285985685022, -0.7026937717022826435 ) ) ;
#97003 = CARTESIAN_POINT ( 'NONE',  ( -13.03847614980558411, 6.113859727637795949, 7.290527864909715383 ) ) ;
#97002 = CARTESIAN_POINT ( 'NONE',  ( 41.59976546006239317, 472.6866688315437841, 16.01926328807780564 ) ) ;
#97004 = EDGE_CURVE ( 'NONE', #80390, #94562, #7272, .T. ) ;
#97005 = CARTESIAN_POINT ( 'NONE',  ( 42.45852508622710531, 486.4193484895208712, 8.300531886079083321 ) ) ;
#97006 = CARTESIAN_POINT ( 'NONE',  ( -27.10511071441192144, 36.60571256639527604, -10.05698433968589178 ) ) ;
#97007 = CARTESIAN_POINT ( 'NONE',  ( -31.04749644452845914, -30.39921546070477731, -30.04532190092515620 ) ) ;
#97008 = CARTESIAN_POINT ( 'NONE',  ( 43.47770857297122404, 484.8227827122696567, 4.253339224811428565 ) ) ;
#97009 = COLOUR_RGB ( '', 0.09019608, 0.27058824, 0.51372549) ;
#97010 = EDGE_LOOP ( 'NONE', ( #8703, #19593, #31654, #61036, #23277 ) ) ;
#97011 = PRESENTATION_STYLE_ASSIGNMENT (( #72211 ) ) ;
#97012 = PRESENTATION_STYLE_ASSIGNMENT (( #37761 ) ) ;
#97013 = AXIS2_PLACEMENT_3D ( 'NONE', #53525, #86454, #104184 ) ;
#97014 = DIRECTION ( 'NONE',  ( 0.000000000000000000, 0.000000000000000000, -1.000000000000000000 ) ) ;
#97016 = CARTESIAN_POINT ( 'NONE',  ( -48.31675829002472256, -60.22826300482149975, -32.41392416354486983 ) ) ;
#97015 = FACE_OUTER_BOUND ( 'NONE', #35014, .T. ) ;
#97017 = ORIENTED_EDGE ( 'NONE', *, *, #102806, .F. ) ;
#97019 = EDGE_LOOP ( 'NONE', ( #26055, #70696, #2894, #80101, #103647 ) ) ;
#97018 = AXIS2_PLACEMENT_3D ( 'NONE', #14436, #54898, #62490 ) ;
#97020 =( LENGTH_UNIT ( ) NAMED_UNIT ( * ) SI_UNIT ( .MILLI., .METRE. ) );
#97021 = LINE ( 'NONE', #63622, #27048 ) ;
#97022 = CARTESIAN_POINT ( 'NONE',  ( -91.89520039571972632, -60.00000000000000711, -14.34466715436823492 ) ) ;
#97023 = ORIENTED_EDGE ( 'NONE', *, *, #50831, .T. ) ;
#97024 = CARTESIAN_POINT ( 'NONE',  ( -6.298933871243637128, 41.33266196705881157, -58.30935828777566599 ) ) ;
#97025 = CARTESIAN_POINT ( 'NONE',  ( -12.50000000000000355, -3.000000000000001776, -76.70872284621019332 ) ) ;
#97026 = CARTESIAN_POINT ( 'NONE',  ( 98.08802719723102825, -37.75359325362526874, 192.4663707679745244 ) ) ;
#97028 = FACE_OUTER_BOUND ( 'NONE', #24400, .T. ) ;
#97027 =( LENGTH_UNIT ( ) NAMED_UNIT ( * ) SI_UNIT ( .MILLI., .METRE. ) );
#97029 = EDGE_CURVE ( 'NONE', #56041, #47515, #38118, .T. ) ;
#97030 = CARTESIAN_POINT ( 'NONE',  ( -80.33501531167325993, -56.88691000900035988, 172.5936903209407660 ) ) ;
#97031 = EDGE_LOOP ( 'NONE', ( #21561, #94680, #65808, #92243 ) ) ;
#97032 = TOROIDAL_SURFACE ( 'NONE', #12643, 5.999999999999996447, 4.000000000000000000 ) ;
#97033 = VERTEX_POINT ( 'NONE', #64993 ) ;
#97034 = ORIENTED_EDGE ( 'NONE', *, *, #30072, .T. ) ;
#97035 = CARTESIAN_POINT ( 'NONE',  ( 41.46910480218704009, 484.7338956289814860, -3.418960549715446717 ) ) ;
#97036 = MECHANICAL_DESIGN_GEOMETRIC_PRESENTATION_REPRESENTATION (  '', ( #69499 ), #78108 ) ;
#97037 = CARTESIAN_POINT ( 'NONE',  ( -5.962730926206976534, -13.90752838006589442, 13.89020537729797766 ) ) ;
#97038 = ORIENTED_EDGE ( 'NONE', *, *, #53423, .T. ) ;
#97039 = CARTESIAN_POINT ( 'NONE',  ( -121.1901574356003550, 4.501353321498349658, 60.59507871780017041 ) ) ;
#97040 = CARTESIAN_POINT ( 'NONE',  ( -9.403185743875484448, 15.24615751665884389, -3.409011323176772912 ) ) ;
#97041 = CARTESIAN_POINT ( 'NONE',  ( -77.81697554521740301, -57.51284286114859157, 196.3444844341304929 ) ) ;
#97042 = CARTESIAN_POINT ( 'NONE',  ( -4.521127550501226722, -65.67610240527666576, 3.944701057164355706 ) ) ;
#97043 = FACE_OUTER_BOUND ( 'NONE', #79434, .T. ) ;
#97044 = AXIS2_PLACEMENT_3D ( 'NONE', #100426, #65414, #1168 ) ;
#97045 = CARTESIAN_POINT ( 'NONE',  ( -26.97491686565329161, 307.4599153070161606, -9.420584459367196573 ) ) ;
#97046 = CARTESIAN_POINT ( 'NONE',  ( 1.099700806557082355, 27.96998724311644935, -38.88428954940741988 ) ) ;
#97047 = CARTESIAN_POINT ( 'NONE',  ( -75.59778980771257295, -60.00000000000000711, -32.85486631586996253 ) ) ;
#97048 = CARTESIAN_POINT ( 'NONE',  ( -32.49743750560201505, -59.99999999999998579, 47.28107978972537495 ) ) ;
#97049 = CARTESIAN_POINT ( 'NONE',  ( -52.96930251354979902, -22.17327373329827722, 49.74579268807322308 ) ) ;
#97050 = ORIENTED_EDGE ( 'NONE', *, *, #77849, .T. ) ;
#97051 = CARTESIAN_POINT ( 'NONE',  ( 1.796381498081899508, 21.43623042924785693, -6.770105592763798086 ) ) ;
#97052 = ORIENTED_EDGE ( 'NONE', *, *, #100243, .T. ) ;
#97053 = CARTESIAN_POINT ( 'NONE',  ( -99.57258923306162046, -45.25279128809092555, 192.9568983376553035 ) ) ;
#97054 = CARTESIAN_POINT ( 'NONE',  ( -5.515535885668342964, 296.1986775320586958, -10.01281319186906948 ) ) ;
#97055 = ORIENTED_EDGE ( 'NONE', *, *, #91312, .T. ) ;
#97056 = CARTESIAN_POINT ( 'NONE',  ( 19.43573259364688965, 49.96699249044939961, 60.75465309941666447 ) ) ;
#97057 = CARTESIAN_POINT ( 'NONE',  ( 109.2343739603617507, -38.35611523210522478, 189.3471561603757038 ) ) ;
#97058 = LINE ( 'NONE', #8579, #70887 ) ;
#97059 = CARTESIAN_POINT ( 'NONE',  ( 6.831979103402614051, 3.295157223185828155, -6.443785395948805395 ) ) ;
#97060 = CARTESIAN_POINT ( 'NONE',  ( -8.647927412449892159, 302.6863289723537491, 9.901865204233580187 ) ) ;
#97061 = FACE_OUTER_BOUND ( 'NONE', #7889, .T. ) ;
#97063 = CARTESIAN_POINT ( 'NONE',  ( 85.00342762049730538, -29.99999999999999289, 170.3482649358438152 ) ) ;
#97062 = UNCERTAINTY_MEASURE_WITH_UNIT (LENGTH_MEASURE( 1.000000000000000082E-05 ), #102514, 'distance_accuracy_value', 'NONE');
#97064 = B_SPLINE_SURFACE_WITH_KNOTS ( 'NONE', 1, 3, ( 
 ( #94785, #20930, #86693, #86167, #102317, #28469, #94238, #19860 ),
 ( #45685, #12235, #35493, #4163, #12762, #27417, #60297, #37094 ) ),
 .UNSPECIFIED., .F., .F., .F.,
 ( 2, 2 ),
 ( 4, 2, 2, 4 ),
 ( 0.000000000000000000, 1.000000000000000000 ),
 ( 0.000000000000000000, 0.04450745600790868145, 0.06676118401186306728, 0.08901491201581737678 ),
 .UNSPECIFIED. ) ;
#97065 = FACE_OUTER_BOUND ( 'NONE', #81687, .T. ) ;
#97066 = CARTESIAN_POINT ( 'NONE',  ( 0.000000000000000000, 0.000000000000000000, -1.581124522925831499 ) ) ;
#97067 = CARTESIAN_POINT ( 'NONE',  ( 3.337162542380456721E-15, 35.08181111624585213, 27.25000000000000000 ) ) ;
#97068 = CARTESIAN_POINT ( 'NONE',  ( -32.87537929228375333, 485.0716560791295819, 1.465306988351862572 ) ) ;
#97069 = ORIENTED_EDGE ( 'NONE', *, *, #60368, .T. ) ;
#97070 = ORIENTED_EDGE ( 'NONE', *, *, #42075, .F. ) ;
#97071 = CARTESIAN_POINT ( 'NONE',  ( 49.74709343585908528, -32.58936152964536603, 48.06759981570923657 ) ) ;
#97072 = DIRECTION ( 'NONE',  ( -0.000000000000000000, 1.000000000000000000, -0.000000000000000000 ) ) ;
#97073 = CYLINDRICAL_SURFACE ( 'NONE', #27328, 3.400000000000000355 ) ;
#97074 = ADVANCED_FACE ( 'NONE', ( #217 ), #22450, .F. ) ;
#97075 = B_SPLINE_CURVE_WITH_KNOTS ( 'NONE', 3,
 ( #57428, #73076, #15929, #7292 ),
 .UNSPECIFIED., .F., .F.,
 ( 4, 4 ),
 ( 3.469446951953614189E-18, 0.0006941752209891988374 ),
 .UNSPECIFIED. ) ;
#97076 = CARTESIAN_POINT ( 'NONE',  ( -110.4642460645833637, -38.35610247955116137, 182.6975338912728262 ) ) ;
#97077 = EDGE_LOOP ( 'NONE', ( #41457, #62514, #104126, #100097, #30751, #33133 ) ) ;
#97078 = CARTESIAN_POINT ( 'NONE',  ( 89.17615470242493814, -38.38424890164885284, -17.73986973391627231 ) ) ;
#97079 = CARTESIAN_POINT ( 'NONE',  ( 10.65963400673390638, 18.20553819351006908, -9.432268096413945813 ) ) ;
#97080 = CARTESIAN_POINT ( 'NONE',  ( -19.44565830096107106, 49.97416012492340087, 60.66528512595754563 ) ) ;
#97081 = SURFACE_SIDE_STYLE ('',( #5939 ) ) ;
#97082 = CARTESIAN_POINT ( 'NONE',  ( 101.2421465956972355, -45.28276229600517411, 139.7551188333355014 ) ) ;
#97083 = CARTESIAN_POINT ( 'NONE',  ( 11.08349330513380515, 1.593028355512270962E-15, 0.000000000000000000 ) ) ;
#97084 =( LENGTH_UNIT ( ) NAMED_UNIT ( * ) SI_UNIT ( .MILLI., .METRE. ) );
#97085 = CARTESIAN_POINT ( 'NONE',  ( -35.51301801062162866, 414.8830440580413210, 6.892597979060226976 ) ) ;
#97086 = CIRCLE ( 'NONE', #102252, 1.999999999999998224 ) ;
#97087 = PRESENTATION_STYLE_ASSIGNMENT (( #39407 ) ) ;
#97088 = CARTESIAN_POINT ( 'NONE',  ( 83.18737980040994273, -60.00000000000000000, 198.9619646874331522 ) ) ;
#97089 = AXIS2_PLACEMENT_3D ( 'NONE', #66797, #82442, #18265 ) ;
#97090 = EDGE_CURVE ( 'NONE', #77591, #93546, #67800, .T. ) ;
#97091 = SURFACE_SIDE_STYLE ('',( #104653 ) ) ;
#97092 = ORIENTED_EDGE ( 'NONE', *, *, #43266, .T. ) ;
#97093 = CARTESIAN_POINT ( 'NONE',  ( 54.89891884253371757, -56.84790269950949693, 67.23841002115719334 ) ) ;
#97094 = EDGE_CURVE ( 'NONE', #74232, #49696, #78005, .T. ) ;
#97095 = CARTESIAN_POINT ( 'NONE',  ( -31.90403345410906155, 299.1470781681827020, -1.045240008406338017 ) ) ;
#97096 = DIRECTION ( 'NONE',  ( 0.000000000000000000, -1.000000000000000000, 0.000000000000000000 ) ) ;
#97097 = CARTESIAN_POINT ( 'NONE',  ( -13.49999999999999645, 0.000000000000000000, -13.00000000000000000 ) ) ;
#97098 = ORIENTED_EDGE ( 'NONE', *, *, #50933, .F. ) ;
#97100 = CARTESIAN_POINT ( 'NONE',  ( -14.89113977972644420, 23.12270858405653584, 0.2439221067019188838 ) ) ;
#97099 = CARTESIAN_POINT ( 'NONE',  ( -108.4974870776933216, -38.35706132716640582, 191.6606617528426852 ) ) ;
#97101 = CARTESIAN_POINT ( 'NONE',  ( 8.000000000000001776, -2.999999999999999556, 1.047197551196597853 ) ) ;
#97102 = FACE_OUTER_BOUND ( 'NONE', #38441, .T. ) ;
#97103 = DIRECTION ( 'NONE',  ( 0.000000000000000000, -1.000000000000000000, 0.000000000000000000 ) ) ;
#97104 = CARTESIAN_POINT ( 'NONE',  ( 5.082755093536325930, -10.34375000204838457, -5.082755093536325042 ) ) ;
#97105 = CARTESIAN_POINT ( 'NONE',  ( -9.999999999999996447, -5.000000000000002665, -83.69100306252320820 ) ) ;
#97106 = EDGE_CURVE ( 'NONE', #25883, #104525, #21325, .T. ) ;
#97107 = EDGE_LOOP ( 'NONE', ( #42057, #105211, #34872, #67148 ) ) ;
#97108 = CARTESIAN_POINT ( 'NONE',  ( 84.37186861624395817, -32.45071114265312673, 171.8667827280741562 ) ) ;
#97109 = CARTESIAN_POINT ( 'NONE',  ( -46.00000000000000000, 463.6727721072930422, 9.768113441060686242 ) ) ;
#97110 = CARTESIAN_POINT ( 'NONE',  ( -34.80483904954093788, 439.1570050480630698, 24.08402132645205640 ) ) ;
#97111 = ORIENTED_EDGE ( 'NONE', *, *, #59439, .T. ) ;
#97112 = FACE_OUTER_BOUND ( 'NONE', #55567, .T. ) ;
#97113 = AXIS2_PLACEMENT_3D ( 'NONE', #41797, #9961, #50406 ) ;
#97114 = CARTESIAN_POINT ( 'NONE',  ( 6.618366600630476881, -4.380080200177129512, -16.79229307443610608 ) ) ;
#97115 = CARTESIAN_POINT ( 'NONE',  ( 38.81331445831525429, 485.4137471979039447, -4.286058349641296950 ) ) ;
#97116 = LINE ( 'NONE', #96606, #3874 ) ;
#97117 = CARTESIAN_POINT ( 'NONE',  ( 25.21823338009918203, 6.123233995736772199E-16, -5.000000000000001776 ) ) ;
#97118 =( BOUNDED_SURFACE ( )  B_SPLINE_SURFACE ( 3, 2, ( 
 ( #71965, #97291, #64422 ),
 ( #80570, #89217, #22913 ),
 ( #16374, #106438, #32598 ),
 ( #74073, #39617, #82166 ) ),
 .UNSPECIFIED., .F., .F., .F. ) 
 B_SPLINE_SURFACE_WITH_KNOTS ( ( 4, 4 ),
 ( 3, 3 ),
 ( -4.336808689942017736E-19, 0.001861785345366374737 ),
 ( 0.000000000000000000, 1.000000000000000000 ),
 .UNSPECIFIED. ) 
 GEOMETRIC_REPRESENTATION_ITEM ( )  RATIONAL_B_SPLINE_SURFACE ( (
 ( 1.000000000000000000, 0.7560596356357087711, 1.000000000000000000),
 ( 1.000000000000000000, 0.7634190799318362197, 1.000000000000000000),
 ( 1.000000000000000000, 0.7696912645870082059, 1.000000000000000000),
 ( 1.000000000000000000, 0.7737149417968428589, 1.000000000000000000) ) ) 
 REPRESENTATION_ITEM ( '' )  SURFACE ( )  );
#97119 = VECTOR ( 'NONE', #69409, 1000.000000000000000 ) ;
#97120 = VERTEX_POINT ( 'NONE', #10989 ) ;
#97121 =( GEOMETRIC_REPRESENTATION_CONTEXT ( 3 ) GLOBAL_UNCERTAINTY_ASSIGNED_CONTEXT ( ( #32755 ) ) GLOBAL_UNIT_ASSIGNED_CONTEXT ( ( #55581, #55058, #79872 ) ) REPRESENTATION_CONTEXT ( 'NONE', 'WORKASPACE' ) );
#97122 = VECTOR ( 'NONE', #487, 1000.000000000000000 ) ;
#97123 = DIRECTION ( 'NONE',  ( 1.000000000000000000, -0.000000000000000000, -0.000000000000000000 ) ) ;
#97124 = CARTESIAN_POINT ( 'NONE',  ( -4.448407490268950326, -48.03096409756967944, 102.6871849564181218 ) ) ;
#97126 = CARTESIAN_POINT ( 'NONE',  ( -12.34042576123834500, 7.435900281208858154, -8.326420812669903526 ) ) ;
#97125 = CARTESIAN_POINT ( 'NONE',  ( 34.88900972249397370, 464.6206820655982028, 18.69027339340997784 ) ) ;
#97127 = EDGE_CURVE ( 'NONE', #91765, #36600, #23011, .T. ) ;
#97128 = CARTESIAN_POINT ( 'NONE',  ( -7.188101187500000044, -18.40625000204838457, -8.802885111219163269E-16 ) ) ;
#97129 = CARTESIAN_POINT ( 'NONE',  ( -29.59387530091278862, 18.41945862786178623, -39.60535821593474992 ) ) ;
#97130 = CONTEXT_DEPENDENT_SHAPE_REPRESENTATION ( #41135, #88200 ) ;
#97131 = VERTEX_POINT ( 'NONE', #2372 ) ;
#97132 = CARTESIAN_POINT ( 'NONE',  ( 7.915340744421998309, 3.857466640755272902, -7.913699667209542987 ) ) ;
#97133 = CARTESIAN_POINT ( 'NONE',  ( -8.420691126345804634, 123.3228360287961607, -1.270215581529552804E-12 ) ) ;
#97134 = EDGE_CURVE ( 'NONE', #56766, #12068, #106244, .T. ) ;
#97135 = LINE ( 'NONE', #80949, #70501 ) ;
#97136 = FACE_OUTER_BOUND ( 'NONE', #35472, .T. ) ;
#97137 = CIRCLE ( 'NONE', #33426, 11.00000000000000000 ) ;
#97138 = VERTEX_POINT ( 'NONE', #51458 ) ;
#97139 = CARTESIAN_POINT ( 'NONE',  ( 83.28888888888889142, 4.172000000000019249, 5.109226446042768454E-16 ) ) ;
#97140 = FACE_OUTER_BOUND ( 'NONE', #10006, .T. ) ;
#97141 = ORIENTED_EDGE ( 'NONE', *, *, #100772, .T. ) ;
#97142 = DIRECTION ( 'NONE',  ( 0.000000000000000000, 1.000000000000000000, 0.000000000000000000 ) ) ;
#97143 = DIRECTION ( 'NONE',  ( -1.000000000000000000, -1.224606353822377258E-16, -0.000000000000000000 ) ) ;
#97144 = CARTESIAN_POINT ( 'NONE',  ( -109.9681397012935378, -60.00000000000001421, 143.1854525654455870 ) ) ;
#97145 = CARTESIAN_POINT ( 'NONE',  ( 28.56372199056505323, 18.54333498561200955, -40.29094744152394014 ) ) ;
#97146 = COLOUR_RGB ( '', 0.31764706, 0.68627451, 0.89019608) ;
#97147 = CYLINDRICAL_SURFACE ( 'NONE', #51181, 8.000000000000000000 ) ;
#97149 =( LENGTH_UNIT ( ) NAMED_UNIT ( * ) SI_UNIT ( .MILLI., .METRE. ) );
#97148 = CARTESIAN_POINT ( 'NONE',  ( -11.68767211932356531, -5.000000000000002665, -81.85902538601600043 ) ) ;
#97150 = EDGE_CURVE ( 'NONE', #10693, #20907, #71492, .T. ) ;
#97151 = CARTESIAN_POINT ( 'NONE',  ( -82.76128424870692868, -46.49188429553897350, 178.0646004425870501 ) ) ;
#97152 = ORIENTED_EDGE ( 'NONE', *, *, #103239, .F. ) ;
#97153 = STYLED_ITEM ( 'NONE', ( #100088 ), #85105 ) ;
#97154 = CARTESIAN_POINT ( 'NONE',  ( 7.500000000000005329, 24.91666666666666430, -71.71180648257555390 ) ) ;
#97155 = ORIENTED_EDGE ( 'NONE', *, *, #81791, .T. ) ;
#97156 = FACE_OUTER_BOUND ( 'NONE', #59387, .T. ) ;
#97157 = EDGE_CURVE ( 'NONE', #48423, #75037, #43684, .T. ) ;
#97158 = CARTESIAN_POINT ( 'NONE',  ( 17.33349330513380337, 4.000000000000003553, 0.000000000000000000 ) ) ;
#97159 = DIRECTION ( 'NONE',  ( -1.000000000000000000, -1.224606353822377258E-16, -0.000000000000000000 ) ) ;
#97160 = CARTESIAN_POINT ( 'NONE',  ( -15.05785784214673306, 3.824195276770051777, -4.604276673498573835 ) ) ;
#97161 = CARTESIAN_POINT ( 'NONE',  ( 3.021274963871837915, 47.67782550506024108, -5.000000000000000000 ) ) ;
#97162 = CARTESIAN_POINT ( 'NONE',  ( -2.370187320824404864, -5.000000000000000000, -97.83589316745488418 ) ) ;
#97163 = CARTESIAN_POINT ( 'NONE',  ( -43.32920196732008122, 484.9664025106967529, 4.870547201827349681 ) ) ;
#97164 = EDGE_CURVE ( 'NONE', #22876, #68944, #48826, .T. ) ;
#97165 = CARTESIAN_POINT ( 'NONE',  ( 109.0818019194042847, -30.00000000000000355, 182.6293461004923131 ) ) ;
#97166 = CARTESIAN_POINT ( 'NONE',  ( -104.6655502547336738, -29.99999999999993250, 124.7729330896767408 ) ) ;
#97167 = CARTESIAN_POINT ( 'NONE',  ( -63.09091515402169392, -32.53411138963832627, 77.17286524773658130 ) ) ;
#97168 = ORIENTED_EDGE ( 'NONE', *, *, #93847, .F. ) ;
#97169 = CARTESIAN_POINT ( 'NONE',  ( 63.23722314639035602, 38.95364102865269018, -7.942460742852443190 ) ) ;
#97170 = CARTESIAN_POINT ( 'NONE',  ( 74.89656030667543973, -59.99999999998028244, 191.9882623802560317 ) ) ;
#97171 = EDGE_LOOP ( 'NONE', ( #70745, #61226, #58044, #79516, #2420 ) ) ;
#97172 = FACE_OUTER_BOUND ( 'NONE', #65582, .T. ) ;
#97173 = CARTESIAN_POINT ( 'NONE',  ( 7.188101187500000933, -20.93750000204839168, -2.977408999572650483 ) ) ;
#97174 = DIRECTION ( 'NONE',  ( 1.000000000000000000, 0.000000000000000000, 0.000000000000000000 ) ) ;
#97175 = ORIENTED_EDGE ( 'NONE', *, *, #80694, .F. ) ;
#97176 = EDGE_CURVE ( 'NONE', #90464, #19124, #14340, .T. ) ;
#97177 = DIRECTION ( 'NONE',  ( 0.000000000000000000, -1.000000000000000000, 0.000000000000000000 ) ) ;
#97178 = VERTEX_POINT ( 'NONE', #66053 ) ;
#97179 = CARTESIAN_POINT ( 'NONE',  ( 10.28624191511809371, 45.38549880562041494, -15.40779740156171762 ) ) ;
#97181 = EDGE_CURVE ( 'NONE', #48447, #31692, #72928, .T. ) ;
#97180 = AXIS2_PLACEMENT_3D ( 'NONE', #88906, #47373, #64634 ) ;
#97182 = DIRECTION ( 'NONE',  ( -1.000000000000000000, -1.224606353822377258E-16, -0.000000000000000000 ) ) ;
#97183 = CARTESIAN_POINT ( 'NONE',  ( -106.6622389571683129, -60.00000000000001421, 197.5332747654210266 ) ) ;
#97184 = CARTESIAN_POINT ( 'NONE',  ( -4.195612334302273538, -1.058759987296271632, 104.4881327927214159 ) ) ;
#97185 = CARTESIAN_POINT ( 'NONE',  ( -2.977408999572650039, -29.56250000204838813, -7.188101187500001821 ) ) ;
#97186 = DIRECTION ( 'NONE',  ( 0.000000000000000000, 0.000000000000000000, 1.000000000000000000 ) ) ;
#97187 = CIRCLE ( 'NONE', #47290, 5.000000000000000000 ) ;
#97188 = CARTESIAN_POINT ( 'NONE',  ( -12.15301166631102703, 17.45470153262807145, 8.961799035703435834 ) ) ;
#97189 = CARTESIAN_POINT ( 'NONE',  ( 1.000000000000000000, -51.23885339960735053, 3.814018968273865440 ) ) ;
#97190 = CARTESIAN_POINT ( 'NONE',  ( 2.617478844991759868, 50.00000000000001421, -94.73972676610910071 ) ) ;
#97191 = CARTESIAN_POINT ( 'NONE',  ( 12.37144696128342503, -4.000000000000004441, 20.44658103856077602 ) ) ;
#97192 = DIRECTION ( 'NONE',  ( 0.000000000000000000, -1.000000000000000000, 0.000000000000000000 ) ) ;
#97193 = CARTESIAN_POINT ( 'NONE',  ( 32.48141916466479984, 312.4572366807472577, -7.733776394823530964 ) ) ;
#97194 = COLOUR_RGB ( '', 0.31764706, 0.68627451, 0.89019608) ;
#97195 = CARTESIAN_POINT ( 'NONE',  ( -33.33496386269368372, -60.31377368949035400, 38.34004965045540558 ) ) ;
#97196 = ORIENTED_EDGE ( 'NONE', *, *, #1768, .F. ) ;
#97197 = CARTESIAN_POINT ( 'NONE',  ( -34.40527838988940346, 463.9171486810813008, 5.550078836969805529 ) ) ;
#97198 = CARTESIAN_POINT ( 'NONE',  ( 41.52545057012824969, -22.24250618979461791, 35.91399818572732983 ) ) ;
#97199 = CARTESIAN_POINT ( 'NONE',  ( 13.60704923275372202, -1.734723475976807094E-15, 10.45706415777666365 ) ) ;
#97200 = EDGE_LOOP ( 'NONE', ( #81347, #11427, #82785, #62374, #85048, #101409 ) ) ;
#97201 = CARTESIAN_POINT ( 'NONE',  ( 6.585468679846620432, -3.617797563910811753, 6.733790807807554124 ) ) ;
#97202 = CARTESIAN_POINT ( 'NONE',  ( -57.79103112299724643, -38.34425813298624064, 89.61988761945933391 ) ) ;
#97203 = ORIENTED_EDGE ( 'NONE', *, *, #16762, .F. ) ;
#97205 = CARTESIAN_POINT ( 'NONE',  ( -31.21759734847655210, 387.2566916973277671, 24.99345285570965913 ) ) ;
#97204 = CARTESIAN_POINT ( 'NONE',  ( 6.746887896522141936, -3.895317543249906755, -6.526184258131190852 ) ) ;
#97206 = DIRECTION ( 'NONE',  ( 0.000000000000000000, -1.000000000000000000, 0.000000000000000000 ) ) ;
#97207 = CARTESIAN_POINT ( 'NONE',  ( 5.996380728651201863, 2.731133088746455329, 6.499999999999997335 ) ) ;
#97208 = FACE_OUTER_BOUND ( 'NONE', #49546, .T. ) ;
#97209 = DIRECTION ( 'NONE',  ( 0.000000000000000000, -1.000000000000000000, 0.000000000000000000 ) ) ;
#97210 = CARTESIAN_POINT ( 'NONE',  ( 4.567209634097050497, -85.93599786085513870, -3.891254717191802381 ) ) ;
#97211 = PRESENTATION_STYLE_ASSIGNMENT (( #47063 ) ) ;
#97212 = CARTESIAN_POINT ( 'NONE',  ( 95.41688625546588298, -60.00000000000000711, 52.01396517246381279 ) ) ;
#97213 = CARTESIAN_POINT ( 'NONE',  ( -44.12472801210822837, 485.7238370326490440, 3.975897585127398770 ) ) ;
#97214 = LINE ( 'NONE', #21781, #97369 ) ;
#97215 = CARTESIAN_POINT ( 'NONE',  ( -33.84761347220297267, 488.7471039746335464, 11.01988148152531899 ) ) ;
#97216 = ORIENTED_EDGE ( 'NONE', *, *, #95863, .T. ) ;
#97217 = EDGE_CURVE ( 'NONE', #56644, #43338, #103969, .T. ) ;
#97218 = B_SPLINE_CURVE_WITH_KNOTS ( 'NONE', 3,
 ( #74031, #82664, #43272, #99349, #58932, #25533, #8766, #24470, #67556, #42736, #75627, #90223, #58388, #91304, #24984, #16328, #1730, #41672, #33083, #66475, #65948, #100434, #92339, #17414, #98827, #74561, #50287, #59471, #33601, #50807, #83189, #18484, #42198, #75081, #1174, #51347, #34145, #8236, #84260, #67023, #57836, #90762, #99903, #35203, #26074, #91828, #17945, #57305, #16878, #4402, #12475, #45409 ),
 .UNSPECIFIED., .F., .F.,
 ( 4, 2, 2, 2, 2, 2, 2, 2, 2, 2, 2, 2, 2, 2, 2, 2, 2, 2, 2, 2, 2, 2, 2, 2, 2, 4 ),
 ( 0.0004915406311061616337, 0.01833906179314000878, 0.02726282237415693019, 0.03618658295517385159, 0.05403410411720769441, 0.06295786469822470255, 0.07188162527924170375, 0.08972914644127570616, 0.09865290702229272124, 0.1075766676033097224, 0.1120385478938182994, 0.1165004281843268902, 0.1209623084748354810, 0.1254241887653440579, 0.1298860690558526487, 0.1321170092011069441, 0.1343479493463612395, 0.1354634194189883734, 0.1365788894916155349, 0.1376943595642426688, 0.1382520946005562912, 0.1388098296368699136, 0.1399252997094971862, 0.1410407697821244311, 0.1421562398547517037, 0.1432717099273789485 ),
 .UNSPECIFIED. ) ;
#97219 = AXIS2_PLACEMENT_3D ( 'NONE', #79033, #5153, #39122 ) ;
#97220 = CARTESIAN_POINT ( 'NONE',  ( -56.65595402317139673, -29.99999999999999289, 59.14054006920170536 ) ) ;
#97221 = EDGE_LOOP ( 'NONE', ( #22610, #104488, #52515, #97473 ) ) ;
#97222 = CARTESIAN_POINT ( 'NONE',  ( -15.86714682456782377, 3.932109987709613286, 3.945841262972282326 ) ) ;
#97223 = CARTESIAN_POINT ( 'NONE',  ( 9.300358455900566312, 11.36566808887731739, -9.192885337679628000E-13 ) ) ;
#97224 = DIRECTION ( 'NONE',  ( 0.000000000000000000, 1.000000000000000000, 0.000000000000000000 ) ) ;
#97225 = CARTESIAN_POINT ( 'NONE',  ( -23.21751746555280249, 27.38103382803677022, -33.20617127781034839 ) ) ;
#97226 = CARTESIAN_POINT ( 'NONE',  ( 7.188101187500001821, -22.43750000204838813, -2.977408999572650483 ) ) ;
#97228 = EDGE_CURVE ( 'NONE', #25041, #38206, #50384, .T. ) ;
#97227 = LINE ( 'NONE', #56214, #103573 ) ;
#97229 = FILL_AREA_STYLE_COLOUR ( '', #2303 ) ;
#97230 = ADVANCED_FACE ( 'NONE', ( #75190 ), #52302, .T. ) ;
#97231 = CARTESIAN_POINT ( 'NONE',  ( 7.316989716473759842, 41.06054036619742220, -70.27553886509497261 ) ) ;
#97232 = EDGE_LOOP ( 'NONE', ( #17561, #16321, #4220, #17082 ) ) ;
#97233 = MECHANICAL_DESIGN_GEOMETRIC_PRESENTATION_REPRESENTATION (  '', ( #18028 ), #35291 ) ;
#97234 =( GEOMETRIC_REPRESENTATION_CONTEXT ( 3 ) GLOBAL_UNCERTAINTY_ASSIGNED_CONTEXT ( ( #44015 ) ) GLOBAL_UNIT_ASSIGNED_CONTEXT ( ( #104759, #8186, #49707 ) ) REPRESENTATION_CONTEXT ( 'NONE', 'WORKASPACE' ) );
#97235 = CIRCLE ( 'NONE', #69690, 5.000000000000000000 ) ;
#97237 = EDGE_LOOP ( 'NONE', ( #79712, #36826, #95510, #5929, #72269 ) ) ;
#97236 = DIRECTION ( 'NONE',  ( 0.000000000000000000, 1.000000000000000000, 0.000000000000000000 ) ) ;
#97238 = CARTESIAN_POINT ( 'NONE',  ( 78.52592673875363971, -60.31111541565864798, 160.5468623774698926 ) ) ;
#97239 = CARTESIAN_POINT ( 'NONE',  ( -38.31422226540048115, 27.60041950521512533, -11.19138753273245257 ) ) ;
#97240 = ORIENTED_EDGE ( 'NONE', *, *, #97418, .F. ) ;
#97241 = DIRECTION ( 'NONE',  ( -1.000000000000000000, -1.224606353822377258E-16, -0.000000000000000000 ) ) ;
#97242 = CARTESIAN_POINT ( 'NONE',  ( -1.106745437108234142, 17.28904319046834459, -49.90271519190591931 ) ) ;
#97243 = CARTESIAN_POINT ( 'NONE',  ( 4.401442555609581635E-16, -14.28125000204838457, -7.188101187500000044 ) ) ;
#97244 = CARTESIAN_POINT ( 'NONE',  ( 7.744991119775241017, 26.53561214574870064, -2.016316005557097224 ) ) ;
#97245 = AXIS2_PLACEMENT_3D ( 'NONE', #30554, #63453, #98315 ) ;
#97246 = CARTESIAN_POINT ( 'NONE',  ( -66.37944403907447111, -57.68041551771388953, 132.8370836190597686 ) ) ;
#97247 = CARTESIAN_POINT ( 'NONE',  ( 16.16318061117915050, 302.5659895892079021, 9.876333854622428632 ) ) ;
#97248 = ADVANCED_FACE ( 'NONE', ( #93535 ), #62248, .T. ) ;
#97249 = EDGE_LOOP ( 'NONE', ( #88527, #23028, #5675, #21137 ) ) ;
#97250 = SURFACE_SIDE_STYLE ('',( #89171 ) ) ;
#97251 = DIRECTION ( 'NONE',  ( -1.000000000000000000, -0.000000000000000000, -0.000000000000000000 ) ) ;
#97252 = DIRECTION ( 'NONE',  ( 0.000000000000000000, 1.000000000000000000, 0.000000000000000000 ) ) ;
#97253 = CARTESIAN_POINT ( 'NONE',  ( -8.000000000000000000, -19.24999999999999289, -9.797174393178825657E-16 ) ) ;
#97254 =( NAMED_UNIT ( * ) SI_UNIT ( $, .STERADIAN. ) SOLID_ANGLE_UNIT ( ) );
#97255 = EDGE_CURVE ( 'NONE', #37427, #5773, #98800, .T. ) ;
#97256 = ORIENTED_EDGE ( 'NONE', *, *, #59770, .F. ) ;
#97257 = CARTESIAN_POINT ( 'NONE',  ( 8.000000000000000000, -14.09375000409676915, -3.313708498984761608 ) ) ;
#97258 = CARTESIAN_POINT ( 'NONE',  ( -34.55953967696941476, -23.85835632124947736, 33.33342719774777407 ) ) ;
#97259 = CARTESIAN_POINT ( 'NONE',  ( -38.17429156479857255, 491.0342884836515509, 12.03746475763302293 ) ) ;
#97260 = DIRECTION ( 'NONE',  ( -1.000000000000000000, -0.000000000000000000, -0.000000000000000000 ) ) ;
#97261 = CARTESIAN_POINT ( 'NONE',  ( -9.333079356992097786, 86.77833080074870509, 3.592383266237784589 ) ) ;
#97262 = FACE_OUTER_BOUND ( 'NONE', #98309, .T. ) ;
#97263 = PRODUCT_CONTEXT ( 'NONE', #16230, 'mechanical' ) ;
#97264 = CARTESIAN_POINT ( 'NONE',  ( -7.163135071507197971, -15.11851566007659464, 14.95876950282627327 ) ) ;
#97265 = ORIENTED_EDGE ( 'NONE', *, *, #94348, .T. ) ;
#97266 = CARTESIAN_POINT ( 'NONE',  ( -4.770986019692863955, -47.38877792675871348, 40.36182486515247803 ) ) ;
#97267 = CARTESIAN_POINT ( 'NONE',  ( -33.21102376836597614, 438.9613914113129454, 23.92328486949907074 ) ) ;
#97268 = CARTESIAN_POINT ( 'NONE',  ( 8.099999999999999645, 3.752776749732562589, -6.500000000000000888 ) ) ;
#97269 = CARTESIAN_POINT ( 'NONE',  ( -56.61081697993206774, -29.99999999999999289, 59.00319635214307112 ) ) ;
#97270 = ADVANCED_FACE ( 'NONE', ( #28839 ), #57451, .T. ) ;
#97271 = DIRECTION ( 'NONE',  ( -1.000000000000000000, -0.000000000000000000, -0.000000000000000000 ) ) ;
#97272 = ORIENTED_EDGE ( 'NONE', *, *, #81833, .T. ) ;
#97273 = DIRECTION ( 'NONE',  ( 0.000000000000000000, -1.000000000000000000, 0.000000000000000000 ) ) ;
#97274 = CARTESIAN_POINT ( 'NONE',  ( 101.8386296196878504, -57.63167174066484932, 203.3325908020501913 ) ) ;
#97275 = CARTESIAN_POINT ( 'NONE',  ( 35.47699217159722451, 463.6829005663142311, 19.36631617874163780 ) ) ;
#97276 = DIRECTION ( 'NONE',  ( 0.000000000000000000, -1.000000000000000000, 0.000000000000000000 ) ) ;
#97277 = CARTESIAN_POINT ( 'NONE',  ( -6.488032186737915374, 53.47822873620448547, 7.647501018148323837 ) ) ;
#97278 = CARTESIAN_POINT ( 'NONE',  ( -75.06267738998585060, -60.00000000000000000, 181.7393887267853074 ) ) ;
#97279 = CARTESIAN_POINT ( 'NONE',  ( -32.16694665535142406, 298.7751107022914425, -9.134474995491629556 ) ) ;
#97280 = CARTESIAN_POINT ( 'NONE',  ( -2.352990130084491319E-16, 7.505553499465148271, -6.064240316920404439 ) ) ;
#97281 = CARTESIAN_POINT ( 'NONE',  ( -29.07128654445882887, 296.9339959557834163, -9.548856946221640385 ) ) ;
#97282 = CARTESIAN_POINT ( 'NONE',  ( -85.45145498079543245, -39.29912314789010708, 185.3035127737040000 ) ) ;
#97283 = ORIENTED_EDGE ( 'NONE', *, *, #49698, .F. ) ;
#97284 = CARTESIAN_POINT ( 'NONE',  ( 31.53716978815729988, 312.6643757245456641, -7.923975285009635883 ) ) ;
#97285 = ORIENTED_EDGE ( 'NONE', *, *, #88378, .F. ) ;
#97286 = CARTESIAN_POINT ( 'NONE',  ( 0.000000000000000000, -1.200000000000000030E-05, -7.749999999999999112 ) ) ;
#97287 = EDGE_CURVE ( 'NONE', #61806, #75040, #20755, .T. ) ;
#97289 = CARTESIAN_POINT ( 'NONE',  ( -5.625019081819782052, 41.66287055468434630, -70.61600276915974916 ) ) ;
#97288 = AXIS2_PLACEMENT_3D ( 'NONE', #20063, #27083, #59968 ) ;
#97290 = CARTESIAN_POINT ( 'NONE',  ( -82.31759468112190348, -37.78304723879290350, -13.10579271544666824 ) ) ;
#97291 = CARTESIAN_POINT ( 'NONE',  ( -42.20540931547679264, 464.9254549434355681, 14.73500713293386966 ) ) ;
#97292 = DIRECTION ( 'NONE',  ( 0.000000000000000000, 1.000000000000000000, 0.000000000000000000 ) ) ;
#97293 = ORIENTED_EDGE ( 'NONE', *, *, #7981, .F. ) ;
#97294 = CARTESIAN_POINT ( 'NONE',  ( -2.691566728956864996, -0.5366288636816407553, 103.4274024144617954 ) ) ;
#97295 = CARTESIAN_POINT ( 'NONE',  ( 10.72709311271703214, 18.42505693645571441, -9.330257298435006064 ) ) ;
#97296 = ADVANCED_FACE ( 'NONE', ( #70843 ), #27775, .T. ) ;
#97297 = CARTESIAN_POINT ( 'NONE',  ( 17.78317311658683408, 9.642355526980000143E-13, 13.66642973271509831 ) ) ;
#97298 = CARTESIAN_POINT ( 'NONE',  ( -37.54559764570181812, 464.1143081516144662, 19.43664670202813838 ) ) ;
#97299 = CARTESIAN_POINT ( 'NONE',  ( 86.47489896066092285, -14.21045842199428932, -14.67047700064687987 ) ) ;
#97300 = CARTESIAN_POINT ( 'NONE',  ( -73.95641269737396328, -53.38221346759030439, 126.4400680314501386 ) ) ;
#97301 = ORIENTED_EDGE ( 'NONE', *, *, #31070, .T. ) ;
#97302 = CARTESIAN_POINT ( 'NONE',  ( 34.32456002071940304, -30.00000000000004263, 42.48759634994703305 ) ) ;
#97303 = CARTESIAN_POINT ( 'NONE',  ( 23.58349330513380337, 1.593028355512270962E-15, 0.000000000000000000 ) ) ;
#97304 = CARTESIAN_POINT ( 'NONE',  ( 83.66466658337685658, -57.54292938958637649, 201.5661420244404098 ) ) ;
#97305 = CARTESIAN_POINT ( 'NONE',  ( 28.09805714684552314, 34.19617451435909317, 9.570894723979119334 ) ) ;
#97306 = AXIS2_PLACEMENT_3D ( 'NONE', #79117, #79641, #47790 ) ;
#97307 = CARTESIAN_POINT ( 'NONE',  ( 33.38428166833018196, 315.1392599553683453, -7.060717463013046924 ) ) ;
#97308 = CARTESIAN_POINT ( 'NONE',  ( -11.46409645960823021, 12.99999999999756994, 10.00000000000000178 ) ) ;
#97309 = ORIENTED_EDGE ( 'NONE', *, *, #10831, .T. ) ;
#97310 = FACE_OUTER_BOUND ( 'NONE', #43356, .T. ) ;
#97311 = EDGE_CURVE ( 'NONE', #83001, #25099, #3300, .T. ) ;
#97312 = EDGE_CURVE ( 'NONE', #35387, #40315, #12586, .T. ) ;
#97313 = CARTESIAN_POINT ( 'NONE',  ( -12.50000000000000178, 11.21173275031592809, -29.16573290955443909 ) ) ;
#97314 = CARTESIAN_POINT ( 'NONE',  ( 16.02260224162418112, 43.96096248673147500, 4.310921585563690428 ) ) ;
#97315 = CARTESIAN_POINT ( 'NONE',  ( -2.977408999572650039, -20.18750000204838457, -7.188101187500001821 ) ) ;
#97316 = CARTESIAN_POINT ( 'NONE',  ( 5.088535779738191600, -5.722386535631965643, -7.491772860716527482 ) ) ;
#97317 =( GEOMETRIC_REPRESENTATION_CONTEXT ( 3 ) GLOBAL_UNCERTAINTY_ASSIGNED_CONTEXT ( ( #84743 ) ) GLOBAL_UNIT_ASSIGNED_CONTEXT ( ( #47502, #34018, #25946 ) ) REPRESENTATION_CONTEXT ( 'NONE', 'WORKASPACE' ) );
#97318 = CARTESIAN_POINT ( 'NONE',  ( 9.842473135306409660, 81.41068182886414206, 1.785129593756284772 ) ) ;
#97319 = CARTESIAN_POINT ( 'NONE',  ( 5.500000018435954097, 42.00000000000000000, -68.91429207046174099 ) ) ;
#97320 = DIRECTION ( 'NONE',  ( 0.000000000000000000, -1.000000000000000000, 0.000000000000000000 ) ) ;
#97321 = CARTESIAN_POINT ( 'NONE',  ( 1.469576158976823750E-15, -80.00000000000000000, 15.00000000000000000 ) ) ;
#97322 = ORIENTED_EDGE ( 'NONE', *, *, #36927, .T. ) ;
#97323 = CARTESIAN_POINT ( 'NONE',  ( 96.28888888888889142, 4.172000000000019249, 5.109226446042768454E-16 ) ) ;
#97325 = CARTESIAN_POINT ( 'NONE',  ( 30.12050400343885670, -60.32946261704295665, 36.84871485504820754 ) ) ;
#97324 = CARTESIAN_POINT ( 'NONE',  ( -28.47812542966827110, -14.21045842199436926, 36.49899343628653270 ) ) ;
#97326 = CARTESIAN_POINT ( 'NONE',  ( 23.62741386766530383, 27.31466638971096472, -33.14007574073367124 ) ) ;
#97327 = ORIENTED_EDGE ( 'NONE', *, *, #77181, .F. ) ;
#97328 = ORIENTED_EDGE ( 'NONE', *, *, #10775, .T. ) ;
#97330 = CARTESIAN_POINT ( 'NONE',  ( 37.24013875201491430, 460.4840697668730058, 2.466806968993466853 ) ) ;
#97329 =( LENGTH_UNIT ( ) NAMED_UNIT ( * ) SI_UNIT ( .MILLI., .METRE. ) );
#97331 = DIRECTION ( 'NONE',  ( 1.000000000000000000, 0.000000000000000000, 0.000000000000000000 ) ) ;
#97332 = CARTESIAN_POINT ( 'NONE',  ( -43.72580207737490809, 464.6834397206225731, 7.653156261463578858 ) ) ;
#97333 = FILL_AREA_STYLE_COLOUR ( '', #13922 ) ;
#97334 = DIRECTION ( 'NONE',  ( 1.000000000000000000, 0.000000000000000000, 0.000000000000000000 ) ) ;
#97335 = ORIENTED_EDGE ( 'NONE', *, *, #25435, .F. ) ;
#97336 = CARTESIAN_POINT ( 'NONE',  ( 8.020137790548009349, -59.99999999999997868, -42.49116362023697491 ) ) ;
#97337 = CARTESIAN_POINT ( 'NONE',  ( 84.45351475738571878, -30.00000000000000711, 165.1268496781745228 ) ) ;
#97338 = DIRECTION ( 'NONE',  ( 0.000000000000000000, 0.000000000000000000, -1.000000000000000000 ) ) ;
#97339 = FILL_AREA_STYLE ('',( #64472 ) ) ;
#97340 = STYLED_ITEM ( 'NONE', ( #24994 ), #99188 ) ;
#97341 = DIRECTION ( 'NONE',  ( -0.000000000000000000, 1.000000000000000000, 0.000000000000000000 ) ) ;
#97342 = ORIENTED_EDGE ( 'NONE', *, *, #58280, .T. ) ;
#97343 = EDGE_CURVE ( 'NONE', #2814, #21525, #33389, .T. ) ;
#97344 = ORIENTED_EDGE ( 'NONE', *, *, #3115, .F. ) ;
#97345 = VERTEX_POINT ( 'NONE', #95132 ) ;
#97346 = CARTESIAN_POINT ( 'NONE',  ( 1.102447643272868261, 53.60738151370213700, 9.611086547314165784 ) ) ;
#97347 = CARTESIAN_POINT ( 'NONE',  ( 16.51905981272399870, 42.00139749746809059, -87.79004739960677739 ) ) ;
#97348 = CARTESIAN_POINT ( 'NONE',  ( -36.94533202345532885, 28.08661236372360293, 11.10948794531283212 ) ) ;
#97349 = CARTESIAN_POINT ( 'NONE',  ( 26.97704838610725631, 306.9562238369655915, 10.88316440979279776 ) ) ;
#97350 = CARTESIAN_POINT ( 'NONE',  ( -42.49116267755303511, 334.6731539865542686, 7.617589167841204656 ) ) ;
#97351 = CARTESIAN_POINT ( 'NONE',  ( -2.751797500100344518, -70.28872839323150856, 13.27139841227441686 ) ) ;
#97352 = SURFACE_STYLE_FILL_AREA ( #89286 ) ;
#97354 = EDGE_CURVE ( 'NONE', #7932, #79952, #28188, .T. ) ;
#97353 = CARTESIAN_POINT ( 'NONE',  ( 12.61650669486618881, 1.474610560812782335E-15, 0.000000000000000000 ) ) ;
#97355 = VERTEX_POINT ( 'NONE', #13113 ) ;
#97356 = CARTESIAN_POINT ( 'NONE',  ( 30.36467006388678769, 11.77175644674778354, 39.80053734054823167 ) ) ;
#97357 = ORIENTED_EDGE ( 'NONE', *, *, #71551, .T. ) ;
#97358 = CARTESIAN_POINT ( 'NONE',  ( 29.83349330513380337, 1.593028355512270567E-15, 0.000000000000000000 ) ) ;
#97359 = CARTESIAN_POINT ( 'NONE',  ( -52.56483885390523625, 48.00000000000000000, -38.23529411764706509 ) ) ;
#97360 = CARTESIAN_POINT ( 'NONE',  ( -41.97131279571158302, 485.5606288621841600, -4.070573943137918427 ) ) ;
#97361 = CARTESIAN_POINT ( 'NONE',  ( 6.936184427528457874, 0.000000000000000000, -8.605212085995399107 ) ) ;
#97362 = CARTESIAN_POINT ( 'NONE',  ( 67.81700998233858968, -49.90853710843107649, 100.7767112817635962 ) ) ;
#97364 = AXIS2_PLACEMENT_3D ( 'NONE', #50821, #83727, #98333 ) ;
#97363 = B_SPLINE_CURVE_WITH_KNOTS ( 'NONE', 3,
 ( #33340, #48419, #7961, #25252, #58111, #42461, #17673, #66749, #50020, #41932, #96062, #99635, #22194, #106118, #32271, #98045, #40872, #73761, #52146, #20384, #28446, #35479, #101767, #19839, #94218, #69419, #27933, #67814, #26864, #51614, #84534, #27403, #26338, #102300 ),
 .UNSPECIFIED., .F., .F.,
 ( 4, 2, 2, 2, 2, 2, 2, 2, 2, 2, 2, 2, 2, 2, 2, 2, 4 ),
 ( 0.01272238763756221823, 0.01351613129786393731, 0.01430987495816565813, 0.01510361861846737722, 0.01589736227876909630, 0.01669110593907081538, 0.01748484959937253447, 0.01827859325967425702, 0.01907233691997597264, 0.01986608058027769519, 0.02065982424057941080, 0.02145356790088112989, 0.02224731156118284550, 0.02304105522148456459, 0.02383479888178628020, 0.02462854254208799581, 0.02542228620238971143 ),
 .UNSPECIFIED. ) ;
#97365 = ORIENTED_EDGE ( 'NONE', *, *, #13566, .T. ) ;
#97366 = DIRECTION ( 'NONE',  ( 0.000000000000000000, 1.000000000000000000, 0.000000000000000000 ) ) ;
#97367 = CARTESIAN_POINT ( 'NONE',  ( -6.559876275494355369, 9.830169646080438639, 2.453497130494364686 ) ) ;
#97368 = EDGE_CURVE ( 'NONE', #78785, #26898, #37982, .T. ) ;
#97369 = VECTOR ( 'NONE', #87557, 1000.000000000000000 ) ;
#97370 = ORIENTED_EDGE ( 'NONE', *, *, #81227, .F. ) ;
#97371 = STYLED_ITEM ( 'NONE', ( #9251 ), #9496 ) ;
#97372 = CARTESIAN_POINT ( 'NONE',  ( 6.390056616433401615, 51.65448240894459531, -6.607212291912419211 ) ) ;
#97373 = CARTESIAN_POINT ( 'NONE',  ( -8.000000000000000000, -28.43750000409677270, -9.797174393178825657E-16 ) ) ;
#97374 = CIRCLE ( 'NONE', #6073, 4.000000000000000888 ) ;
#97375 = SURFACE_STYLE_FILL_AREA ( #29007 ) ;
#97376 = STYLED_ITEM ( 'NONE', ( #32203 ), #56902 ) ;
#97377 = CARTESIAN_POINT ( 'NONE',  ( 9.699121749566376849, 246.8233123972417786, 2.444499528233566199 ) ) ;
#97378 = CARTESIAN_POINT ( 'NONE',  ( 9.989690267985800176, 33.97444416594910876, -0.5238310916885827728 ) ) ;
#97379 = CIRCLE ( 'NONE', #18204, 1.999999999999999778 ) ;
#97380 = PRESENTATION_STYLE_ASSIGNMENT (( #14870 ) ) ;
#97381 = ORIENTED_EDGE ( 'NONE', *, *, #41896, .F. ) ;
#97382 = SURFACE_STYLE_USAGE ( .BOTH. , #55330 ) ;
#97383 = DIRECTION ( 'NONE',  ( 0.000000000000000000, 0.000000000000000000, -1.000000000000000000 ) ) ;
#97384 = CARTESIAN_POINT ( 'NONE',  ( 18.35737871519194897, -59.99999999999998579, 40.03727238643882202 ) ) ;
#97385 = CARTESIAN_POINT ( 'NONE',  ( -97.91306529131917102, -30.00000000000001066, 190.6200330007610830 ) ) ;
#97386 = DIRECTION ( 'NONE',  ( 0.000000000000000000, 5.412337245047638135E-13, 1.000000000000000000 ) ) ;
#97387 = CARTESIAN_POINT ( 'NONE',  ( 51.82355698883625195, -57.67687465298720184, 82.20230154831503455 ) ) ;
#97389 =( NAMED_UNIT ( * ) PLANE_ANGLE_UNIT ( ) SI_UNIT ( $, .RADIAN. ) );
#97388 = DIRECTION ( 'NONE',  ( 0.000000000000000000, -1.000000000000000000, 0.000000000000000000 ) ) ;
#97390 = CARTESIAN_POINT ( 'NONE',  ( 5.094487508937581843, -21.66492762252005733, -38.54749912668833645 ) ) ;
#97391 = CARTESIAN_POINT ( 'NONE',  ( 56.96666666666666856, 3.309500000000014541, 4.052968581778174646E-16 ) ) ;
#97392 = FILL_AREA_STYLE_COLOUR ( '', #46027 ) ;
#97393 =( NAMED_UNIT ( * ) SI_UNIT ( $, .STERADIAN. ) SOLID_ANGLE_UNIT ( ) );
#97394 = CARTESIAN_POINT ( 'NONE',  ( -25.28100474081467297, -60.00000000000000000, 41.24667794035808299 ) ) ;
#97395 = CARTESIAN_POINT ( 'NONE',  ( 12.15653237801438280, 10.26022287888880946, 9.623545464154791063 ) ) ;
#97396 = CARTESIAN_POINT ( 'NONE',  ( -86.82857037991892923, -24.34865412473423874, 185.7447558296186116 ) ) ;
#97397 = ORIENTED_EDGE ( 'NONE', *, *, #48658, .T. ) ;
#97398 = CARTESIAN_POINT ( 'NONE',  ( 17.50000000000567368, 49.98040874966400082, 61.78610620011910726 ) ) ;
#97399 = CARTESIAN_POINT ( 'NONE',  ( 5.656854249492378806, -12.68749999999999467, 5.656854249492381470 ) ) ;
#97400 = CARTESIAN_POINT ( 'NONE',  ( -12.39957699862355867, -39.47617499352052306, 30.52395290649034720 ) ) ;
#97401 = CARTESIAN_POINT ( 'NONE',  ( 25.21823338009918203, 1.482358050883964840E-15, 0.000000000000000000 ) ) ;
#97403 =( LENGTH_UNIT ( ) NAMED_UNIT ( * ) SI_UNIT ( .MILLI., .METRE. ) );
#97402 = CARTESIAN_POINT ( 'NONE',  ( -102.8242071241121494, -60.00000000000002132, 193.0618602036044251 ) ) ;
#97404 = EDGE_CURVE ( 'NONE', #93202, #80922, #36916, .T. ) ;
#97405 = VERTEX_POINT ( 'NONE', #29879 ) ;
#97406 = CARTESIAN_POINT ( 'NONE',  ( -7.500000000000007105, 11.33333333333400006, -68.91429205785459544 ) ) ;
#97407 = ADVANCED_FACE ( 'NONE', ( #101619 ), #78924, .T. ) ;
#97408 = CARTESIAN_POINT ( 'NONE',  ( -9.509302320691752186, -5.000000000000001776, -19.39567712392218368 ) ) ;
#97409 = CARTESIAN_POINT ( 'NONE',  ( 56.22793774957824553, 6.975173280561618775E-15, 0.000000000000000000 ) ) ;
#97410 = DIRECTION ( 'NONE',  ( 0.000000000000000000, 0.000000000000000000, 1.000000000000000000 ) ) ;
#97411 = EDGE_CURVE ( 'NONE', #56430, #57955, #62759, .T. ) ;
#97412 = CARTESIAN_POINT ( 'NONE',  ( -7.986468734911285949, -81.02686320276920640, 0.5341897780976099241 ) ) ;
#97413 = CARTESIAN_POINT ( 'NONE',  ( 73.19597753742192481, -59.99999999999999289, 164.2624391722602581 ) ) ;
#97414 = CARTESIAN_POINT ( 'NONE',  ( -30.95643954367146833, 313.8918926584737505, -7.857037206977866006 ) ) ;
#97415 = ORIENTED_EDGE ( 'NONE', *, *, #92939, .T. ) ;
#97416 = CARTESIAN_POINT ( 'NONE',  ( 44.12472801211155371, 485.7238370326410859, 3.975897585125152123 ) ) ;
#97417 = DIRECTION ( 'NONE',  ( 0.000000000000000000, 0.000000000000000000, 1.000000000000000000 ) ) ;
#97418 = EDGE_CURVE ( 'NONE', #92046, #673, #44448, .T. ) ;
#97420 = DIRECTION ( 'NONE',  ( 0.000000000000000000, -1.000000000000000000, 0.000000000000000000 ) ) ;
#97419 = CARTESIAN_POINT ( 'NONE',  ( 17.10696384799877379, -59.99999999999999289, 42.25337809451749393 ) ) ;
#97421 = DIRECTION ( 'NONE',  ( -1.000000000000000000, 0.000000000000000000, 0.000000000000000000 ) ) ;
#97422 = CARTESIAN_POINT ( 'NONE',  ( -4.188755055078491552, -1.571875576994959278, 102.8981131900555113 ) ) ;
#97423 = EDGE_LOOP ( 'NONE', ( #98641, #64757, #57011, #90750, #34464, #3749 ) ) ;
#97424 = EDGE_CURVE ( 'NONE', #16452, #19990, #61168, .T. ) ;
#97425 = CARTESIAN_POINT ( 'NONE',  ( -29.62245443890884644, 328.1031406420239023, 15.64580783456615976 ) ) ;
#97426 = ORIENTED_EDGE ( 'NONE', *, *, #83507, .T. ) ;
#97427 = CARTESIAN_POINT ( 'NONE',  ( 3.572352985695675276, 15.21714514899109894, 9.341953373613073097 ) ) ;
#97428 = DIRECTION ( 'NONE',  ( -0.8191520442889974607, 0.000000000000000000, -0.5735764363510380548 ) ) ;
#97429 = CARTESIAN_POINT ( 'NONE',  ( 79.82022815836235452, 1.016364837396684119E-14, 0.000000000000000000 ) ) ;
#97430 = VERTEX_POINT ( 'NONE', #2899 ) ;
#97431 = AXIS2_PLACEMENT_3D ( 'NONE', #32917, #33446, #49057 ) ;
#97432 = CARTESIAN_POINT ( 'NONE',  ( -23.38163988261910831, 48.00000000000000000, 60.94087333798633210 ) ) ;
#97433 = CARTESIAN_POINT ( 'NONE',  ( -114.3713164436567808, -59.99999999998046718, 179.7174110124658171 ) ) ;
#97434 = CARTESIAN_POINT ( 'NONE',  ( 43.90061006400386390, 485.1244223267523239, -0.3741013042735300553 ) ) ;
#97435 = CARTESIAN_POINT ( 'NONE',  ( 59.88169702972975017, -60.00000000000000000, 100.0279864558745970 ) ) ;
#97436 = DIRECTION ( 'NONE',  ( 0.000000000000000000, 1.000000000000000000, 0.000000000000000000 ) ) ;
#97437 = CARTESIAN_POINT ( 'NONE',  ( 1.219356500951631173, 25.50065391225449574, -39.81801105826245646 ) ) ;
#97439 = CARTESIAN_POINT ( 'NONE',  ( 17.67110049161424001, -29.03104148580605681, 29.02232790898393944 ) ) ;
#97438 = CARTESIAN_POINT ( 'NONE',  ( -109.3240689110004524, -30.00000000000000355, 163.9542341103382057 ) ) ;
#97440 = CARTESIAN_POINT ( 'NONE',  ( 82.65902591454842252, -38.00000000000001421, 4.571707806879225622 ) ) ;
#97441 = CARTESIAN_POINT ( 'NONE',  ( 0.7788225383843935257, 53.48454317400725699, -9.981205654210052458 ) ) ;
#97442 = CARTESIAN_POINT ( 'NONE',  ( -45.26055152525536585, -18.78576083745453573, 38.35371795687179741 ) ) ;
#97443 = CARTESIAN_POINT ( 'NONE',  ( -1.249019603477211415, 34.73419941383219367, -28.17738922607452778 ) ) ;
#97445 = B_SPLINE_CURVE_WITH_KNOTS ( 'NONE', 3,
 ( #11640, #102258, #61281, #29475 ),
 .UNSPECIFIED., .F., .F.,
 ( 4, 4 ),
 ( 8.069727767687917553E-17, 0.001738772145482940555 ),
 .UNSPECIFIED. ) ;
#97444 = CONICAL_SURFACE ( 'NONE', #7908, 5.000000000000010658, 0.9599310885968697082 ) ;
#97446 = ORIENTED_EDGE ( 'NONE', *, *, #19691, .F. ) ;
#97447 = CIRCLE ( 'NONE', #7910, 4.000000000000000888 ) ;
#97448 = CARTESIAN_POINT ( 'NONE',  ( 10.51296777078104050, 50.00000000000000000, -92.64705882352942012 ) ) ;
#97449 = PRESENTATION_LAYER_ASSIGNMENT (  '', '', ( #57873 ) ) ;
#97450 = CARTESIAN_POINT ( 'NONE',  ( 30.00000000000000000, 7.347880794884133541E-16, 6.000000000000012434 ) ) ;
#97451 = CARTESIAN_POINT ( 'NONE',  ( 0.4033376246892503292, 7.198601258566900363, -0.5316568767328675449 ) ) ;
#97452 = AXIS2_PLACEMENT_3D ( 'NONE', #9869, #83761, #100482 ) ;
#97453 = DIRECTION ( 'NONE',  ( -0.000000000000000000, -1.000000000000000000, -0.000000000000000000 ) ) ;
#97454 = CARTESIAN_POINT ( 'NONE',  ( 4.815811321232739139, -8.199232923026272601, 3.581116321197040708 ) ) ;
#97455 = CARTESIAN_POINT ( 'NONE',  ( 29.45362385905110969, 325.9253963054578662, 15.14270878922920716 ) ) ;
#97456 = ORIENTED_EDGE ( 'NONE', *, *, #77389, .T. ) ;
#97457 = CARTESIAN_POINT ( 'NONE',  ( 4.211261491273226909, -48.41319459705742645, 103.7733746176744347 ) ) ;
#97458 = EDGE_LOOP ( 'NONE', ( #99816, #62313, #74655, #82893, #42301, #84195, #27440, #26558 ) ) ;
#97459 = CARTESIAN_POINT ( 'NONE',  ( 102.8143635727166725, -29.99999999998916778, 197.6080321013283196 ) ) ;
#97460 = SURFACE_STYLE_USAGE ( .BOTH. , #80217 ) ;
#97461 = CARTESIAN_POINT ( 'NONE',  ( 6.236082931826281595, 41.88001976074639998, -59.13168102063718123 ) ) ;
#97462 = CIRCLE ( 'NONE', #37158, 5.000000000000010658 ) ;
#97463 = CARTESIAN_POINT ( 'NONE',  ( 92.40083123715065483, -30.00000000000000000, 102.5190540915925794 ) ) ;
#97464 = CARTESIAN_POINT ( 'NONE',  ( 7.344505440741524893, 102.5538107270129586, -3.175463080953002226 ) ) ;
#97465 = VERTEX_POINT ( 'NONE', #53069 ) ;
#97466 = ADVANCED_FACE ( 'NONE', ( #35859 ), #9393, .T. ) ;
#97467 = ORIENTED_EDGE ( 'NONE', *, *, #96878, .T. ) ;
#97468 = ORIENTED_EDGE ( 'NONE', *, *, #50831, .F. ) ;
#97469 = CARTESIAN_POINT ( 'NONE',  ( 0.000000000000000000, 41.79151656018385097, -22.55262289886175608 ) ) ;
#97470 = CARTESIAN_POINT ( 'NONE',  ( 22.20562253605685044, 26.05647078817540674, 31.21756717792845137 ) ) ;
#97471 = SURFACE_STYLE_USAGE ( .BOTH. , #99061 ) ;
#97472 = EDGE_CURVE ( 'NONE', #42880, #17716, #26483, .T. ) ;
#97473 = ORIENTED_EDGE ( 'NONE', *, *, #102694, .F. ) ;
#97474 = EDGE_LOOP ( 'NONE', ( #18169, #75216, #98413, #23663 ) ) ;
#97475 = DIRECTION ( 'NONE',  ( 0.000000000000000000, -1.000000000000000000, 0.000000000000000000 ) ) ;
#97476 = CARTESIAN_POINT ( 'NONE',  ( 77.82015756661967032, -38.55211276278178900, 187.6246246428004554 ) ) ;
#97477 = CARTESIAN_POINT ( 'NONE',  ( 12.60067755036020287, 9.254571314429075102, 9.287679252113578698 ) ) ;
#97478 = CARTESIAN_POINT ( 'NONE',  ( 60.26117253150567876, -38.00000000000000711, 72.16388681341805977 ) ) ;
#97479 = CARTESIAN_POINT ( 'NONE',  ( 37.64249068469757731, 314.2742867948412027, 14.64262686200194885 ) ) ;
#97480 = CARTESIAN_POINT ( 'NONE',  ( 9.956561055908812463, 45.46170052629870639, -15.37429631330344471 ) ) ;
#97481 = CARTESIAN_POINT ( 'NONE',  ( 3.400000000000000355, 0.000000000000000000, -8.000000000000000000 ) ) ;
#97482 = CIRCLE ( 'NONE', #27013, 56.32976553137783782 ) ;
#97483 = DIRECTION ( 'NONE',  ( 0.000000000000000000, 0.000000000000000000, 1.000000000000000000 ) ) ;
#97484 = CARTESIAN_POINT ( 'NONE',  ( -5.238409285680669214, -48.00301508172829301, 104.1169421774613824 ) ) ;
#97485 = CARTESIAN_POINT ( 'NONE',  ( -1.469576158976823947E-15, -10.06250000409677092, 8.000000000000000000 ) ) ;
#97486 = EDGE_CURVE ( 'NONE', #10296, #90150, #39429, .T. ) ;
#97487 = EDGE_LOOP ( 'NONE', ( #59229, #32746, #28979, #20587 ) ) ;
#97488 = CARTESIAN_POINT ( 'NONE',  ( 0.000000000000000000, -30.00000000000000000, 8.000000000000000000 ) ) ;
#97489 = CARTESIAN_POINT ( 'NONE',  ( -32.67001420327693495, 300.1801760985952683, 3.134090012117491497 ) ) ;
#97490 = CARTESIAN_POINT ( 'NONE',  ( -12.12055188808705708, -4.677944472895712913, -76.82403236456319462 ) ) ;
#97491 = CARTESIAN_POINT ( 'NONE',  ( 0.000000000000000000, 0.000000000000000000, 0.000000000000000000 ) ) ;
#97492 = CARTESIAN_POINT ( 'NONE',  ( -8.000000000000000000, -13.34374999999999467, -3.313708498984762496 ) ) ;
#97493 = DIRECTION ( 'NONE',  ( 0.000000000000000000, -1.000000000000000000, 0.000000000000000000 ) ) ;
#97494 = EDGE_CURVE ( 'NONE', #91137, #35268, #91888, .T. ) ;
#97495 = DIRECTION ( 'NONE',  ( 0.000000000000000000, 0.000000000000000000, -1.000000000000000000 ) ) ;
#97496 = ORIENTED_EDGE ( 'NONE', *, *, #101283, .T. ) ;
#97497 = CARTESIAN_POINT ( 'NONE',  ( 85.84491179312431086, -28.47452358815500872, 180.7459189754015085 ) ) ;
#97498 = ADVANCED_FACE ( 'NONE', ( #53852 ), #31706, .F. ) ;
#97499 = ORIENTED_EDGE ( 'NONE', *, *, #98009, .T. ) ;
#97500 = CARTESIAN_POINT ( 'NONE',  ( 95.55007516758162467, -57.67170984176614468, 37.60999171965882937 ) ) ;
#97501 = CARTESIAN_POINT ( 'NONE',  ( 36.87655955837854549, 438.2068510013161813, 3.933030107424686950 ) ) ;
#97502 = CARTESIAN_POINT ( 'NONE',  ( 4.250000000000000000, 0.000000000000000000, -10.00000000000000000 ) ) ;
#97503 = CARTESIAN_POINT ( 'NONE',  ( 4.250000000000000000, 0.000000000000000000, -4.814498510800145681 ) ) ;
#97504 = AXIS2_PLACEMENT_3D ( 'NONE', #102831, #13264, #53216 ) ;
#97505 = B_SPLINE_CURVE_WITH_KNOTS ( 'NONE', 3,
 ( #85510, #12127, #45057, #18670, #35389, #68257, #60191, #52054, #43977, #75806, #44517, #36463, #77940, #76864, #83894, #11589, #2973, #34855, #4050, #69329, #10007, #42914, #105394, #20821, #29426, #4583, #47672, #39085, #12651, #95717, #38556, #46623, #71963, #63891, #79520, #6687, #62303, #46109, #103277, #95194, #6152, #78462, #96780, #80568, #22911, #55748, #62825, #70381, #21327, #78991, #14775, #47145, #88682 ),
 .UNSPECIFIED., .F., .F.,
 ( 4, 2, 2, 2, 2, 2, 2, 2, 2, 2, 2, 2, 2, 2, 2, 2, 2, 2, 2, 2, 2, 2, 2, 2, 1, 2, 4 ),
 ( 0.0004461995168100071582, 0.01816948080801145810, 0.03589276209921291039, 0.05361604339041435574, 0.06247768403601508536, 0.07133932468161581497, 0.08020096532721653071, 0.08906260597281724645, 0.1067858872640188722, 0.1156475279096197406, 0.1200783482324201817, 0.1245091685552206229, 0.1267245787166209614, 0.1278322837973212001, 0.1289399888780214110, 0.1311553990394218605, 0.1333708092008223101, 0.1344785142815225487, 0.1355862193622227319, 0.1366939244429229705, 0.1378016295236231814, 0.1400170396850236032, 0.1411247447657238419, 0.1416785973060739334, 0.1419555235762489931, 0.1420939867113365507, 0.1422324498464240805 ),
 .UNSPECIFIED. ) ;
#97506 = CIRCLE ( 'NONE', #51011, 4.000000000000000888 ) ;
#97507 = CARTESIAN_POINT ( 'NONE',  ( -68.81967529573854847, -38.00000000000000711, 97.19646116308891237 ) ) ;
#97508 = CARTESIAN_POINT ( 'NONE',  ( -4.175893272573466319, -3.000000000000000000, -7.137815226411295733 ) ) ;
#97509 = CARTESIAN_POINT ( 'NONE',  ( 52.75515435479064763, -30.00000000000000355, 51.54203667234443031 ) ) ;
#97511 = CARTESIAN_POINT ( 'NONE',  ( -44.08840282922865583, 485.7747746244177165, 4.178803824087112595 ) ) ;
#97510 = CARTESIAN_POINT ( 'NONE',  ( 0.000000000000000000, 5.629165124598848102, 3.250000000000005329 ) ) ;
#97512 = ORIENTED_EDGE ( 'NONE', *, *, #84348, .T. ) ;
#97513 = FACE_OUTER_BOUND ( 'NONE', #47876, .T. ) ;
#97514 = CONICAL_SURFACE ( 'NONE', #11368, 4.000000000000000000, 0.9599310885968912466 ) ;
#97515 = CARTESIAN_POINT ( 'NONE',  ( -10.50000000000000000, -5.000000000000000000, -8.595933841506989026 ) ) ;
#97516 = CARTESIAN_POINT ( 'NONE',  ( -27.42575526752855808, 36.50017221940704815, -10.02597686312969572 ) ) ;
#97517 = CARTESIAN_POINT ( 'NONE',  ( 9.999999999999998224, 15.00000000000000000, -2.832769448823991188E-15 ) ) ;
#97518 = SURFACE_STYLE_USAGE ( .BOTH. , #6929 ) ;
#97519 =( GEOMETRIC_REPRESENTATION_CONTEXT ( 3 ) GLOBAL_UNCERTAINTY_ASSIGNED_CONTEXT ( ( #13753 ) ) GLOBAL_UNIT_ASSIGNED_CONTEXT ( ( #69387, #21914, #44582 ) ) REPRESENTATION_CONTEXT ( 'NONE', 'WORKASPACE' ) );
#97520 = CIRCLE ( 'NONE', #47635, 65.00000000000000000 ) ;
#97521 = AXIS2_PLACEMENT_3D ( 'NONE', #92254, #17870, #50213 ) ;
#97522 = CARTESIAN_POINT ( 'NONE',  ( 66.64570889441912982, -29.85741638960125144, -22.35595166279332346 ) ) ;
#97523 = AXIS2_PLACEMENT_3D ( 'NONE', #22267, #37931, #13063 ) ;
#97524 = VERTEX_POINT ( 'NONE', #96458 ) ;
#97525 = CARTESIAN_POINT ( 'NONE',  ( 32.33349330513379982, -7.703719777548943412E-31, 4.000000000000001776 ) ) ;
#97526 = AXIS2_PLACEMENT_3D ( 'NONE', #23961, #40626, #73512 ) ;
#97527 = CARTESIAN_POINT ( 'NONE',  ( -17.49999999999999645, 2.500000000000000444, 25.00000000000000000 ) ) ;
#97529 = CARTESIAN_POINT ( 'NONE',  ( -53.22631969426956999, -34.58940849159185404, -27.04708426754712036 ) ) ;
#97528 = CARTESIAN_POINT ( 'NONE',  ( 6.249999999999998224, -4.618802153517012954, -8.000000000000001776 ) ) ;
#97530 = ADVANCED_FACE ( 'NONE', ( #86782 ), #80240, .F. ) ;
#97531 = EDGE_LOOP ( 'NONE', ( #88303, #78111, #46910 ) ) ;
#97532 = AXIS2_PLACEMENT_3D ( 'NONE', #21659, #37852, #70715 ) ;
#97533 = ORIENTED_EDGE ( 'NONE', *, *, #18926, .T. ) ;
#97534 = EDGE_CURVE ( 'NONE', #43629, #66517, #76472, .T. ) ;
#97535 = ADVANCED_FACE ( 'NONE', ( #88362 ), #91965, .T. ) ;
#97536 = DIRECTION ( 'NONE',  ( -0.000000000000000000, -0.000000000000000000, -1.000000000000000000 ) ) ;
#97537 = CARTESIAN_POINT ( 'NONE',  ( -92.42151101069008234, -60.00000000000004263, -0.1434650216276215917 ) ) ;
#97538 = ORIENTED_EDGE ( 'NONE', *, *, #88367, .T. ) ;
#97539 = DIRECTION ( 'NONE',  ( 0.000000000000000000, 0.7456561006171790185, 0.6663309835302448914 ) ) ;
#97540 = CARTESIAN_POINT ( 'NONE',  ( 95.56019984581097049, -45.27097885572743508, 194.1693090572786957 ) ) ;
#97542 = CARTESIAN_POINT ( 'NONE',  ( -46.78648606410043698, 13.65508681559504112, 15.44775621776469698 ) ) ;
#97541 = DIRECTION ( 'NONE',  ( -1.000000000000000000, -1.224606353822377258E-16, -0.000000000000000000 ) ) ;
#97543 = ADVANCED_FACE ( 'NONE', ( #13913 ), #98863, .T. ) ;
#97544 = CARTESIAN_POINT ( 'NONE',  ( -82.82964344457306538, -36.02023518659409262, 162.7145647415955239 ) ) ;
#97545 = ORIENTED_EDGE ( 'NONE', *, *, #34229, .F. ) ;
#97546 = ADVANCED_FACE ( 'NONE', ( #72167 ), #82493, .F. ) ;
#97547 = EDGE_CURVE ( 'NONE', #105779, #50732, #73748, .T. ) ;
#97548 = EDGE_LOOP ( 'NONE', ( #30786, #105341, #100874, #79064, #35034 ) ) ;
#97549 = CIRCLE ( 'NONE', #54516, 4.000000000000000000 ) ;
#97550 = VERTEX_POINT ( 'NONE', #6893 ) ;
#97551 = DIRECTION ( 'NONE',  ( 0.000000000000000000, -1.000000000000000000, 0.000000000000000000 ) ) ;
#97552 = CARTESIAN_POINT ( 'NONE',  ( -5.988549711970257761, -14.40160760345779600, 14.13124080977631714 ) ) ;
#97553 = FILL_AREA_STYLE ('',( #71689 ) ) ;
#97554 = EDGE_LOOP ( 'NONE', ( #34264, #28558, #40274, #82658, #44109 ) ) ;
#97555 = CARTESIAN_POINT ( 'NONE',  ( -42.45852508623016774, 486.4193484895183701, 8.300531886066563558 ) ) ;
#97556 = CARTESIAN_POINT ( 'NONE',  ( -98.18081844100633759, 27.55047179872464724, -49.09040922050319011 ) ) ;
#97557 = SURFACE_STYLE_USAGE ( .BOTH. , #77690 ) ;
#97558 = CARTESIAN_POINT ( 'NONE',  ( -105.5530292394789882, -57.64680470462099038, 201.3003284212183246 ) ) ;
#97559 = CARTESIAN_POINT ( 'NONE',  ( -43.86560043478159088, 486.1043823555137919, 5.341761608528194039 ) ) ;
#97560 = FACE_OUTER_BOUND ( 'NONE', #102112, .T. ) ;
#97561 = CARTESIAN_POINT ( 'NONE',  ( -0.3345794276167288750, 26.06210933331781376, 38.29266687495983490 ) ) ;
#97562 = DIRECTION ( 'NONE',  ( 0.000000000000000000, -1.000000000000000000, 0.000000000000000000 ) ) ;
#97563 = CARTESIAN_POINT ( 'NONE',  ( -24.50860473033056053, -14.21045842199433018, -36.19504829128915446 ) ) ;
#97564 = CARTESIAN_POINT ( 'NONE',  ( -35.95074892501450847, -14.21045842199431242, 40.03088108345822604 ) ) ;
#97565 = CARTESIAN_POINT ( 'NONE',  ( -55.06617873199689228, -22.15486436616988186, 53.58246572885349224 ) ) ;
#97566 = CARTESIAN_POINT ( 'NONE',  ( 3.313708498984743844, -27.78124999999999645, 8.000000000000017764 ) ) ;
#97567 = VERTEX_POINT ( 'NONE', #41919 ) ;
#97568 = CARTESIAN_POINT ( 'NONE',  ( -94.99629163939333409, -37.68183183142493675, 193.0097866583948587 ) ) ;
#97569 = CARTESIAN_POINT ( 'NONE',  ( -2.524354896707237777E-26, 294.8518027762758038, -10.00000000000000178 ) ) ;
#97570 = ORIENTED_EDGE ( 'NONE', *, *, #92479, .F. ) ;
#97571 = CARTESIAN_POINT ( 'NONE',  ( 42.61140200160144786, 465.9030374194822457, 13.21253569360410829 ) ) ;
#97572 = AXIS2_PLACEMENT_3D ( 'NONE', #42855, #11002, #84916 ) ;
#97573 = CARTESIAN_POINT ( 'NONE',  ( 89.79343125311589802, -38.39299482666958596, -16.49077915764583224 ) ) ;
#97574 = DIRECTION ( 'NONE',  ( -0.000000000000000000, -1.000000000000000000, -0.000000000000000000 ) ) ;
#97575 = CARTESIAN_POINT ( 'NONE',  ( 0.000000000000000000, -4.999999999999999112, 8.000000000000000000 ) ) ;
#97576 = CARTESIAN_POINT ( 'NONE',  ( -12.03689052648907420, 294.5862333106543929, 9.880550891260135415 ) ) ;
#97577 = CARTESIAN_POINT ( 'NONE',  ( 0.000000000000000000, 0.000000000000000000, -8.000000000000000000 ) ) ;
#97578 = CARTESIAN_POINT ( 'NONE',  ( 80.71650499981790006, -30.00000000000000000, 138.4101816275387762 ) ) ;
#97579 = PLANE ( 'NONE',  #88947 ) ;
#97580 = CARTESIAN_POINT ( 'NONE',  ( -33.85195725564127400, 465.2464970902067307, 17.18122764674263436 ) ) ;
#97581 = CARTESIAN_POINT ( 'NONE',  ( -37.54639605868532470, 463.7795194819277640, 19.50795070292539179 ) ) ;
#97582 = FILL_AREA_STYLE ('',( #50110 ) ) ;
#97583 = ORIENTED_EDGE ( 'NONE', *, *, #76541, .F. ) ;
#97584 = ORIENTED_EDGE ( 'NONE', *, *, #25919, .F. ) ;
#97585 = CARTESIAN_POINT ( 'NONE',  ( 49.07992270265078361, -53.36225572876357148, 53.76467797184545105 ) ) ;
#97586 = VECTOR ( 'NONE', #13569, 1000.000000000000000 ) ;
#97587 = CARTESIAN_POINT ( 'NONE',  ( 6.907083959255992056, 41.55068448857264940, -58.85924345847777062 ) ) ;
#97588 = CONICAL_SURFACE ( 'NONE', #56236, 3.309500000000001663, 0.9599310885968770357 ) ;
#97589 = DIRECTION ( 'NONE',  ( -0.000000000000000000, -0.000000000000000000, -1.000000000000000000 ) ) ;
#97590 =( BOUNDED_SURFACE ( )  B_SPLINE_SURFACE ( 3, 2, ( 
 ( #60354, #45225, #95891 ),
 ( #45740, #38722, #70555 ),
 ( #103961, #5289, #29593 ),
 ( #72134, #20986, #80214 ),
 ( #78101, #61948, #38210 ),
 ( #103442, #54327, #30643 ),
 ( #79691, #62463, #14405 ),
 ( #71590, #37152, #46798 ),
 ( #87271, #94841, #104496 ),
 ( #102915, #78618, #105043 ),
 ( #63531, #4219, #88333 ),
 ( #6319, #47318, #54872 ),
 ( #64069, #30105, #5800 ),
 ( #96429, #62994, #22564 ),
 ( #29083, #53306, #95354 ),
 ( #13348, #53819, #55402 ),
 ( #21491, #39258, #87801 ),
 ( #13881, #22016, #4751 ),
 ( #46276, #31184, #86751 ),
 ( #20464, #12297, #70017 ) ),
 .UNSPECIFIED., .F., .F., .F. ) 
 B_SPLINE_SURFACE_WITH_KNOTS ( ( 4, 2, 2, 2, 2, 2, 2, 2, 2, 4 ),
 ( 3, 3 ),
 ( 0.04523211244313660867, 0.04749178741066553688, 0.04975146237819445816, 0.05088129986195892573, 0.05201113734572338637, 0.05427081231325231458, 0.05653048728078123586, 0.05879016224831016407, 0.06104983721583909229, 0.06330951218336801356 ),
 ( 0.000000000000000000, 1.000000000000000000 ),
 .UNSPECIFIED. ) 
 GEOMETRIC_REPRESENTATION_ITEM ( )  RATIONAL_B_SPLINE_SURFACE ( (
 ( 1.000000000000000000, 0.4978119256231663958, 1.000000000000000000),
 ( 1.000000000000000000, 0.4952435806854573741, 1.000000000000000000),
 ( 1.000000000000000000, 0.4926028278389767978, 1.000000000000000000),
 ( 1.000000000000000000, 0.4880840605303077839, 1.000000000000000000),
 ( 1.000000000000000000, 0.4861908647209867707, 1.000000000000000000),
 ( 1.000000000000000000, 0.4843174878990902377, 1.000000000000000000),
 ( 1.000000000000000000, 0.4838530966740423600, 1.000000000000000000),
 ( 1.000000000000000000, 0.4832976052536793188, 1.000000000000000000),
 ( 1.000000000000000000, 0.4832078365194457104, 1.000000000000000000),
 ( 1.000000000000000000, 0.4835465747219757637, 1.000000000000000000),
 ( 1.000000000000000000, 0.4845818995314541966, 1.000000000000000000),
 ( 1.000000000000000000, 0.4880562902870073105, 1.000000000000000000),
 ( 1.000000000000000000, 0.4905018916449791488, 1.000000000000000000),
 ( 1.000000000000000000, 0.4962841545783361896, 1.000000000000000000),
 ( 1.000000000000000000, 0.4995601523126184107, 1.000000000000000000),
 ( 1.000000000000000000, 0.5062178729972902635, 1.000000000000000000),
 ( 1.000000000000000000, 0.5096177700154203016, 1.000000000000000000),
 ( 1.000000000000000000, 0.5157644467808917277, 1.000000000000000000),
 ( 1.000000000000000000, 0.5185252516010817603, 1.000000000000000000),
 ( 1.000000000000000000, 0.5207636911093219689, 1.000000000000000000) ) ) 
 REPRESENTATION_ITEM ( '' )  SURFACE ( )  );
#97591 = EDGE_CURVE ( 'NONE', #58722, #79056, #676, .T. ) ;
#97592 = ORIENTED_EDGE ( 'NONE', *, *, #53495, .F. ) ;
#97593 = CARTESIAN_POINT ( 'NONE',  ( -103.1838665334889811, -38.42661002002991211, 199.0052621351852622 ) ) ;
#97594 = ORIENTED_EDGE ( 'NONE', *, *, #90378, .F. ) ;
#97595 = CARTESIAN_POINT ( 'NONE',  ( 28.30697985939074357, 34.24750371692589823, -8.453642661119904034 ) ) ;
#97596 = CARTESIAN_POINT ( 'NONE',  ( 110.3407746192199710, -38.35604946154091266, 158.5393008408863693 ) ) ;
#97597 = CARTESIAN_POINT ( 'NONE',  ( 11.99035031454962485, 8.175746249152963330, -8.773473083764660174 ) ) ;
#97598 = CARTESIAN_POINT ( 'NONE',  ( 30.00000000000000355, 461.8887775513396150, 11.55279652844105520 ) ) ;
#97600 = CARTESIAN_POINT ( 'NONE',  ( 99.88553850844114379, -45.28285284022323509, 130.2282180348674956 ) ) ;
#97599 = AXIS2_PLACEMENT_3D ( 'NONE', #77342, #13648, #5565 ) ;
#97601 = CONICAL_SURFACE ( 'NONE', #35683, 5.000000000000010658, 0.9599310885968697082 ) ;
#97602 = PRESENTATION_STYLE_ASSIGNMENT (( #15102 ) ) ;
#97604 = AXIS2_PLACEMENT_3D ( 'NONE', #3272, #35672, #91751 ) ;
#97603 = CARTESIAN_POINT ( 'NONE',  ( -34.72287390941859542, 327.1428504792561966, -4.289995664657297425 ) ) ;
#97605 = CARTESIAN_POINT ( 'NONE',  ( 98.72690313425520969, -60.00000000000001421, 202.2179184582266203 ) ) ;
#97606 = AXIS2_PLACEMENT_3D ( 'NONE', #2454, #11606, #99553 ) ;
#97607 = AXIS2_PLACEMENT_3D ( 'NONE', #62294, #101281, #61770 ) ;
#97608 = CARTESIAN_POINT ( 'NONE',  ( 28.17977184163764193, 1.482358050883964840E-15, 0.000000000000000000 ) ) ;
#97609 = ADVANCED_FACE ( 'NONE', ( #888 ), #102291, .T. ) ;
#97610 = ORIENTED_EDGE ( 'NONE', *, *, #65922, .T. ) ;
#97611 = CARTESIAN_POINT ( 'NONE',  ( 57.41795923026059967, -39.49217349359543761, 65.75899213438894719 ) ) ;
#97612 = CARTESIAN_POINT ( 'NONE',  ( -30.89844457542884015, 298.0228418896831499, -9.303756596353716546 ) ) ;
#97613 = CARTESIAN_POINT ( 'NONE',  ( 9.960763185286923616, -50.12841120676987572, 26.07764662560745705 ) ) ;
#97614 = CARTESIAN_POINT ( 'NONE',  ( -7.016701986871722418, -4.999999999999999112, -15.40549185441076396 ) ) ;
#97615 = EDGE_LOOP ( 'NONE', ( #15736, #94940, #13474, #32120 ) ) ;
#97617 = CARTESIAN_POINT ( 'NONE',  ( -9.728280252476675827, -50.82205733719180785, 24.67413300948206967 ) ) ;
#97616 = CARTESIAN_POINT ( 'NONE',  ( -88.77003120989235185, -38.37858000208290576, -18.43781038091345081 ) ) ;
#97618 = CARTESIAN_POINT ( 'NONE',  ( 7.791781413346524410, -3.000000000000000444, 2.093983074874241623 ) ) ;
#97619 = CARTESIAN_POINT ( 'NONE',  ( 31.35596682365711274, 438.0939828603570732, 22.55458131664589061 ) ) ;
#97620 = DIRECTION ( 'NONE',  ( -1.000000000000000000, -1.224606353822377258E-16, -0.000000000000000000 ) ) ;
#97621 = CARTESIAN_POINT ( 'NONE',  ( -8.000000000000000000, -32.74999999999999289, -9.797174393178825657E-16 ) ) ;
#97622 = CARTESIAN_POINT ( 'NONE',  ( 38.58349330513380693, -4.000000000000000000, 4.898587196589415787E-16 ) ) ;
#97623 = EDGE_CURVE ( 'NONE', #62753, #95206, #86987, .T. ) ;
#97624 = DIRECTION ( 'NONE',  ( -1.000000000000000000, -1.224606353822377258E-16, -0.000000000000000000 ) ) ;
#97625 = ORIENTED_EDGE ( 'NONE', *, *, #6584, .F. ) ;
#97626 = CARTESIAN_POINT ( 'NONE',  ( 81.99978726385299410, -53.51631961905815160, 181.3751107682264490 ) ) ;
#97627 = ADVANCED_FACE ( 'NONE', ( #68883 ), #5871, .F. ) ;
#97629 = AXIS2_PLACEMENT_3D ( 'NONE', #33667, #57903, #15866 ) ;
#97628 = CARTESIAN_POINT ( 'NONE',  ( 4.551587301587293410, -48.79941684889506348, 104.4018401814738013 ) ) ;
#97630 = CARTESIAN_POINT ( 'NONE',  ( 36.80384673170812704, 28.12620022927966801, 11.20205233349968843 ) ) ;
#97631 = ORIENTED_EDGE ( 'NONE', *, *, #88311, .F. ) ;
#97632 = CARTESIAN_POINT ( 'NONE',  ( 6.289692432696784685, 1.244805614057421469E-13, 6.828989928337167115 ) ) ;
#97633 = CARTESIAN_POINT ( 'NONE',  ( 7.468840097761512808, -3.123202671104334360, -19.53083092318933822 ) ) ;
#97634 = CARTESIAN_POINT ( 'NONE',  ( 26.34381013455766052, 35.00016137052017484, -7.801548275680215916 ) ) ;
#97635 = CARTESIAN_POINT ( 'NONE',  ( 14.11595029532508860, 2.410436752314647713, 5.024000119269133258 ) ) ;
#97636 = CARTESIAN_POINT ( 'NONE',  ( -43.54556210147816842, 41.43866363024021382, -50.63474964717280358 ) ) ;
#97637 = AXIS2_PLACEMENT_3D ( 'NONE', #11639, #9506, #3571 ) ;
#97638 = CARTESIAN_POINT ( 'NONE',  ( -44.19066549755412865, 435.2576907183107551, 14.58870676253298804 ) ) ;
#97639 = ORIENTED_EDGE ( 'NONE', *, *, #51266, .T. ) ;
#97640 = B_SPLINE_CURVE_WITH_KNOTS ( 'NONE', 3,
 ( #19999, #19465, #45824, #86825 ),
 .UNSPECIFIED., .F., .F.,
 ( 4, 4 ),
 ( 9.511364005193116742E-18, 0.001259908249732733529 ),
 .UNSPECIFIED. ) ;
#97641 = CARTESIAN_POINT ( 'NONE',  ( 7.045755811259133417, 106.3034160301355513, 3.790843699961855773 ) ) ;
#97642 = DIRECTION ( 'NONE',  ( 1.000000000000000000, 0.000000000000000000, 0.000000000000000000 ) ) ;
#97644 = CARTESIAN_POINT ( 'NONE',  ( -11.00659270837914683, 16.89444621032363969, -9.217848032971012628 ) ) ;
#97643 = CARTESIAN_POINT ( 'NONE',  ( -22.00283802693145674, -27.01760079402097503, 37.33722609614333265 ) ) ;
#97645 = CARTESIAN_POINT ( 'NONE',  ( -7.188101187500000044, -15.40625000204838635, -8.802885111219163269E-16 ) ) ;
#97646 = CARTESIAN_POINT ( 'NONE',  ( -29.32938745888669274, 18.70033273455118916, -39.65510828929056686 ) ) ;
#97647 = SURFACE_STYLE_USAGE ( .BOTH. , #56660 ) ;
#97648 = CIRCLE ( 'NONE', #47688, 4.000000000000001776 ) ;
#97649 = CIRCLE ( 'NONE', #73481, 4.000000000000000888 ) ;
#97650 = ORIENTED_EDGE ( 'NONE', *, *, #98100, .F. ) ;
#97651 = DIRECTION ( 'NONE',  ( 0.000000000000000000, 1.000000000000000000, 0.000000000000000000 ) ) ;
#97652 = CARTESIAN_POINT ( 'NONE',  ( 23.21751746555303342, 25.98869614573808207, 30.70617127781016720 ) ) ;
#97653 = CARTESIAN_POINT ( 'NONE',  ( -7.844405524230078086, 79.54154322733928950, -4.999999999994920508 ) ) ;
#97654 = B_SPLINE_CURVE_WITH_KNOTS ( 'NONE', 3,
 ( #71177, #80315, #63099, #39365, #64173, #23184, #15058, #100756, #9613, #91103 ),
 .UNSPECIFIED., .F., .F.,
 ( 4, 2, 2, 2, 4 ),
 ( 1.155223362816825029E-19, 0.001989602278884367026, 0.003979204557768734052, 0.005968806836653101078, 0.007958409115537469838 ),
 .UNSPECIFIED. ) ;
#97655 = DIRECTION ( 'NONE',  ( -1.000000000000000000, -0.000000000000000000, -0.000000000000000000 ) ) ;
#97656 = CARTESIAN_POINT ( 'NONE',  ( 5.416666666666665186, 4.378239541354655984, -5.848636054922034866 ) ) ;
#97657 = ORIENTED_EDGE ( 'NONE', *, *, #52053, .F. ) ;
#97658 = FILL_AREA_STYLE_COLOUR ( '', #82522 ) ;
#97659 = EDGE_CURVE ( 'NONE', #101395, #103450, #21405, .T. ) ;
#97660 = CARTESIAN_POINT ( 'NONE',  ( 28.86650669486618881, 1.474610560812782335E-15, 0.000000000000000000 ) ) ;
#97661 = CONICAL_SURFACE ( 'NONE', #59828, 23.23666318551310539, 1.221730476396026388 ) ;
#97662 = ORIENTED_EDGE ( 'NONE', *, *, #20474, .F. ) ;
#97663 = ADVANCED_FACE ( 'NONE', ( #44603 ), #9541, .F. ) ;
#97664 = FACE_OUTER_BOUND ( 'NONE', #85433, .T. ) ;
#97665 = DIRECTION ( 'NONE',  ( -0.000000000000000000, -1.000000000000000000, -0.000000000000000000 ) ) ;
#97666 = UNCERTAINTY_MEASURE_WITH_UNIT (LENGTH_MEASURE( 1.000000000000000082E-05 ), #85512, 'distance_accuracy_value', 'NONE');
#97667 = CARTESIAN_POINT ( 'NONE',  ( -108.6743357863307011, -60.00000000000000711, 133.6544377956901997 ) ) ;
#97668 = CIRCLE ( 'NONE', #47711, 1.000000000000024203 ) ;
#97669 = PRESENTATION_LAYER_ASSIGNMENT (  '', '', ( #40790 ) ) ;
#97670 = CARTESIAN_POINT ( 'NONE',  ( 28.58254312158936727, 16.23466659877848528, -41.45958612840302493 ) ) ;
#97671 = DIRECTION ( 'NONE',  ( 0.000000000000000000, 0.4999999999999991673, -0.8660254037844390407 ) ) ;
#97672 = VECTOR ( 'NONE', #81253, 1000.000000000000000 ) ;
#97673 = LINE ( 'NONE', #82015, #24335 ) ;
#97674 = DIRECTION ( 'NONE',  ( 0.3968475291348042555, -0.1146398630990779210, 0.9106973923363488321 ) ) ;
#97676 = CARTESIAN_POINT ( 'NONE',  ( -5.929271424378248057, 41.34548848424987000, -58.36914649109142772 ) ) ;
#97675 = CARTESIAN_POINT ( 'NONE',  ( 2.617478844991767861, -5.000000000000002665, -75.26027323389092771 ) ) ;
#97677 = CARTESIAN_POINT ( 'NONE',  ( -84.06399816896501420, -35.95112890273957618, 174.2808740462292576 ) ) ;
#97678 = VERTEX_POINT ( 'NONE', #59186 ) ;
#97679 = FILL_AREA_STYLE ('',( #56137 ) ) ;
#97680 = EDGE_CURVE ( 'NONE', #43584, #92586, #18208, .T. ) ;
#97681 = ORIENTED_EDGE ( 'NONE', *, *, #87583, .F. ) ;
#97682 = ORIENTED_EDGE ( 'NONE', *, *, #56763, .T. ) ;
#97683 = CIRCLE ( 'NONE', #42572, 5.000000000000001776 ) ;
#97684 = FACE_OUTER_BOUND ( 'NONE', #67853, .T. ) ;
#97685 = EDGE_CURVE ( 'NONE', #80260, #4508, #7564, .T. ) ;
#97686 = CYLINDRICAL_SURFACE ( 'NONE', #64611, 5.000000000000000888 ) ;
#97687 = CARTESIAN_POINT ( 'NONE',  ( 41.85000000000000142, 1.533819458162526451E-15, 0.000000000000000000 ) ) ;
#97688 = CARTESIAN_POINT ( 'NONE',  ( 9.518114776853952463, 9.451441023381173423, 3.089571038418899033E-13 ) ) ;
#97689 = CARTESIAN_POINT ( 'NONE',  ( -4.692623589391090810, -5.000000000000000000, -97.18000954721273388 ) ) ;
#97690 = CARTESIAN_POINT ( 'NONE',  ( 27.61650669486618881, 1.474610560812782335E-15, 0.000000000000000000 ) ) ;
#97691 = CARTESIAN_POINT ( 'NONE',  ( 113.3390500081078613, -59.99999999999998579, 187.7085336688584221 ) ) ;
#97692 = CARTESIAN_POINT ( 'NONE',  ( -105.8602000712061368, -14.21045842199440656, 153.6005699772977096 ) ) ;
#97693 = CARTESIAN_POINT ( 'NONE',  ( -63.65786723876805553, -29.05667524070321761, 77.00078859873751469 ) ) ;
#97694 = VECTOR ( 'NONE', #100002, 1000.000000000000000 ) ;
#97695 = ORIENTED_EDGE ( 'NONE', *, *, #15723, .F. ) ;
#97696 = CARTESIAN_POINT ( 'NONE',  ( -43.60327462000223875, 484.3404548884703900, 1.191632258386134069 ) ) ;
#97697 = CARTESIAN_POINT ( 'NONE',  ( 114.4128415685117517, -60.00000000000000000, 179.0782004262347868 ) ) ;
#97698 = ORIENTED_EDGE ( 'NONE', *, *, #59216, .F. ) ;
#97699 = CARTESIAN_POINT ( 'NONE',  ( 1.492275824608998712E-05, -32.51050348448658411, 29.30806720701680845 ) ) ;
#97700 = CARTESIAN_POINT ( 'NONE',  ( -2.977408999572654480, -12.50000000204838813, 7.188101187499999156 ) ) ;
#97701 = CARTESIAN_POINT ( 'NONE',  ( -7.225703553025883963, -5.000000000000000888, -73.19314196553557395 ) ) ;
#97702 = EDGE_LOOP ( 'NONE', ( #59561, #7764 ) ) ;
#97703 = CIRCLE ( 'NONE', #30544, 0.9999999999999971134 ) ;
#97704 = LINE ( 'NONE', #82600, #88925 ) ;
#97705 = ORIENTED_EDGE ( 'NONE', *, *, #48755, .F. ) ;
#97706 = CARTESIAN_POINT ( 'NONE',  ( -46.00000000000000000, 487.9408407045908689, 0.4609445041378137931 ) ) ;
#97707 = CARTESIAN_POINT ( 'NONE',  ( 5.082755093536324154, -28.71875000204838813, 5.082755093536326818 ) ) ;
#97708 = CARTESIAN_POINT ( 'NONE',  ( -111.6036597322333392, -59.99999999999998579, 158.4792128661873107 ) ) ;
#97709 = FILL_AREA_STYLE_COLOUR ( '', #91537 ) ;
#97710 = CARTESIAN_POINT ( 'NONE',  ( -2.977408999572650039, -25.06250000204838457, -7.188101187500001821 ) ) ;
#97711 = CARTESIAN_POINT ( 'NONE',  ( 33.24561022503103658, 485.0000549217729713, 0.3114934373725461447 ) ) ;
#97712 = PRESENTATION_LAYER_ASSIGNMENT (  '', '', ( #75319 ) ) ;
#97713 = CARTESIAN_POINT ( 'NONE',  ( -5.457196206890739809, 53.44502160359606080, -8.522729681404539903 ) ) ;
#97714 = CARTESIAN_POINT ( 'NONE',  ( 7.149395896920095848E-21, 27.29656849860388235, -40.75000000000000000 ) ) ;
#97715 = PRESENTATION_STYLE_ASSIGNMENT (( #17897 ) ) ;
#97716 = CARTESIAN_POINT ( 'NONE',  ( 0.000000000000000000, 0.000000000000000000, 0.000000000000000000 ) ) ;
#97717 = CARTESIAN_POINT ( 'NONE',  ( 97.58930920902680839, -60.00000000000000711, 101.0550937258192903 ) ) ;
#97718 = CARTESIAN_POINT ( 'NONE',  ( -32.89073344312465252, -29.09100879441119147, 32.34260077112399756 ) ) ;
#97719 = PRESENTATION_STYLE_ASSIGNMENT (( #58889 ) ) ;
#97720 = PRESENTATION_LAYER_ASSIGNMENT (  '', '', ( #1534 ) ) ;
#97721 = CARTESIAN_POINT ( 'NONE',  ( 38.48534256757758953, -25.67948113044661085, 34.55249355692391333 ) ) ;
#97722 = ORIENTED_EDGE ( 'NONE', *, *, #20641, .T. ) ;
#97723 = FACE_OUTER_BOUND ( 'NONE', #13128, .T. ) ;
#97724 = EDGE_CURVE ( 'NONE', #45785, #52343, #11031, .T. ) ;
#97725 = CARTESIAN_POINT ( 'NONE',  ( -61.07287120190940044, -38.34218409855068899, 99.79094347136515353 ) ) ;
#97726 = ORIENTED_EDGE ( 'NONE', *, *, #75342, .F. ) ;
#97728 = CARTESIAN_POINT ( 'NONE',  ( -24.60488647473181345, 306.9835580411500473, 10.41807558718820914 ) ) ;
#97727 = DIRECTION ( 'NONE',  ( 0.000000000000000000, -0.000000000000000000, 1.000000000000000000 ) ) ;
#97729 = CARTESIAN_POINT ( 'NONE',  ( -51.48757442383523397, 38.95383793070303113, -37.45149417477429665 ) ) ;
#97730 = CARTESIAN_POINT ( 'NONE',  ( -6.951447413152005872, 41.73217189154441087, -59.36631701933644933 ) ) ;
#97731 = CARTESIAN_POINT ( 'NONE',  ( 1.219995453278951203, 43.50041496824643161, -17.81587387532546884 ) ) ;
#97732 = CARTESIAN_POINT ( 'NONE',  ( 27.02022815836235026, 6.123233995736770227E-16, -5.000000000000002665 ) ) ;
#97733 = CARTESIAN_POINT ( 'NONE',  ( 5.856955515201466511, -88.78289058880865525, 1.326217528971465942 ) ) ;
#97734 = DIRECTION ( 'NONE',  ( 0.000000000000000000, -1.000000000000000000, 0.000000000000000000 ) ) ;
#97735 = CARTESIAN_POINT ( 'NONE',  ( 100.7731613570876448, -59.99999999999998579, 85.56916059977524469 ) ) ;
#97736 = COLOUR_RGB ( '', 0.40784314, 0.44705882, 0.49803922) ;
#97737 = CARTESIAN_POINT ( 'NONE',  ( -6.474893736874855144, -49.25205468179242274, 39.41360864784692097 ) ) ;
#97738 =( BOUNDED_SURFACE ( )  B_SPLINE_SURFACE ( 3, 2, ( 
 ( #97215, #67396, #1006 ),
 ( #91671, #14166, #89142 ),
 ( #88609, #42041, #47069 ),
 ( #58774, #56203, #88086 ) ),
 .UNSPECIFIED., .F., .F., .F. ) 
 B_SPLINE_SURFACE_WITH_KNOTS ( ( 4, 4 ),
 ( 3, 3 ),
 ( -8.673617379884035472E-19, 0.002038086101534569098 ),
 ( 0.000000000000000000, 1.000000000000000000 ),
 .UNSPECIFIED. ) 
 GEOMETRIC_REPRESENTATION_ITEM ( )  RATIONAL_B_SPLINE_SURFACE ( (
 ( 1.000000000000000000, 0.7927020107002231697, 1.000000000000000000),
 ( 1.000000000000000000, 0.8068894940779135494, 1.000000000000000000),
 ( 1.000000000000000000, 0.8212065780166435403, 1.000000000000000000),
 ( 1.000000000000000000, 0.8350736500408031393, 1.000000000000000000) ) ) 
 REPRESENTATION_ITEM ( '' )  SURFACE ( )  );
#97739 = DIRECTION ( 'NONE',  ( 0.000000000000000000, 1.000000000000000000, 0.000000000000000000 ) ) ;
#97740 = CARTESIAN_POINT ( 'NONE',  ( -2.499999999999999556, -8.000000000000000000, 17.89626171146327493 ) ) ;
#97741 = EDGE_CURVE ( 'NONE', #88742, #74576, #30022, .T. ) ;
#97742 = ORIENTED_EDGE ( 'NONE', *, *, #13257, .F. ) ;
#97743 = CARTESIAN_POINT ( 'NONE',  ( -90.05569471966944661, -29.99999999998339106, -4.911636287503251985 ) ) ;
#97744 = VERTEX_POINT ( 'NONE', #83976 ) ;
#97745 = CARTESIAN_POINT ( 'NONE',  ( -3.352941176470589646, -48.79941684889505638, 104.5794940929807524 ) ) ;
#97746 = CARTESIAN_POINT ( 'NONE',  ( -15.31585736565601508, 3.092902776791752295, -3.111329462075727914 ) ) ;
#97747 = CARTESIAN_POINT ( 'NONE',  ( 0.000000000000000000, 152.0000000000000000, -5.000000000000000000 ) ) ;
#97749 = CARTESIAN_POINT ( 'NONE',  ( -23.13430097919831496, 28.13531915807118367, -30.70617127781035194 ) ) ;
#97748 = CIRCLE ( 'NONE', #30657, 8.000000000000000000 ) ;
#97750 = CARTESIAN_POINT ( 'NONE',  ( 2.977408999572650927, -26.75000000204838457, -7.188101187500001821 ) ) ;
#97751 = DIRECTION ( 'NONE',  ( 0.000000000000000000, -1.000000000000000000, 0.000000000000000000 ) ) ;
#97752 = CARTESIAN_POINT ( 'NONE',  ( 6.846597144391294520, 41.54610357422821920, -70.31839272398791252 ) ) ;
#97753 = ORIENTED_EDGE ( 'NONE', *, *, #61910, .F. ) ;
#97754 =( GEOMETRIC_REPRESENTATION_CONTEXT ( 3 ) GLOBAL_UNCERTAINTY_ASSIGNED_CONTEXT ( ( #79562 ) ) GLOBAL_UNIT_ASSIGNED_CONTEXT ( ( #51343, #42194, #60534 ) ) REPRESENTATION_CONTEXT ( 'NONE', 'WORKASPACE' ) );
#97755 = AXIS2_PLACEMENT_3D ( 'NONE', #47777, #6803, #31643 ) ;
#97756 = AXIS2_PLACEMENT_3D ( 'NONE', #15041, #38300, #31273 ) ;
#97757 = AXIS2_PLACEMENT_3D ( 'NONE', #10430, #77306, #68150 ) ;
#97759 = ORIENTED_EDGE ( 'NONE', *, *, #30119, .T. ) ;
#97758 = CARTESIAN_POINT ( 'NONE',  ( 4.022544416453471605, -1.369395410676485625, 103.0357414394655962 ) ) ;
#97760 = CARTESIAN_POINT ( 'NONE',  ( 79.40570566424929666, -60.32724123763684787, 168.9258148112880349 ) ) ;
#97761 = EDGE_CURVE ( 'NONE', #56223, #10253, #60270, .T. ) ;
#97762 = CARTESIAN_POINT ( 'NONE',  ( 0.000000000000000000, 0.000000000000000000, 5.000000000000000888 ) ) ;
#97763 = VERTEX_POINT ( 'NONE', #19310 ) ;
#97764 = SURFACE_STYLE_USAGE ( .BOTH. , #16322 ) ;
#97765 = CARTESIAN_POINT ( 'NONE',  ( -14.11595029531626722, 2.410436752329290222, 5.024000119293328126 ) ) ;
#97766 = CARTESIAN_POINT ( 'NONE',  ( -7.188101187500000933, -14.00000000204838457, -2.977408999572651371 ) ) ;
#97767 = CARTESIAN_POINT ( 'NONE',  ( 7.046289519167717508, 28.69408180055621926, -3.789821819998816732 ) ) ;
#97768 = CIRCLE ( 'NONE', #65054, 7.499999999992679633 ) ;
#97769 = CARTESIAN_POINT ( 'NONE',  ( -61.06992298392258078, -57.67755795743399716, 111.0944920020532862 ) ) ;
#97770 = EDGE_CURVE ( 'NONE', #80344, #53891, #71324, .T. ) ;
#97771 = CARTESIAN_POINT ( 'NONE',  ( 6.326592304916279552, -6.579439845142160515, -2.267162479624770022 ) ) ;
#97772 = ORIENTED_EDGE ( 'NONE', *, *, #86409, .F. ) ;
#97773 = SURFACE_SIDE_STYLE ('',( #80528 ) ) ;
#97774 = AXIS2_PLACEMENT_3D ( 'NONE', #103643, #29792, #55072 ) ;
#97775 =( LENGTH_UNIT ( ) NAMED_UNIT ( * ) SI_UNIT ( .MILLI., .METRE. ) );
#97776 = DIRECTION ( 'NONE',  ( -0.000000000000000000, -1.000000000000000000, -0.000000000000000000 ) ) ;
#97777 = CARTESIAN_POINT ( 'NONE',  ( 7.479728634662563103, 40.83274492738546257, -59.46320897030336283 ) ) ;
#97778 = DIRECTION ( 'NONE',  ( 0.000000000000000000, -1.000000000000000000, 0.000000000000000000 ) ) ;
#97779 = AXIS2_PLACEMENT_3D ( 'NONE', #96677, #31956, #47576 ) ;
#97780 = VERTEX_POINT ( 'NONE', #99621 ) ;
#97781 = CARTESIAN_POINT ( 'NONE',  ( 7.188101187499999156, -29.75000000204838813, 2.977408999572654924 ) ) ;
#97782 = CARTESIAN_POINT ( 'NONE',  ( -10.95918059713568837, -14.00797954113551747, 31.84498254503383663 ) ) ;
#97783 = CARTESIAN_POINT ( 'NONE',  ( 0.8424608613547267533, 51.37392267887781117, -9.927074889301541916 ) ) ;
#97784 = CIRCLE ( 'NONE', #65072, 3.400000000000000355 ) ;
#97786 = EDGE_CURVE ( 'NONE', #79431, #45302, #47224, .T. ) ;
#97785 = CARTESIAN_POINT ( 'NONE',  ( -9.536842176398147686, 87.64235369883989790, 3.014135744008184847 ) ) ;
#97787 = CARTESIAN_POINT ( 'NONE',  ( 0.000000000000000000, 56.87938524157181774, -0.6840402866513453084 ) ) ;
#97789 = EDGE_CURVE ( 'NONE', #96664, #22950, #78020, .T. ) ;
#97788 = PRODUCT_CONTEXT ( 'NONE', #43806, 'mechanical' ) ;
#97790 = CARTESIAN_POINT ( 'NONE',  ( 49.27893332326006259, 7.918143476871231101, 15.56220613712076606 ) ) ;
#97791 = ORIENTED_EDGE ( 'NONE', *, *, #34273, .T. ) ;
#97792 = CARTESIAN_POINT ( 'NONE',  ( 69.92761780597730592, 6.856755485862130937E-15, 0.000000000000000000 ) ) ;
#97793 = AXIS2_PLACEMENT_3D ( 'NONE', #95215, #27863, #86609 ) ;
#97794 = CARTESIAN_POINT ( 'NONE',  ( -33.16501691561005316, 438.9509064377054415, 23.91453236866925636 ) ) ;
#97795 = CARTESIAN_POINT ( 'NONE',  ( -15.58318277380108263, -24.24093616901115311, -38.53689649557993846 ) ) ;
#97796 = DIRECTION ( 'NONE',  ( 0.000000000000000000, -1.000000000000000000, 0.000000000000000000 ) ) ;
#97797 = DIRECTION ( 'NONE',  ( -1.000000000000000000, -0.000000000000000000, -0.000000000000000000 ) ) ;
#97798 = ORIENTED_EDGE ( 'NONE', *, *, #30119, .F. ) ;
#97799 = STYLED_ITEM ( 'NONE', ( #65969 ), #75757 ) ;
#97800 = CARTESIAN_POINT ( 'NONE',  ( 0.000000000000000000, 1.502314598737159228E-15, -8.000000000000000000 ) ) ;
#97801 = CARTESIAN_POINT ( 'NONE',  ( 101.9220456111045507, -57.63191952442775801, 203.3003234520283513 ) ) ;
#97802 = CIRCLE ( 'NONE', #47829, 2.999999999999999112 ) ;
#97803 = CYLINDRICAL_SURFACE ( 'NONE', #14373, 4.999999999999999112 ) ;
#97804 = CARTESIAN_POINT ( 'NONE',  ( 0.5805565836007648972, -7.505553499465138501, -1.190388518514737689E-16 ) ) ;
#97805 = B_SPLINE_CURVE_WITH_KNOTS ( 'NONE', 3,
 ( #18644, #92493, #51503, #9431, #42352, #2421, #18101, #35364, #75239, #1335, #101126, #34300, #8386, #41288, #67176, #21837, #28336, #21307 ),
 .UNSPECIFIED., .F., .F.,
 ( 4, 2, 2, 2, 2, 2, 2, 2, 4 ),
 ( 0.000000000000000000, 0.0008424128194421235966, 0.001684825638884247193, 0.003369651277768483978, 0.004212064097210603889, 0.005054476916652722931, 0.005475683326373779851, 0.005896889736094835903, 0.006739302555536954079 ),
 .UNSPECIFIED. ) ;
#97806 = SURFACE_STYLE_FILL_AREA ( #29541 ) ;
#97807 = DIRECTION ( 'NONE',  ( -1.000000000000000000, -1.224606353822377258E-16, -0.000000000000000000 ) ) ;
#97808 = CARTESIAN_POINT ( 'NONE',  ( -73.84812816836441129, -60.00000000000000000, 170.6796079630115912 ) ) ;
#97809 = CARTESIAN_POINT ( 'NONE',  ( -21.51569398614858031, 294.9107018935607130, -9.987480606144490736 ) ) ;
#97811 = AXIS2_PLACEMENT_3D ( 'NONE', #89498, #14513, #22125 ) ;
#97810 = CARTESIAN_POINT ( 'NONE',  ( 7.760110535507928807E-13, 7.790254909845448772, -6.526045885145578040 ) ) ;
#97812 = CARTESIAN_POINT ( 'NONE',  ( -40.07586470527510158, 337.7832441655235129, 20.21182470898328631 ) ) ;
#97813 = AXIS2_PLACEMENT_3D ( 'NONE', #72575, #16464, #105477 ) ;
#97814 = CARTESIAN_POINT ( 'NONE',  ( -85.63198936259853156, -32.10030600112477828, 181.8800658012134477 ) ) ;
#97815 = EDGE_LOOP ( 'NONE', ( #66849, #70712, #53220, #105874 ) ) ;
#97816 = CARTESIAN_POINT ( 'NONE',  ( 25.50300299142718075, 306.4699755070969900, -8.645387582429501450 ) ) ;
#97817 = ADVANCED_FACE ( 'NONE', ( #37063 ), #78177, .T. ) ;
#97818 = VERTEX_POINT ( 'NONE', #22469 ) ;
#97819 = DIRECTION ( 'NONE',  ( 0.000000000000000000, -1.000000000000000000, 0.000000000000000000 ) ) ;
#97820 = EDGE_CURVE ( 'NONE', #234, #78207, #74161, .T. ) ;
#97821 = CARTESIAN_POINT ( 'NONE',  ( -119.9999999999999858, 0.000000000000000000, 59.99999999999997158 ) ) ;
#97822 = B_SPLINE_CURVE_WITH_KNOTS ( 'NONE', 3,
 ( #59932, #52872, #45331, #4326, #20031, #27046, #3801, #61523, #62063, #103031, #10799, #12400, #67998, #60466, #86855, #68546, #94952, #51801, #43717, #21087, #53416, #36740, #92797, #78725, #100883, #76607, #2721, #94416, #18958, #35668, #85802, #101433, #78212, #53924 ),
 .UNSPECIFIED., .F., .F.,
 ( 4, 2, 2, 2, 2, 2, 2, 2, 2, 2, 2, 2, 2, 2, 2, 2, 4 ),
 ( 0.01272238763756220782, 0.01351613129786392517, 0.01430987495816564252, 0.01510361861846735987, 0.01589736227876907895, 0.01669110593907079457, 0.01748484959937251365, 0.01827859325967422927, 0.01907233691997594835, 0.01986608058027766396, 0.02065982424057938305, 0.02145356790088109866, 0.02224731156118281775, 0.02304105522148453683, 0.02383479888178625244, 0.02462854254208796806, 0.02542228620238968714 ),
 .UNSPECIFIED. ) ;
#97823 = CARTESIAN_POINT ( 'NONE',  ( -87.02619266019526378, -60.19139343833020206, -6.136718658578977248 ) ) ;
#97824 = DIRECTION ( 'NONE',  ( 0.000000000000000000, -1.000000000000000000, 0.000000000000000000 ) ) ;
#97825 = DIRECTION ( 'NONE',  ( 0.000000000000000000, -1.000000000000000000, 0.000000000000000000 ) ) ;
#97826 = AXIS2_PLACEMENT_3D ( 'NONE', #84592, #35002, #36608 ) ;
#97827 = ORIENTED_EDGE ( 'NONE', *, *, #21429, .T. ) ;
#97828 = COLOUR_RGB ( '', 0.31764706, 0.68627451, 0.89019608) ;
#97830 = CARTESIAN_POINT ( 'NONE',  ( 6.289572920342627604, 6.243622107253692377, -2.843693100100564308 ) ) ;
#97829 = AXIS2_PLACEMENT_3D ( 'NONE', #284, #74206, #84448 ) ;
#97831 = EDGE_CURVE ( 'NONE', #44258, #59773, #4135, .T. ) ;
#97832 = CARTESIAN_POINT ( 'NONE',  ( 11.42180900222615669, 7.623507745330639018, -9.491908323009569770 ) ) ;
#97833 = CARTESIAN_POINT ( 'NONE',  ( -2.910977163135976653, -8.673617379884035472E-16, -22.23822744035697241 ) ) ;
#97834 = CARTESIAN_POINT ( 'NONE',  ( -71.63495682827519317, -59.99999999999997868, -34.46936934826943855 ) ) ;
#97835 = CARTESIAN_POINT ( 'NONE',  ( -74.87526142751326574, -53.38099747595546773, 130.5593691470315605 ) ) ;
#97836 = EDGE_LOOP ( 'NONE', ( #105641, #15580, #59013, #88821, #5339 ) ) ;
#97837 = CARTESIAN_POINT ( 'NONE',  ( 52.32017852953563164, -14.21045842199431242, 63.23906622249963760 ) ) ;
#97838 = CARTESIAN_POINT ( 'NONE',  ( -6.750000000000015099, -11.69134295108991495, -13.00000000000000000 ) ) ;
#97839 = CARTESIAN_POINT ( 'NONE',  ( 92.21232009249456496, -57.65949651113772489, -18.94920474166798385 ) ) ;
#97840 = AXIS2_PLACEMENT_3D ( 'NONE', #30319, #79375, #33917 ) ;
#97841 = AXIS2_PLACEMENT_3D ( 'NONE', #37601, #59722, #70463 ) ;
#97842 = DIRECTION ( 'NONE',  ( 0.000000000000000000, 0.000000000000000000, 1.000000000000000000 ) ) ;
#97843 = DIRECTION ( 'NONE',  ( -0.000000000000000000, -1.000000000000000000, -0.000000000000000000 ) ) ;
#97844 = EDGE_LOOP ( 'NONE', ( #82555, #66404, #52664, #76253 ) ) ;
#97845 = CARTESIAN_POINT ( 'NONE',  ( 0.000000000000000000, 299.9999999999999432, 0.000000000000000000 ) ) ;
#97846 = DIRECTION ( 'NONE',  ( -1.000000000000000000, -1.224606353822377258E-16, -0.000000000000000000 ) ) ;
#97847 = DIRECTION ( 'NONE',  ( -0.000000000000000000, -0.000000000000000000, -1.000000000000000000 ) ) ;
#97848 = CARTESIAN_POINT ( 'NONE',  ( 2.977408999572650927, -18.87500000204838457, -7.188101187500001821 ) ) ;
#97849 = CARTESIAN_POINT ( 'NONE',  ( 0.9763930676201736381, -8.096533237419009765, -7.213065638942138591 ) ) ;
#97850 = CARTESIAN_POINT ( 'NONE',  ( 6.463178677061754307, -2.643201791673488010, -6.839998497243178655 ) ) ;
#97851 = CARTESIAN_POINT ( 'NONE',  ( 0.000000000000000000, 45.50000000000000711, 0.000000000000000000 ) ) ;
#97852 = CARTESIAN_POINT ( 'NONE',  ( -7.500000000000667910, 3.157052757786715791, -7.642767288268637493 ) ) ;
#97853 = SURFACE_STYLE_USAGE ( .BOTH. , #15880 ) ;
#97854 = COLOUR_RGB ( '', 0.72549020, 0.75294118, 0.79215686) ;
#97855 = ORIENTED_EDGE ( 'NONE', *, *, #74554, .T. ) ;
#97856 = CARTESIAN_POINT ( 'NONE',  ( -5.500000000000006217, 42.00000000000000000, -59.88032989329961708 ) ) ;
#97858 = CARTESIAN_POINT ( 'NONE',  ( 29.88845415383573823, -29.06604919746129667, 31.22394821666031817 ) ) ;
#97857 = FILL_AREA_STYLE_COLOUR ( '', #59602 ) ;
#97859 = CARTESIAN_POINT ( 'NONE',  ( -23.38275356398436244, 25.95242394571446098, 30.70617127781060418 ) ) ;
#97860 = EDGE_LOOP ( 'NONE', ( #69504, #53282, #74141, #75524 ) ) ;
#97861 = EDGE_CURVE ( 'NONE', #87634, #47033, #63448, .T. ) ;
#97862 = UNCERTAINTY_MEASURE_WITH_UNIT (LENGTH_MEASURE( 1.000000000000000082E-05 ), #68842, 'distance_accuracy_value', 'NONE');
#97863 = B_SPLINE_CURVE_WITH_KNOTS ( 'NONE', 3,
 ( #105403, #56289, #63374, #46119, #13724, #14785 ),
 .UNSPECIFIED., .F., .F.,
 ( 4, 2, 4 ),
 ( 2.380733003144472638E-07, 0.001898835937927383305, 0.003797433802554452380 ),
 .UNSPECIFIED. ) ;
#97864 = VERTEX_POINT ( 'NONE', #80124 ) ;
#97866 = CARTESIAN_POINT ( 'NONE',  ( 38.51502786939605727, 460.0233756673479206, 2.043034587344084940 ) ) ;
#97865 = DIRECTION ( 'NONE',  ( -1.000000000000000000, -0.000000000000000000, -0.000000000000000000 ) ) ;
#97867 = SURFACE_STYLE_USAGE ( .BOTH. , #22433 ) ;
#97868 = CARTESIAN_POINT ( 'NONE',  ( 100.0424503805845831, 1.016364837396684119E-14, 0.000000000000000000 ) ) ;
#97869 = LINE ( 'NONE', #31062, #20856 ) ;
#97870 = LINE ( 'NONE', #74116, #13859 ) ;
#97871 = CARTESIAN_POINT ( 'NONE',  ( -7.499999999999998224, 1.489914625144000082, -0.1187923833806731472 ) ) ;
#97873 = ORIENTED_EDGE ( 'NONE', *, *, #10028, .F. ) ;
#97872 = CONICAL_SURFACE ( 'NONE', #89264, 8.000000000000000000, 0.9599310885968798113 ) ;
#97874 = ADVANCED_FACE ( 'NONE', ( #71502 ), #13794, .T. ) ;
#97875 = CARTESIAN_POINT ( 'NONE',  ( 65.84150895268908243, -60.00000000000000000, -33.94149391649602165 ) ) ;
#97876 = DIRECTION ( 'NONE',  ( -0.5735764363510510444, -0.8191520442889883569, 0.000000000000000000 ) ) ;
#97877 = CARTESIAN_POINT ( 'NONE',  ( 32.09753956878954284, 464.8111968410944996, 11.80755753166117650 ) ) ;
#97878 = CARTESIAN_POINT ( 'NONE',  ( 46.00000000000000000, 461.9428920847514632, 12.03309428281642823 ) ) ;
#97879 = DIRECTION ( 'NONE',  ( -1.000000000000000000, 0.000000000000000000, 0.000000000000000000 ) ) ;
#97880 = EDGE_CURVE ( 'NONE', #83314, #76218, #62722, .T. ) ;
#97881 = EDGE_LOOP ( 'NONE', ( #5873, #79139, #105553, #22222 ) ) ;
#97882 = ORIENTED_EDGE ( 'NONE', *, *, #85211, .T. ) ;
#97883 = ORIENTED_EDGE ( 'NONE', *, *, #44250, .T. ) ;
#97884 = CARTESIAN_POINT ( 'NONE',  ( 1.126990790682043331, 54.02434422481241683, 8.453431372524891074 ) ) ;
#97885 = CARTESIAN_POINT ( 'NONE',  ( 0.000000000000000000, 0.000000000000000000, -0.5776712190230098853 ) ) ;
#97886 = CARTESIAN_POINT ( 'NONE',  ( -36.89235641323539028, 438.8966234958797941, 23.87184663332199364 ) ) ;
#97887 = CARTESIAN_POINT ( 'NONE',  ( 32.29035655572196362, 338.5555644040533707, 18.47678205815309127 ) ) ;
#97888 = CARTESIAN_POINT ( 'NONE',  ( -35.15293763552459438, 323.3451953424660701, -4.993677134961036046 ) ) ;
#97889 = CARTESIAN_POINT ( 'NONE',  ( -5.051174013757951720, -64.37264992930795415, 13.91140790810193018 ) ) ;
#97890 = CARTESIAN_POINT ( 'NONE',  ( -44.23892967119426345, 485.3473288767967802, 2.237067153676693732 ) ) ;
#97891 = CARTESIAN_POINT ( 'NONE',  ( -5.385673916453011856, 0.000000000000000000, 18.57417562100670949 ) ) ;
#97892 = VECTOR ( 'NONE', #95643, 999.9999999999998863 ) ;
#97893 = ORIENTED_EDGE ( 'NONE', *, *, #70224, .T. ) ;
#97894 = DIRECTION ( 'NONE',  ( 0.000000000000000000, 1.000000000000000000, 0.000000000000000000 ) ) ;
#97895 = ORIENTED_EDGE ( 'NONE', *, *, #15042, .F. ) ;
#97896 = DIRECTION ( 'NONE',  ( -1.000000000000000000, -1.224606353822377258E-16, -0.000000000000000000 ) ) ;
#97897 = CIRCLE ( 'NONE', #77269, 4.172000000000001485 ) ;
#97898 = FACE_BOUND ( 'NONE', #86961, .T. ) ;
#97899 = CARTESIAN_POINT ( 'NONE',  ( 63.59140386760513053, -56.86218274724328126, 91.13360387561940001 ) ) ;
#97900 = B_SPLINE_CURVE_WITH_KNOTS ( 'NONE', 3,
 ( #38996, #88601, #14156, #105313 ),
 .UNSPECIFIED., .F., .F.,
 ( 4, 4 ),
 ( 0.0007371174630664029549, 0.02698393829534635746 ),
 .UNSPECIFIED. ) ;
#97901 = ORIENTED_EDGE ( 'NONE', *, *, #32315, .T. ) ;
#97902 =( NAMED_UNIT ( * ) PLANE_ANGLE_UNIT ( ) SI_UNIT ( $, .RADIAN. ) );
#97903 = CARTESIAN_POINT ( 'NONE',  ( 0.01372220897662188889, -5.948365447239590154, -2.697128823393880825 ) ) ;
#97904 = CARTESIAN_POINT ( 'NONE',  ( -64.02773510654475331, -57.67113784069211135, -36.59462343474526591 ) ) ;
#97905 = EDGE_CURVE ( 'NONE', #67283, #17532, #85111, .T. ) ;
#97906 = ORIENTED_EDGE ( 'NONE', *, *, #334, .F. ) ;
#97907 = B_SPLINE_CURVE_WITH_KNOTS ( 'NONE', 3,
 ( #32269, #65144, #31227, #31741, #106657 ),
 .UNSPECIFIED., .F., .F.,
 ( 4, 1, 4 ),
 ( 0.000000000000000000, 0.003752776749732572668, 0.007505553499465145335 ),
 .UNSPECIFIED. ) ;
#97908 = SURFACE_SIDE_STYLE ('',( #106525 ) ) ;
#97909 = STYLED_ITEM ( 'NONE', ( #84843 ), #41411 ) ;
#97910 = EDGE_CURVE ( 'NONE', #43603, #101117, #61859, .T. ) ;
#97911 = AXIS2_PLACEMENT_3D ( 'NONE', #96052, #45907, #104658 ) ;
#97912 = CARTESIAN_POINT ( 'NONE',  ( -35.80547854524250084, 490.7930927354825030, 12.38248481219812902 ) ) ;
#97913 = CARTESIAN_POINT ( 'NONE',  ( 7.999999999999998224, -32.28125000409677625, 3.313708498984766493 ) ) ;
#97914 = EDGE_CURVE ( 'NONE', #15190, #45269, #19722, .T. ) ;
#97915 = CARTESIAN_POINT ( 'NONE',  ( -2.094395098902661179, -4.999999999999998224, 8.000000000000000000 ) ) ;
#97916 = CIRCLE ( 'NONE', #47929, 5.000000000000010658 ) ;
#97917 = CYLINDRICAL_SURFACE ( 'NONE', #15441, 1.250000000000001110 ) ;
#97918 = CARTESIAN_POINT ( 'NONE',  ( 9.165151389911679658, 30.00000000000000000, 4.000000000000000000 ) ) ;
#97919 = CARTESIAN_POINT ( 'NONE',  ( 7.002641335706727865, -8.949127373191689827, 3.868676264653292840 ) ) ;
#97921 =( NAMED_UNIT ( * ) SI_UNIT ( $, .STERADIAN. ) SOLID_ANGLE_UNIT ( ) );
#97920 = CARTESIAN_POINT ( 'NONE',  ( 51.88291765283141643, 168.1183258647170362, 182.1969486012845891 ) ) ;
#97922 = CARTESIAN_POINT ( 'NONE',  ( 18.95008105897379025, 304.6966521252900293, 8.904021126966123134 ) ) ;
#97923 = ORIENTED_EDGE ( 'NONE', *, *, #29060, .T. ) ;
#97924 = DIRECTION ( 'NONE',  ( 0.000000000000000000, -0.8784936690177046481, 0.4777539884666709424 ) ) ;
#97925 = DIRECTION ( 'NONE',  ( -1.000000000000000000, 0.000000000000000000, 0.000000000000000000 ) ) ;
#97926 = DIRECTION ( 'NONE',  ( 0.5735764363510468256, 0.8191520442889913545, 0.000000000000000000 ) ) ;
#97927 = CARTESIAN_POINT ( 'NONE',  ( -94.21191784372652478, -30.00000000000000355, 191.2965387815471843 ) ) ;
#97928 = CIRCLE ( 'NONE', #51427, 4.000000000000007105 ) ;
#97929 = LINE ( 'NONE', #16486, #57202 ) ;
#97930 = CARTESIAN_POINT ( 'NONE',  ( 35.43536369062855584, -57.69560819355115910, 49.59754854414701697 ) ) ;
#97932 = CARTESIAN_POINT ( 'NONE',  ( -9.973775868872957417, 7.480993720211312592, 0.6548301084105181413 ) ) ;
#97931 = CARTESIAN_POINT ( 'NONE',  ( 5.902962692465450800, 41.87327339699978523, -59.02279353628206593 ) ) ;
#97933 = STYLED_ITEM ( 'NONE', ( #64592 ), #32808 ) ;
#97934 = B_SPLINE_CURVE_WITH_KNOTS ( 'NONE', 3,
 ( #33708, #67659, #92438, #100538, #1831, #35316, #49861, #50912, #42302, #58502, #51984, #91407, #68734, #84901, #34252, #75189, #82767, #59036, #2370, #101075, #84371, #27235, #10462, #83822, #67124, #34788, #50382, #99465, #75735, #17521, #26701, #76264, #83295, #68180 ),
 .UNSPECIFIED., .F., .F.,
 ( 4, 2, 2, 2, 2, 2, 2, 2, 2, 2, 2, 2, 2, 2, 2, 2, 4 ),
 ( 0.000000000000000000, 0.0007951492273476383141, 0.001590298454695276628, 0.002385447682042914942, 0.003180596909390553256, 0.003975746136738191570, 0.004770895364085829884, 0.005566044591433468199, 0.006361193818781106513, 0.007156343046128744827, 0.007951492273476383141, 0.008746641500824020588, 0.009541790728171659769, 0.01033693995551929895, 0.01113208918286693640, 0.01192723841021457384, 0.01272238763756221303 ),
 .UNSPECIFIED. ) ;
#97935 = CIRCLE ( 'NONE', #20558, 4.172000000000001485 ) ;
#97936 = CARTESIAN_POINT ( 'NONE',  ( 9.997272199965776096, -22.62240898069702411, -38.54272479879313806 ) ) ;
#97937 = CARTESIAN_POINT ( 'NONE',  ( -1.250245718140553297, 43.55766156206008333, 17.65597227886197373 ) ) ;
#97938 = UNCERTAINTY_MEASURE_WITH_UNIT (LENGTH_MEASURE( 1.000000000000000082E-05 ), #4038, 'distance_accuracy_value', 'NONE');
#97939 = CARTESIAN_POINT ( 'NONE',  ( -44.03912857160338490, 435.2850055576093951, 15.29440791316631909 ) ) ;
#97940 = CARTESIAN_POINT ( 'NONE',  ( -21.06506537777876531, -59.99999999999999289, 40.36978327349123674 ) ) ;
#97941 =( LENGTH_UNIT ( ) NAMED_UNIT ( * ) SI_UNIT ( .MILLI., .METRE. ) );
#97942 = AXIS2_PLACEMENT_3D ( 'NONE', #69389, #83961, #101740 ) ;
#97943 = CARTESIAN_POINT ( 'NONE',  ( 93.97977184163765685, -5.000000000000000000, 6.123233995736778115E-16 ) ) ;
#97944 = CARTESIAN_POINT ( 'NONE',  ( -86.90711792063859775, -24.33407301245372523, 186.0904578520139978 ) ) ;
#97945 = ORIENTED_EDGE ( 'NONE', *, *, #30299, .F. ) ;
#97946 = CARTESIAN_POINT ( 'NONE',  ( 17.50000000000003197, 51.99999999999912603, 59.56761335715597028 ) ) ;
#97947 = CARTESIAN_POINT ( 'NONE',  ( 7.398498408818926286, -14.96086698649159530, 15.11142416646496578 ) ) ;
#97948 = CARTESIAN_POINT ( 'NONE',  ( -9.411392529996735590, -60.36588867045908557, 33.95496757082129591 ) ) ;
#97949 = CARTESIAN_POINT ( 'NONE',  ( 0.000000000000000000, -5.629165124598848990, -3.250000000000003553 ) ) ;
#97950 = B_SPLINE_SURFACE_WITH_KNOTS ( 'NONE', 3, 3, ( 
 ( #66268, #68414, #27456, #85117, #11202, #74350, #428, #17207 ),
 ( #27989, #71053, #61389, #4733, #37671, #54308, #61931, #37131 ),
 ( #101823, #3676, #3136, #4201, #44674, #45720, #5267, #95337 ),
 ( #62973, #95874, #21999, #36609, #68952, #70531, #69997, #103424 ),
 ( #62446, #21472, #13330, #20443, #54852, #28506, #29573, #102898 ),
 ( #87780, #78083, #19899, #94821, #29062, #53802, #77561, #87254 ),
 ( #46255, #79141, #45209, #44136, #38193, #60856, #103943, #30089 ),
 ( #77019, #36081, #20967, #93745, #52741, #85664, #69474, #102358 ) ),
 .UNSPECIFIED., .F., .F., .F.,
 ( 4, 2, 2, 4 ),
 ( 4, 2, 2, 4 ),
 ( 0.000000000000000000, 0.2500000000000000000, 0.5000000000000000000, 1.000000000000000000 ),
 ( 0.000000000000000000, 0.2500000000000000000, 0.5000000000000000000, 1.000000000000000000 ),
 .UNSPECIFIED. ) ;
#97952 = CARTESIAN_POINT ( 'NONE',  ( 5.000000000000000000, -60.71953810597847223, 12.61250543006446989 ) ) ;
#97951 = DIRECTION ( 'NONE',  ( -1.000000000000000000, -1.224606353822377258E-16, -0.000000000000000000 ) ) ;
#97953 = EDGE_CURVE ( 'NONE', #54847, #21676, #34280, .T. ) ;
#97954 = ORIENTED_EDGE ( 'NONE', *, *, #42489, .F. ) ;
#97955 = MECHANICAL_DESIGN_GEOMETRIC_PRESENTATION_REPRESENTATION (  '', ( #37730 ), #18781 ) ;
#97956 = CARTESIAN_POINT ( 'NONE',  ( -9.499999896953589484, -5.000000000000002665, -20.99851281918368784 ) ) ;
#97957 = CARTESIAN_POINT ( 'NONE',  ( 16.58588328558601788, 34.28973238854128880, 24.30698433968584027 ) ) ;
#97958 = CARTESIAN_POINT ( 'NONE',  ( 29.07074031792576463, 306.7727993643221112, -9.118181477239474475 ) ) ;
#97959 = EDGE_CURVE ( 'NONE', #48048, #29468, #31096, .T. ) ;
#97960 = DIRECTION ( 'NONE',  ( 0.000000000000000000, 0.000000000000000000, 1.000000000000000000 ) ) ;
#97961 = CARTESIAN_POINT ( 'NONE',  ( 61.46887122245544077, -60.00000000000000000, 105.4469840523393458 ) ) ;
#97962 = CARTESIAN_POINT ( 'NONE',  ( 5.299999999999999822, -3.752776749732553263, 6.499999999999999112 ) ) ;
#97963 = ORIENTED_EDGE ( 'NONE', *, *, #31638, .T. ) ;
#97964 = DIRECTION ( 'NONE',  ( -1.000000000000000000, 0.000000000000000000, 0.000000000000000000 ) ) ;
#97965 = CARTESIAN_POINT ( 'NONE',  ( -9.334514330295453632, 251.7862273768178909, -3.588704711590601004 ) ) ;
#97966 = DIRECTION ( 'NONE',  ( 1.000000000000000000, 1.224606353822377258E-16, 0.000000000000000000 ) ) ;
#97967 = AXIS2_PLACEMENT_3D ( 'NONE', #10971, #92425, #50898 ) ;
#97969 = LINE ( 'NONE', #17066, #66603 ) ;
#97968 = CARTESIAN_POINT ( 'NONE',  ( 44.75958163560274272, -30.00000000000001776, 54.38364795613178870 ) ) ;
#97970 = CIRCLE ( 'NONE', #92813, 4.000000000000007105 ) ;
#97971 = PRESENTATION_STYLE_ASSIGNMENT (( #22530 ) ) ;
#97972 = ORIENTED_EDGE ( 'NONE', *, *, #25289, .F. ) ;
#97973 = DIRECTION ( 'NONE',  ( 0.000000000000000000, 1.000000000000000000, 0.000000000000000000 ) ) ;
#97974 = EDGE_LOOP ( 'NONE', ( #99797, #15760, #16133, #99924 ) ) ;
#97975 = CARTESIAN_POINT ( 'NONE',  ( 38.81358894280361937, 485.1131561813197095, -4.191378885297321055 ) ) ;
#97976 = DIRECTION ( 'NONE',  ( -1.000000000000000000, 0.000000000000000000, 0.000000000000000000 ) ) ;
#97977 = ORIENTED_EDGE ( 'NONE', *, *, #93443, .T. ) ;
#97978 = ADVANCED_FACE ( 'NONE', ( #65012 ), #14562, .F. ) ;
#97979 = CARTESIAN_POINT ( 'NONE',  ( -55.22048556080177661, 48.00000000000000000, 34.80214219306111545 ) ) ;
#97980 = CARTESIAN_POINT ( 'NONE',  ( 6.923875968564608741, -12.36264606019372714, 8.501481527785209380 ) ) ;
#97981 = CARTESIAN_POINT ( 'NONE',  ( -73.56062074102059967, -60.00000000001949019, 187.3333967129919131 ) ) ;
#97982 = DIRECTION ( 'NONE',  ( 0.000000000000000000, -1.000000000000000000, 0.000000000000000000 ) ) ;
#97983 = CARTESIAN_POINT ( 'NONE',  ( 64.60710420547525246, -60.00000000000000000, 116.1616718869901632 ) ) ;
#97984 = DIRECTION ( 'NONE',  ( 0.000000000000000000, 0.000000000000000000, -1.000000000000000000 ) ) ;
#97986 = CARTESIAN_POINT ( 'NONE',  ( 15.66189778777191854, -39.47289686819183174, 30.64853919330023402 ) ) ;
#97985 = CARTESIAN_POINT ( 'NONE',  ( -112.8607363433238930, -60.00000000000000000, 189.7948125560051551 ) ) ;
#97987 = AXIS2_PLACEMENT_3D ( 'NONE', #88365, #82379, #8487 ) ;
#97988 = CARTESIAN_POINT ( 'NONE',  ( 82.45244879800553406, -37.99999999999995737, 11.14743738424387764 ) ) ;
#97989 = DIRECTION ( 'NONE',  ( -0.000000000000000000, -0.000000000000000000, 1.000000000000000000 ) ) ;
#97990 = CARTESIAN_POINT ( 'NONE',  ( -47.00008757630948253, -53.35960851535460137, 50.29090797156688097 ) ) ;
#97991 = EDGE_CURVE ( 'NONE', #72492, #42175, #97075, .T. ) ;
#97992 = CARTESIAN_POINT ( 'NONE',  ( -1.125072770816725631, 34.85036833913648735, -27.86405521226426529 ) ) ;
#97993 = ORIENTED_EDGE ( 'NONE', *, *, #104657, .F. ) ;
#97994 = CARTESIAN_POINT ( 'NONE',  ( 0.000000000000000000, 79.50000000000000000, 0.000000000000000000 ) ) ;
#97995 = VECTOR ( 'NONE', #40471, 1000.000000000000000 ) ;
#97996 = CARTESIAN_POINT ( 'NONE',  ( 5.983613182656019269, -12.98062839397017143, 13.15810238988798275 ) ) ;
#97997 = CARTESIAN_POINT ( 'NONE',  ( 0.000000000000000000, -30.00000000000000000, 0.000000000000000000 ) ) ;
#97998 = DIRECTION ( 'NONE',  ( 0.000000000000000000, -1.000000000000000000, 0.000000000000000000 ) ) ;
#97999 = CARTESIAN_POINT ( 'NONE',  ( 34.72474116627837759, 338.3618661353910966, -1.881472242819908436 ) ) ;
#98000 = EDGE_LOOP ( 'NONE', ( #102998, #29440, #61459, #82077 ) ) ;
#98001 = CARTESIAN_POINT ( 'NONE',  ( 5.164787682159408533, -48.11244280217346869, 104.1470044518087121 ) ) ;
#98002 = ORIENTED_EDGE ( 'NONE', *, *, #5398, .T. ) ;
#98003 = CARTESIAN_POINT ( 'NONE',  ( 88.03191322166020427, -30.00000000001757883, 198.6467012898908138 ) ) ;
#98004 = CARTESIAN_POINT ( 'NONE',  ( 46.89473120401049044, 12.86731181406132940, 16.16132821689873467 ) ) ;
#98005 = CARTESIAN_POINT ( 'NONE',  ( 5.484632749660399931, 41.99999999999999289, -59.73832504088978368 ) ) ;
#98006 =( LENGTH_UNIT ( ) NAMED_UNIT ( * ) SI_UNIT ( .MILLI., .METRE. ) );
#98007 = CARTESIAN_POINT ( 'NONE',  ( 100.5443587151843587, -29.99999999999998934, 159.7778150890727034 ) ) ;
#98008 = CARTESIAN_POINT ( 'NONE',  ( 7.800703710507054467, 101.4140430734205722, 1.791736796405269505 ) ) ;
#98009 = EDGE_CURVE ( 'NONE', #76835, #22614, #93276, .T. ) ;
#98010 = ORIENTED_EDGE ( 'NONE', *, *, #92939, .F. ) ;
#98011 = AXIS2_PLACEMENT_3D ( 'NONE', #3662, #77544, #5251 ) ;
#98012 = ORIENTED_EDGE ( 'NONE', *, *, #101069, .F. ) ;
#98013 = ORIENTED_EDGE ( 'NONE', *, *, #10031, .F. ) ;
#98015 = STYLED_ITEM ( 'NONE', ( #19326 ), #6315 ) ;
#98014 = PLANE ( 'NONE',  #95622 ) ;
#98016 = CARTESIAN_POINT ( 'NONE',  ( 43.21893375708788909, 435.1753267431913059, 16.08377476661154049 ) ) ;
#98017 = CARTESIAN_POINT ( 'NONE',  ( -40.24406161231355128, 464.3083606258045393, 17.73326746338202398 ) ) ;
#98019 = EDGE_LOOP ( 'NONE', ( #5525, #29709, #106188, #91093, #56038, #57197 ) ) ;
#98018 = CONICAL_SURFACE ( 'NONE', #6698, 4.172000000000001485, 0.9599310885968750373 ) ;
#98020 = CARTESIAN_POINT ( 'NONE',  ( 43.50377727019363050, 435.9167426301696082, 18.24083946424738656 ) ) ;
#98021 = ORIENTED_EDGE ( 'NONE', *, *, #102050, .F. ) ;
#98022 = DIRECTION ( 'NONE',  ( 0.000000000000000000, -0.5000000000000008882, 0.8660254037844382635 ) ) ;
#98023 = CARTESIAN_POINT ( 'NONE',  ( 85.15092372543439581, -38.69193916550122481, 198.5729534848597950 ) ) ;
#98024 = CARTESIAN_POINT ( 'NONE',  ( 11.56920740162696504, 7.271532733520360559, 9.332439291405307813 ) ) ;
#98025 = DIRECTION ( 'NONE',  ( -0.000000000000000000, -0.000000000000000000, -1.000000000000000000 ) ) ;
#98026 = CARTESIAN_POINT ( 'NONE',  ( 28.92518549787927284, 311.7025783839076780, 12.06490527370083576 ) ) ;
#98027 = CARTESIAN_POINT ( 'NONE',  ( 0.000000000000000000, 6.123233995736770227E-16, -5.000000000000002665 ) ) ;
#98028 = COLOUR_RGB ( '', 0.31764706, 0.68627451, 0.89019608) ;
#98029 = SURFACE_STYLE_FILL_AREA ( #17130 ) ;
#98030 = CARTESIAN_POINT ( 'NONE',  ( -41.35053930173865666, 461.4196900451802321, 2.572867796569714205 ) ) ;
#98031 = CARTESIAN_POINT ( 'NONE',  ( -4.869065774733876140, -47.04879514974081189, 102.3543991519893979 ) ) ;
#98032 = DIRECTION ( 'NONE',  ( -1.000000000000000000, -0.000000000000000000, -0.000000000000000000 ) ) ;
#98033 = EDGE_CURVE ( 'NONE', #37408, #22326, #48808, .T. ) ;
#98034 = ORIENTED_EDGE ( 'NONE', *, *, #1640, .T. ) ;
#98035 = CARTESIAN_POINT ( 'NONE',  ( 0.9999999999999940048, -50.00000000000000000, 101.0455488498966758 ) ) ;
#98036 = VECTOR ( 'NONE', #2656, 1000.000000000000000 ) ;
#98038 = CARTESIAN_POINT ( 'NONE',  ( -26.69297641637695406, 296.2154876107852601, 2.232032846593750897 ) ) ;
#98037 = FILL_AREA_STYLE ('',( #98559 ) ) ;
#98039 = UNCERTAINTY_MEASURE_WITH_UNIT (LENGTH_MEASURE( 1.000000000000000082E-05 ), #4210, 'distance_accuracy_value', 'NONE');
#98040 = DIRECTION ( 'NONE',  ( -0.000000000000000000, -1.000000000000000000, -0.000000000000000000 ) ) ;
#98041 = CARTESIAN_POINT ( 'NONE',  ( -8.000000000000000000, -14.84374999999999112, -3.313708498984762496 ) ) ;
#98042 = DIRECTION ( 'NONE',  ( -1.000000000000000000, -1.224606353822377258E-16, -0.000000000000000000 ) ) ;
#98043 = CLOSED_SHELL ( 'NONE', ( #69524, #66648, #94703, #96860, #83799, #21406, #14116, #99493, #62498, #64748, #66999, #27714, #47389, #40942, #1752, #13602, #505, #55549, #62227, #104882, #14426, #27464, #61509, #6877, #37327, #62768, #56566, #3189, #13303, #30595, #35311, #13769, #63372, #11836, #27063, #103015, #26337, #34035, #81244, #97609, #58944, #102245, #15267, #57278, #95487, #26422, #60693, #50060, #104004, #43296, #27509, #18188, #8247, #105709, #10749, #80567, #27111, #22048, #10102, #44656, #45138, #47896, #45528, #8060, #55224, #21279, #30697, #55875, #24968, #25068, #42835, #10532, #48288, #88320, #55302, #71172, #87791, #95563, #7806, #41848, #103487, #58396, #85777, #93866, #15421, #4149, #41812, #14742, #47052, #93818, #53083, #59212, #46011, #86919, #97230, #101262, #80968, #83141, #39227, #56710, #57246, #80038, #454, #79103, #82680, #42027, #86186, #59562, #8864, #22477, #82249, #33781, #89372, #72805, #39313, #13221, #25923, #53735, #15472, #76443, #39383, #46236, #43525, #52078, #62258, #44106, #13910, #92882, #43248, #9275, #26173, #73640, #46477, #65497, #44233, #31709, #31854 ) ) ;
#98044 = ADVANCED_FACE ( 'NONE', ( #105471 ), #31772, .T. ) ;
#98045 = CARTESIAN_POINT ( 'NONE',  ( -7.986468734911285949, 101.0268632027691922, 0.5341897780976139209 ) ) ;
#98046 = ORIENTED_EDGE ( 'NONE', *, *, #106672, .F. ) ;
#98047 = CARTESIAN_POINT ( 'NONE',  ( 85.12736371515951816, -39.33789070826465206, 184.1504447524897046 ) ) ;
#98048 = CARTESIAN_POINT ( 'NONE',  ( 0.000000000000000000, 0.000000000000000000, 0.000000000000000000 ) ) ;
#98049 = CARTESIAN_POINT ( 'NONE',  ( 1.102182119232618897E-15, -20.00000000000001776, 9.000000000000007105 ) ) ;
#98050 = ORIENTED_EDGE ( 'NONE', *, *, #710, .F. ) ;
#98051 = CARTESIAN_POINT ( 'NONE',  ( 82.54125890550720612, -57.67110014045612587, -28.70085741798137846 ) ) ;
#98052 = EDGE_CURVE ( 'NONE', #62602, #31698, #78400, .T. ) ;
#98053 = CARTESIAN_POINT ( 'NONE',  ( 36.14862957314556269, 438.2394791802972236, 3.891583768389438092 ) ) ;
#98054 = CARTESIAN_POINT ( 'NONE',  ( -81.57465289304622047, -30.00000000000000711, -5.224175191359936576 ) ) ;
#98055 = CARTESIAN_POINT ( 'NONE',  ( -85.74343386013892143, -37.99999999999996447, 185.6815049747404487 ) ) ;
#98056 = CARTESIAN_POINT ( 'NONE',  ( 4.175893272575848414, -4.999999999999998224, 7.137815226408912750 ) ) ;
#98057 = DIRECTION ( 'NONE',  ( 0.000000000000000000, 1.000000000000000000, 0.000000000000000000 ) ) ;
#98058 = AXIS2_PLACEMENT_3D ( 'NONE', #74296, #29776, #15532 ) ;
#98060 = CARTESIAN_POINT ( 'NONE',  ( 59.89460441624491693, 4.000000000000014211, 0.000000000000000000 ) ) ;
#98059 = CARTESIAN_POINT ( 'NONE',  ( 22.57792046605466041, 0.000000000000000000, 5.000000000000002665 ) ) ;
#98061 = FILL_AREA_STYLE_COLOUR ( '', #56244 ) ;
#98062 = CARTESIAN_POINT ( 'NONE',  ( -29.49662366984263073, 18.54149253525968177, 39.61409757040016189 ) ) ;
#98063 = CARTESIAN_POINT ( 'NONE',  ( -12.50000000000000711, -3.000000000000000000, -79.51734232575269345 ) ) ;
#98064 = CARTESIAN_POINT ( 'NONE',  ( 29.66054107240687543, -5.000000000000000888, 6.123233995736769241E-16 ) ) ;
#98065 = B_SPLINE_CURVE_WITH_KNOTS ( 'NONE', 3,
 ( #92632, #101789, #9573, #84555, #76439, #2551, #3637, #62937, #79628, #12764, #102321, #37097, #71014, #29537, #94242, #38155, #69960, #21431, #86696, #53250, #104432, #103387, #102860, #103905, #30581, #87745, #13826, #55343, #88272, #63476, #29027, #30050, #61891, #28472, #95831, #5228, #87212, #37633, #12238, #38664, #21960, #4165, #54815, #71532, #70496, #94787, #46738, #96374, #22503, #95303, #5745, #14349, #20931, #47256, #62409, #80155, #36573, #69440, #61350, #79106 ),
 .UNSPECIFIED., .F., .F.,
 ( 4, 1, 1, 1, 1, 1, 1, 2, 2, 1, 1, 1, 1, 1, 2, 2, 2, 1, 1, 1, 1, 2, 2, 1, 1, 1, 2, 2, 1, 2, 2, 1, 1, 1, 2, 2, 1, 1, 1, 1, 2, 2, 4 ),
 ( 0.000000000000000000, 0.06250000000007288614, 0.09375000000010748347, 0.1093750000001247752, 0.1171875000001345590, 0.1210937500001394579, 0.1230468750001419004, 0.1240234375001431216, 0.1250000000001443290, 0.1875000000001278977, 0.2187500000001189882, 0.2343750000001152134, 0.2421875000001140199, 0.2460937500001134093, 0.2480468750001131040, 0.2500000000001127987, 0.3750000000001774136, 0.4375000000002063905, 0.4687500000002197686, 0.4843750000002270961, 0.4921875000002307043, 0.4960937500002312595, 0.5000000000002318146, 0.5312500000002529088, 0.5468750000002652323, 0.5546875000002742251, 0.5585937500002765566, 0.5625000000002788880, 0.5937500000002960965, 0.6093750000003039791, 0.6250000000003118616, 0.6875000000003395062, 0.7187500000003508305, 0.7343750000003561595, 0.7421875000003588241, 0.7500000000003614886, 0.8125000000003130829, 0.8437500000002844391, 0.8593750000002658984, 0.8671875000002566836, 0.8710937500002481348, 0.8750000000002395861, 1.000000000000000000 ),
 .UNSPECIFIED. ) ;
#98066 = CARTESIAN_POINT ( 'NONE',  ( 9.403185743875306812, 15.24615751665919916, -3.409011323176907027 ) ) ;
#98067 = DIRECTION ( 'NONE',  ( -0.000000000000000000, -1.000000000000000000, -0.000000000000000000 ) ) ;
#98068 = AXIS2_PLACEMENT_3D ( 'NONE', #53059, #100529, #36905 ) ;
#98069 = CARTESIAN_POINT ( 'NONE',  ( 71.30924092933392444, -30.00000000000000711, -20.00752902790307530 ) ) ;
#98070 = VERTEX_POINT ( 'NONE', #19037 ) ;
#98071 = CARTESIAN_POINT ( 'NONE',  ( 0.000000000000000000, -5.000000000000000888, -73.00000000000001421 ) ) ;
#98072 = CARTESIAN_POINT ( 'NONE',  ( 7.549006887134069643, -4.358421158401203144, -7.700127545397313256 ) ) ;
#98073 = CARTESIAN_POINT ( 'NONE',  ( -26.77005346869424329, -20.63395408316250723, -32.73886166069684123 ) ) ;
#98075 = CARTESIAN_POINT ( 'NONE',  ( -32.37202873548481818, -60.22819029308026728, -34.89880865881568894 ) ) ;
#98074 = CARTESIAN_POINT ( 'NONE',  ( 34.83349330513380693, -4.000000000000000888, 4.898587196589416773E-16 ) ) ;
#98076 = ADVANCED_FACE ( 'NONE', ( #17411 ), #84791, .F. ) ;
#98077 = VERTEX_POINT ( 'NONE', #9285 ) ;
#98078 = VECTOR ( 'NONE', #2987, 1000.000000000000000 ) ;
#98079 = VERTEX_POINT ( 'NONE', #9816 ) ;
#98080 = DIRECTION ( 'NONE',  ( -0.000000000000000000, -0.000000000000000000, -1.000000000000000000 ) ) ;
#98081 = EDGE_CURVE ( 'NONE', #7161, #39006, #17942, .T. ) ;
#98082 = AXIS2_PLACEMENT_3D ( 'NONE', #77777, #36300, #70738 ) ;
#98083 = DIRECTION ( 'NONE',  ( 1.000000000000000000, 0.000000000000000000, 0.000000000000000000 ) ) ;
#98084 = DIRECTION ( 'NONE',  ( -0.1108331996454381269, -0.9715652913456128692, -0.2092292678113389093 ) ) ;
#98085 = CARTESIAN_POINT ( 'NONE',  ( -87.91029806970415450, -60.00000000000000000, -21.68455642860508448 ) ) ;
#98086 = ORIENTED_EDGE ( 'NONE', *, *, #61923, .F. ) ;
#98087 = CARTESIAN_POINT ( 'NONE',  ( 33.86650669486618881, 1.474610560812782335E-15, 0.000000000000000000 ) ) ;
#98088 = CARTESIAN_POINT ( 'NONE',  ( -9.246279647933185686, 16.00000000000000000, 3.826931552919418777 ) ) ;
#98089 = CARTESIAN_POINT ( 'NONE',  ( 93.93808739026684407, -37.70322700098001434, 192.9552561637989925 ) ) ;
#98091 = CARTESIAN_POINT ( 'NONE',  ( 4.284822031654949015, -48.90716638558772900, 104.4267991316944943 ) ) ;
#98090 = CARTESIAN_POINT ( 'NONE',  ( -30.00000000000000000, 0.000000000000000000, -7.999999999999986677 ) ) ;
#98092 = AXIS2_PLACEMENT_3D ( 'NONE', #34754, #34218, #58464 ) ;
#98093 = ORIENTED_EDGE ( 'NONE', *, *, #81625, .T. ) ;
#98094 = ORIENTED_EDGE ( 'NONE', *, *, #93302, .F. ) ;
#98095 = VERTEX_POINT ( 'NONE', #99346 ) ;
#98096 = CARTESIAN_POINT ( 'NONE',  ( 29.62325201385431228, 328.1122814157980088, 15.64796472796876792 ) ) ;
#98097 = CARTESIAN_POINT ( 'NONE',  ( -6.073384266107519913, -15.26795065999669276, 14.38582946078376779 ) ) ;
#98098 = DIRECTION ( 'NONE',  ( 0.000000000000000000, 0.000000000000000000, 1.000000000000000000 ) ) ;
#98099 = EDGE_LOOP ( 'NONE', ( #15246, #96982, #69854, #32303 ) ) ;
#98100 = EDGE_CURVE ( 'NONE', #36949, #35464, #8763, .T. ) ;
#98101 = CARTESIAN_POINT ( 'NONE',  ( 37.33349330513379982, 4.000000000000003553, 0.000000000000000000 ) ) ;
#98102 = CARTESIAN_POINT ( 'NONE',  ( -113.4944653854903862, 14.17434517210798006, 56.74723269274519311 ) ) ;
#98103 = CARTESIAN_POINT ( 'NONE',  ( -9.999999999999998224, 15.00000000000000000, 1.836970198721029589E-15 ) ) ;
#98104 = CARTESIAN_POINT ( 'NONE',  ( -90.87004379432312362, -57.61277171722555579, 204.1615020926832358 ) ) ;
#98105 = CARTESIAN_POINT ( 'NONE',  ( 2.977408999572651815, -29.93750000204839523, 7.188101187500000933 ) ) ;
#98106 = CONICAL_SURFACE ( 'NONE', #86143, 4.000000000000001776, 0.9599310885968808105 ) ;
#98107 = CARTESIAN_POINT ( 'NONE',  ( -63.45785145800994798, 47.99999999999999289, -14.99006954567219196 ) ) ;
#98108 = CARTESIAN_POINT ( 'NONE',  ( -26.27902093981875709, 306.9027577142574614, -9.548073367147230428 ) ) ;
#98109 = DIRECTION ( 'NONE',  ( -0.2529971249647862130, 0.000000000000000000, -0.9674670303217327572 ) ) ;
#98110 = CARTESIAN_POINT ( 'NONE',  ( -64.67113474307254251, -14.21045842199435505, -28.81208810413780697 ) ) ;
#98111 = EDGE_CURVE ( 'NONE', #712, #25935, #72619, .T. ) ;
#98112 = CARTESIAN_POINT ( 'NONE',  ( -36.05833693101251214, -60.00000000000004263, 50.77755985414292184 ) ) ;
#98113 = CARTESIAN_POINT ( 'NONE',  ( -52.39849268324191200, -39.50851378549550930, 55.00951463007811526 ) ) ;
#98114 = PRESENTATION_LAYER_ASSIGNMENT (  '', '', ( #67182 ) ) ;
#98115 = CARTESIAN_POINT ( 'NONE',  ( 68.45015997180047407, 6.975173280561618775E-15, 0.000000000000000000 ) ) ;
#98116 = ORIENTED_EDGE ( 'NONE', *, *, #26587, .F. ) ;
#98117 = CARTESIAN_POINT ( 'NONE',  ( -100.2666838828567677, -52.75501491069231719, 194.0125142992028202 ) ) ;
#98118 = CARTESIAN_POINT ( 'NONE',  ( -2.922700453530358899, 295.7443989526400401, -10.00347189219610122 ) ) ;
#98119 = AXIS2_PLACEMENT_3D ( 'NONE', #103401, #104452, #64027 ) ;
#98120 = VERTEX_POINT ( 'NONE', #10353 ) ;
#98121 = CARTESIAN_POINT ( 'NONE',  ( -17.37648585630541120, 34.80701782457118298, -21.96231721963981443 ) ) ;
#98122 = CARTESIAN_POINT ( 'NONE',  ( 90.99775346010591193, -38.40525435722307179, -12.64124594595937090 ) ) ;
#98123 = CARTESIAN_POINT ( 'NONE',  ( 5.007715329123898279E-16, -7.505553499465175804, -6.177805531629075197 ) ) ;
#98124 = CARTESIAN_POINT ( 'NONE',  ( -37.56673239365863282, 25.75719283951018568, -10.95617127781023648 ) ) ;
#98125 = CARTESIAN_POINT ( 'NONE',  ( -15.88586298981787337, 294.5610647945437108, 1.875232895083775331 ) ) ;
#98126 = DIRECTION ( 'NONE',  ( 0.000000000000000000, 0.000000000000000000, 1.000000000000000000 ) ) ;
#98127 = CARTESIAN_POINT ( 'NONE',  ( 84.03711676261723085, -30.00000000000000000, 161.3372059342742943 ) ) ;
#98128 = CARTESIAN_POINT ( 'NONE',  ( 6.683837171061802529, 3.955946848495962787, 6.851900933636986935 ) ) ;
#98129 = CARTESIAN_POINT ( 'NONE',  ( -28.73053610125101542, 13.62316949804204569, 40.04352587319202428 ) ) ;
#98130 = CARTESIAN_POINT ( 'NONE',  ( 0.000000000000000000, -6.505213034913025026E-15, 0.000000000000000000 ) ) ;
#98131 = B_SPLINE_CURVE_WITH_KNOTS ( 'NONE', 3,
 ( #103860, #4121, #87170, #5185 ),
 .UNSPECIFIED., .F., .F.,
 ( 4, 4 ),
 ( 0.000000000000000000, 0.002002928617504379401 ),
 .UNSPECIFIED. ) ;
#98132 = ORIENTED_EDGE ( 'NONE', *, *, #48425, .T. ) ;
#98133 = VERTEX_POINT ( 'NONE', #75624 ) ;
#98134 = CARTESIAN_POINT ( 'NONE',  ( 49.98497805703834729, -18.73844719463555819, 43.94240058066204568 ) ) ;
#98135 = CARTESIAN_POINT ( 'NONE',  ( 5.662865377646750353, 41.84935275029727819, -58.94136771051215362 ) ) ;
#98136 = CARTESIAN_POINT ( 'NONE',  ( 36.48035061666895018, 28.19748189396849725, -11.58222015087291012 ) ) ;
#98137 = ORIENTED_EDGE ( 'NONE', *, *, #40286, .T. ) ;
#98138 = CARTESIAN_POINT ( 'NONE',  ( -108.1787983003200395, -38.35626379967903432, 139.1432696700099143 ) ) ;
#98139 = VERTEX_POINT ( 'NONE', #50284 ) ;
#98140 = DIRECTION ( 'NONE',  ( -1.000000000000000000, -1.224606353822377258E-16, -0.000000000000000000 ) ) ;
#98141 = CARTESIAN_POINT ( 'NONE',  ( 90.86182427071091183, -38.35175685699187653, 20.64787121975910367 ) ) ;
#98142 = CARTESIAN_POINT ( 'NONE',  ( 11.12482241898927349, 19.59647781357509899, -8.686708111164573864 ) ) ;
#98143 = CARTESIAN_POINT ( 'NONE',  ( -36.74627714604517337, 26.01170350572267154, -11.25947311975635223 ) ) ;
#98144 = CARTESIAN_POINT ( 'NONE',  ( 98.81654218035373560, -52.71701439775952025, 115.6172114277043050 ) ) ;
#98145 = CARTESIAN_POINT ( 'NONE',  ( -31.67837264767364402, 439.4052006294236890, 23.39994154329854226 ) ) ;
#98146 = CARTESIAN_POINT ( 'NONE',  ( 22.46054152223527467, 27.61307239794278345, 32.95409374511044831 ) ) ;
#98147 = CARTESIAN_POINT ( 'NONE',  ( -33.28951410023742596, 318.6302480808201381, -6.419669330273621632 ) ) ;
#98148 = DIRECTION ( 'NONE',  ( 0.000000000000000000, -1.000000000000000000, 0.000000000000000000 ) ) ;
#98149 = CARTESIAN_POINT ( 'NONE',  ( 74.92543916372812873, -60.00000000000000711, 180.6976430414843833 ) ) ;
#98150 = CARTESIAN_POINT ( 'NONE',  ( 17.53356643429805573, 45.00000000000002842, 63.42504839209897938 ) ) ;
#98151 = ORIENTED_EDGE ( 'NONE', *, *, #24278, .T. ) ;
#98152 = CARTESIAN_POINT ( 'NONE',  ( 56.07231050077595569, -49.90802284892470908, 67.05805815868586706 ) ) ;
#98153 = CARTESIAN_POINT ( 'NONE',  ( -26.03744394287809882, 295.8532420388733044, -9.784778624385232604 ) ) ;
#98154 = FACE_OUTER_BOUND ( 'NONE', #67343, .T. ) ;
#98155 = ADVANCED_FACE ( 'NONE', ( #1727 ), #26595, .F. ) ;
#98156 = AXIS2_PLACEMENT_3D ( 'NONE', #106606, #16541, #56451 ) ;
#98157 = CARTESIAN_POINT ( 'NONE',  ( -9.402149768019080867, -5.000000000000001776, -18.95237023718975422 ) ) ;
#98159 = CARTESIAN_POINT ( 'NONE',  ( -9.269408785705698151, -52.95403500424551169, 23.24750950774772562 ) ) ;
#98158 = CARTESIAN_POINT ( 'NONE',  ( -80.04809061299876305, -30.00000000001593392, 190.5044041146019538 ) ) ;
#98160 = DIRECTION ( 'NONE',  ( 0.000000000000000000, 0.000000000000000000, -1.000000000000000000 ) ) ;
#98161 = CARTESIAN_POINT ( 'NONE',  ( 23.52633860068766225, 305.9421485136137449, 9.176037288099113454 ) ) ;
#98162 = CARTESIAN_POINT ( 'NONE',  ( -43.00000000000000000, 464.8825480873695710, 15.07585856869432206 ) ) ;
#98163 = CIRCLE ( 'NONE', #24137, 35.82893434829263413 ) ;
#98164 = CARTESIAN_POINT ( 'NONE',  ( -8.000000000000000000, -34.24999999999999289, -9.797174393178825657E-16 ) ) ;
#98165 = EDGE_CURVE ( 'NONE', #12822, #31480, #97187, .T. ) ;
#98166 =( GEOMETRIC_REPRESENTATION_CONTEXT ( 3 ) GLOBAL_UNCERTAINTY_ASSIGNED_CONTEXT ( ( #76364 ) ) GLOBAL_UNIT_ASSIGNED_CONTEXT ( ( #44633, #68371, #10635 ) ) REPRESENTATION_CONTEXT ( 'NONE', 'WORKASPACE' ) );
#98167 = EDGE_CURVE ( 'NONE', #40315, #12958, #104116, .T. ) ;
#98168 = CARTESIAN_POINT ( 'NONE',  ( -33.21174982058442282, 465.5907685032092331, 15.87814633360742178 ) ) ;
#98169 = ORIENTED_EDGE ( 'NONE', *, *, #66298, .F. ) ;
#98170 = CARTESIAN_POINT ( 'NONE',  ( 82.89656108765285580, -46.49426597450035104, 178.9984722453477275 ) ) ;
#98171 = LINE ( 'NONE', #24325, #89497 ) ;
#98172 = CARTESIAN_POINT ( 'NONE',  ( -38.91012333415075375, 438.0862499651277631, 23.13793682581813371 ) ) ;
#98173 = ORIENTED_EDGE ( 'NONE', *, *, #27739, .T. ) ;
#98174 = DIRECTION ( 'NONE',  ( 0.000000000000000000, 1.000000000000000000, 0.000000000000000000 ) ) ;
#98176 = EDGE_CURVE ( 'NONE', #92586, #34646, #21465, .T. ) ;
#98175 = VECTOR ( 'NONE', #14895, 1000.000000000000000 ) ;
#98177 = CARTESIAN_POINT ( 'NONE',  ( 5.076160773007416083, -4.320849473519435158, -17.10810059243997472 ) ) ;
#98178 = CARTESIAN_POINT ( 'NONE',  ( 0.000000000000000000, 274.9999999999999432, 0.000000000000000000 ) ) ;
#98179 = FILL_AREA_STYLE ('',( #31877 ) ) ;
#98180 = CARTESIAN_POINT ( 'NONE',  ( -35.64423825752726316, 42.51604778590805722, -61.49727402875218019 ) ) ;
#98181 = CARTESIAN_POINT ( 'NONE',  ( -28.98512335478656610, 9.657432045445705882, -41.89946025606985813 ) ) ;
#98182 =( GEOMETRIC_REPRESENTATION_CONTEXT ( 3 ) GLOBAL_UNCERTAINTY_ASSIGNED_CONTEXT ( ( #90485 ) ) GLOBAL_UNIT_ASSIGNED_CONTEXT ( ( #54746, #103326, #80616 ) ) REPRESENTATION_CONTEXT ( 'NONE', 'WORKASPACE' ) );
#98183 = VECTOR ( 'NONE', #93434, 1000.000000000000227 ) ;
#98184 = CARTESIAN_POINT ( 'NONE',  ( 6.500000000000597744, 2.679956093905103920, -6.238387772031950718 ) ) ;
#98185 = CARTESIAN_POINT ( 'NONE',  ( 14.54015256618498242, 142.2617268803927288, -5.000000000000000000 ) ) ;
#98187 = CARTESIAN_POINT ( 'NONE',  ( -11.46642418865753754, 14.78850670498192166, -9.842947063719719836 ) ) ;
#98186 = CARTESIAN_POINT ( 'NONE',  ( -8.717155287858316726, -19.71234147751727761, 35.28392597056648583 ) ) ;
#98188 = AXIS2_PLACEMENT_3D ( 'NONE', #27217, #75720, #85972 ) ;
#98189 = CARTESIAN_POINT ( 'NONE',  ( -7.188101187500002709, -12.31250000204838635, 2.977408999572648707 ) ) ;
#98190 = CARTESIAN_POINT ( 'NONE',  ( -51.78317192877783981, 40.83906611472826853, 39.73656039209301838 ) ) ;
#98191 = CARTESIAN_POINT ( 'NONE',  ( 34.10284876471455817, 1.482358050883964840E-15, 0.000000000000000000 ) ) ;
#98192 = CIRCLE ( 'NONE', #80944, 2.999999999999987121 ) ;
#98193 = EDGE_LOOP ( 'NONE', ( #54987, #18584, #85114, #36836, #94456 ) ) ;
#98194 = CARTESIAN_POINT ( 'NONE',  ( -17.50000000000251887, 49.98040874965850122, 61.78610620011964016 ) ) ;
#98195 = DIRECTION ( 'NONE',  ( -0.3845251595717362192, -0.02506431005118274144, -0.9227741771516956293 ) ) ;
#98196 = CARTESIAN_POINT ( 'NONE',  ( -7.939742226425032356, 97.07168777238570101, -5.000000000007622347 ) ) ;
#98197 = CARTESIAN_POINT ( 'NONE',  ( -9.500000025475724641, -4.999999999999998224, -69.85526497430338111 ) ) ;
#98198 = CARTESIAN_POINT ( 'NONE',  ( 26.36650669486618881, 1.474610560812782335E-15, 0.000000000000000000 ) ) ;
#98199 = EDGE_CURVE ( 'NONE', #35444, #68049, #65001, .T. ) ;
#98200 = ORIENTED_EDGE ( 'NONE', *, *, #91986, .T. ) ;
#98201 = CARTESIAN_POINT ( 'NONE',  ( -4.503026011213025370, -85.54341862283318676, 3.965236350746919047 ) ) ;
#98202 = DIRECTION ( 'NONE',  ( 0.000000000000000000, 0.000000000000000000, 1.000000000000000000 ) ) ;
#98203 = ORIENTED_EDGE ( 'NONE', *, *, #81227, .T. ) ;
#98204 = VECTOR ( 'NONE', #84406, 1000.000000000000000 ) ;
#98205 = EDGE_CURVE ( 'NONE', #17856, #73615, #53486, .T. ) ;
#98206 = B_SPLINE_CURVE_WITH_KNOTS ( 'NONE', 3,
 ( #24216, #15016, #6390, #23147, #48964, #88398, #57066, #16084, #54939, #72204, #81862, #7987, #105108, #97007, #104029, #95960, #22084, #46861, #66773, #920, #58137, #43031, #34444, #66228, #92098, #74317, #99661, #42485 ),
 .UNSPECIFIED., .F., .F.,
 ( 4, 2, 2, 2, 2, 2, 2, 2, 2, 2, 2, 2, 2, 4 ),
 ( 0.07710222747882937433, 0.08159137518423913160, 0.08383594903694401024, 0.08608052288964888887, 0.09056967059505866002, 0.09505881830046841729, 0.1040371137112879457, 0.1130154091221074741, 0.1219937045329270164, 0.1309719999437465587, 0.1354611476491563160, 0.1399502953545660733, 0.1444394430599758306, 0.1489285907653855878 ),
 .UNSPECIFIED. ) ;
#98207 = CARTESIAN_POINT ( 'NONE',  ( -7.199040112754230057E-19, 54.30758622938872549, -7.749999999999999112 ) ) ;
#98208 = CARTESIAN_POINT ( 'NONE',  ( 8.572527594031465301E-16, 0.000000000000000000, 6.999999999999993783 ) ) ;
#98209 = CARTESIAN_POINT ( 'NONE',  ( -99.55134491157069476, -60.00000000000000000, 78.35702824496748065 ) ) ;
#98210 = CARTESIAN_POINT ( 'NONE',  ( 28.88608732843768223, 18.87339843927420091, -39.88959139356639838 ) ) ;
#98211 = CARTESIAN_POINT ( 'NONE',  ( 9.183192031130861521E-06, -29.03115897286976832, 28.72817645508066775 ) ) ;
#98212 = CARTESIAN_POINT ( 'NONE',  ( 22.42417502586373246, 305.3961751430792333, 10.05444931189341773 ) ) ;
#98213 = CARTESIAN_POINT ( 'NONE',  ( -32.87547266101637433, 465.6993878536673606, 10.91512469976170330 ) ) ;
#98215 = CARTESIAN_POINT ( 'NONE',  ( 32.06550094448246568, 486.4396568316712433, 6.103009648082660554 ) ) ;
#98214 = CARTESIAN_POINT ( 'NONE',  ( 3.140974613991526887, -5.000000000000002665, -96.68767211932356531 ) ) ;
#98216 = B_SPLINE_CURVE_WITH_KNOTS ( 'NONE', 3,
 ( #49133, #81489, #73407, #80444, #56145, #7090 ),
 .UNSPECIFIED., .F., .F.,
 ( 4, 2, 4 ),
 ( 0.000000000000000000, 0.001670251840623334597, 0.003340503681246669195 ),
 .UNSPECIFIED. ) ;
#98217 = CARTESIAN_POINT ( 'NONE',  ( -83.59314024080309480, -39.46891138312180658, 175.2148047660766679 ) ) ;
#98218 = ORIENTED_EDGE ( 'NONE', *, *, #45381, .F. ) ;
#98219 = CARTESIAN_POINT ( 'NONE',  ( 7.500000000000005329, 42.83333333333328596, -68.91429205785459544 ) ) ;
#98220 = ORIENTED_EDGE ( 'NONE', *, *, #19748, .F. ) ;
#98221 = VERTEX_POINT ( 'NONE', #20647 ) ;
#98222 = LINE ( 'NONE', #58850, #37149 ) ;
#98223 = DIRECTION ( 'NONE',  ( 0.000000000000000000, 0.000000000000000000, 1.000000000000000000 ) ) ;
#98224 = EDGE_CURVE ( 'NONE', #25084, #22876, #36806, .T. ) ;
#98225 = CIRCLE ( 'NONE', #5242, 5.000000000000001776 ) ;
#98226 = CARTESIAN_POINT ( 'NONE',  ( 2.019483917365790222E-25, 303.8518027762758038, 9.936999415352289589 ) ) ;
#98227 = FACE_OUTER_BOUND ( 'NONE', #1751, .T. ) ;
#98228 = CARTESIAN_POINT ( 'NONE',  ( -7.002990960197235104, -63.94733181616542339, 3.868040364119525343 ) ) ;
#98229 = CARTESIAN_POINT ( 'NONE',  ( 8.441132293785429397, 28.00851920974988118, -1.228519433277404106E-12 ) ) ;
#98230 = CARTESIAN_POINT ( 'NONE',  ( -11.76475894966304026, -5.000000000000000888, -79.34634670506437715 ) ) ;
#98231 = CARTESIAN_POINT ( 'NONE',  ( -43.75401118688380819, 486.3173572309548263, 5.908089951475190560 ) ) ;
#98232 = CARTESIAN_POINT ( 'NONE',  ( 104.4271199315001013, -14.21045842199428932, 141.4133776126798523 ) ) ;
#98233 = AXIS2_PLACEMENT_3D ( 'NONE', #54147, #88664, #29406 ) ;
#98234 = EDGE_CURVE ( 'NONE', #57343, #99482, #92879, .T. ) ;
#98235 = CARTESIAN_POINT ( 'NONE',  ( -104.7861223705664599, -14.21045842199442433, 190.1679628257406875 ) ) ;
#98236 = CARTESIAN_POINT ( 'NONE',  ( -63.02399650324780112, -22.10761227753726743, 71.83296306885770832 ) ) ;
#98237 = ORIENTED_EDGE ( 'NONE', *, *, #62637, .T. ) ;
#98238 = CARTESIAN_POINT ( 'NONE',  ( -43.03265099499957813, 484.2747968070553384, -0.8099405866661226749 ) ) ;
#98239 = CARTESIAN_POINT ( 'NONE',  ( 112.1647626997707192, -60.00000000000001421, 192.1852754171339654 ) ) ;
#98240 = CIRCLE ( 'NONE', #5252, 3.309500000000001663 ) ;
#98241 = VERTEX_POINT ( 'NONE', #28184 ) ;
#98242 = CARTESIAN_POINT ( 'NONE',  ( -2.304441091496778042E-06, -22.06731698597467428, 27.56753612393148956 ) ) ;
#98243 = CARTESIAN_POINT ( 'NONE',  ( 2.977408999572652260, -15.31250000204838813, 7.188101187500000044 ) ) ;
#98244 = EDGE_CURVE ( 'NONE', #87879, #92559, #98950, .T. ) ;
#98245 = CARTESIAN_POINT ( 'NONE',  ( -6.390201886731505354, 51.65431772680223332, 6.607700835476884471 ) ) ;
#98246 = ORIENTED_EDGE ( 'NONE', *, *, #84912, .T. ) ;
#98247 = CARTESIAN_POINT ( 'NONE',  ( 6.249999999999998224, 9.237604307034018802, 0.000000000000000000 ) ) ;
#98248 = ORIENTED_EDGE ( 'NONE', *, *, #104320, .T. ) ;
#98249 = DIRECTION ( 'NONE',  ( 0.000000000000000000, -0.9238632370064382426, 0.3827227708250269256 ) ) ;
#98250 = CARTESIAN_POINT ( 'NONE',  ( 5.082755093536325930, -29.84375000204838813, -5.082755093536325042 ) ) ;
#98251 = CARTESIAN_POINT ( 'NONE',  ( -107.0982019125352593, -60.00000000000001421, 196.9758988471260182 ) ) ;
#98252 = CARTESIAN_POINT ( 'NONE',  ( 9.204611235795193025, -55.29781778581994445, 30.90985867601607850 ) ) ;
#98253 = CARTESIAN_POINT ( 'NONE',  ( -5.082755093536325042, -29.46875000204838813, -5.082755093536325930 ) ) ;
#98254 = VECTOR ( 'NONE', #77474, 1000.000000000000227 ) ;
#98255 = CARTESIAN_POINT ( 'NONE',  ( 105.5720000000000312, 0.000000000000000000, 0.000000000000000000 ) ) ;
#98256 = CARTESIAN_POINT ( 'NONE',  ( 17.71899192986533222, 43.32325553723746481, -4.750071910800272690 ) ) ;
#98257 = CARTESIAN_POINT ( 'NONE',  ( -6.518111695417504237, 53.49350304183202809, -7.567621837673542018 ) ) ;
#98258 = CARTESIAN_POINT ( 'NONE',  ( 1.000000000000000000, -15.67194501421539599, -10.31047629133078480 ) ) ;
#98259 = AXIS2_PLACEMENT_3D ( 'NONE', #90314, #64978, #16422 ) ;
#98260 = PRESENTATION_STYLE_ASSIGNMENT (( #24930 ) ) ;
#98261 = CARTESIAN_POINT ( 'NONE',  ( -22.87160824404999815, 295.0982458469678136, -1.947616908246118106 ) ) ;
#98262 = CARTESIAN_POINT ( 'NONE',  ( 106.1377881480577088, -60.00000000000000000, 180.8750096036389436 ) ) ;
#98263 = CARTESIAN_POINT ( 'NONE',  ( -33.15903214888006545, -56.84432955689586464, 37.61496284774349874 ) ) ;
#98264 = B_SPLINE_CURVE_WITH_KNOTS ( 'NONE', 3,
 ( #70498, #87214, #38666, #71533, #20407, #21962 ),
 .UNSPECIFIED., .F., .F.,
 ( 4, 2, 4 ),
 ( 0.000000000000000000, 0.0003910247833730985559, 0.0007820495667461968949 ),
 .UNSPECIFIED. ) ;
#98265 = AXIS2_PLACEMENT_3D ( 'NONE', #25692, #84421, #45951 ) ;
#98266 = CARTESIAN_POINT ( 'NONE',  ( 40.03051666693097133, -36.06173267250149905, 37.97872145570595137 ) ) ;
#98267 = SURFACE_SIDE_STYLE ('',( #9775 ) ) ;
#98268 = VERTEX_POINT ( 'NONE', #61057 ) ;
#98269 = CARTESIAN_POINT ( 'NONE',  ( 43.77664590664291211, 434.3717993398995532, 11.97532627841538755 ) ) ;
#98270 = CONICAL_SURFACE ( 'NONE', #67331, 3.309500000000001663, 0.9599310885968770357 ) ;
#98271 = CARTESIAN_POINT ( 'NONE',  ( -81.56573377466280306, -38.84171562881364537, 195.3582572410830096 ) ) ;
#98272 = ORIENTED_EDGE ( 'NONE', *, *, #104253, .F. ) ;
#98274 = CARTESIAN_POINT ( 'NONE',  ( 42.09210974227526947, 317.4093497706929270, -4.557617623460385126 ) ) ;
#98273 = DIRECTION ( 'NONE',  ( -1.000000000000000000, -1.224606353822377258E-16, -0.000000000000000000 ) ) ;
#98275 = CARTESIAN_POINT ( 'NONE',  ( -10.99305341285137771, 19.22662180895261486, -8.903504237805147881 ) ) ;
#98276 = B_SPLINE_CURVE_WITH_KNOTS ( 'NONE', 3,
 ( #38709, #89378, #9354, #14930 ),
 .UNSPECIFIED., .F., .F.,
 ( 4, 4 ),
 ( 3.469446951953614189E-18, 0.001842998688485824764 ),
 .UNSPECIFIED. ) ;
#98277 = CARTESIAN_POINT ( 'NONE',  ( -38.51502786940066869, 460.6916007118362018, 1.299075388248767116 ) ) ;
#98278 = CARTESIAN_POINT ( 'NONE',  ( 6.585304040558099814, -4.021874164301465271, 6.499999999999999112 ) ) ;
#98279 = CARTESIAN_POINT ( 'NONE',  ( 0.000000000000000000, 0.000000000000000000, 0.000000000000000000 ) ) ;
#98280 = CARTESIAN_POINT ( 'NONE',  ( -40.32369798409565931, 437.3250542437391459, 5.179402639112346662 ) ) ;
#98281 = CARTESIAN_POINT ( 'NONE',  ( -28.24509918527273555, 316.3792769537042773, 11.76181215083657250 ) ) ;
#98282 = DIRECTION ( 'NONE',  ( 0.000000000000000000, 1.000000000000000000, 0.000000000000000000 ) ) ;
#98283 = MECHANICAL_DESIGN_GEOMETRIC_PRESENTATION_REPRESENTATION (  '', ( #38036 ), #34568 ) ;
#98284 = CARTESIAN_POINT ( 'NONE',  ( 110.0488610262806048, -60.00000000000001421, 143.8402947968523904 ) ) ;
#98285 = CARTESIAN_POINT ( 'NONE',  ( 64.78349330513380266, 6.975173280561618775E-15, 0.000000000000000000 ) ) ;
#98286 = VERTEX_POINT ( 'NONE', #95533 ) ;
#98287 = EDGE_CURVE ( 'NONE', #7125, #50869, #4399, .T. ) ;
#98288 = CARTESIAN_POINT ( 'NONE',  ( -86.48208369142494689, -30.00000000000002132, 181.4558340259839895 ) ) ;
#98289 = EDGE_LOOP ( 'NONE', ( #91096, #51738, #13876, #66401, #1982 ) ) ;
#98290 = CARTESIAN_POINT ( 'NONE',  ( -18.99999999999999289, -5.000000000000000000, 25.00000000000000000 ) ) ;
#98291 = CARTESIAN_POINT ( 'NONE',  ( -15.85122647056153156, 4.114663126756375355, -4.288211754877433002 ) ) ;
#98292 = FILL_AREA_STYLE_COLOUR ( '', #12649 ) ;
#98293 = DIRECTION ( 'NONE',  ( -1.000000000000000000, -1.224606353822377258E-16, -0.000000000000000000 ) ) ;
#98294 = CARTESIAN_POINT ( 'NONE',  ( -22.10829536976837417, 28.16405687208418129, -31.35662012625487804 ) ) ;
#98295 = CARTESIAN_POINT ( 'NONE',  ( -2.977408999572650039, -23.56250000204839168, -7.188101187500001821 ) ) ;
#98296 = MECHANICAL_DESIGN_GEOMETRIC_PRESENTATION_REPRESENTATION (  '', ( #31119 ), #84533 ) ;
#98297 = SURFACE_STYLE_USAGE ( .BOTH. , #58370 ) ;
#98298 = CARTESIAN_POINT ( 'NONE',  ( 7.251642494156181229, 41.54835750584383192, -68.91429206127320128 ) ) ;
#98299 = EDGE_CURVE ( 'NONE', #29166, #15460, #69647, .T. ) ;
#98300 = ORIENTED_EDGE ( 'NONE', *, *, #93967, .F. ) ;
#98301 = EDGE_CURVE ( 'NONE', #75752, #18205, #16272, .T. ) ;
#98302 = AXIS2_PLACEMENT_3D ( 'NONE', #62484, #86245, #45243 ) ;
#98303 =( REPRESENTATION_RELATIONSHIP ('NONE','NONE', #69581, #22031 ) REPRESENTATION_RELATIONSHIP_WITH_TRANSFORMATION ( #105235 )SHAPE_REPRESENTATION_RELATIONSHIP( ) );
#98305 = ORIENTED_EDGE ( 'NONE', *, *, #64330, .T. ) ;
#98304 = CARTESIAN_POINT ( 'NONE',  ( -7.439204957583139155, 40.67212726423260705, -59.07661279408126376 ) ) ;
#98306 = CARTESIAN_POINT ( 'NONE',  ( 82.86123803554382050, -22.15437991950470931, 144.5942242259914394 ) ) ;
#98307 = CARTESIAN_POINT ( 'NONE',  ( 57.70539558375507738, 4.000000000000015099, 4.898587196589422689E-16 ) ) ;
#98308 = CARTESIAN_POINT ( 'NONE',  ( 9.333555687487612218, 86.78102696608972622, 3.591168747312686982 ) ) ;
#98309 = EDGE_LOOP ( 'NONE', ( #62132, #20476, #85261, #12555, #14276 ) ) ;
#98310 = CARTESIAN_POINT ( 'NONE',  ( -19.50010530980351220, 50.00000000000000000, 59.90637122617393828 ) ) ;
#98311 = ADVANCED_FACE ( 'NONE', ( #78282 ), #86903, .F. ) ;
#98312 = CARTESIAN_POINT ( 'NONE',  ( 12.49989493515518646, 18.64301898209307140, -36.27145154709465658 ) ) ;
#98313 = CARTESIAN_POINT ( 'NONE',  ( -1.320432766682874540E-15, -12.03125000204838635, 7.188101187500000044 ) ) ;
#98314 = CARTESIAN_POINT ( 'NONE',  ( 6.943482370013980720, 29.47151629739275691, 3.973876482044365499 ) ) ;
#98315 = DIRECTION ( 'NONE',  ( 0.000000000000000000, 0.000000000000000000, -1.000000000000000000 ) ) ;
#98316 = DIRECTION ( 'NONE',  ( -0.000000000000000000, -1.000000000000000000, -0.000000000000000000 ) ) ;
#98317 = CARTESIAN_POINT ( 'NONE',  ( -33.05273490460238861, 434.2935873781336795, 15.73821027039317855 ) ) ;
#98318 = ORIENTED_EDGE ( 'NONE', *, *, #96973, .F. ) ;
#98319 = CIRCLE ( 'NONE', #84547, 7.500000000001509015 ) ;
#98320 = AXIS2_PLACEMENT_3D ( 'NONE', #4633, #38602, #87149 ) ;
#98321 = DIRECTION ( 'NONE',  ( 0.000000000000000000, -1.000000000000000000, 0.000000000000000000 ) ) ;
#98322 = FACE_OUTER_BOUND ( 'NONE', #2468, .T. ) ;
#98323 = DIRECTION ( 'NONE',  ( 0.000000000000000000, 1.000000000000000000, 0.000000000000000000 ) ) ;
#98324 = ORIENTED_EDGE ( 'NONE', *, *, #91659, .T. ) ;
#98325 = CARTESIAN_POINT ( 'NONE',  ( 4.401442555609581635E-16, -32.28125000204838813, -7.188101187500000044 ) ) ;
#98326 = CARTESIAN_POINT ( 'NONE',  ( 29.70662014929110839, -32.25496426234150249, 40.40754308457954380 ) ) ;
#98327 = CARTESIAN_POINT ( 'NONE',  ( 4.000000000000000000, 4.898587196589412829E-16, -1.161000000000000032 ) ) ;
#98328 = DIRECTION ( 'NONE',  ( 0.000000000000000000, -1.000000000000000000, 0.000000000000000000 ) ) ;
#98329 = CARTESIAN_POINT ( 'NONE',  ( 39.41877109955689917, 438.9233561163386526, 23.32050101277916454 ) ) ;
#98330 = APPLICATION_PROTOCOL_DEFINITION ( 'draft international standard', 'automotive_design', 1998, #82395 ) ;
#98331 = CARTESIAN_POINT ( 'NONE',  ( 49.10020235979921921, 7.817788915495893498, 16.25178062802444146 ) ) ;
#98332 = ORIENTED_EDGE ( 'NONE', *, *, #26697, .F. ) ;
#98333 = DIRECTION ( 'NONE',  ( 0.000000000000000000, 0.000000000000000000, 1.000000000000000000 ) ) ;
#98334 = CARTESIAN_POINT ( 'NONE',  ( 13.20204525318317401, 42.70098935138261709, -92.35018848971670025 ) ) ;
#98335 = VECTOR ( 'NONE', #93123, 1000.000000000000000 ) ;
#98336 = DIRECTION ( 'NONE',  ( -1.000000000000000000, -1.224606353822377258E-16, -0.000000000000000000 ) ) ;
#98337 = DIRECTION ( 'NONE',  ( 0.000000000000000000, 0.000000000000000000, 1.000000000000000000 ) ) ;
#98338 = ORIENTED_EDGE ( 'NONE', *, *, #45609, .T. ) ;
#98339 = VECTOR ( 'NONE', #65718, 1000.000000000000000 ) ;
#98340 = CARTESIAN_POINT ( 'NONE',  ( 5.656854249492378806, -9.875000004096769146, 5.656854249492381470 ) ) ;
#98341 = CARTESIAN_POINT ( 'NONE',  ( 102.6741165558615450, -57.67098198743860138, 85.02274040594497251 ) ) ;
#98342 = CONICAL_SURFACE ( 'NONE', #51836, 3.309499999999999886, 0.7853981633974407295 ) ;
#98343 = EDGE_CURVE ( 'NONE', #25185, #18921, #82947, .T. ) ;
#98345 = CARTESIAN_POINT ( 'NONE',  ( 34.83844953170066816, 463.9146721063449377, 18.82558425661361667 ) ) ;
#98344 = CONICAL_SURFACE ( 'NONE', #46610, 4.000000000000001776, 0.9599310885968808105 ) ;
#98346 = CARTESIAN_POINT ( 'NONE',  ( 4.000000000000001776, 17.58240661545486105, 5.744562646538042827 ) ) ;
#98347 = DIRECTION ( 'NONE',  ( 0.000000000000000000, 0.000000000000000000, -1.000000000000000000 ) ) ;
#98348 = CARTESIAN_POINT ( 'NONE',  ( 63.56127108291158123, -4.000000000000000888, 4.898587196589422689E-16 ) ) ;
#98349 = CARTESIAN_POINT ( 'NONE',  ( -73.88487227173887106, -60.00000000000001421, 171.0524701157142999 ) ) ;
#98350 = CARTESIAN_POINT ( 'NONE',  ( -22.91651842568168362, 295.0901107613288445, -9.949346074078583513 ) ) ;
#98351 = CARTESIAN_POINT ( 'NONE',  ( -32.35336999986095208, 300.6590557721156642, 11.25190399080426751 ) ) ;
#98352 = CARTESIAN_POINT ( 'NONE',  ( -83.75545966347903004, -61.02389094001022585, 191.9544639385318590 ) ) ;
#98353 = ORIENTED_EDGE ( 'NONE', *, *, #51386, .T. ) ;
#98354 = CARTESIAN_POINT ( 'NONE',  ( 30.88074124778558271, 314.2284791753184550, -6.769356187408334335 ) ) ;
#98355 = EDGE_LOOP ( 'NONE', ( #62884, #15362, #96266, #2653, #44843 ) ) ;
#98357 = ADVANCED_FACE ( 'NONE', ( #24330 ), #64497, .T. ) ;
#98356 = LINE ( 'NONE', #16923, #16473 ) ;
#98358 = DIRECTION ( 'NONE',  ( 0.000000000000000000, -1.000000000000000000, 0.000000000000000000 ) ) ;
#98359 = CARTESIAN_POINT ( 'NONE',  ( -83.25986436703819038, -37.78524753907071698, -7.278281021959687180 ) ) ;
#98360 = CARTESIAN_POINT ( 'NONE',  ( 4.999999999999995559, -50.00000000000000000, 40.07669683062201926 ) ) ;
#98361 = SURFACE_SIDE_STYLE ('',( #72491 ) ) ;
#98362 = VERTEX_POINT ( 'NONE', #47498 ) ;
#98363 = AXIS2_PLACEMENT_3D ( 'NONE', #63916, #80594, #31557 ) ;
#98364 = DIRECTION ( 'NONE',  ( 0.000000000000000000, 0.9371777605526924182, 0.3488521823429523994 ) ) ;
#98365 = CARTESIAN_POINT ( 'NONE',  ( 17.01589776168603407, -1.734723475976807094E-15, -2.227375807149030162 ) ) ;
#98366 = CARTESIAN_POINT ( 'NONE',  ( -34.62305774441605166, 437.4305192986070665, 5.012907847576948406 ) ) ;
#98367 = CARTESIAN_POINT ( 'NONE',  ( -16.35184830034500791, -14.21045842199432663, -36.83529024868766300 ) ) ;
#98368 = AXIS2_PLACEMENT_3D ( 'NONE', #90465, #51051, #91547 ) ;
#98369 = CARTESIAN_POINT ( 'NONE',  ( -75.40408572285984690, -56.85084406233583110, 136.0574973080508983 ) ) ;
#98370 = VERTEX_POINT ( 'NONE', #57177 ) ;
#98371 = CARTESIAN_POINT ( 'NONE',  ( 37.62958953315902022, -14.21045842199429288, 41.24408864243086015 ) ) ;
#98372 = CARTESIAN_POINT ( 'NONE',  ( 6.928203230275509661, 85.26479267253573369, 3.999999999999999112 ) ) ;
#98373 = CARTESIAN_POINT ( 'NONE',  ( 100.8522003986677475, -57.67122939875248022, 74.21107199178662484 ) ) ;
#98374 = ORIENTED_EDGE ( 'NONE', *, *, #52882, .T. ) ;
#98375 = DIRECTION ( 'NONE',  ( 0.000000000000000000, -1.000000000000000000, 0.000000000000000000 ) ) ;
#98376 = EDGE_CURVE ( 'NONE', #74189, #9380, #74784, .T. ) ;
#98377 = CARTESIAN_POINT ( 'NONE',  ( 6.928203230275510549, 85.00000000000000000, 4.000000000000000000 ) ) ;
#98378 = ORIENTED_EDGE ( 'NONE', *, *, #85655, .F. ) ;
#98379 = DIRECTION ( 'NONE',  ( 0.000000000000000000, 0.000000000000000000, 1.000000000000000000 ) ) ;
#98380 = CARTESIAN_POINT ( 'NONE',  ( -7.188101187500000044, -21.40625000204838457, -8.802885111219163269E-16 ) ) ;
#98381 = DIRECTION ( 'NONE',  ( 0.000000000000000000, -0.4999999999999991673, 0.8660254037844390407 ) ) ;
#98382 =( BOUNDED_SURFACE ( )  B_SPLINE_SURFACE ( 2, 3, ( 
 ( #56938, #96895, #79636, #6266, #48319, #6809, #71538, #15431, #39204, #105509, #15967, #72605, #104441, #32714, #89860, #64533, #106563, #81213, #65583, #72081, #23029, #39727, #65050, #89339, #24621, #55863, #23560, #40240, #22510, #97946 ),
 ( #14891, #98468, #47786, #73116, #80689, #13834, #24096, #48845, #81738, #5753, #31649, #56404, #97398, #106021, #38674, #7861, #40768, #7328, #57469, #32167, #73659, #46746, #30591, #96380, #55350, #88278, #60047, #11984, #90933, #43825 ),
 ( #58008, #17045, #98989, #68101, #33236, #8401, #85356, #82828, #41304, #36843, #76187, #92906, #36320, #60571, #44369, #49920, #28221, #74190, #102062, #69710, #90392, #25152, #269, #93461, #2830, #66110, #3911, #35784, #10906, #3378 ) ),
 .UNSPECIFIED., .F., .F., .F. ) 
 B_SPLINE_SURFACE_WITH_KNOTS ( ( 3, 3 ),
 ( 4, 2, 2, 2, 2, 2, 2, 2, 2, 2, 2, 2, 2, 2, 4 ),
 ( 0.000000000000000000, 1.000000000000000000 ),
 ( 0.000000000000000000, 0.0008794597212711405482, 0.001758919442542281096, 0.002638379163813421753, 0.003078109024448992190, 0.003517838885084562193, 0.003957568745720132196, 0.004397298606355702633, 0.005276758327626843506, 0.006156218048897984380, 0.006595947909533553949, 0.006650914142113000145, 0.006705880374692446341, 0.006815812839851338734, 0.007035677770169124386 ),
 .UNSPECIFIED. ) 
 GEOMETRIC_REPRESENTATION_ITEM ( )  RATIONAL_B_SPLINE_SURFACE ( (
 ( 1.000000000000000000, 1.000000000000000000, 1.000000000000000000, 1.000000000000000000, 1.000000000000000000, 1.000000000000000000, 1.000000000000000000, 1.000000000000000000, 1.000000000000000000, 1.000000000000000000, 1.000000000000000000, 1.000000000000000000, 1.000000000000000000, 1.000000000000000000, 1.000000000000000000, 1.000000000000000000, 1.000000000000000000, 1.000000000000000000, 1.000000000000000000, 1.000000000000000000, 1.000000000000000000, 1.000000000000000000, 1.000000000000000000, 1.000000000000000000, 1.000000000000000000, 1.000000000000000000, 1.000000000000000000, 1.000000000000000000, 1.000000000000000000, 1.000000000000000000),
 ( 1.857142857142858317, 1.857142857142858317, 1.857142857142858317, 1.857142857142858317, 1.857142857142858317, 1.857142857142858317, 1.857142857142858317, 1.857142857142858317, 1.857142857142858317, 1.857142857142858317, 1.857142857142858317, 1.857142857142858317, 1.857142857142858317, 1.857142857142858317, 1.857142857142858317, 1.857142857142858317, 1.857142857142858317, 1.857142857142858317, 1.857142857142858317, 1.857142857142858317, 1.857142857142858317, 1.857142857142858317, 1.857142857142858317, 1.857142857142858317, 1.857142857142858317, 1.857142857142858317, 1.857142857142858317, 1.857142857142858317, 1.857142857142858317, 1.857142857142858317),
 ( 1.000000000000000000, 1.000000000000000000, 1.000000000000000000, 1.000000000000000000, 1.000000000000000000, 1.000000000000000000, 1.000000000000000000, 1.000000000000000000, 1.000000000000000000, 1.000000000000000000, 1.000000000000000000, 1.000000000000000000, 1.000000000000000000, 1.000000000000000000, 1.000000000000000000, 1.000000000000000000, 1.000000000000000000, 1.000000000000000000, 1.000000000000000000, 1.000000000000000000, 1.000000000000000000, 1.000000000000000000, 1.000000000000000000, 1.000000000000000000, 1.000000000000000000, 1.000000000000000000, 1.000000000000000000, 1.000000000000000000, 1.000000000000000000, 1.000000000000000000) ) ) 
 REPRESENTATION_ITEM ( '' )  SURFACE ( )  );
#98383 = FACE_OUTER_BOUND ( 'NONE', #46269, .T. ) ;
#98384 =( NAMED_UNIT ( * ) SI_UNIT ( $, .STERADIAN. ) SOLID_ANGLE_UNIT ( ) );
#98385 = CARTESIAN_POINT ( 'NONE',  ( -17.88790647107488496, 45.31130133375064872, -5.552611910813008755 ) ) ;
#98386 = CARTESIAN_POINT ( 'NONE',  ( -8.841337832402279773, 48.00000000000001421, -97.17444126923535919 ) ) ;
#98387 = B_SPLINE_CURVE_WITH_KNOTS ( 'NONE', 3,
 ( #92668, #75419, #58169, #57620, #8555, #18826, #91095, #26392, #90546, #51670, #84590, #50590, #91622, #10672, #65741, #25867, #82984, #41456, #41987, #74868 ),
 .UNSPECIFIED., .F., .F.,
 ( 4, 2, 2, 2, 2, 2, 2, 2, 2, 4 ),
 ( 0.002921171163060745646, 0.003426533276933593948, 0.003931895390806442250, 0.004184576447742869437, 0.004437257504679297491, 0.004942619618552150998, 0.005447981732425004504, 0.005953343846297858011, 0.006458705960170712385, 0.006964068074043565891 ),
 .UNSPECIFIED. ) ;
#98388 = PRESENTATION_LAYER_ASSIGNMENT (  '', '', ( #19224 ) ) ;
#98389 = ORIENTED_EDGE ( 'NONE', *, *, #2529, .F. ) ;
#98390 = CARTESIAN_POINT ( 'NONE',  ( -7.500000000000006217, 40.00000000000056133, -69.29143328409377034 ) ) ;
#98392 = CARTESIAN_POINT ( 'NONE',  ( 29.36420834963063342, -18.64469661114391030, 29.18565830806650752 ) ) ;
#98391 = CARTESIAN_POINT ( 'NONE',  ( -3.476223215531647803E-15, 7.124194613927619990, 3.660532965668822580 ) ) ;
#98393 = CARTESIAN_POINT ( 'NONE',  ( -32.78741055188834963, 485.3331003366709524, 5.977022408746728743 ) ) ;
#98394 = ORIENTED_EDGE ( 'NONE', *, *, #32172, .F. ) ;
#98395 = VERTEX_POINT ( 'NONE', #80394 ) ;
#98397 = CARTESIAN_POINT ( 'NONE',  ( 1.217738148383409991, 51.81134339436971459, 8.675808517492017202 ) ) ;
#98396 = FACE_OUTER_BOUND ( 'NONE', #5576, .T. ) ;
#98398 = FILL_AREA_STYLE ('',( #65510 ) ) ;
#98399 = FACE_OUTER_BOUND ( 'NONE', #16779, .T. ) ;
#98400 = CARTESIAN_POINT ( 'NONE',  ( 89.99999999999997158, -52.00000000000000000, 196.0238439516549818 ) ) ;
#98401 = FACE_OUTER_BOUND ( 'NONE', #86851, .T. ) ;
#98402 = CARTESIAN_POINT ( 'NONE',  ( -36.00698207622544800, 463.3390700132996471, 20.06331035628171477 ) ) ;
#98403 = ORIENTED_EDGE ( 'NONE', *, *, #95539, .T. ) ;
#98404 = CARTESIAN_POINT ( 'NONE',  ( 32.33349330513379982, 4.000000000000003553, 0.000000000000000000 ) ) ;
#98405 = CARTESIAN_POINT ( 'NONE',  ( -11.24762705481934333, 45.31580660681511574, -14.96115168073767698 ) ) ;
#98407 = CARTESIAN_POINT ( 'NONE',  ( 30.00000000003604583, 464.1992935685874500, 14.61140485305311287 ) ) ;
#98406 = AXIS2_PLACEMENT_3D ( 'NONE', #92071, #91036, #74810 ) ;
#98408 = LINE ( 'NONE', #64984, #89235 ) ;
#98409 = VECTOR ( 'NONE', #38113, 1000.000000000000000 ) ;
#98410 = CARTESIAN_POINT ( 'NONE',  ( 47.50581258546137065, 12.72782412601330115, -14.46700746232373369 ) ) ;
#98411 = ORIENTED_EDGE ( 'NONE', *, *, #97176, .F. ) ;
#98412 = CARTESIAN_POINT ( 'NONE',  ( -36.49060748323162073, 28.04595687074818144, 12.86268870334000525 ) ) ;
#98413 = ORIENTED_EDGE ( 'NONE', *, *, #39209, .F. ) ;
#98414 = EDGE_LOOP ( 'NONE', ( #69261, #33750, #4469, #58511, #46413, #96812 ) ) ;
#98415 = CARTESIAN_POINT ( 'NONE',  ( 0.6452690800229740065, 53.45118871115546710, 10.08352034291727684 ) ) ;
#98416 = CARTESIAN_POINT ( 'NONE',  ( 0.000000000000000000, 4.898587196589412829E-16, -4.000000000000000000 ) ) ;
#98417 = CARTESIAN_POINT ( 'NONE',  ( 16.64348903516512834, -1.200000000000000030E-05, -5.407797401561770023 ) ) ;
#98418 = DIRECTION ( 'NONE',  ( -0.000000000000000000, 1.000000000000000000, -0.000000000000000000 ) ) ;
#98419 = CARTESIAN_POINT ( 'NONE',  ( -43.51548580532710986, 326.4597452001241891, -2.301069477277255082 ) ) ;
#98420 = CARTESIAN_POINT ( 'NONE',  ( -4.473249400556560396, -67.33440330485672121, 13.71903601027506348 ) ) ;
#98421 = CARTESIAN_POINT ( 'NONE',  ( 2.678351059745897711, -49.64194654076311508, 103.0656783881315874 ) ) ;
#98422 = CYLINDRICAL_SURFACE ( 'NONE', #77715, 1.250000000000001110 ) ;
#98423 = VERTEX_POINT ( 'NONE', #104680 ) ;
#98424 = CARTESIAN_POINT ( 'NONE',  ( -9.067040280756096138, 43.96870084527508027, 13.87029715775338801 ) ) ;
#98425 = AXIS2_PLACEMENT_3D ( 'NONE', #4265, #13927, #95396 ) ;
#98426 = ORIENTED_EDGE ( 'NONE', *, *, #75508, .T. ) ;
#98427 = CARTESIAN_POINT ( 'NONE',  ( 0.000000000000000000, 0.000000000000000000, 0.000000000000000000 ) ) ;
#98428 = CARTESIAN_POINT ( 'NONE',  ( 13.82057366821712030, 304.5462546222179299, 9.872053150317878334 ) ) ;
#98429 = CARTESIAN_POINT ( 'NONE',  ( 41.71962970575597041, 464.4826118731726865, 17.11510788665847471 ) ) ;
#98430 = CARTESIAN_POINT ( 'NONE',  ( 0.000000000000000000, 36.79151656018385097, 0.000000000000000000 ) ) ;
#98431 = CARTESIAN_POINT ( 'NONE',  ( 64.89962780002818477, -56.86111594249680934, 95.13482168274560991 ) ) ;
#98432 = ORIENTED_EDGE ( 'NONE', *, *, #24112, .F. ) ;
#98433 = CARTESIAN_POINT ( 'NONE',  ( 4.999999999999995559, -46.27021379719273142, 42.58845726913239105 ) ) ;
#98434 = ADVANCED_FACE ( 'NONE', ( #7040 ), #81837, .T. ) ;
#98435 = CARTESIAN_POINT ( 'NONE',  ( -5.744562646538029504, 12.99999999999999289, 4.000000000000000000 ) ) ;
#98436 = ADVANCED_FACE ( 'NONE', ( #63177 ), #55575, .F. ) ;
#98437 = LINE ( 'NONE', #22471, #70513 ) ;
#98438 = ORIENTED_EDGE ( 'NONE', *, *, #80293, .F. ) ;
#98439 = CIRCLE ( 'NONE', #95069, 5.000000000000000888 ) ;
#98440 = CONICAL_SURFACE ( 'NONE', #89831, 3.309500000000001663, 0.9599310885968770357 ) ;
#98441 = CARTESIAN_POINT ( 'NONE',  ( -37.50059943756435388, 490.7879993827817771, 12.38039871356567545 ) ) ;
#98442 = CARTESIAN_POINT ( 'NONE',  ( 12.33349330513380337, -7.703719777548943412E-31, 4.000000000000001776 ) ) ;
#98443 = CARTESIAN_POINT ( 'NONE',  ( 7.999999999999998224, -26.28125000409677270, 3.313708498984766493 ) ) ;
#98444 = LINE ( 'NONE', #101110, #29636 ) ;
#98445 = CARTESIAN_POINT ( 'NONE',  ( -16.64348903516517098, 45.88445698070336221, 4.157797401561652784 ) ) ;
#98446 = DIRECTION ( 'NONE',  ( -1.000000000000000000, -1.224606353822377258E-16, -0.000000000000000000 ) ) ;
#98447 = CARTESIAN_POINT ( 'NONE',  ( -10.41860328468742658, 6.902172553357893037, 0.000000000000000000 ) ) ;
#98448 = CARTESIAN_POINT ( 'NONE',  ( 6.400000000000000355, -4.618802153516994302, 8.000000000000000000 ) ) ;
#98449 = SHAPE_REPRESENTATION_RELATIONSHIP ( 'NONE' , 'NONE' ,  #22031, #82029 ) ;
#98450 = CARTESIAN_POINT ( 'NONE',  ( -2.802461721337844658, 15.83563386295778308, -9.606080321247102205 ) ) ;
#98451 = FACE_OUTER_BOUND ( 'NONE', #41753, .T. ) ;
#98452 = CARTESIAN_POINT ( 'NONE',  ( 28.17977184163764193, 1.482358050883964840E-15, 0.000000000000000000 ) ) ;
#98453 = CARTESIAN_POINT ( 'NONE',  ( -95.67697799131535419, -30.00000000000000355, 191.3169455322079671 ) ) ;
#98454 = FACE_OUTER_BOUND ( 'NONE', #98603, .T. ) ;
#98455 = CARTESIAN_POINT ( 'NONE',  ( 72.46540426577622895, -57.66615126196867180, 176.6242912695971370 ) ) ;
#98457 = CARTESIAN_POINT ( 'NONE',  ( -9.864698715442679955, 7.401921974702807994, 1.292231847184868609 ) ) ;
#98456 = CARTESIAN_POINT ( 'NONE',  ( -1.220499935668712288, 25.50207722378707587, -39.81406367740636654 ) ) ;
#98458 = EDGE_CURVE ( 'NONE', #52601, #14924, #5949, .T. ) ;
#98459 = CARTESIAN_POINT ( 'NONE',  ( 19.32975784459248203, -25.59227486960913467, -38.49241694374236289 ) ) ;
#98460 = CARTESIAN_POINT ( 'NONE',  ( 3.250000000000002220, -5.629165124598879189, -5.592027715088716988 ) ) ;
#98461 = SURFACE_STYLE_USAGE ( .BOTH. , #32707 ) ;
#98462 = CARTESIAN_POINT ( 'NONE',  ( -4.212150072450890903, -59.99999999999999289, 39.63086106002882048 ) ) ;
#98463 = CARTESIAN_POINT ( 'NONE',  ( 16.51905981272399870, 42.00139749746809059, -87.79004739960677739 ) ) ;
#98464 = CARTESIAN_POINT ( 'NONE',  ( 6.544664027967929343, 53.53201714234263164, 7.403362352172786487 ) ) ;
#98465 = CARTESIAN_POINT ( 'NONE',  ( -86.48841333095882078, -50.13869857804851193, 191.3748143931806283 ) ) ;
#98466 = CIRCLE ( 'NONE', #67549, 14.00000000000000000 ) ;
#98467 = ORIENTED_EDGE ( 'NONE', *, *, #46957, .T. ) ;
#98468 = CARTESIAN_POINT ( 'NONE',  ( 17.49999999999444000, 48.26617306479607095, 62.61753806993364435 ) ) ;
#98469 = DIRECTION ( 'NONE',  ( -0.000000000000000000, 1.000000000000000000, 2.311253228826400140E-16 ) ) ;
#98470 = CARTESIAN_POINT ( 'NONE',  ( -7.230353591503060784, -53.40254472460676283, 32.78041106468180743 ) ) ;
#98471 = LINE ( 'NONE', #105511, #29039 ) ;
#98472 = CIRCLE ( 'NONE', #50203, 5.000000000000011546 ) ;
#98475 = ADVANCED_FACE ( 'NONE', ( #39439 ), #81697, .T. ) ;
#98474 = CARTESIAN_POINT ( 'NONE',  ( 1.843375668371956433, -70.60499474404922182, 13.11394492857258065 ) ) ;
#98473 = CARTESIAN_POINT ( 'NONE',  ( 2.055025722542327404, -6.319083845363749674, -5.720331885005380812 ) ) ;
#98476 = ORIENTED_EDGE ( 'NONE', *, *, #24868, .F. ) ;
#98477 = CARTESIAN_POINT ( 'NONE',  ( 5.406991766687864853, 42.00000000000000000, -69.18631089694002867 ) ) ;
#98478 = CARTESIAN_POINT ( 'NONE',  ( -9.256208135401527315, -5.000000000000035527, -17.97305361429047821 ) ) ;
#98479 = CARTESIAN_POINT ( 'NONE',  ( 16.41969624815436646, 35.05500855676915961, 21.84035938125508025 ) ) ;
#98480 = CARTESIAN_POINT ( 'NONE',  ( 31.90370271533504720, 298.6862772617328687, -9.153364518401147620 ) ) ;
#98481 = CARTESIAN_POINT ( 'NONE',  ( 4.970849588242775674, -46.55209929711413253, 102.2755693391596168 ) ) ;
#98482 = CARTESIAN_POINT ( 'NONE',  ( -7.801777176595948937, -81.41172014187365846, -1.786991866639921822 ) ) ;
#98483 = CARTESIAN_POINT ( 'NONE',  ( 4.898587196589412829E-16, -28.81250000409677270, -8.000000000000000000 ) ) ;
#98484 = CARTESIAN_POINT ( 'NONE',  ( 107.5810510768942549, -30.00000000000001066, 145.3411688640341879 ) ) ;
#98485 = CARTESIAN_POINT ( 'NONE',  ( 42.61650669486618881, -3.999999999999998224, 0.000000000000000000 ) ) ;
#98486 = ORIENTED_EDGE ( 'NONE', *, *, #28328, .T. ) ;
#98487 = CARTESIAN_POINT ( 'NONE',  ( -7.893907107745417484, -29.99999999999998934, 0.07081340544336872656 ) ) ;
#98488 = PRESENTATION_STYLE_ASSIGNMENT (( #48866 ) ) ;
#98489 = CARTESIAN_POINT ( 'NONE',  ( 5.802268690544502228, -3.456390741716395265, 103.8899761878886636 ) ) ;
#98490 = CARTESIAN_POINT ( 'NONE',  ( 45.42099917976970858, 373.9660313122255957, 6.497677916510750329 ) ) ;
#98491 = EDGE_CURVE ( 'NONE', #64333, #11951, #50833, .T. ) ;
#98492 = CARTESIAN_POINT ( 'NONE',  ( 43.61182701071368939, 463.4400368046298127, 6.347502766232850924 ) ) ;
#98493 = ORIENTED_EDGE ( 'NONE', *, *, #6597, .F. ) ;
#98494 = FACE_OUTER_BOUND ( 'NONE', #85869, .T. ) ;
#98495 = EDGE_LOOP ( 'NONE', ( #88230, #83639, #45691, #62443 ) ) ;
#98496 = LINE ( 'NONE', #33800, #81022 ) ;
#98498 = EDGE_CURVE ( 'NONE', #5193, #67017, #59333, .T. ) ;
#98497 =( NAMED_UNIT ( * ) SI_UNIT ( $, .STERADIAN. ) SOLID_ANGLE_UNIT ( ) );
#98499 = CARTESIAN_POINT ( 'NONE',  ( 7.849088363683611291, 76.00000000000000000, -5.000000000000000000 ) ) ;
#98500 = CARTESIAN_POINT ( 'NONE',  ( 9.177191262247363923, 46.16966304056472836, 13.55798985375333565 ) ) ;
#98501 = VERTEX_POINT ( 'NONE', #22202 ) ;
#98502 = CARTESIAN_POINT ( 'NONE',  ( -11.91432047182415133, 48.00000000000000000, 64.17585289259233150 ) ) ;
#98503 = CARTESIAN_POINT ( 'NONE',  ( 5.000000000000157208, -12.42851940633512520, 8.537252933897461205 ) ) ;
#98505 = CARTESIAN_POINT ( 'NONE',  ( -11.24474098223441665, -60.00000000000000711, 42.02457686618004828 ) ) ;
#98504 = AXIS2_PLACEMENT_3D ( 'NONE', #40530, #82585, #84189 ) ;
#98506 = CARTESIAN_POINT ( 'NONE',  ( 0.000000000000000000, 50.00000000000000000, 64.50000000000000000 ) ) ;
#98507 = CARTESIAN_POINT ( 'NONE',  ( 110.4355216320049635, -59.99999999999998579, 146.6424206039912121 ) ) ;
#98508 = AXIS2_PLACEMENT_3D ( 'NONE', #43610, #76502, #2611 ) ;
#98510 = CARTESIAN_POINT ( 'NONE',  ( 14.72031451962790172, -49.91564338959982905, 32.33869626530814401 ) ) ;
#98509 = CARTESIAN_POINT ( 'NONE',  ( -105.8602000712061368, -14.21045842199440656, 153.6005699772977096 ) ) ;
#98511 = ADVANCED_FACE ( 'NONE', ( #55053 ), #23156, .T. ) ;
#98513 =( LENGTH_UNIT ( ) NAMED_UNIT ( * ) SI_UNIT ( .MILLI., .METRE. ) );
#98512 = UNCERTAINTY_MEASURE_WITH_UNIT (LENGTH_MEASURE( 1.000000000000000082E-05 ), #44885, 'distance_accuracy_value', 'NONE');
#98514 = CARTESIAN_POINT ( 'NONE',  ( -41.71313970803240778, -53.34689749798402403, 43.42087845691148829 ) ) ;
#98515 = AXIS2_PLACEMENT_3D ( 'NONE', #69839, #104311, #80030 ) ;
#98516 = CARTESIAN_POINT ( 'NONE',  ( -0.4145836998305446053, 34.19552549475105963, -29.68225718326698370 ) ) ;
#98517 = ORIENTED_EDGE ( 'NONE', *, *, #2691, .T. ) ;
#98518 = ADVANCED_FACE ( 'NONE', ( #65815 ), #35074, .T. ) ;
#98519 = SURFACE_SIDE_STYLE ('',( #7911 ) ) ;
#98520 = CARTESIAN_POINT ( 'NONE',  ( 16.14595037822613932, 20.23371447307979665, -4.922994507609789849 ) ) ;
#98521 = CARTESIAN_POINT ( 'NONE',  ( 40.93292669599463096, 378.0706848361106722, 26.55786848468904537 ) ) ;
#98522 = CARTESIAN_POINT ( 'NONE',  ( 28.58349330513380337, 1.593028355512270567E-15, 0.000000000000000000 ) ) ;
#98523 = CARTESIAN_POINT ( 'NONE',  ( -3.313708498984760276, -28.71875000409677625, -8.000000000000000000 ) ) ;
#98524 = CARTESIAN_POINT ( 'NONE',  ( 10.17470798438142410, -0.7156995453649822592, 20.10980123007764675 ) ) ;
#98525 = ORIENTED_EDGE ( 'NONE', *, *, #83544, .F. ) ;
#98526 = DIRECTION ( 'NONE',  ( -1.000000000000000000, -1.224606353822377258E-16, -0.000000000000000000 ) ) ;
#98527 = ORIENTED_EDGE ( 'NONE', *, *, #15775, .T. ) ;
#98528 = CARTESIAN_POINT ( 'NONE',  ( 75.85296913857929724, -29.99999999993386623, 164.1495175436531895 ) ) ;
#98529 = CARTESIAN_POINT ( 'NONE',  ( 23.70473373808798101, 41.64033039645621415, -74.70427921067390287 ) ) ;
#98530 = EDGE_CURVE ( 'NONE', #36517, #75948, #95508, .T. ) ;
#98531 = CARTESIAN_POINT ( 'NONE',  ( 23.21751746555220564, 25.25267828308493634, -33.20617127781077471 ) ) ;
#98532 = DIRECTION ( 'NONE',  ( -0.000000000000000000, -1.000000000000000000, -0.000000000000000000 ) ) ;
#98533 = CARTESIAN_POINT ( 'NONE',  ( 90.44129752230823271, -29.99999999999999645, 91.07386086299301553 ) ) ;
#98534 = CARTESIAN_POINT ( 'NONE',  ( 8.000086790516061086, 100.9998264189399322, 0.2639471549312805698 ) ) ;
#98535 = VERTEX_POINT ( 'NONE', #51205 ) ;
#98536 = ORIENTED_EDGE ( 'NONE', *, *, #23260, .F. ) ;
#98537 = ORIENTED_EDGE ( 'NONE', *, *, #59285, .F. ) ;
#98538 = CARTESIAN_POINT ( 'NONE',  ( 0.000000000000000000, 1.502314598737159031E-15, -8.000000000000000000 ) ) ;
#98539 = CARTESIAN_POINT ( 'NONE',  ( -3.653369855178271397, -8.635023481229975317, -12.30779604435681129 ) ) ;
#98540 = CARTESIAN_POINT ( 'NONE',  ( -41.75466287779232033, 464.7989438035445460, 15.73053683052044960 ) ) ;
#98541 = ORIENTED_EDGE ( 'NONE', *, *, #99726, .T. ) ;
#98542 = CARTESIAN_POINT ( 'NONE',  ( 9.381593208289373820, 107.0143863811950666, -3.465401811657803144 ) ) ;
#98543 = ORIENTED_EDGE ( 'NONE', *, *, #28814, .T. ) ;
#98544 = CARTESIAN_POINT ( 'NONE',  ( 32.96114378239634846, 439.7497662205600477, 24.15381041467298928 ) ) ;
#98545 = CARTESIAN_POINT ( 'NONE',  ( 79.97203214341874400, -38.78014282313012728, 192.9381993355203804 ) ) ;
#98546 = FACE_OUTER_BOUND ( 'NONE', #100586, .T. ) ;
#98547 = CARTESIAN_POINT ( 'NONE',  ( 40.27367167681648397, 320.5181970100869648, 8.188281879750116232 ) ) ;
#98548 = CARTESIAN_POINT ( 'NONE',  ( 41.66301127302160978, 485.3863426732067978, -3.409513628943111829 ) ) ;
#98549 = CARTESIAN_POINT ( 'NONE',  ( 0.000000000000000000, -14.49999999999999822, 9.500000000000000000 ) ) ;
#98550 = STYLED_ITEM ( 'NONE', ( #8101 ), #82998 ) ;
#98551 = CARTESIAN_POINT ( 'NONE',  ( -28.32689090366336160, 34.16882244950244996, -9.120241557729505288 ) ) ;
#98552 = CARTESIAN_POINT ( 'NONE',  ( -19.50000000000000000, 12.99999999999999289, 6.999999999999999112 ) ) ;
#98553 = ADVANCED_FACE ( 'NONE', ( #41535 ), #99773, .F. ) ;
#98554 = CARTESIAN_POINT ( 'NONE',  ( 32.62553167428433198, 485.9570050037727356, 7.214059741204942533 ) ) ;
#98555 = B_SPLINE_CURVE_WITH_KNOTS ( 'NONE', 3,
 ( #99527, #74716, #56935, #75249, #1350, #34312, #81209, #40237, #73112, #106018, #98464, #40764, #106559, #24618, #8157, #53202, #86121, #19815, #11118, #37587, #36527, #12722 ),
 .UNSPECIFIED., .F., .F.,
 ( 4, 2, 2, 2, 2, 2, 2, 2, 2, 2, 4 ),
 ( 0.003041022514278852139, 0.003544801402695308724, 0.003796690846903537017, 0.004048580291111764443, 0.004552359179528218426, 0.005056138067944675012, 0.005559916956361130730, 0.006063695844777587315, 0.006567474733194043901, 0.006819364177402275663, 0.007071253621610506558 ),
 .UNSPECIFIED. ) ;
#98556 = CARTESIAN_POINT ( 'NONE',  ( -5.749819765084808409, 4.859478910914223349, 5.000000000000001776 ) ) ;
#98557 = ORIENTED_EDGE ( 'NONE', *, *, #76286, .F. ) ;
#98558 = CARTESIAN_POINT ( 'NONE',  ( 6.281178480976150169, 7.505553499465138501, 5.007024290797826235E-17 ) ) ;
#98560 = CARTESIAN_POINT ( 'NONE',  ( -29.13995660218273898, 297.4011841907129110, 2.495382766646905282 ) ) ;
#98559 = FILL_AREA_STYLE_COLOUR ( '', #71028 ) ;
#98561 =( LENGTH_UNIT ( ) NAMED_UNIT ( * ) SI_UNIT ( .MILLI., .METRE. ) );
#98562 =( LENGTH_UNIT ( ) NAMED_UNIT ( * ) SI_UNIT ( .MILLI., .METRE. ) );
#98563 = DIRECTION ( 'NONE',  ( 0.000000000000000000, 0.000000000000000000, 1.000000000000000000 ) ) ;
#98564 = CARTESIAN_POINT ( 'NONE',  ( 33.86650669486618881, 1.474610560812782335E-15, 0.000000000000000000 ) ) ;
#98565 = CIRCLE ( 'NONE', #5568, 5.000000000000002665 ) ;
#98566 = EDGE_CURVE ( 'NONE', #92227, #78717, #831, .T. ) ;
#98567 = VECTOR ( 'NONE', #94781, 1000.000000000000000 ) ;
#98568 = CARTESIAN_POINT ( 'NONE',  ( 2.361169560329932526, 300.9835946509371070, 9.719902681333095984 ) ) ;
#98569 = FILL_AREA_STYLE ('',( #55967 ) ) ;
#98570 = EDGE_CURVE ( 'NONE', #16221, #36441, #59414, .T. ) ;
#98571 = ORIENTED_EDGE ( 'NONE', *, *, #81615, .T. ) ;
#98572 = CARTESIAN_POINT ( 'NONE',  ( 85.04290646969892009, -50.19384762663964494, 189.2821407580086088 ) ) ;
#98573 = CARTESIAN_POINT ( 'NONE',  ( 8.999999999999996447, -80.00000000000000000, 42.58845726811989607 ) ) ;
#98574 =( LENGTH_UNIT ( ) NAMED_UNIT ( * ) SI_UNIT ( .MILLI., .METRE. ) );
#98575 = ORIENTED_EDGE ( 'NONE', *, *, #103217, .F. ) ;
#98576 = CARTESIAN_POINT ( 'NONE',  ( 94.47643939734095397, -57.66978673744599604, -1.231856577211943637 ) ) ;
#98577 = CARTESIAN_POINT ( 'NONE',  ( 38.86650669486618881, -3.999999999999998224, 0.000000000000000000 ) ) ;
#98578 = FILL_AREA_STYLE_COLOUR ( '', #43766 ) ;
#98579 = CARTESIAN_POINT ( 'NONE',  ( 21.29975379448946171, 294.8969325209483259, -1.990407376643353210 ) ) ;
#98580 = AXIS2_PLACEMENT_3D ( 'NONE', #106380, #10350, #98821 ) ;
#98581 = CARTESIAN_POINT ( 'NONE',  ( -80.98454112480462186, -30.00000000000000355, 4.285213993873024485 ) ) ;
#98582 = ADVANCED_FACE ( 'NONE', ( #74425 ), #53514, .F. ) ;
#98583 = CIRCLE ( 'NONE', #105455, 4.172000000000001485 ) ;
#98584 = CARTESIAN_POINT ( 'NONE',  ( 29.49550841906154375, 18.54274624009278583, 39.61427208276940348 ) ) ;
#98585 = CARTESIAN_POINT ( 'NONE',  ( 22.43826451847985837, 28.20713089197013446, -30.97515248374633146 ) ) ;
#98586 = CARTESIAN_POINT ( 'NONE',  ( 52.44308130789431033, -29.98757490428321759, 50.93680095260226182 ) ) ;
#98587 = FACE_OUTER_BOUND ( 'NONE', #81340, .T. ) ;
#98588 = ADVANCED_FACE ( 'NONE', ( #17283 ), #85268, .F. ) ;
#98589 = LINE ( 'NONE', #99110, #35031 ) ;
#98590 = CARTESIAN_POINT ( 'NONE',  ( -16.64348903516521005, 43.47556584774768140, -6.657797401561535544 ) ) ;
#98591 = CARTESIAN_POINT ( 'NONE',  ( 4.497431761510337189, -84.45901875748972998, -3.972160586670088200 ) ) ;
#98592 = CARTESIAN_POINT ( 'NONE',  ( -22.07885140346273900, 26.01882032652172327, 31.43383091546978036 ) ) ;
#98593 = DIRECTION ( 'NONE',  ( 0.000000000000000000, 1.000000000000000000, 0.000000000000000000 ) ) ;
#98594 = AXIS2_PLACEMENT_3D ( 'NONE', #35857, #19148, #91923 ) ;
#98595 = CARTESIAN_POINT ( 'NONE',  ( -99.16883851872213995, -37.99999999999991473, 191.7725159787542282 ) ) ;
#98596 = ORIENTED_EDGE ( 'NONE', *, *, #38606, .F. ) ;
#98597 = FACE_OUTER_BOUND ( 'NONE', #44037, .T. ) ;
#98598 = CARTESIAN_POINT ( 'NONE',  ( -7.551892080562057075, 81.99012297460615173, 2.647003822403972695 ) ) ;
#98599 = CARTESIAN_POINT ( 'NONE',  ( -48.02835407290515946, 14.94086294439721030, 16.85535821593516559 ) ) ;
#98602 = ADVANCED_FACE ( 'NONE', ( #50662 ), #38779, .T. ) ;
#98601 = DIRECTION ( 'NONE',  ( 0.000000000000000000, 0.000000000000000000, 1.000000000000000000 ) ) ;
#98600 = CARTESIAN_POINT ( 'NONE',  ( 66.00571552735603120, 6.975173280561618775E-15, 0.000000000000000000 ) ) ;
#98603 = EDGE_LOOP ( 'NONE', ( #68405, #49149, #47703, #3339 ) ) ;
#98604 = CARTESIAN_POINT ( 'NONE',  ( -9.000000000000001776, -80.00000000000000000, 42.58845726811989607 ) ) ;
#98605 = EDGE_LOOP ( 'NONE', ( #4258, #8227, #31183, #26948, #68564 ) ) ;
#98606 = CARTESIAN_POINT ( 'NONE',  ( -26.49116892277528024, 34.70576323815743081, 9.907392575990456862 ) ) ;
#98607 = CARTESIAN_POINT ( 'NONE',  ( -4.366061277241459315, 4.984806845751375448, -0.09463688534106240446 ) ) ;
#98608 = CARTESIAN_POINT ( 'NONE',  ( -33.99305469949648284, -60.00000000000000000, -40.43516885408138961 ) ) ;
#98609 = ORIENTED_EDGE ( 'NONE', *, *, #59334, .T. ) ;
#98610 = CARTESIAN_POINT ( 'NONE',  ( 0.1061556211655344389, -4.836380039389415408, 4.623144047065558482 ) ) ;
#98611 = LINE ( 'NONE', #62432, #81585 ) ;
#98612 = CARTESIAN_POINT ( 'NONE',  ( 96.81084219511998867, -52.81891926509837276, 195.3532482584386969 ) ) ;
#98613 = AXIS2_PLACEMENT_3D ( 'NONE', #17476, #694, #33659 ) ;
#98614 = DIRECTION ( 'NONE',  ( 0.000000000000000000, -1.000000000000000000, 0.000000000000000000 ) ) ;
#98615 = ORIENTED_EDGE ( 'NONE', *, *, #15299, .T. ) ;
#98616 = STYLED_ITEM ( 'NONE', ( #2543 ), #83469 ) ;
#98617 = ORIENTED_EDGE ( 'NONE', *, *, #102815, .F. ) ;
#98618 = ORIENTED_EDGE ( 'NONE', *, *, #104539, .T. ) ;
#98619 = CARTESIAN_POINT ( 'NONE',  ( 31.16300488023808057, 374.7522420000291277, 23.86485433879470364 ) ) ;
#98620 = EDGE_CURVE ( 'NONE', #51023, #58545, #100731, .T. ) ;
#98621 = CARTESIAN_POINT ( 'NONE',  ( -6.459500862575596969, -11.87485980093857485, 10.39038571060303262 ) ) ;
#98622 = CARTESIAN_POINT ( 'NONE',  ( 8.719144900081944982, 53.90630142508563694, 1.531152949374442462 ) ) ;
#98623 = ORIENTED_EDGE ( 'NONE', *, *, #34689, .T. ) ;
#98624 = CARTESIAN_POINT ( 'NONE',  ( -43.31290673308605221, 487.3457497296792553, 8.045183856861967797 ) ) ;
#98625 = DIRECTION ( 'NONE',  ( 0.000000000000000000, -1.000000000000000000, 0.000000000000000000 ) ) ;
#98626 = FACE_OUTER_BOUND ( 'NONE', #22634, .T. ) ;
#98627 = CARTESIAN_POINT ( 'NONE',  ( -29.04643245788701122, -57.68166065953202093, 44.76603692081018693 ) ) ;
#98628 = CARTESIAN_POINT ( 'NONE',  ( -7.188101187500002709, -33.31250000204838813, 2.977408999572648707 ) ) ;
#98629 = CARTESIAN_POINT ( 'NONE',  ( -30.90153257058555170, 13.61190038887007248, 41.14606609713253249 ) ) ;
#98630 = CARTESIAN_POINT ( 'NONE',  ( -0.4139846110599526008, 25.19206125174364175, 40.68244515147750917 ) ) ;
#98631 = CARTESIAN_POINT ( 'NONE',  ( 0.8405003012203439150, 27.41029791806389326, -40.42883694400927652 ) ) ;
#98632 = CARTESIAN_POINT ( 'NONE',  ( 32.64290048136811606, -14.21045842199427867, -35.33280650708731230 ) ) ;
#98633 = EDGE_CURVE ( 'NONE', #47418, #105782, #37036, .T. ) ;
#98634 = CARTESIAN_POINT ( 'NONE',  ( -43.51084452654468748, 465.2903130129606666, 9.421687747985890482 ) ) ;
#98635 = CARTESIAN_POINT ( 'NONE',  ( -52.73927720795784069, -56.84651578577485509, 62.26472032949996560 ) ) ;
#98636 = LINE ( 'NONE', #39373, #93489 ) ;
#98637 = ORIENTED_EDGE ( 'NONE', *, *, #89345, .F. ) ;
#98638 = CARTESIAN_POINT ( 'NONE',  ( -98.60539400174438640, -37.75072670319377011, 192.1773030902787980 ) ) ;
#98639 = CARTESIAN_POINT ( 'NONE',  ( -2.569942033241107815, 295.6515237736050494, -10.00266688365466017 ) ) ;
#98640 = CARTESIAN_POINT ( 'NONE',  ( 9.346890874034901486, -3.133782013405083777, 14.76170641224502589 ) ) ;
#98641 = ORIENTED_EDGE ( 'NONE', *, *, #71551, .F. ) ;
#98642 = CARTESIAN_POINT ( 'NONE',  ( -17.89171299917695279, 43.20822152669683902, 5.300773039380033858 ) ) ;
#98643 = CARTESIAN_POINT ( 'NONE',  ( 84.23062891746764080, -38.75005706687972662, 197.9527241322343230 ) ) ;
#98644 = CARTESIAN_POINT ( 'NONE',  ( 48.02835407290544367, 14.94086294439726892, 16.85535821593427386 ) ) ;
#98645 = DIRECTION ( 'NONE',  ( -1.000000000000000000, -1.224606353822377258E-16, -0.000000000000000000 ) ) ;
#98646 = EDGE_CURVE ( 'NONE', #18895, #44460, #6018, .T. ) ;
#98647 = CARTESIAN_POINT ( 'NONE',  ( -17.49999999999997513, 45.00000000000000711, 64.09953197936602010 ) ) ;
#98648 = CARTESIAN_POINT ( 'NONE',  ( 55.65414010178471926, 42.00000000000000000, 72.41885610124163009 ) ) ;
#98649 = CARTESIAN_POINT ( 'NONE',  ( 84.63983498852250875, -30.00000000000000355, 166.8986807930797340 ) ) ;
#98650 = CARTESIAN_POINT ( 'NONE',  ( 37.51493083963053721, 491.7337707781528024, 12.51683509955209672 ) ) ;
#98651 = DIRECTION ( 'NONE',  ( 0.000000000000000000, -1.000000000000000000, 0.000000000000000000 ) ) ;
#98652 = CARTESIAN_POINT ( 'NONE',  ( -34.16218064238212548, 484.1154536690855252, 0.7177099017928977309 ) ) ;
#98653 = MECHANICAL_DESIGN_GEOMETRIC_PRESENTATION_REPRESENTATION (  '', ( #79728 ), #5666 ) ;
#98654 = ORIENTED_EDGE ( 'NONE', *, *, #74195, .T. ) ;
#98655 = VERTEX_POINT ( 'NONE', #27529 ) ;
#98656 = CARTESIAN_POINT ( 'NONE',  ( 49.01680650270304795, -56.82380834871364783, 54.79513700058014081 ) ) ;
#98657 = MECHANICAL_DESIGN_GEOMETRIC_PRESENTATION_REPRESENTATION (  '', ( #40086 ), #10801 ) ;
#98658 = CARTESIAN_POINT ( 'NONE',  ( 6.641837668257388749, 41.74662779905570176, -59.04567176600482270 ) ) ;
#98659 = DIRECTION ( 'NONE',  ( 0.000000000000000000, -1.000000000000000000, 0.000000000000000000 ) ) ;
#98660 = ORIENTED_EDGE ( 'NONE', *, *, #95698, .F. ) ;
#98661 = CARTESIAN_POINT ( 'NONE',  ( -97.41561983528457347, -38.35525745205964654, 73.11340283102843784 ) ) ;
#98662 = VERTEX_POINT ( 'NONE', #78672 ) ;
#98663 = CARTESIAN_POINT ( 'NONE',  ( 91.87323331309748653, -38.35385193510057178, 33.51482854396223132 ) ) ;
#98664 = CARTESIAN_POINT ( 'NONE',  ( 13.70298725226294501, 22.84579378370908742, -1.781593527410179956 ) ) ;
#98665 = CARTESIAN_POINT ( 'NONE',  ( 104.4246528305459378, -52.71695562033825411, 156.3626540467217865 ) ) ;
#98666 = CARTESIAN_POINT ( 'NONE',  ( -31.38091039062430099, 439.2456886734215118, 22.99800500073227738 ) ) ;
#98667 = CARTESIAN_POINT ( 'NONE',  ( -32.33884982129379182, 318.8862026410800468, -6.596051802676561771 ) ) ;
#98668 = SURFACE_STYLE_USAGE ( .BOTH. , #91148 ) ;
#98669 = CARTESIAN_POINT ( 'NONE',  ( 74.36230277464828475, -60.00000000000001421, 175.8080994144255840 ) ) ;
#98670 = CARTESIAN_POINT ( 'NONE',  ( 17.50000000000002842, 45.00000000000000711, 64.09953197936602010 ) ) ;
#98671 = ORIENTED_EDGE ( 'NONE', *, *, #8848, .F. ) ;
#98672 = CARTESIAN_POINT ( 'NONE',  ( 60.90451431562469509, -56.86322954724349898, 83.15454531713724862 ) ) ;
#98673 = CARTESIAN_POINT ( 'NONE',  ( -25.12920025922564449, 295.5949704605591251, -9.840788051256282642 ) ) ;
#98674 = EDGE_CURVE ( 'NONE', #23216, #70045, #25003, .T. ) ;
#98675 = CARTESIAN_POINT ( 'NONE',  ( 9.934750400155193617, -50.13194482833283416, 28.16945530398552222 ) ) ;
#98676 = CARTESIAN_POINT ( 'NONE',  ( -8.759832293797922276, -5.000000000000000000, -16.81557763462109278 ) ) ;
#98678 = CARTESIAN_POINT ( 'NONE',  ( -4.647051454204487619, 54.31004531717275796, 6.195923535874935162 ) ) ;
#98677 = CARTESIAN_POINT ( 'NONE',  ( -71.41185097590582131, -30.00000000016128965, 134.2290320126720928 ) ) ;
#98679 = CARTESIAN_POINT ( 'NONE',  ( -41.26652560176431450, 329.6458478461855179, 10.39356917096987054 ) ) ;
#98680 = CARTESIAN_POINT ( 'NONE',  ( -3.749999999999998224, -6.495190528383299799, -6.991905250253757309 ) ) ;
#98681 = CARTESIAN_POINT ( 'NONE',  ( -40.67741014324408155, 464.1451327582763042, 18.19863275169177896 ) ) ;
#98682 = CARTESIAN_POINT ( 'NONE',  ( 5.656854249492380582, -28.81249999999999289, -5.656854249492379694 ) ) ;
#98683 = EDGE_CURVE ( 'NONE', #30956, #31239, #74924, .T. ) ;
#98684 = CARTESIAN_POINT ( 'NONE',  ( 7.894787914004607998, -0.7647108141804129788, -7.591390474663422872 ) ) ;
#98685 = AXIS2_PLACEMENT_3D ( 'NONE', #44144, #59805, #10686 ) ;
#98686 = EDGE_LOOP ( 'NONE', ( #8300, #61672, #53934, #27262, #57888 ) ) ;
#98687 = CARTESIAN_POINT ( 'NONE',  ( 85.24943635772166317, -25.41792041905209842, 169.5202013333633033 ) ) ;
#98688 = CARTESIAN_POINT ( 'NONE',  ( 44.08840282922842846, 485.7747746244180576, 4.178803824088268115 ) ) ;
#98689 = CARTESIAN_POINT ( 'NONE',  ( 46.00000000000000000, 500.0000000000002274, 0.000000000000000000 ) ) ;
#98690 = VERTEX_POINT ( 'NONE', #78153 ) ;
#98691 = AXIS2_PLACEMENT_3D ( 'NONE', #25977, #2159, #76589 ) ;
#98692 = DIRECTION ( 'NONE',  ( 1.000000000000000000, 1.224606353822377258E-16, 0.000000000000000000 ) ) ;
#98693 = CARTESIAN_POINT ( 'NONE',  ( 38.09999999999999432, 1.533819458162526451E-15, 0.000000000000000000 ) ) ;
#98694 = CARTESIAN_POINT ( 'NONE',  ( 92.82022815836235452, 1.016364837396684119E-14, 0.000000000000000000 ) ) ;
#98695 = DIRECTION ( 'NONE',  ( 0.000000000000000000, -1.000000000000000000, 0.000000000000000000 ) ) ;
#98696 = CARTESIAN_POINT ( 'NONE',  ( -43.02643730873325012, 41.50233601984075449, -51.34842824453740207 ) ) ;
#98697 = CARTESIAN_POINT ( 'NONE',  ( 0.000000000000000000, 0.000000000000000000, 0.000000000000000000 ) ) ;
#98698 = EDGE_CURVE ( 'NONE', #25211, #3119, #76631, .T. ) ;
#98699 = SHAPE_REPRESENTATION_RELATIONSHIP ( 'NONE' , 'NONE' ,  #77771, #48600 ) ;
#98700 = AXIS2_PLACEMENT_3D ( 'NONE', #66857, #41507, #98148 ) ;
#98701 = CARTESIAN_POINT ( 'NONE',  ( 38.31547885847380286, 25.47151378724775839, 11.19247416203105416 ) ) ;
#98702 = DIRECTION ( 'NONE',  ( -1.000000000000000000, -0.000000000000000000, -0.000000000000000000 ) ) ;
#98704 = CARTESIAN_POINT ( 'NONE',  ( -13.46984034094769633, 22.45595379590175966, 3.284040074602051718 ) ) ;
#98703 = CARTESIAN_POINT ( 'NONE',  ( -10.71489332182602361, -20.52239476129827267, 35.44028641706174199 ) ) ;
#98705 = CARTESIAN_POINT ( 'NONE',  ( 2.977408999572651815, -13.43750000204838457, 7.188101187500000933 ) ) ;
#98706 = CARTESIAN_POINT ( 'NONE',  ( -28.43348347353486005, 17.76907357228462558, -40.77956405912765803 ) ) ;
#98707 = CARTESIAN_POINT ( 'NONE',  ( -0.6511518506208961998, 8.763486134561265573, -7.907570769506046204 ) ) ;
#98708 = ORIENTED_EDGE ( 'NONE', *, *, #15124, .T. ) ;
#98709 = B_SPLINE_CURVE_WITH_KNOTS ( 'NONE', 3,
 ( #105837, #31981, #41117, #90733, #33571, #607 ),
 .UNSPECIFIED., .F., .F.,
 ( 4, 2, 4 ),
 ( 2.380731631042988191E-07, 0.002336973833157631863, 0.004673709593152160051 ),
 .UNSPECIFIED. ) ;
#98710 = CARTESIAN_POINT ( 'NONE',  ( -19.50000000000149925, 49.99999999999985789, 59.64162155654717168 ) ) ;
#98711 = MECHANICAL_DESIGN_GEOMETRIC_PRESENTATION_REPRESENTATION (  '', ( #14569 ), #26480 ) ;
#98712 = CARTESIAN_POINT ( 'NONE',  ( 23.78270938940518420, 25.17287789278546128, 33.07427373539508864 ) ) ;
#98713 = CARTESIAN_POINT ( 'NONE',  ( -9.291918545211730773, 140.5484994665884244, -5.000000000000000888 ) ) ;
#98714 = AXIS2_PLACEMENT_3D ( 'NONE', #88395, #64642, #14469 ) ;
#98715 = CARTESIAN_POINT ( 'NONE',  ( -7.500000017879060010, -4.999999999997784883, -69.80246344213135501 ) ) ;
#98717 = CARTESIAN_POINT ( 'NONE',  ( 64.34530734380760464, -47.40884564742954410, -26.19147373469116502 ) ) ;
#98716 = CARTESIAN_POINT ( 'NONE',  ( 41.85000000000000142, 1.533819458162526451E-15, 0.000000000000000000 ) ) ;
#98718 = ORIENTED_EDGE ( 'NONE', *, *, #1113, .T. ) ;
#98719 = PRESENTATION_LAYER_ASSIGNMENT (  '', '', ( #66232 ) ) ;
#98720 = LINE ( 'NONE', #24873, #15144 ) ;
#98721 = CARTESIAN_POINT ( 'NONE',  ( -5.123687866623413356, 51.38063399059588932, 8.522745146031866170 ) ) ;
#98722 = CIRCLE ( 'NONE', #79802, 4.000000000000000888 ) ;
#98723 = ORIENTED_EDGE ( 'NONE', *, *, #50012, .F. ) ;
#98724 = DIRECTION ( 'NONE',  ( 0.000000000000000000, 0.000000000000000000, -1.000000000000000000 ) ) ;
#98725 = CARTESIAN_POINT ( 'NONE',  ( -20.13249097554416167, 41.84298886347988855, -79.53117214682279723 ) ) ;
#98726 = CARTESIAN_POINT ( 'NONE',  ( -98.09259472220433906, -59.99999999999999289, 69.49854301730701422 ) ) ;
#98727 = FACE_OUTER_BOUND ( 'NONE', #18418, .T. ) ;
#98728 = DIRECTION ( 'NONE',  ( -1.000000000000000000, -1.224606353822377258E-16, -0.000000000000000000 ) ) ;
#98729 = CARTESIAN_POINT ( 'NONE',  ( 6.499999999999999112, 3.752776749732559036, -8.000000000000000000 ) ) ;
#98730 = CARTESIAN_POINT ( 'NONE',  ( -32.12958771267398816, 464.7275665249426311, 11.12424126545965386 ) ) ;
#98732 = CARTESIAN_POINT ( 'NONE',  ( 32.15552878745101140, 487.8964323476858453, 8.685603495209447189 ) ) ;
#98731 = CARTESIAN_POINT ( 'NONE',  ( -2.617478844992371823, -5.000000000000002665, -75.26027323389158141 ) ) ;
#98733 = CARTESIAN_POINT ( 'NONE',  ( -85.81337131230007742, -21.82407471985175818, 170.1709790121419985 ) ) ;
#98734 = VERTEX_POINT ( 'NONE', #94358 ) ;
#98735 = VERTEX_POINT ( 'NONE', #69546 ) ;
#98736 = ORIENTED_EDGE ( 'NONE', *, *, #37988, .F. ) ;
#98737 = DIRECTION ( 'NONE',  ( -1.000000000000000000, 0.000000000000000000, 0.000000000000000000 ) ) ;
#98738 = EDGE_CURVE ( 'NONE', #7738, #50186, #44363, .T. ) ;
#98739 = CARTESIAN_POINT ( 'NONE',  ( 32.43176025740030610, 464.5282231481863846, 9.485014939590488581 ) ) ;
#98741 = VERTEX_POINT ( 'NONE', #12876 ) ;
#98740 = B_SPLINE_CURVE_WITH_KNOTS ( 'NONE', 3,
 ( #81396, #24276, #57129, #16146, #40963, #73851, #32895, #101332, #68978, #77047, #11234, #67895, #76509, #3163, #75448, #26419, #34508, #101852, #2617, #84616, #100256, #59819 ),
 .UNSPECIFIED., .F., .F.,
 ( 4, 2, 2, 2, 2, 2, 2, 2, 2, 2, 4 ),
 ( 0.007079440862166612621, 0.007331525063779767253, 0.007583609265392921885, 0.008087777668619232016, 0.008339861870232388383, 0.008591946071845546484, 0.009096114475071866157, 0.009600282878298185829, 0.01010445128152450724, 0.01060861968475082691, 0.01111278808797714832 ),
 .UNSPECIFIED. ) ;
#98742 = DIRECTION ( 'NONE',  ( -1.000000000000000000, -0.000000000000000000, -0.000000000000000000 ) ) ;
#98743 = EDGE_CURVE ( 'NONE', #89958, #44258, #92107, .T. ) ;
#98744 = CARTESIAN_POINT ( 'NONE',  ( 0.000000000000000000, -15.00000000000000000, 0.000000000000000000 ) ) ;
#98745 = CARTESIAN_POINT ( 'NONE',  ( 4.250000000000000000, 0.000000000000000000, -10.00000000000000000 ) ) ;
#98746 = CARTESIAN_POINT ( 'NONE',  ( -6.928203230275509661, -65.00000000000000000, -4.000000000000002665 ) ) ;
#98747 = LINE ( 'NONE', #42654, #8397 ) ;
#98748 = CARTESIAN_POINT ( 'NONE',  ( 7.814555105279644920, -5.000000000000000000, -95.45731198298756226 ) ) ;
#98749 = CARTESIAN_POINT ( 'NONE',  ( 0.3173508448886524502, 5.375634714784618851, -6.689127551062007626 ) ) ;
#98750 = CARTESIAN_POINT ( 'NONE',  ( 108.8241408383580193, -29.99999999999998224, 157.0475695436092565 ) ) ;
#98751 = EDGE_CURVE ( 'NONE', #90863, #46570, #559, .T. ) ;
#98752 = CARTESIAN_POINT ( 'NONE',  ( -106.1779193982466580, -14.21045842199435860, 156.9944278011976451 ) ) ;
#98753 = CARTESIAN_POINT ( 'NONE',  ( -62.01645086870617973, -49.91653808238077517, 82.86907591662273376 ) ) ;
#98754 = ORIENTED_EDGE ( 'NONE', *, *, #34710, .T. ) ;
#98755 = DIRECTION ( 'NONE',  ( 0.000000000000000000, -1.000000000000000000, 0.000000000000000000 ) ) ;
#98756 = CARTESIAN_POINT ( 'NONE',  ( 95.11636133611268917, -59.99999999998292566, -7.883470413377934527 ) ) ;
#98757 = ORIENTED_EDGE ( 'NONE', *, *, #3471, .T. ) ;
#98758 = CARTESIAN_POINT ( 'NONE',  ( 1.013586109042279082, -49.91581433662842926, 32.20895234904045168 ) ) ;
#98759 = CARTESIAN_POINT ( 'NONE',  ( -97.91261498135648367, -37.82064874998170723, 125.6660091448068073 ) ) ;
#98760 = CARTESIAN_POINT ( 'NONE',  ( -2.977408999572650039, -14.56250000204838457, -7.188101187500000933 ) ) ;
#98761 = VECTOR ( 'NONE', #15479, 1000.000000000000000 ) ;
#98762 = CARTESIAN_POINT ( 'NONE',  ( 5.799999999999999822, -9.237604307034013473, 7.924929828396943928E-16 ) ) ;
#98763 = ORIENTED_EDGE ( 'NONE', *, *, #104963, .F. ) ;
#98764 = CARTESIAN_POINT ( 'NONE',  ( 6.006401927973604060, -30.00000000000000355, 3.977000602544253027 ) ) ;
#98765 = VERTEX_POINT ( 'NONE', #53355 ) ;
#98766 = CARTESIAN_POINT ( 'NONE',  ( -3.250000000000013767, -5.629165124598844550, 1.734723475976807094E-15 ) ) ;
#98767 = AXIS2_PLACEMENT_3D ( 'NONE', #53789, #12788, #45705 ) ;
#98768 = CARTESIAN_POINT ( 'NONE',  ( -94.01890188198808573, -59.99999999999997158, 202.5480236000225034 ) ) ;
#98769 = CARTESIAN_POINT ( 'NONE',  ( 9.668268460383899310, -57.17502809900269511, 29.56382476086920974 ) ) ;
#98770 = CARTESIAN_POINT ( 'NONE',  ( -5.082755093536325042, -20.46875000204838813, -5.082755093536325930 ) ) ;
#98771 = EDGE_CURVE ( 'NONE', #1686, #51764, #53347, .T. ) ;
#98772 = CARTESIAN_POINT ( 'NONE',  ( 44.16317469766475057, 463.2893454858578366, 6.606904447375195666 ) ) ;
#98773 = CARTESIAN_POINT ( 'NONE',  ( -24.47192364801391662, 27.44308780173428985, -32.07880713851005083 ) ) ;
#98774 = AXIS2_PLACEMENT_3D ( 'NONE', #83906, #93612, #84983 ) ;
#98775 = CARTESIAN_POINT ( 'NONE',  ( -3.973065139046256800, 18.38687860884221337, -5.763576303916519983 ) ) ;
#98776 = DIRECTION ( 'NONE',  ( -1.000000000000000000, -1.224606353822377258E-16, -0.000000000000000000 ) ) ;
#98777 = CARTESIAN_POINT ( 'NONE',  ( -29.99999999999696243, 464.1078291054902252, 11.04693782968386628 ) ) ;
#98778 = DIRECTION ( 'NONE',  ( -1.000000000000000000, -1.224606353822377258E-16, -0.000000000000000000 ) ) ;
#98779 = CARTESIAN_POINT ( 'NONE',  ( -31.75048384320466255, 299.0195043205505385, -1.074641621235506772 ) ) ;
#98780 = CARTESIAN_POINT ( 'NONE',  ( 105.5007349313588634, -60.00000000000002842, 154.8517593642223744 ) ) ;
#98781 = CARTESIAN_POINT ( 'NONE',  ( -33.91206465489236876, -53.37053416063930200, 37.37971910314460189 ) ) ;
#98782 = CARTESIAN_POINT ( 'NONE',  ( -3.677502082062658051, -48.98465343287618623, 104.5296620117538424 ) ) ;
#98783 = CARTESIAN_POINT ( 'NONE',  ( 42.79026094202129116, -60.24709657765144755, 46.28082913036630686 ) ) ;
#98784 = VERTEX_POINT ( 'NONE', #11814 ) ;
#98785 = CARTESIAN_POINT ( 'NONE',  ( 43.80679553849883945, 434.9371637098674910, 12.86766421698563967 ) ) ;
#98786 = CARTESIAN_POINT ( 'NONE',  ( -81.60022401860847197, -38.84181500998843006, 195.4017998612470137 ) ) ;
#98787 = ORIENTED_EDGE ( 'NONE', *, *, #28265, .T. ) ;
#98789 = CARTESIAN_POINT ( 'NONE',  ( -42.20041562234357713, 435.2369744135580731, 7.788607701745519307 ) ) ;
#98788 = CARTESIAN_POINT ( 'NONE',  ( 2.499999999999999556, -8.000000000000000000, 17.89626171146327138 ) ) ;
#98790 = CARTESIAN_POINT ( 'NONE',  ( -12.52541344640442311, 5.240320085686820839, 8.131572623655657139 ) ) ;
#98791 = CARTESIAN_POINT ( 'NONE',  ( 14.83349330513380337, 1.593028355512270567E-15, 0.000000000000000000 ) ) ;
#98792 = CARTESIAN_POINT ( 'NONE',  ( -7.087005865465108911, 41.65067171707818261, -59.33604907184044919 ) ) ;
#98793 = CARTESIAN_POINT ( 'NONE',  ( 6.912476950049422086, 40.56175661822392442, -71.08408186712233601 ) ) ;
#98794 = CARTESIAN_POINT ( 'NONE',  ( -37.72755895515653890, 25.42103013220621577, 13.45617127781066280 ) ) ;
#98795 = CARTESIAN_POINT ( 'NONE',  ( 5.909155701201243893, -88.86261680188731304, 1.073778020691686486 ) ) ;
#98796 = DIRECTION ( 'NONE',  ( 0.000000000000000000, -1.000000000000000000, 0.000000000000000000 ) ) ;
#98797 = CARTESIAN_POINT ( 'NONE',  ( 110.7605312682850780, -60.00000000000000711, 149.8757700383887936 ) ) ;
#98798 = CARTESIAN_POINT ( 'NONE',  ( -7.000000000000002665, -46.47749919162729526, 39.12435565298215323 ) ) ;
#98799 = VECTOR ( 'NONE', #76551, 1000.000000000000000 ) ;
#98800 = CIRCLE ( 'NONE', #62654, 8.542937654374686218 ) ;
#98801 = B_SPLINE_CURVE_WITH_KNOTS ( 'NONE', 3,
 ( #42678, #35148, #66416, #82607 ),
 .UNSPECIFIED., .F., .F.,
 ( 4, 4 ),
 ( 4.718958039861916012E-17, 0.002256496660504680660 ),
 .UNSPECIFIED. ) ;
#98802 = CARTESIAN_POINT ( 'NONE',  ( -44.47534256803313468, -38.31161230092084224, 57.00189278798902137 ) ) ;
#98803 = ORIENTED_EDGE ( 'NONE', *, *, #4191, .F. ) ;
#98804 = EDGE_CURVE ( 'NONE', #56644, #52640, #43926, .T. ) ;
#98805 = CARTESIAN_POINT ( 'NONE',  ( -90.04282506516243245, -29.99999999999963407, 189.9068615740519590 ) ) ;
#98806 = ORIENTED_EDGE ( 'NONE', *, *, #90378, .T. ) ;
#98807 = CARTESIAN_POINT ( 'NONE',  ( 93.97977184163765685, 6.123233995736568081E-16, -5.000000000000011546 ) ) ;
#98808 = LINE ( 'NONE', #27105, #33981 ) ;
#98809 = CARTESIAN_POINT ( 'NONE',  ( 7.955551520411029642, 98.60650887776560580, 5.000000000000000888 ) ) ;
#98810 = CARTESIAN_POINT ( 'NONE',  ( -22.80797863425463490, 28.18718824344973228, -30.77216081686040283 ) ) ;
#98811 = AXIS2_PLACEMENT_3D ( 'NONE', #96203, #22332, #89160 ) ;
#98812 = CARTESIAN_POINT ( 'NONE',  ( -7.188101187500000044, -24.78125000204838813, -8.802885111219163269E-16 ) ) ;
#98813 = CARTESIAN_POINT ( 'NONE',  ( 14.27307692307692299, 1.411358822780289120E-15, 0.000000000000000000 ) ) ;
#98815 = EDGE_CURVE ( 'NONE', #87682, #92773, #54218, .T. ) ;
#98814 = CARTESIAN_POINT ( 'NONE',  ( 7.354130389523831468, 40.93126280921548243, -70.29718522916981271 ) ) ;
#98816 = ADVANCED_FACE ( 'NONE', ( #84662 ), #2661, .T. ) ;
#98817 = ORIENTED_EDGE ( 'NONE', *, *, #67494, .F. ) ;
#98819 = ORIENTED_EDGE ( 'NONE', *, *, #89297, .F. ) ;
#98818 = DIRECTION ( 'NONE',  ( 0.5735764363510491570, -0.8191520442889895781, 1.003171929053522035E-16 ) ) ;
#98820 = CARTESIAN_POINT ( 'NONE',  ( 79.31590203019780461, -53.37304251699236346, 157.6480627266177805 ) ) ;
#98821 = DIRECTION ( 'NONE',  ( -1.000000000000000000, 0.000000000000000000, 0.000000000000000000 ) ) ;
#98822 = ORIENTED_EDGE ( 'NONE', *, *, #41428, .F. ) ;
#98823 = DIRECTION ( 'NONE',  ( 0.000000000000000000, 0.000000000000000000, 1.000000000000000000 ) ) ;
#98824 = CARTESIAN_POINT ( 'NONE',  ( 38.81129420777568839, 27.30432117811967530, -12.34979214484390475 ) ) ;
#98825 = CARTESIAN_POINT ( 'NONE',  ( 7.551437640244097693, 26.99127537477090399, -2.648272645923380519 ) ) ;
#98826 = DIRECTION ( 'NONE',  ( -1.000000000000000000, 0.000000000000000000, -0.000000000000000000 ) ) ;
#98827 = CARTESIAN_POINT ( 'NONE',  ( -30.83208909486066318, 321.1666868008755955, 14.44335677805165119 ) ) ;
#98828 = DIRECTION ( 'NONE',  ( 0.000000000000000000, -1.000000000000000000, 0.000000000000000000 ) ) ;
#98829 = EDGE_CURVE ( 'NONE', #40330, #82202, #65021, .T. ) ;
#98830 = ORIENTED_EDGE ( 'NONE', *, *, #105476, .T. ) ;
#98831 = CARTESIAN_POINT ( 'NONE',  ( 46.85000000000000142, 0.000000000000000000, 0.000000000000000000 ) ) ;
#98832 = CARTESIAN_POINT ( 'NONE',  ( 12.49989493515518646, 18.64301898209307140, -36.27145154709465658 ) ) ;
#98833 = CARTESIAN_POINT ( 'NONE',  ( 86.51326442782708170, -53.78086573019226080, 192.4535467407390570 ) ) ;
#98834 = CARTESIAN_POINT ( 'NONE',  ( 0.6419170815367052363, 35.01568727531654446, -27.42424321200550352 ) ) ;
#98835 = CARTESIAN_POINT ( 'NONE',  ( 7.188101187500001821, -34.06250000204839523, -2.977408999572650483 ) ) ;
#98836 = CARTESIAN_POINT ( 'NONE',  ( 21.62698502147047819, -26.76882475084324042, 37.23665029981403052 ) ) ;
#98837 = CARTESIAN_POINT ( 'NONE',  ( -39.98667076425689260, 490.5869148090167187, 11.68052433275972746 ) ) ;
#98838 = CARTESIAN_POINT ( 'NONE',  ( -16.05785784214753775, 4.775831776487168945, 3.710403933803116949 ) ) ;
#98839 = ADVANCED_FACE ( 'NONE', ( #23535 ), #56317, .F. ) ;
#98840 = CARTESIAN_POINT ( 'NONE',  ( 36.61006234131809833, 439.8077055994807552, 24.20807427523271826 ) ) ;
#98841 =( GEOMETRIC_REPRESENTATION_CONTEXT ( 3 ) GLOBAL_UNCERTAINTY_ASSIGNED_CONTEXT ( ( #26150 ) ) GLOBAL_UNIT_ASSIGNED_CONTEXT ( ( #82847, #40789, #1915 ) ) REPRESENTATION_CONTEXT ( 'NONE', 'WORKASPACE' ) );
#98842 = SHAPE_DEFINITION_REPRESENTATION ( #59534, #19231 ) ;
#98843 = CARTESIAN_POINT ( 'NONE',  ( -9.221249107921748234, 31.04821371498486471, 3.869340886054256856 ) ) ;
#98844 = VERTEX_POINT ( 'NONE', #81190 ) ;
#98845 = CARTESIAN_POINT ( 'NONE',  ( 0.7854637262267426534, 43.26570879096288280, 18.48601689480677734 ) ) ;
#98846 = COLOUR_RGB ( '', 0.08235294, 0.09019608, 0.10196078) ;
#98847 = CARTESIAN_POINT ( 'NONE',  ( 82.70911704725124025, -5.000000000000000000, 0.000000000000000000 ) ) ;
#98848 = FACE_OUTER_BOUND ( 'NONE', #78347, .T. ) ;
#98849 = ORIENTED_EDGE ( 'NONE', *, *, #53996, .F. ) ;
#98850 = CARTESIAN_POINT ( 'NONE',  ( -42.19180677453720563, 462.2931784592651638, 3.389262873192010694 ) ) ;
#98851 = CARTESIAN_POINT ( 'NONE',  ( 112.9101767622411643, -57.67113815742245464, 187.8873526033939640 ) ) ;
#98852 = CARTESIAN_POINT ( 'NONE',  ( 36.18016141387847284, 463.3220971514209054, 20.09605424492473702 ) ) ;
#98853 = LINE ( 'NONE', #41705, #58775 ) ;
#98854 = CARTESIAN_POINT ( 'NONE',  ( 26.08349330513380337, 1.593028355512270567E-15, 0.000000000000000000 ) ) ;
#98855 = CARTESIAN_POINT ( 'NONE',  ( 19.00000000000000711, 4.000000000000000888, 25.00000000000000000 ) ) ;
#98856 = CARTESIAN_POINT ( 'NONE',  ( -77.66702251434536208, -59.99999999999999289, 192.1189785543494963 ) ) ;
#98857 = DIRECTION ( 'NONE',  ( -1.000000000000000000, 0.000000000000000000, 0.000000000000000000 ) ) ;
#98858 = FACE_OUTER_BOUND ( 'NONE', #84366, .T. ) ;
#98859 = CARTESIAN_POINT ( 'NONE',  ( -84.46326382266198607, -53.81991241739247300, 189.8031309934812327 ) ) ;
#98861 = VERTEX_POINT ( 'NONE', #73086 ) ;
#98860 = CIRCLE ( 'NONE', #5865, 3.309500000000001663 ) ;
#98862 = CARTESIAN_POINT ( 'NONE',  ( 28.19925613136460640, 308.7765882544961755, -9.111076883841365159 ) ) ;
#98863 = CONICAL_SURFACE ( 'NONE', #93739, 4.171999999999999709, 0.7853981633974603804 ) ;
#98864 = EDGE_LOOP ( 'NONE', ( #45003, #40860, #7383, #26514 ) ) ;
#98865 = DIRECTION ( 'NONE',  ( 0.000000000000000000, -1.000000000000000000, 0.000000000000000000 ) ) ;
#98866 = ADVANCED_FACE ( 'NONE', ( #25122 ), #106533, .T. ) ;
#98867 = CARTESIAN_POINT ( 'NONE',  ( -6.392921701574284299, 41.54610357429506706, -70.64273452805430509 ) ) ;
#98868 = CONICAL_SURFACE ( 'NONE', #81617, 4.000000000000001776, 0.9599310885968808105 ) ;
#98869 = CARTESIAN_POINT ( 'NONE',  ( -87.03135510228767657, -60.19613468631837350, -6.661356676301259050 ) ) ;
#98870 = CARTESIAN_POINT ( 'NONE',  ( -5.939725004866447833, -11.78992312938697218, -9.289959103330964751 ) ) ;
#98871 = ORIENTED_EDGE ( 'NONE', *, *, #89092, .T. ) ;
#98872 = CARTESIAN_POINT ( 'NONE',  ( 6.326445470157510798, 6.578717624163893163, -2.268395195563515543 ) ) ;
#98873 = CARTESIAN_POINT ( 'NONE',  ( 7.126148245860624009, 41.12758397993106740, -58.55282951229289523 ) ) ;
#98874 = EDGE_CURVE ( 'NONE', #58778, #87270, #105885, .T. ) ;
#98875 = CARTESIAN_POINT ( 'NONE',  ( 21.65942590380180022, -2.602085213965209853E-15, -5.820808985962528936 ) ) ;
#98876 = FACE_OUTER_BOUND ( 'NONE', #31214, .T. ) ;
#98877 = EDGE_CURVE ( 'NONE', #34973, #25863, #90423, .T. ) ;
#98878 = CARTESIAN_POINT ( 'NONE',  ( -8.180708021844917965, -14.21045842199436926, -37.25108655295423432 ) ) ;
#98879 = CARTESIAN_POINT ( 'NONE',  ( -76.80044675745622840, -49.90808875740508910, 137.4838826220702401 ) ) ;
#98880 = EDGE_LOOP ( 'NONE', ( #100048, #104264, #34499, #66802, #100960 ) ) ;
#98881 = CARTESIAN_POINT ( 'NONE',  ( 78.54417320222145804, -14.21045842199432307, 165.9036888455924270 ) ) ;
#98882 = CARTESIAN_POINT ( 'NONE',  ( 6.928203230275510549, 85.00000000000000000, 4.000000000000000000 ) ) ;
#98883 = CARTESIAN_POINT ( 'NONE',  ( 113.9274098329656084, -57.67114099918555326, 180.4894649156854598 ) ) ;
#98884 = ORIENTED_EDGE ( 'NONE', *, *, #65982, .T. ) ;
#98885 = LINE ( 'NONE', #16393, #104317 ) ;
#98886 = ADVANCED_FACE ( 'NONE', ( #90902 ), #14630, .T. ) ;
#98887 = FACE_OUTER_BOUND ( 'NONE', #3526, .T. ) ;
#98888 = VERTEX_POINT ( 'NONE', #98445 ) ;
#98889 = CARTESIAN_POINT ( 'NONE',  ( 1.306730854166997080, 14.06983854460715300, -6.878153045988232073 ) ) ;
#98890 = B_SPLINE_CURVE_WITH_KNOTS ( 'NONE', 3,
 ( #101093, #59051, #67671, #1303, #27251, #68750, #84387, #10475 ),
 .UNSPECIFIED., .F., .F.,
 ( 4, 2, 2, 4 ),
 ( 0.000000000000000000, 0.5000000000000000000, 0.7500000000000000000, 1.000000000000000000 ),
 .UNSPECIFIED. ) ;
#98891 = EDGE_CURVE ( 'NONE', #54176, #4111, #48162, .T. ) ;
#98892 = CARTESIAN_POINT ( 'NONE',  ( 30.00000000000000000, 500.0000000000002274, -5.000000000000001776 ) ) ;
#98893 = DIRECTION ( 'NONE',  ( 0.000000000000000000, 0.000000000000000000, 1.000000000000000000 ) ) ;
#98894 = CARTESIAN_POINT ( 'NONE',  ( 7.188101187500001821, -19.06250000204838813, -2.977408999572650483 ) ) ;
#98895 = EDGE_CURVE ( 'NONE', #77883, #57259, #28482, .T. ) ;
#98896 = CARTESIAN_POINT ( 'NONE',  ( 10.01915592506146879, 302.6453132215669939, -2.043889601136144485 ) ) ;
#98897 = CARTESIAN_POINT ( 'NONE',  ( 9.253817200599835147, 83.70007270083139872, -3.791916801615157873 ) ) ;
#98898 = SURFACE_STYLE_FILL_AREA ( #24009 ) ;
#98899 = FACE_OUTER_BOUND ( 'NONE', #14091, .T. ) ;
#98900 = CARTESIAN_POINT ( 'NONE',  ( 23.21751746555303342, -1.200000000000000030E-05, 31.95617127781017075 ) ) ;
#98901 = AXIS2_PLACEMENT_3D ( 'NONE', #89654, #15755, #82620 ) ;
#98902 = ORIENTED_EDGE ( 'NONE', *, *, #10751, .T. ) ;
#98903 = CARTESIAN_POINT ( 'NONE',  ( -7.071721883978239198, 41.30029441324972339, -70.42654640881200123 ) ) ;
#98904 = CARTESIAN_POINT ( 'NONE',  ( 31.54446617496518712, -49.90305043662050366, 35.58892852745655233 ) ) ;
#98905 = CARTESIAN_POINT ( 'NONE',  ( 32.16569164323090035, 318.9480643375377440, -5.577539070780133557 ) ) ;
#98906 = ORIENTED_EDGE ( 'NONE', *, *, #50250, .T. ) ;
#98907 = CARTESIAN_POINT ( 'NONE',  ( 33.94783393359906398, 484.1261039197348737, 1.321740980885009353 ) ) ;
#98908 = ORIENTED_EDGE ( 'NONE', *, *, #101267, .T. ) ;
#98910 = CARTESIAN_POINT ( 'NONE',  ( -0.4138759434715034158, 44.05905633758010964, -16.31753750977479811 ) ) ;
#98909 = FACE_OUTER_BOUND ( 'NONE', #74337, .T. ) ;
#98911 = PLANE ( 'NONE',  #92211 ) ;
#98912 = CARTESIAN_POINT ( 'NONE',  ( 0.000000000000000000, 35.00000000000000000, -11.18527996897366528 ) ) ;
#98913 = CIRCLE ( 'NONE', #5913, 4.000000000000001776 ) ;
#98914 = DIRECTION ( 'NONE',  ( 0.8191520442889974607, 1.003171929053531649E-16, -0.5735764363510379438 ) ) ;
#98915 = DIRECTION ( 'NONE',  ( 0.000000000000000000, 1.000000000000000000, 0.000000000000000000 ) ) ;
#98916 = CARTESIAN_POINT ( 'NONE',  ( 0.5340534162559666953, 13.17884539425582346, -51.63681601966053591 ) ) ;
#98917 = EDGE_LOOP ( 'NONE', ( #70432, #33795 ) ) ;
#98918 = CARTESIAN_POINT ( 'NONE',  ( 92.74135359634635734, -60.00000000000000000, -6.602453662847219462 ) ) ;
#98919 = FACE_OUTER_BOUND ( 'NONE', #21530, .T. ) ;
#98920 = AXIS2_PLACEMENT_3D ( 'NONE', #30374, #46015, #78894 ) ;
#98921 = CARTESIAN_POINT ( 'NONE',  ( -15.66596225472208914, -1.206787384264950580, 14.95386751741624920 ) ) ;
#98922 = CARTESIAN_POINT ( 'NONE',  ( 12.08334041755991706, 304.5866437775407007, -10.05636128505472726 ) ) ;
#98923 = DIRECTION ( 'NONE',  ( 0.000000000000000000, -1.000000000000000000, 0.000000000000000000 ) ) ;
#98924 = ORIENTED_EDGE ( 'NONE', *, *, #8535, .F. ) ;
#98925 = CARTESIAN_POINT ( 'NONE',  ( -36.35825146749015602, 28.12716662175846949, 12.56482682837719977 ) ) ;
#98926 = ORIENTED_EDGE ( 'NONE', *, *, #70467, .T. ) ;
#98927 = EDGE_LOOP ( 'NONE', ( #65177, #46792, #29506, #50692, #3019, #4094 ) ) ;
#98928 = CARTESIAN_POINT ( 'NONE',  ( 9.491091496279695579E-16, 54.30758622938872549, 7.749999999999999112 ) ) ;
#98929 = CARTESIAN_POINT ( 'NONE',  ( 28.49160136855818948, 41.56004681549217139, -71.33052401751463378 ) ) ;
#98930 = CARTESIAN_POINT ( 'NONE',  ( -16.34909811654727818, 34.35725799356371368, -24.24308462023440214 ) ) ;
#98931 = CARTESIAN_POINT ( 'NONE',  ( 32.13832923886224080, 335.6472655370285452, 17.84808702340633602 ) ) ;
#98932 = CARTESIAN_POINT ( 'NONE',  ( 83.10245286683164068, -37.83958788250053829, -2.435592654216626851 ) ) ;
#98933 = CARTESIAN_POINT ( 'NONE',  ( -36.51946503641791253, 336.4369612853828357, -1.859061548502462857 ) ) ;
#98934 = CARTESIAN_POINT ( 'NONE',  ( -3.195909155964999027, -68.75976616688309662, 13.04431807157711454 ) ) ;
#98935 = CARTESIAN_POINT ( 'NONE',  ( 12.50000000000000711, 41.41911216696205855, -74.42394764531675833 ) ) ;
#98936 = ORIENTED_EDGE ( 'NONE', *, *, #6733, .F. ) ;
#98938 = EDGE_CURVE ( 'NONE', #48619, #31429, #57676, .T. ) ;
#98937 = CARTESIAN_POINT ( 'NONE',  ( 30.63590201688485593, 10.93049107008198817, 40.03749794393651484 ) ) ;
#98939 = EDGE_LOOP ( 'NONE', ( #63638, #84050, #36307, #5241, #59721 ) ) ;
#98940 = CARTESIAN_POINT ( 'NONE',  ( 8.717352708370867731, 51.77858799192747341, -1.531152949374622985 ) ) ;
#98941 = DIRECTION ( 'NONE',  ( 0.000000000000000000, 0.000000000000000000, 1.000000000000000000 ) ) ;
#98942 = CARTESIAN_POINT ( 'NONE',  ( 3.866514940527741029, -48.81811806873775339, 103.9726926151936652 ) ) ;
#98944 = ORIENTED_EDGE ( 'NONE', *, *, #1768, .T. ) ;
#98943 = CARTESIAN_POINT ( 'NONE',  ( -14.60449729785899464, -60.00000000000003553, 34.00514524257540927 ) ) ;
#98945 = CARTESIAN_POINT ( 'NONE',  ( 70.22185649915901706, -49.90760283489759530, 108.7999883389251181 ) ) ;
#98946 = COLOUR_RGB ( '', 0.72549020, 0.75294118, 0.79215686) ;
#98947 = ORIENTED_EDGE ( 'NONE', *, *, #100585, .F. ) ;
#98948 =( NAMED_UNIT ( * ) SI_UNIT ( $, .STERADIAN. ) SOLID_ANGLE_UNIT ( ) );
#98949 = CARTESIAN_POINT ( 'NONE',  ( 4.401442555609581635E-16, -29.28125000204838813, -7.188101187500000044 ) ) ;
#98950 = CIRCLE ( 'NONE', #12799, 4.000000000000003553 ) ;
#98951 = CARTESIAN_POINT ( 'NONE',  ( -94.70367724826090239, -57.65721615037961811, -8.919493359160306056 ) ) ;
#98952 = PRODUCT_DEFINITION_FORMATION_WITH_SPECIFIED_SOURCE ( 'ANY', '', #14592, .NOT_KNOWN. ) ;
#98954 = ORIENTED_EDGE ( 'NONE', *, *, #7287, .T. ) ;
#98953 = CIRCLE ( 'NONE', #88588, 4.000000000000000888 ) ;
#98955 = CARTESIAN_POINT ( 'NONE',  ( -37.54559764570181812, 464.1143081516144662, 19.43664670202813838 ) ) ;
#98956 = CARTESIAN_POINT ( 'NONE',  ( -36.13333162057816139, 491.8038228668677903, 12.56276695383520092 ) ) ;
#98957 = EDGE_CURVE ( 'NONE', #54096, #60365, #74847, .T. ) ;
#98958 = DIRECTION ( 'NONE',  ( 1.000000000000000000, 0.000000000000000000, 0.000000000000000000 ) ) ;
#98959 = CARTESIAN_POINT ( 'NONE',  ( -8.000000000000000000, -22.53125000409677980, -3.313708498984762496 ) ) ;
#98960 = DIRECTION ( 'NONE',  ( -0.5735764363510510444, -0.8191520442889883569, 0.000000000000000000 ) ) ;
#98961 = FACE_OUTER_BOUND ( 'NONE', #3349, .T. ) ;
#98962 = EDGE_CURVE ( 'NONE', #73621, #28073, #23232, .T. ) ;
#98963 = CARTESIAN_POINT ( 'NONE',  ( 9.165151389911679658, 30.26295510916337150, 3.999999999999999112 ) ) ;
#98964 = CARTESIAN_POINT ( 'NONE',  ( -17.24303157407923237, 294.5700599009814482, 9.877113118490870036 ) ) ;
#98965 = FILL_AREA_STYLE ('',( #74695 ) ) ;
#98966 = VERTEX_POINT ( 'NONE', #52021 ) ;
#98967 = CARTESIAN_POINT ( 'NONE',  ( 1.250000000000000444, -7.938566201357371455, -7.198902722707432922 ) ) ;
#98968 = CARTESIAN_POINT ( 'NONE',  ( -6.499999999999999112, 3.752776749732556816, -0.7999999999999821698 ) ) ;
#98969 = CARTESIAN_POINT ( 'NONE',  ( 4.633946686836865503, -60.00000000000000000, 39.63006500553967726 ) ) ;
#98970 = CARTESIAN_POINT ( 'NONE',  ( -91.23729876660307525, -30.00000000000000355, 190.5897172708922369 ) ) ;
#98971 = VECTOR ( 'NONE', #38736, 1000.000000000000000 ) ;
#98972 = DIRECTION ( 'NONE',  ( 0.000000000000000000, -1.000000000000000000, 0.000000000000000000 ) ) ;
#98973 = CARTESIAN_POINT ( 'NONE',  ( 73.86186822093814897, -57.61872494714916115, 186.3625796096756915 ) ) ;
#98975 = CARTESIAN_POINT ( 'NONE',  ( 19.61638200451619696, 1.340359594676612611E-15, 0.000000000000000000 ) ) ;
#98974 = CARTESIAN_POINT ( 'NONE',  ( 4.699999999999999289, -3.752776749732578132, -6.500000000000000888 ) ) ;
#98976 = CARTESIAN_POINT ( 'NONE',  ( 9.893172293432595410, -22.59654125385418766, -38.54281256708559766 ) ) ;
#98977 = SURFACE_SIDE_STYLE ('',( #81726 ) ) ;
#98980 = B_SPLINE_CURVE_WITH_KNOTS ( 'NONE', 3,
 ( #1514, #50081, #51136, #34482 ),
 .UNSPECIFIED., .F., .F.,
 ( 4, 4 ),
 ( 1.734723475976807094E-17, 0.003262827847960974702 ),
 .UNSPECIFIED. ) ;
#98979 = AXIS2_PLACEMENT_3D ( 'NONE', #10280, #2177, #82032 ) ;
#98978 = PRODUCT_DEFINITION ( 'UNKNOWN', '', #47295, #43483 ) ;
#98981 = CARTESIAN_POINT ( 'NONE',  ( -32.82504303899613518, -60.00000000000001421, 44.72063024855318503 ) ) ;
#98982 = CIRCLE ( 'NONE', #11216, 4.000000000000001776 ) ;
#98983 = CIRCLE ( 'NONE', #92077, 6.500000000000000000 ) ;
#98984 = CIRCLE ( 'NONE', #66283, 4.000000000000000888 ) ;
#98985 = CARTESIAN_POINT ( 'NONE',  ( 11.69631794847444617, 16.06060599891873508, 9.527053589674022049 ) ) ;
#98986 = CARTESIAN_POINT ( 'NONE',  ( 36.02493936428268029, 463.3371199957072690, 20.06709031638022367 ) ) ;
#98987 = CARTESIAN_POINT ( 'NONE',  ( -86.58206345380148150, -50.13197549991983237, 191.4801916809975637 ) ) ;
#98988 = ORIENTED_EDGE ( 'NONE', *, *, #73802, .F. ) ;
#98989 = CARTESIAN_POINT ( 'NONE',  ( 18.91769957617489695, 48.49892424866627039, 62.17828500952007431 ) ) ;
#98990 = CARTESIAN_POINT ( 'NONE',  ( 8.000000000000000000, -12.40624999999999289, -3.313708498984761164 ) ) ;
#98991 = CARTESIAN_POINT ( 'NONE',  ( -8.311032557564669077, -56.88425799153385753, 33.36415341410724977 ) ) ;
#98992 = VECTOR ( 'NONE', #35322, 1000.000000000000227 ) ;
#98993 =( BOUNDED_SURFACE ( )  B_SPLINE_SURFACE ( 3, 3, ( 
 ( #45625, #79038, #37561, #95759 ),
 ( #21898, #70427, #13756, #54743 ),
 ( #103323, #38089, #103839, #86631 ),
 ( #78499, #87676, #60753, #29471 ) ),
 .UNSPECIFIED., .F., .F., .T. ) 
 B_SPLINE_SURFACE_WITH_KNOTS ( ( 4, 4 ),
 ( 4, 4 ),
 ( 0.000000000000000000, 1.000000000000000000 ),
 ( 0.000000000000000000, 1.000000000000000000 ),
 .UNSPECIFIED. ) 
 GEOMETRIC_REPRESENTATION_ITEM ( )  RATIONAL_B_SPLINE_SURFACE ( (
 ( 1.000000000000000000, 0.3333333333333334259, 0.3333333333333334259, 1.000000000000000000),
 ( 1.000000000000000000, 0.3333333333333334259, 0.3333333333333334259, 1.000000000000000000),
 ( 1.000000000000000000, 0.3333333333333334259, 0.3333333333333334259, 1.000000000000000000),
 ( 1.000000000000000000, 0.3333333333333334259, 0.3333333333333334259, 1.000000000000000000) ) ) 
 REPRESENTATION_ITEM ( '' )  SURFACE ( )  );
#98995 = CARTESIAN_POINT ( 'NONE',  ( 4.856083419063446094, -65.85369684545175062, 13.84668161063944503 ) ) ;
#98994 = CARTESIAN_POINT ( 'NONE',  ( 6.878751942472529635, -3.924677726130942457, -6.573129608219093534 ) ) ;
#98996 = EDGE_LOOP ( 'NONE', ( #85129, #76402, #85944, #72044, #70753 ) ) ;
#98997 = CARTESIAN_POINT ( 'NONE',  ( -7.347171990171222689, -3.439186728100687596, -18.43985286355804831 ) ) ;
#98998 = LINE ( 'NONE', #57478, #51620 ) ;
#98999 = CARTESIAN_POINT ( 'NONE',  ( 29.10832111663954791, 306.8131183972279814, -9.108704873592294859 ) ) ;
#99000 = CARTESIAN_POINT ( 'NONE',  ( 4.022544416453469829, -48.63060458932351793, 103.0357414394656104 ) ) ;
#99001 = EDGE_CURVE ( 'NONE', #16154, #103256, #42140, .T. ) ;
#99002 = CARTESIAN_POINT ( 'NONE',  ( -7.151597709147949011, -83.21070734947784331, 3.587174531012140566 ) ) ;
#99003 = SURFACE_SIDE_STYLE ('',( #106578 ) ) ;
#99004 = CARTESIAN_POINT ( 'NONE',  ( 104.9451034742319706, -14.21045842199432663, 145.4709692194043669 ) ) ;
#99005 = CARTESIAN_POINT ( 'NONE',  ( 8.082668874372532400E-15, 79.50000000000000000, 66.00000000000000000 ) ) ;
#99006 = ORIENTED_EDGE ( 'NONE', *, *, #98234, .F. ) ;
#99007 = DIRECTION ( 'NONE',  ( -1.000000000000000000, -0.000000000000000000, -0.000000000000000000 ) ) ;
#99008 = DIRECTION ( 'NONE',  ( 1.000000000000000000, 1.224606353822377258E-16, 0.000000000000000000 ) ) ;
#99009 = FACE_OUTER_BOUND ( 'NONE', #52268, .T. ) ;
#99010 = CARTESIAN_POINT ( 'NONE',  ( -7.500000000000000888, -3.000671055698259870, -20.99923901233272971 ) ) ;
#99011 = CARTESIAN_POINT ( 'NONE',  ( 43.65158569082660733, 382.1618310280565538, 15.13503673623559820 ) ) ;
#99012 = CARTESIAN_POINT ( 'NONE',  ( 43.70836520789914914, 463.8610993545788119, 7.295416580059431055 ) ) ;
#99013 = ORIENTED_EDGE ( 'NONE', *, *, #57481, .T. ) ;
#99014 = UNCERTAINTY_MEASURE_WITH_UNIT (LENGTH_MEASURE( 1.000000000000000082E-05 ), #48405, 'distance_accuracy_value', 'NONE');
#99015 = CARTESIAN_POINT ( 'NONE',  ( -21.93428938517136118, 305.2394520450566233, 9.020384747005401493 ) ) ;
#99016 = EDGE_CURVE ( 'NONE', #43396, #45302, #35351, .T. ) ;
#99017 = ORIENTED_EDGE ( 'NONE', *, *, #27110, .F. ) ;
#99018 = CARTESIAN_POINT ( 'NONE',  ( 36.09356709110171124, 485.3869947698531178, -3.408842397901690635 ) ) ;
#99019 = AXIS2_PLACEMENT_3D ( 'NONE', #94894, #101896, #37201 ) ;
#99020 = EDGE_CURVE ( 'NONE', #1420, #51255, #9405, .T. ) ;
#99021 = SURFACE_STYLE_FILL_AREA ( #79272 ) ;
#99022 = CARTESIAN_POINT ( 'NONE',  ( 10.20373343965789381, 45.40217293244036512, 15.40779740156149735 ) ) ;
#99023 = ORIENTED_EDGE ( 'NONE', *, *, #10630, .T. ) ;
#99024 = CARTESIAN_POINT ( 'NONE',  ( 5.957442974701732119, 48.00000000000000000, 65.00000000000000000 ) ) ;
#99025 = CARTESIAN_POINT ( 'NONE',  ( 6.081241251370853362, -12.38970427209928005, 12.35256966254937971 ) ) ;
#99026 = CARTESIAN_POINT ( 'NONE',  ( -68.94556730486883112, -59.99999999997069722, 149.4068084800686904 ) ) ;
#99027 = CARTESIAN_POINT ( 'NONE',  ( 45.99999999999999289, 436.0322433031492437, 12.60696238181549234 ) ) ;
#99028 = VERTEX_POINT ( 'NONE', #84404 ) ;
#99029 = CARTESIAN_POINT ( 'NONE',  ( 99.83762202063759617, -60.00000000000000000, 80.07466358523365102 ) ) ;
#99031 = CARTESIAN_POINT ( 'NONE',  ( 17.45845221745307541, -18.58884928908958400, 27.26027009539929935 ) ) ;
#99030 = CARTESIAN_POINT ( 'NONE',  ( -78.26172670240529783, -14.21045842199445275, 161.8221046207387985 ) ) ;
#99032 = CARTESIAN_POINT ( 'NONE',  ( 82.55061241810440720, -37.99999999999995026, -12.61180328641926174 ) ) ;
#99033 = CARTESIAN_POINT ( 'NONE',  ( 0.6428726534874711351, 53.45391827455260625, -10.07519478865332196 ) ) ;
#99034 = CARTESIAN_POINT ( 'NONE',  ( -42.02556652957100880, -36.07178335321912499, 39.65759594440722680 ) ) ;
#99035 = CARTESIAN_POINT ( 'NONE',  ( -34.45841046840646982, 18.64284798593094550, 17.01587130353618704 ) ) ;
#99036 = VERTEX_POINT ( 'NONE', #35891 ) ;
#99037 = DIRECTION ( 'NONE',  ( 0.000000000000000000, 0.000000000000000000, -1.000000000000000000 ) ) ;
#99038 = CARTESIAN_POINT ( 'NONE',  ( 8.349999999999999645, 1.411358822780289120E-15, 0.000000000000000000 ) ) ;
#99039 = CARTESIAN_POINT ( 'NONE',  ( 22.42417502586373246, 305.3961751430792333, 10.05444931189341773 ) ) ;
#99040 = CARTESIAN_POINT ( 'NONE',  ( 0.000000000000000000, 0.000000000000000000, 4.000000000000000000 ) ) ;
#99041 = CARTESIAN_POINT ( 'NONE',  ( -3.313708498984756723, -28.15625000409677270, 8.000000000000008882 ) ) ;
#99042 = CARTESIAN_POINT ( 'NONE',  ( 0.000000000000000000, 70.00000000000000000, 0.000000000000000000 ) ) ;
#99043 = EDGE_LOOP ( 'NONE', ( #28207, #25421, #51564, #103869 ) ) ;
#99044 = CARTESIAN_POINT ( 'NONE',  ( 5.803898591548438901, -46.53140123172246945, 103.8893302396402589 ) ) ;
#99045 = ORIENTED_EDGE ( 'NONE', *, *, #35630, .F. ) ;
#99046 = CIRCLE ( 'NONE', #56231, 5.000000000000001776 ) ;
#99047 = CARTESIAN_POINT ( 'NONE',  ( 80.09155444759548459, -30.00000000000000000, -13.68037423625693627 ) ) ;
#99048 = CARTESIAN_POINT ( 'NONE',  ( 19.24594220831874836, 41.87959112737684109, -80.73234005663204016 ) ) ;
#99049 = UNCERTAINTY_MEASURE_WITH_UNIT (LENGTH_MEASURE( 1.000000000000000082E-05 ), #6295, 'distance_accuracy_value', 'NONE');
#99050 = CARTESIAN_POINT ( 'NONE',  ( 23.38273396131690518, 25.95242824884117283, -30.70617127781076405 ) ) ;
#99051 = CARTESIAN_POINT ( 'NONE',  ( 51.01037695545453232, 500.0000000000002274, 0.000000000000000000 ) ) ;
#99052 = CARTESIAN_POINT ( 'NONE',  ( 97.89039143310566260, -30.00000000000000000, 136.7614787515506691 ) ) ;
#99053 = CARTESIAN_POINT ( 'NONE',  ( 7.046289519167718396, 103.6940818005561908, -3.789821819998814512 ) ) ;
#99054 = VERTEX_POINT ( 'NONE', #9969 ) ;
#99055 = ORIENTED_EDGE ( 'NONE', *, *, #78805, .T. ) ;
#99056 = ORIENTED_EDGE ( 'NONE', *, *, #5854, .T. ) ;
#99057 = CARTESIAN_POINT ( 'NONE',  ( -5.500000000000006217, 42.00000000000000000, -59.88032989329961708 ) ) ;
#99058 = CARTESIAN_POINT ( 'NONE',  ( 22.57676703600024837, 26.08017106655005790, 30.86991111420691425 ) ) ;
#99059 = CARTESIAN_POINT ( 'NONE',  ( 43.03357534759661718, 463.2291678140137492, 4.675918524166122303 ) ) ;
#99060 = AXIS2_PLACEMENT_3D ( 'NONE', #74264, #339, #106632 ) ;
#99061 = SURFACE_SIDE_STYLE ('',( #16035 ) ) ;
#99062 = CARTESIAN_POINT ( 'NONE',  ( -31.14081447784786505, 433.9613651262616827, 24.00306230370002325 ) ) ;
#99063 = FACE_BOUND ( 'NONE', #4305, .T. ) ;
#99064 = ORIENTED_EDGE ( 'NONE', *, *, #86267, .F. ) ;
#99066 = EDGE_CURVE ( 'NONE', #87833, #53038, #83483, .T. ) ;
#99065 = CARTESIAN_POINT ( 'NONE',  ( 42.21835935851049726, 436.4384481632509392, 19.62208033733266888 ) ) ;
#99067 = ORIENTED_EDGE ( 'NONE', *, *, #20641, .F. ) ;
#99068 = LINE ( 'NONE', #58090, #94929 ) ;
#99069 = CARTESIAN_POINT ( 'NONE',  ( 79.61952492946029736, -38.75123715105880962, 192.2766210044055981 ) ) ;
#99070 = CARTESIAN_POINT ( 'NONE',  ( 6.445370176743034918, 7.262437273742029298, -1.101027156350743663 ) ) ;
#99071 = AXIS2_PLACEMENT_3D ( 'NONE', #13038, #28763, #37905 ) ;
#99072 = CARTESIAN_POINT ( 'NONE',  ( 33.31031872651021075, 302.0743058889032113, 11.59258997849307526 ) ) ;
#99073 = AXIS2_PLACEMENT_3D ( 'NONE', #71297, #95585, #22780 ) ;
#99074 =( NAMED_UNIT ( * ) PLANE_ANGLE_UNIT ( ) SI_UNIT ( $, .RADIAN. ) );
#99075 = CIRCLE ( 'NONE', #28523, 4.000000000000007105 ) ;
#99076 = CIRCLE ( 'NONE', #61157, 5.000000000000010658 ) ;
#99077 = CIRCLE ( 'NONE', #886, 6.999999999999982236 ) ;
#99078 = CARTESIAN_POINT ( 'NONE',  ( -28.35171477237968318, 34.21495322681006712, -8.616345005959455960 ) ) ;
#99079 = CARTESIAN_POINT ( 'NONE',  ( 42.77045538396055946, 384.7557768097599364, 19.23094703895946012 ) ) ;
#99080 = EDGE_CURVE ( 'NONE', #100006, #60457, #34823, .T. ) ;
#99081 = LINE ( 'NONE', #34933, #66981 ) ;
#99082 = FACE_OUTER_BOUND ( 'NONE', #53046, .T. ) ;
#99083 = VERTEX_POINT ( 'NONE', #68770 ) ;
#99085 = CARTESIAN_POINT ( 'NONE',  ( -24.84125933061083558, 295.6108665521396119, 2.099934395011584520 ) ) ;
#99084 =( NAMED_UNIT ( * ) SI_UNIT ( $, .STERADIAN. ) SOLID_ANGLE_UNIT ( ) );
#99086 = UNCERTAINTY_MEASURE_WITH_UNIT (LENGTH_MEASURE( 1.000000000000000082E-05 ), #9638, 'distance_accuracy_value', 'NONE');
#99087 = FACE_BOUND ( 'NONE', #9288, .T. ) ;
#99088 = CARTESIAN_POINT ( 'NONE',  ( -4.912105445019744998, -10.03270236560008932, 6.401603053965017054 ) ) ;
#99089 = DIRECTION ( 'NONE',  ( -1.000000000000000000, -1.224606353822377258E-16, -0.000000000000000000 ) ) ;
#99090 = CARTESIAN_POINT ( 'NONE',  ( 9.017160581220602822, 295.0459686547099523, 4.334444195353072793 ) ) ;
#99091 = CARTESIAN_POINT ( 'NONE',  ( 46.00000000000000000, 464.2883104330365995, 11.80345442597034555 ) ) ;
#99092 = CARTESIAN_POINT ( 'NONE',  ( 84.96757647266667846, -50.19333676378905551, 189.1419654610012628 ) ) ;
#99093 = CARTESIAN_POINT ( 'NONE',  ( 0.1546360390246568628, 18.85543002168095938, 49.25752556588032860 ) ) ;
#99094 = EDGE_CURVE ( 'NONE', #45425, #50509, #76829, .T. ) ;
#99095 = PRESENTATION_STYLE_ASSIGNMENT (( #83457 ) ) ;
#99096 = ORIENTED_EDGE ( 'NONE', *, *, #100717, .F. ) ;
#99097 = CARTESIAN_POINT ( 'NONE',  ( 93.07912069066024685, -57.65568903999214001, -17.02304421024389924 ) ) ;
#99098 = B_SPLINE_CURVE_WITH_KNOTS ( 'NONE', 3,
 ( #82091, #74000, #90734, #16850, #8739, #53464, #3313, #35178, #70175, #20622, #102001, #37312, #52926, #103080, #43768, #35721, #77204, #29232, #86383, #93923, #43246, #78259, #76659, #4371, #60513, #36259, #28160, #85852, #61573, #76131, #94465, #61035, #62109, #3853 ),
 .UNSPECIFIED., .F., .F.,
 ( 4, 2, 2, 2, 2, 2, 2, 2, 2, 2, 2, 2, 2, 2, 2, 2, 4 ),
 ( 0.000000000000000000, 0.0007951492273476392899, 0.001590298454695278580, 0.002385447682042917544, 0.003180596909390557159, 0.003975746136738196775, 0.004770895364085835089, 0.005566044591433475137, 0.006361193818781114319, 0.007156343046128752633, 0.007951492273476393549, 0.008746641500824030996, 0.009541790728171668443, 0.01033693995551930589, 0.01113208918286694334, 0.01192723841021458252, 0.01272238763756221996 ),
 .UNSPECIFIED. ) ;
#99099 = DIRECTION ( 'NONE',  ( 0.000000000000000000, -0.3420201433256725987, -0.9396926207859068736 ) ) ;
#99100 = DIRECTION ( 'NONE',  ( 0.000000000000000000, -1.000000000000000000, 0.000000000000000000 ) ) ;
#99101 = DIRECTION ( 'NONE',  ( -1.000000000000000000, -1.224606353822377258E-16, -0.000000000000000000 ) ) ;
#99102 = AXIS2_PLACEMENT_3D ( 'NONE', #12488, #11421, #45941 ) ;
#99103 = EDGE_CURVE ( 'NONE', #66879, #79335, #22428, .T. ) ;
#99104 = CARTESIAN_POINT ( 'NONE',  ( -81.36966163465557145, -30.00000000000000000, -1.517807414885295580 ) ) ;
#99105 = CARTESIAN_POINT ( 'NONE',  ( 0.000000000000000000, 0.000000000000000000, 0.000000000000000000 ) ) ;
#99106 = CARTESIAN_POINT ( 'NONE',  ( -6.819782170910313468, 41.52802923942638103, -70.37695045795369708 ) ) ;
#99107 = FACE_OUTER_BOUND ( 'NONE', #37844, .T. ) ;
#99108 = CARTESIAN_POINT ( 'NONE',  ( -32.96117425224259989, 439.7497740807306741, 24.15381775812842946 ) ) ;
#99109 = DIRECTION ( 'NONE',  ( 0.000000000000000000, 0.000000000000000000, 1.000000000000000000 ) ) ;
#99110 = CARTESIAN_POINT ( 'NONE',  ( 33.52307692307692122, 4.172000000000003261, 5.109226446042759579E-16 ) ) ;
#99111 = CARTESIAN_POINT ( 'NONE',  ( 0.000000000000000000, 0.000000000000000000, 0.000000000000000000 ) ) ;
#99112 = CARTESIAN_POINT ( 'NONE',  ( 5.075566108724593128, -4.332661967060489339, -17.09624963492156269 ) ) ;
#99113 = CARTESIAN_POINT ( 'NONE',  ( 34.16642289233210050, 464.7650419733888043, 19.36631221618525345 ) ) ;
#99114 = CARTESIAN_POINT ( 'NONE',  ( -43.75010090113929806, 464.8337800386750018, 11.75004750934965791 ) ) ;
#99115 = CARTESIAN_POINT ( 'NONE',  ( 10.41054107240687188, -5.000000000000000888, 6.123233995736769241E-16 ) ) ;
#99116 = AXIS2_PLACEMENT_3D ( 'NONE', #36308, #12492, #78300 ) ;
#99117 = EDGE_CURVE ( 'NONE', #60981, #27380, #89255, .T. ) ;
#99118 = ORIENTED_EDGE ( 'NONE', *, *, #15394, .F. ) ;
#99119 = CARTESIAN_POINT ( 'NONE',  ( 5.834906339164278144, 11.94543000914187303, -3.867544450381311005 ) ) ;
#99120 = DIRECTION ( 'NONE',  ( -1.000000000000000000, 0.000000000000000000, 0.000000000000000000 ) ) ;
#99121 = CARTESIAN_POINT ( 'NONE',  ( -7.151597709147946347, 83.21070734947782910, 3.587174531012138790 ) ) ;
#99122 = CARTESIAN_POINT ( 'NONE',  ( -46.15551534976521708, -26.57306916659460683, -28.92868944221968164 ) ) ;
#99124 = CARTESIAN_POINT ( 'NONE',  ( -69.47170429735781738, -60.22820986096264306, -26.63212845803639084 ) ) ;
#99123 = CARTESIAN_POINT ( 'NONE',  ( 0.000000000000000000, 0.000000000000000000, 0.000000000000000000 ) ) ;
#99125 = AXIS2_PLACEMENT_3D ( 'NONE', #97608, #74925, #90600 ) ;
#99126 = VERTEX_POINT ( 'NONE', #36943 ) ;
#99127 = CYLINDRICAL_SURFACE ( 'NONE', #97840, 1.250000000000001110 ) ;
#99128 = VERTEX_POINT ( 'NONE', #12611 ) ;
#99129 = CARTESIAN_POINT ( 'NONE',  ( 41.98130293123185197, 462.0609698853055534, 3.143960326150163187 ) ) ;
#99130 = CARTESIAN_POINT ( 'NONE',  ( 11.29895642217514684, 43.19531110207578450, -14.89530219903277519 ) ) ;
#99131 = DIRECTION ( 'NONE',  ( -0.000000000000000000, -0.000000000000000000, 1.000000000000000000 ) ) ;
#99132 = B_SPLINE_CURVE_WITH_KNOTS ( 'NONE', 3,
 ( #39303, #65146, #106119, #81313, #22609, #80254, #57564, #32275, #7425, #81841 ),
 .UNSPECIFIED., .F., .F.,
 ( 4, 2, 2, 2, 4 ),
 ( -5.999999999154135157E-08, 0.002478699646394690818, 0.004957459292789372605, 0.009914978585578743120, 0.01983001717115747548 ),
 .UNSPECIFIED. ) ;
#99133 =( GEOMETRIC_REPRESENTATION_CONTEXT ( 3 ) GLOBAL_UNCERTAINTY_ASSIGNED_CONTEXT ( ( #89517 ) ) GLOBAL_UNIT_ASSIGNED_CONTEXT ( ( #714, #41216, #58474 ) ) REPRESENTATION_CONTEXT ( 'NONE', 'WORKASPACE' ) );
#99134 = CARTESIAN_POINT ( 'NONE',  ( -49.88581133959984726, -60.00000000000000711, -37.92708229162208511 ) ) ;
#99135 = EDGE_LOOP ( 'NONE', ( #67847, #22952, #34846 ) ) ;
#99136 = CARTESIAN_POINT ( 'NONE',  ( 0.5805565836007605673, -3.752776749732561257, 6.500000000000000000 ) ) ;
#99137 = CIRCLE ( 'NONE', #71582, 17.00000000000000000 ) ;
#99138 = CARTESIAN_POINT ( 'NONE',  ( -43.99980723760477730, 434.6400489724846921, 17.20555692211243581 ) ) ;
#99139 = CIRCLE ( 'NONE', #42336, 8.605212085995399107 ) ;
#99140 = CARTESIAN_POINT ( 'NONE',  ( 101.2319675162309807, -52.73591760636113435, 193.1241288170249959 ) ) ;
#99141 = VECTOR ( 'NONE', #58297, 1000.000000000000000 ) ;
#99143 = CARTESIAN_POINT ( 'NONE',  ( -47.57472544752269528, 12.59044387134402321, 14.43844179794134952 ) ) ;
#99142 = CARTESIAN_POINT ( 'NONE',  ( 26.44954341376113049, -28.72239887604681385, 30.17119393485961609 ) ) ;
#99144 = ORIENTED_EDGE ( 'NONE', *, *, #35567, .F. ) ;
#99145 = ORIENTED_EDGE ( 'NONE', *, *, #46604, .F. ) ;
#99146 = CIRCLE ( 'NONE', #9602, 3.309500000000007880 ) ;
#99147 = EDGE_CURVE ( 'NONE', #32237, #58039, #33702, .T. ) ;
#99148 = ORIENTED_EDGE ( 'NONE', *, *, #97228, .F. ) ;
#99149 = CARTESIAN_POINT ( 'NONE',  ( 32.19533246082933431, 392.4695659865649304, 25.42398475254776358 ) ) ;
#99150 = ADVANCED_FACE ( 'NONE', ( #28871 ), #30434, .T. ) ;
#99151 = DIRECTION ( 'NONE',  ( -1.000000000000000000, -1.224606353822377258E-16, -0.000000000000000000 ) ) ;
#99152 = CARTESIAN_POINT ( 'NONE',  ( 9.317657253014628438, 53.46886534697259918, 3.778385012062984050 ) ) ;
#99153 = ORIENTED_EDGE ( 'NONE', *, *, #90121, .F. ) ;
#99154 = DIRECTION ( 'NONE',  ( 0.000000000000000000, 0.000000000000000000, 1.000000000000000000 ) ) ;
#99155 = CARTESIAN_POINT ( 'NONE',  ( 6.326592304916279552, 6.579439845142156074, 2.267162479624769134 ) ) ;
#99156 = CARTESIAN_POINT ( 'NONE',  ( -18.91791044776116237, 47.00000000000000000, 62.18611311450884926 ) ) ;
#99157 = CARTESIAN_POINT ( 'NONE',  ( -72.23603530542938245, -57.67079283669161782, 174.4370243615865661 ) ) ;
#99158 = CARTESIAN_POINT ( 'NONE',  ( 2.977408999572651815, -31.43750000204839168, 7.188101187500000933 ) ) ;
#99159 = CARTESIAN_POINT ( 'NONE',  ( -30.80732993440543410, 13.24159032961888549, 41.41050123719129772 ) ) ;
#99160 = CARTESIAN_POINT ( 'NONE',  ( -31.03867016165222026, 468.3124986733989772, 18.90871194958903345 ) ) ;
#99161 = CARTESIAN_POINT ( 'NONE',  ( 28.50099738913158376, 1.340359594676612611E-15, 0.000000000000000000 ) ) ;
#99162 = ADVANCED_FACE ( 'NONE', ( #54658 ), #89436, .F. ) ;
#99163 = CARTESIAN_POINT ( 'NONE',  ( -48.21571607899795708, -30.00000000000001066, -35.59733477200444440 ) ) ;
#99164 = CARTESIAN_POINT ( 'NONE',  ( -28.47812542966827110, -14.21045842199436926, 36.49899343628653270 ) ) ;
#99165 = CARTESIAN_POINT ( 'NONE',  ( -50.22257761704449308, -39.51501898924006895, 51.10941894695140775 ) ) ;
#99166 = CARTESIAN_POINT ( 'NONE',  ( -17.49999999999997513, 45.00000000000000711, 100.0000000000000000 ) ) ;
#99167 = ORIENTED_EDGE ( 'NONE', *, *, #34551, .F. ) ;
#99168 = CARTESIAN_POINT ( 'NONE',  ( -100.3692683177832947, -52.75229974785736431, 193.9353176766608726 ) ) ;
#99169 = CARTESIAN_POINT ( 'NONE',  ( -0.3768998506200362253, 294.9778291542829152, -9.999928804128023430 ) ) ;
#99170 = CARTESIAN_POINT ( 'NONE',  ( 11.48053704661521479, -1.561145388285825275, 20.53821296167100030 ) ) ;
#99171 = ORIENTED_EDGE ( 'NONE', *, *, #17161, .F. ) ;
#99172 = CARTESIAN_POINT ( 'NONE',  ( 42.09158233638500235, 465.7816406625409513, 14.79318349170030089 ) ) ;
#99173 = CARTESIAN_POINT ( 'NONE',  ( 93.05610975779491412, -38.49596479831048157, 201.1399583442435528 ) ) ;
#99174 = CARTESIAN_POINT ( 'NONE',  ( 48.55387420720872171, 13.84642135131330853, 16.74239769522738897 ) ) ;
#99175 = DIRECTION ( 'NONE',  ( 0.000000000000000000, -1.000000000000000000, 0.000000000000000000 ) ) ;
#99176 = CARTESIAN_POINT ( 'NONE',  ( 69.18888888888888289, -3.309500000000000774, 0.000000000000000000 ) ) ;
#99177 = CARTESIAN_POINT ( 'NONE',  ( 85.25411052359936548, -29.99999999999999645, 172.6780782422512743 ) ) ;
#99178 = CARTESIAN_POINT ( 'NONE',  ( 36.65190467452017486, 491.8432146685188968, 12.58836626716453644 ) ) ;
#99179 = SURFACE_STYLE_FILL_AREA ( #9110 ) ;
#99180 = DIRECTION ( 'NONE',  ( 0.000000000000000000, 0.000000000000000000, -1.000000000000000000 ) ) ;
#99181 = ORIENTED_EDGE ( 'NONE', *, *, #81838, .T. ) ;
#99182 = ORIENTED_EDGE ( 'NONE', *, *, #6595, .T. ) ;
#99183 = CARTESIAN_POINT ( 'NONE',  ( 53.26745199980564394, -29.10185247891099891, 52.81664263156634576 ) ) ;
#99184 = CARTESIAN_POINT ( 'NONE',  ( -7.737907992291022552, 302.4298231441208031, -10.02991391761277207 ) ) ;
#99185 = CARTESIAN_POINT ( 'NONE',  ( 9.169967954764700835, 51.60694363734955914, 1.678936458957752009 ) ) ;
#99186 = ORIENTED_EDGE ( 'NONE', *, *, #37385, .F. ) ;
#99188 = ADVANCED_FACE ( 'NONE', ( #90774 ), #64382, .T. ) ;
#99187 = CARTESIAN_POINT ( 'NONE',  ( -106.3081487713218394, -38.35654553538349631, 126.0309737019096303 ) ) ;
#99189 = ORIENTED_EDGE ( 'NONE', *, *, #87050, .T. ) ;
#99190 = CARTESIAN_POINT ( 'NONE',  ( 5.656854249492378806, -29.37500000409677270, 5.656854249492381470 ) ) ;
#99191 = CARTESIAN_POINT ( 'NONE',  ( 99.83938914365424466, -38.35585918022645302, 87.51053804860399055 ) ) ;
#99192 = CARTESIAN_POINT ( 'NONE',  ( 14.81305988563250331, 21.99659144501054442, -4.400106377329072060 ) ) ;
#99193 = B_SPLINE_CURVE_WITH_KNOTS ( 'NONE', 3,
 ( #55078, #89594, #24356, #58276, #16757, #81466, #25417, #57198, #8657, #73919, #40503, #91721, #74448, #99799, #529, #9712 ),
 .UNSPECIFIED., .F., .F.,
 ( 4, 2, 2, 2, 2, 2, 2, 4 ),
 ( 0.06710770102819928196, 0.06840367950113611373, 0.06969965797407294550, 0.07099563644700979115, 0.07229161491994662292, 0.07488357186582030034, 0.07617955033875714599, 0.07747552881169397776 ),
 .UNSPECIFIED. ) ;
#99194 = CARTESIAN_POINT ( 'NONE',  ( 85.81162101844391543, -52.71496586455459976, 30.16212271239476905 ) ) ;
#99195 = CARTESIAN_POINT ( 'NONE',  ( -31.31625665069342190, 438.7960044619113660, 22.44465281717054950 ) ) ;
#99196 = CARTESIAN_POINT ( 'NONE',  ( 33.00496812083888898, 465.6658704666191966, 15.15901827093884258 ) ) ;
#99197 = CARTESIAN_POINT ( 'NONE',  ( -29.13274776455849846, 308.3486360454327269, -8.978973805476414327 ) ) ;
#99198 = CARTESIAN_POINT ( 'NONE',  ( 3.510631567122396657, -68.36704268726951739, 13.08651599561504497 ) ) ;
#99199 = CARTESIAN_POINT ( 'NONE',  ( 75.45779768849573088, -60.00000000000001421, 184.2411573433691672 ) ) ;
#99200 = EDGE_CURVE ( 'NONE', #34748, #75985, #57847, .T. ) ;
#99201 = AXIS2_PLACEMENT_3D ( 'NONE', #13018, #56115, #45946 ) ;
#99202 = DIRECTION ( 'NONE',  ( 0.000000000000000000, -1.000000000000000000, 0.000000000000000000 ) ) ;
#99203 = VERTEX_POINT ( 'NONE', #22879 ) ;
#99204 = CARTESIAN_POINT ( 'NONE',  ( 62.38864196659469741, -32.53364364072947268, 75.22878982978467377 ) ) ;
#99205 = CARTESIAN_POINT ( 'NONE',  ( -25.82432753990636698, 295.8677741265493637, -1.781385710556211421 ) ) ;
#99206 = ADVANCED_FACE ( 'NONE', ( #31502 ), #64544, .F. ) ;
#99207 = CARTESIAN_POINT ( 'NONE',  ( 6.162888688655347558, 7.505553499465140277, 0.000000000000000000 ) ) ;
#99208 = CIRCLE ( 'NONE', #9663, 4.000000000000000888 ) ;
#99209 = CARTESIAN_POINT ( 'NONE',  ( -8.763666794316772979, -5.000000000000000000, -16.82232303772159909 ) ) ;
#99211 = CARTESIAN_POINT ( 'NONE',  ( -34.05377651491208013, 485.0003423799789743, 0.6720595971183709327 ) ) ;
#99210 = CARTESIAN_POINT ( 'NONE',  ( -89.66675816820549016, -38.39121966713390322, -16.77064573778548962 ) ) ;
#99212 = CARTESIAN_POINT ( 'NONE',  ( -33.12749645818041699, 378.6598013907594691, 24.66483730404220154 ) ) ;
#99213 = CARTESIAN_POINT ( 'NONE',  ( -4.999999999999999112, -5.773502691896267969, -7.063244554130005071 ) ) ;
#99214 = CARTESIAN_POINT ( 'NONE',  ( -39.73517528558786438, 463.8619862608260860, 18.93615324539412370 ) ) ;
#99215 = CARTESIAN_POINT ( 'NONE',  ( 7.999999999999998224, -27.59374999999999289, 3.313708498984766493 ) ) ;
#99216 = CIRCLE ( 'NONE', #23515, 4.000000000000001776 ) ;
#99217 = AXIS2_PLACEMENT_3D ( 'NONE', #79412, #14653, #97177 ) ;
#99218 = CARTESIAN_POINT ( 'NONE',  ( 15.54899369231023343, 44.07947967433609904, -4.780801059126263297 ) ) ;
#99219 = ORIENTED_EDGE ( 'NONE', *, *, #77049, .T. ) ;
#99220 = CARTESIAN_POINT ( 'NONE',  ( 82.39197520823663012, -53.57314957911707864, 183.5891899450602409 ) ) ;
#99221 = CARTESIAN_POINT ( 'NONE',  ( 4.401189997858475422, -13.27310044850791471, -9.172641694124337164 ) ) ;
#99222 = CARTESIAN_POINT ( 'NONE',  ( 80.97977184163765685, 1.030564683017419500E-14, 0.000000000000000000 ) ) ;
#99223 = ORIENTED_EDGE ( 'NONE', *, *, #61085, .F. ) ;
#99224 = LINE ( 'NONE', #9153, #66990 ) ;
#99225 = DIRECTION ( 'NONE',  ( 0.000000000000000000, -1.000000000000000000, 0.000000000000000000 ) ) ;
#99226 = CARTESIAN_POINT ( 'NONE',  ( -32.22120753352773193, 464.6691781026584636, 10.60621122532597305 ) ) ;
#99227 = CARTESIAN_POINT ( 'NONE',  ( -39.04768351285803618, 42.03798982804668327, -56.81831037689468644 ) ) ;
#99228 = AXIS2_PLACEMENT_3D ( 'NONE', #51769, #60433, #58271 ) ;
#99229 = CARTESIAN_POINT ( 'NONE',  ( -8.022151257807545122, -0.1402635695912273495, 19.37061829778098954 ) ) ;
#99230 = EDGE_CURVE ( 'NONE', #26488, #104525, #92177, .T. ) ;
#99231 = CARTESIAN_POINT ( 'NONE',  ( 52.36387915676058924, -60.00000000000000000, 77.90990540846810575 ) ) ;
#99232 = DIRECTION ( 'NONE',  ( -1.000000000000000000, -0.000000000000000000, -0.000000000000000000 ) ) ;
#99233 = CARTESIAN_POINT ( 'NONE',  ( 19.31324592808787699, -16.82044274283948226, 31.48938567249289733 ) ) ;
#99234 = EDGE_CURVE ( 'NONE', #44820, #58911, #54280, .T. ) ;
#99236 = CARTESIAN_POINT ( 'NONE',  ( -13.10092205524128062, 21.81812862912754980, -4.743381763050468436 ) ) ;
#99235 = CARTESIAN_POINT ( 'NONE',  ( -15.48955457585431184, -22.96514382653771236, 36.00456892657421548 ) ) ;
#99237 = CARTESIAN_POINT ( 'NONE',  ( 7.188101187499999156, -11.75000000204838813, 2.977408999572654924 ) ) ;
#99238 = DIRECTION ( 'NONE',  ( 0.000000000000000000, 0.000000000000000000, 1.000000000000000000 ) ) ;
#99239 = ORIENTED_EDGE ( 'NONE', *, *, #5986, .F. ) ;
#99240 = AXIS2_PLACEMENT_3D ( 'NONE', #23748, #23211, #22688 ) ;
#99241 = CARTESIAN_POINT ( 'NONE',  ( -17.49999999999969091, 50.00252300264565264, 59.96656198872882726 ) ) ;
#99242 = EDGE_CURVE ( 'NONE', #4316, #16221, #45695, .T. ) ;
#99243 = CARTESIAN_POINT ( 'NONE',  ( 23.85631536739324332, 25.16912815653500246, 33.03393598700190381 ) ) ;
#99244 = VECTOR ( 'NONE', #49281, 1000.000000000000000 ) ;
#99245 = CARTESIAN_POINT ( 'NONE',  ( -41.97866624869027419, 465.7384095647168465, 15.05473019647155830 ) ) ;
#99247 = CARTESIAN_POINT ( 'NONE',  ( 41.46650182939242058, -47.40888185850945291, -31.47352802185152854 ) ) ;
#99246 = CARTESIAN_POINT ( 'NONE',  ( 5.290067270632322405, 53.47475093287481940, 8.531152949374478212 ) ) ;
#99248 = EDGE_LOOP ( 'NONE', ( #51774, #63650, #81496, #97328, #44331, #37237 ) ) ;
#99249 = CARTESIAN_POINT ( 'NONE',  ( -5.647817967127097383, -88.45126406528795826, -2.038183545141173614 ) ) ;
#99250 = VERTEX_POINT ( 'NONE', #93437 ) ;
#99251 = FILL_AREA_STYLE_COLOUR ( '', #17956 ) ;
#99252 = DIRECTION ( 'NONE',  ( -1.000000000000000000, -0.000000000000000000, -0.000000000000000000 ) ) ;
#99253 = CARTESIAN_POINT ( 'NONE',  ( -35.21289418190758624, 40.42438906900185458, -59.33026139110200603 ) ) ;
#99254 = CARTESIAN_POINT ( 'NONE',  ( -95.52932323723678110, -60.00000000000000000, 52.80250551557467276 ) ) ;
#99255 = FACE_BOUND ( 'NONE', #7460, .T. ) ;
#99256 = CARTESIAN_POINT ( 'NONE',  ( 6.683837171061802529, 3.955946848495962787, 6.851900933636986935 ) ) ;
#99257 = CARTESIAN_POINT ( 'NONE',  ( 33.63427961064055438, 325.9154870834976236, -4.827994974213513757 ) ) ;
#99258 = CARTESIAN_POINT ( 'NONE',  ( 40.18832759596136128, 460.7626523741619167, 2.139563623142427762 ) ) ;
#99260 = CARTESIAN_POINT ( 'NONE',  ( -6.716227137650916390, 41.28548431013199860, -58.40643990737236635 ) ) ;
#99259 = CARTESIAN_POINT ( 'NONE',  ( -2.617478844992338516, -5.000000000000015099, -94.73972676610841859 ) ) ;
#99261 = CARTESIAN_POINT ( 'NONE',  ( -84.26947212678977905, -32.46855681540231586, 170.8702711660567104 ) ) ;
#99262 = ORIENTED_EDGE ( 'NONE', *, *, #16592, .F. ) ;
#99263 = CARTESIAN_POINT ( 'NONE',  ( -43.59756234217329762, 434.3244621007154365, 14.55946156040307926 ) ) ;
#99264 = EDGE_LOOP ( 'NONE', ( #72966, #60996, #96799, #23828, #64562 ) ) ;
#99265 = ORIENTED_EDGE ( 'NONE', *, *, #3930, .T. ) ;
#99266 = CARTESIAN_POINT ( 'NONE',  ( 0.000000000000000000, 1.999999999999998224, 0.000000000000000000 ) ) ;
#99267 = EDGE_CURVE ( 'NONE', #33881, #9120, #6106, .T. ) ;
#99268 = CIRCLE ( 'NONE', #68282, 4.000000000000000888 ) ;
#99269 = ORIENTED_EDGE ( 'NONE', *, *, #95429, .T. ) ;
#99270 = CARTESIAN_POINT ( 'NONE',  ( -16.53877150159848242, 304.5679819412924871, 8.876634200354359905 ) ) ;
#99271 = CARTESIAN_POINT ( 'NONE',  ( -22.45002021702217121, -57.67118433041228798, -43.66150106997372404 ) ) ;
#99272 = CARTESIAN_POINT ( 'NONE',  ( 31.36650669486618881, 0.000000000000000000, 4.000000000000000888 ) ) ;
#99273 = CARTESIAN_POINT ( 'NONE',  ( -7.986711519608431509, -61.02638096376566779, -0.5300249774147625104 ) ) ;
#99274 = AXIS2_PLACEMENT_3D ( 'NONE', #76583, #100864, #35647 ) ;
#99275 = DIRECTION ( 'NONE',  ( 0.000000000000000000, -1.000000000000000000, 0.000000000000000000 ) ) ;
#99276 = CARTESIAN_POINT ( 'NONE',  ( -11.04994576751742130, -5.000000000000000000, -91.95135554698900648 ) ) ;
#99277 = CARTESIAN_POINT ( 'NONE',  ( -5.000000000000000000, -13.80280838537006538, 10.52502860397554230 ) ) ;
#99278 = ADVANCED_FACE ( 'NONE', ( #25544, #26084 ), #100979, .T. ) ;
#99279 = CARTESIAN_POINT ( 'NONE',  ( 106.4976671120242173, -30.00000000000003553, 137.1020467228335349 ) ) ;
#99280 = CARTESIAN_POINT ( 'NONE',  ( -106.4855387602377732, -14.21045842199444564, 182.1782270149441558 ) ) ;
#99281 = CARTESIAN_POINT ( 'NONE',  ( -60.16549379149508070, -18.65118697126286662, 63.02844734512476066 ) ) ;
#99282 = VERTEX_POINT ( 'NONE', #83201 ) ;
#99283 = CARTESIAN_POINT ( 'NONE',  ( 38.28344347328716424, 38.95431846541184484, 51.20698281621823611 ) ) ;
#99284 = CARTESIAN_POINT ( 'NONE',  ( 111.6472127090487731, -60.00000000002953016, 193.6361861217306455 ) ) ;
#99285 = VECTOR ( 'NONE', #34387, 1000.000000000000000 ) ;
#99287 = EDGE_LOOP ( 'NONE', ( #18274, #24166 ) ) ;
#99286 = AXIS2_PLACEMENT_3D ( 'NONE', #94373, #20535, #98593 ) ;
#99288 = CARTESIAN_POINT ( 'NONE',  ( 7.055885070595124375, -29.02937926490056952, 28.71821008264055664 ) ) ;
#99289 =( GEOMETRIC_REPRESENTATION_CONTEXT ( 3 ) GLOBAL_UNCERTAINTY_ASSIGNED_CONTEXT ( ( #68576 ) ) GLOBAL_UNIT_ASSIGNED_CONTEXT ( ( #97149, #37516, #46105 ) ) REPRESENTATION_CONTEXT ( 'NONE', 'WORKASPACE' ) );
#99290 = CARTESIAN_POINT ( 'NONE',  ( -101.4585684387344173, -37.82058770419944693, 151.6467883671373897 ) ) ;
#99292 = CIRCLE ( 'NONE', #75206, 4.000000000000007105 ) ;
#99291 = CARTESIAN_POINT ( 'NONE',  ( 4.401442555609581635E-16, -16.15625000204838457, -7.188101187500000044 ) ) ;
#99293 = DIRECTION ( 'NONE',  ( -1.000000000000000000, -1.224606353822377258E-16, -0.000000000000000000 ) ) ;
#99294 = ORIENTED_EDGE ( 'NONE', *, *, #99001, .T. ) ;
#99295 = FILL_AREA_STYLE_COLOUR ( '', #92409 ) ;
#99296 = CARTESIAN_POINT ( 'NONE',  ( -69.88467371534370898, -59.99999999999997868, 140.7241876569264605 ) ) ;
#99297 = CARTESIAN_POINT ( 'NONE',  ( 9.901632022247257581, -57.79079078909488487, 28.42038564161779135 ) ) ;
#99298 = CARTESIAN_POINT ( 'NONE',  ( 7.188101187499999156, -18.12500000204838457, 2.977408999572654924 ) ) ;
#99299 = CARTESIAN_POINT ( 'NONE',  ( 45.99999999999412381, 462.6092035404159333, 6.975422689164243018 ) ) ;
#99300 =( GEOMETRIC_REPRESENTATION_CONTEXT ( 3 ) GLOBAL_UNCERTAINTY_ASSIGNED_CONTEXT ( ( #92283 ) ) GLOBAL_UNIT_ASSIGNED_CONTEXT ( ( #148, #15836, #81095 ) ) REPRESENTATION_CONTEXT ( 'NONE', 'WORKASPACE' ) );
#99301 =( BOUNDED_SURFACE ( )  B_SPLINE_SURFACE ( 3, 2, ( 
 ( #53577, #91272, #66441 ),
 ( #58353, #1143, #17383 ),
 ( #24949, #50257, #73993 ),
 ( #16841, #33565, #7135 ) ),
 .UNSPECIFIED., .F., .F., .F. ) 
 B_SPLINE_SURFACE_WITH_KNOTS ( ( 4, 4 ),
 ( 3, 3 ),
 ( 5.642621786483559276E-15, 0.002106423517718437628 ),
 ( 0.000000000000000000, 1.000000000000000000 ),
 .UNSPECIFIED. ) 
 GEOMETRIC_REPRESENTATION_ITEM ( )  RATIONAL_B_SPLINE_SURFACE ( (
 ( 1.000000000000000000, 0.7977970988453120249, 1.000000000000000000),
 ( 1.000000000000000000, 0.8078744440618467193, 1.000000000000000000),
 ( 1.000000000000000000, 0.8177468419060218707, 1.000000000000000000),
 ( 1.000000000000000000, 0.8274831119534205026, 1.000000000000000000) ) ) 
 REPRESENTATION_ITEM ( '' )  SURFACE ( )  );
#99302 = CARTESIAN_POINT ( 'NONE',  ( 6.928203230275507885, -85.00000000000000000, -4.000000000000001776 ) ) ;
#99303 = CARTESIAN_POINT ( 'NONE',  ( 5.000000000000000888, -4.607437535715905419, -14.28092741399824384 ) ) ;
#99304 = CARTESIAN_POINT ( 'NONE',  ( -30.00000000000005329, 464.1062179653383168, 10.70584622102857786 ) ) ;
#99305 = DIRECTION ( 'NONE',  ( 0.000000000000000000, -1.000000000000000000, 0.000000000000000000 ) ) ;
#99306 = CARTESIAN_POINT ( 'NONE',  ( -23.29992259251663711, 27.36384728240174979, 33.20617127781060418 ) ) ;
#99307 = EDGE_CURVE ( 'NONE', #85478, #35775, #75638, .T. ) ;
#99308 = CARTESIAN_POINT ( 'NONE',  ( 86.30257998548809439, -60.00000000000005684, -13.06867930585625714 ) ) ;
#99309 = CARTESIAN_POINT ( 'NONE',  ( -33.60394201097540190, -53.37182691420839120, 37.21343069149457961 ) ) ;
#99310 = CARTESIAN_POINT ( 'NONE',  ( -2.807206530941451561, -49.57822929777214682, 102.9378052260345839 ) ) ;
#99311 = CARTESIAN_POINT ( 'NONE',  ( 45.62230598746199917, -49.89328325408317966, 47.30517501752983378 ) ) ;
#99312 = DIRECTION ( 'NONE',  ( 0.000000000000000000, 0.000000000000000000, 1.000000000000000000 ) ) ;
#99313 = ORIENTED_EDGE ( 'NONE', *, *, #87722, .F. ) ;
#99314 = CARTESIAN_POINT ( 'NONE',  ( 44.33427973454571713, 435.2106362794496590, 13.55537084937271430 ) ) ;
#99315 = CARTESIAN_POINT ( 'NONE',  ( -76.45337711124132341, -38.40897008212451880, 181.4709146294509594 ) ) ;
#99316 = EDGE_LOOP ( 'NONE', ( #91618, #18744, #86952, #23410, #90668 ) ) ;
#99318 = LINE ( 'NONE', #25492, #49085 ) ;
#99317 = CARTESIAN_POINT ( 'NONE',  ( 0.000000000000000000, 0.000000000000000000, 5.000000000000002665 ) ) ;
#99319 = CARTESIAN_POINT ( 'NONE',  ( 6.026974479199131350E-05, -59.99999999999998579, 33.88964995960238014 ) ) ;
#99320 = CARTESIAN_POINT ( 'NONE',  ( 16.75187969033571989, 36.38380281757302726, 24.30698433968583316 ) ) ;
#99321 = CARTESIAN_POINT ( 'NONE',  ( 5.856349485908122432, 1.359279156792585930, 6.499999999999997335 ) ) ;
#99322 = CARTESIAN_POINT ( 'NONE',  ( 33.22325481135199965, 463.2504524720463337, 6.140871053189498774 ) ) ;
#99323 = CARTESIAN_POINT ( 'NONE',  ( -38.81120307428947314, 25.17591441068872982, 12.35054225871727596 ) ) ;
#99324 = CARTESIAN_POINT ( 'NONE',  ( -30.13306121044136177, 331.7621428518107223, 15.49882586424142694 ) ) ;
#99325 = CIRCLE ( 'NONE', #83860, 4.000000000000007105 ) ;
#99326 = CARTESIAN_POINT ( 'NONE',  ( 102.0663143730366897, -60.00000000000000711, 93.13200012967355690 ) ) ;
#99327 = CARTESIAN_POINT ( 'NONE',  ( 14.44768974034866993, 5.957293599828267006, -7.129930386717066249 ) ) ;
#99328 = FACE_OUTER_BOUND ( 'NONE', #94013, .T. ) ;
#99329 = ORIENTED_EDGE ( 'NONE', *, *, #100030, .T. ) ;
#99330 = EDGE_CURVE ( 'NONE', #653, #25026, #68085, .T. ) ;
#99331 = CARTESIAN_POINT ( 'NONE',  ( -100.6601205862880306, -29.99999999999999289, 181.6786300687315077 ) ) ;
#99332 = EDGE_LOOP ( 'NONE', ( #96541, #9579, #75435, #58762, #95273 ) ) ;
#99333 = CARTESIAN_POINT ( 'NONE',  ( 1.715570313355265775, -4.332661967060491115, -17.83376356531591966 ) ) ;
#99334 = DIRECTION ( 'NONE',  ( 0.000000000000000000, 0.000000000000000000, -1.000000000000000000 ) ) ;
#99335 = CARTESIAN_POINT ( 'NONE',  ( 20.01715961282798872, 303.8268864493743422, 9.931703227614395502 ) ) ;
#99336 = CARTESIAN_POINT ( 'NONE',  ( 43.58349330513380693, 1.593028355512270567E-15, 0.000000000000000000 ) ) ;
#99337 = CARTESIAN_POINT ( 'NONE',  ( -2.977408999572650039, -19.06250000204838813, -7.188101187500001821 ) ) ;
#99338 = CARTESIAN_POINT ( 'NONE',  ( 16.75187969033441604, 36.38380281757147827, -24.30698433969211791 ) ) ;
#99339 = VECTOR ( 'NONE', #102584, 1000.000000000000000 ) ;
#99341 = ORIENTED_EDGE ( 'NONE', *, *, #53875, .F. ) ;
#99340 = CARTESIAN_POINT ( 'NONE',  ( -40.35113922517010110, 477.0906381947924046, -2.238203954573617871 ) ) ;
#99342 = CARTESIAN_POINT ( 'NONE',  ( 83.70516314075617004, -32.52322900293838615, 165.3182127895680935 ) ) ;
#99343 = AXIS2_PLACEMENT_3D ( 'NONE', #11534, #91935, #9949 ) ;
#99344 = ORIENTED_EDGE ( 'NONE', *, *, #42754, .T. ) ;
#99345 = CARTESIAN_POINT ( 'NONE',  ( 21.84999999999999787, 1.533819458162526451E-15, 0.000000000000000000 ) ) ;
#99346 = CARTESIAN_POINT ( 'NONE',  ( -7.500000000000001776, 0.000000000000000000, -5.000000000000000000 ) ) ;
#99347 = CARTESIAN_POINT ( 'NONE',  ( 20.00000000000000000, 12.99999999999999289, -4.000000000000000000 ) ) ;
#99348 = CARTESIAN_POINT ( 'NONE',  ( -5.382954851612910652, 252.9998749148943489, -2.657971597726735524 ) ) ;
#99349 = CARTESIAN_POINT ( 'NONE',  ( -33.13378764655153930, 418.1818430120953280, 25.61784589414144264 ) ) ;
#99350 = DIRECTION ( 'NONE',  ( 0.000000000000000000, 0.000000000000000000, -1.000000000000000000 ) ) ;
#99351 = EDGE_CURVE ( 'NONE', #87241, #91829, #1187, .T. ) ;
#99352 = ORIENTED_EDGE ( 'NONE', *, *, #96715, .T. ) ;
#99353 = B_SPLINE_CURVE_WITH_KNOTS ( 'NONE', 3,
 ( #51783, #26501, #74459, #10780, #84696, #51240, #43699, #76058, #17319, #9189 ),
 .UNSPECIFIED., .F., .F.,
 ( 4, 2, 2, 2, 4 ),
 ( 0.000000000000000000, 0.002305503304226492068, 0.004611006608452984136, 0.006916509912679475770, 0.009222013216905964803 ),
 .UNSPECIFIED. ) ;
#99354 =( NAMED_UNIT ( * ) SI_UNIT ( $, .STERADIAN. ) SOLID_ANGLE_UNIT ( ) );
#99355 = CARTESIAN_POINT ( 'NONE',  ( -33.00000000000000000, 450.0000000000002274, 13.20242257375370976 ) ) ;
#99356 = ADVANCED_FACE ( 'NONE', ( #60026 ), #59481, .T. ) ;
#99357 = CARTESIAN_POINT ( 'NONE',  ( 34.45841046839812094, 18.64284798592741410, 17.01587130354588595 ) ) ;
#99358 = CARTESIAN_POINT ( 'NONE',  ( 86.75617746412517306, -28.06358367585517755, 186.0038586487513896 ) ) ;
#99359 = EDGE_CURVE ( 'NONE', #65357, #91640, #101520, .T. ) ;
#99360 = CARTESIAN_POINT ( 'NONE',  ( 24.05868969682389036, 0.000000000000000000, 5.000000000000002665 ) ) ;
#99361 = CARTESIAN_POINT ( 'NONE',  ( -7.188101187500002709, -31.81250000204839168, 2.977408999572648707 ) ) ;
#99362 = MECHANICAL_DESIGN_GEOMETRIC_PRESENTATION_REPRESENTATION (  '', ( #102787 ), #45963 ) ;
#99363 = AXIS2_PLACEMENT_3D ( 'NONE', #45688, #37635, #54272 ) ;
#99364 = CARTESIAN_POINT ( 'NONE',  ( 9.789044728060087408, 294.6486233851415477, -2.043184600578025201 ) ) ;
#99365 = CIRCLE ( 'NONE', #87398, 5.000000000000010658 ) ;
#99366 = VECTOR ( 'NONE', #91105, 1000.000000000000114 ) ;
#99367 = CARTESIAN_POINT ( 'NONE',  ( 7.312797294236363932, 52.12749630495425635, 2.972055287740744234 ) ) ;
#99368 = CARTESIAN_POINT ( 'NONE',  ( 36.96037796283875565, 439.3711962631035703, 23.79839446779178402 ) ) ;
#99369 = CARTESIAN_POINT ( 'NONE',  ( -9.253583916535177423, 31.29803908005034785, 3.792462592445554392 ) ) ;
#99370 = ORIENTED_EDGE ( 'NONE', *, *, #104133, .T. ) ;
#99371 = EDGE_CURVE ( 'NONE', #77299, #76326, #9297, .T. ) ;
#99372 = CARTESIAN_POINT ( 'NONE',  ( 46.84999999999999432, 3.309500000000003439, 4.052968581778167743E-16 ) ) ;
#99373 = AXIS2_PLACEMENT_3D ( 'NONE', #52993, #62686, #70239 ) ;
#99374 = CARTESIAN_POINT ( 'NONE',  ( 14.75116209840774495, 43.55504285524111907, -90.22050492864485705 ) ) ;
#99375 = CARTESIAN_POINT ( 'NONE',  ( -5.938874586546019962, 4.582654186248475980, -4.999999999999999112 ) ) ;
#99376 = ORIENTED_EDGE ( 'NONE', *, *, #17834, .F. ) ;
#99377 = LINE ( 'NONE', #97391, #80817 ) ;
#99378 = CARTESIAN_POINT ( 'NONE',  ( -7.500000000000005329, 24.91666666666666430, -68.91429205785459544 ) ) ;
#99379 = CARTESIAN_POINT ( 'NONE',  ( 109.7502093377535886, -57.66773119830670424, 196.5356198408315436 ) ) ;
#99380 = FACE_OUTER_BOUND ( 'NONE', #55046, .T. ) ;
#99381 = DIRECTION ( 'NONE',  ( -8.673617379884035472E-17, -0.000000000000000000, -1.000000000000000000 ) ) ;
#99382 = CARTESIAN_POINT ( 'NONE',  ( 0.000000000000000000, 0.000000000000000000, 0.000000000000000000 ) ) ;
#99383 = CYLINDRICAL_SURFACE ( 'NONE', #35837, 1.250000000000001110 ) ;
#99384 = PRODUCT ( '4. Handle', '4. Handle', '', ( #33096 ) ) ;
#99385 = CARTESIAN_POINT ( 'NONE',  ( -76.54204534339102395, -60.00000000000000000, 189.0398269527300386 ) ) ;
#99386 = CARTESIAN_POINT ( 'NONE',  ( 9.034543481159971634, 43.90162183362577508, -14.11077590592769049 ) ) ;
#99387 = CARTESIAN_POINT ( 'NONE',  ( -25.93947128054312756, 296.0094280503604978, 10.18659011856751384 ) ) ;
#99388 = AXIS2_PLACEMENT_3D ( 'NONE', #88974, #40414, #82472 ) ;
#99389 = CARTESIAN_POINT ( 'NONE',  ( -84.65018232938496112, -39.39540612587336454, 182.1018301571575080 ) ) ;
#99390 = EDGE_LOOP ( 'NONE', ( #60311, #34528, #309, #79112 ) ) ;
#99391 = CARTESIAN_POINT ( 'NONE',  ( 23.06742787864941846, 305.3843356243662015, -9.885683119079418546 ) ) ;
#99392 = VECTOR ( 'NONE', #8879, 1000.000000000000227 ) ;
#99393 = ORIENTED_EDGE ( 'NONE', *, *, #80978, .F. ) ;
#99394 = CARTESIAN_POINT ( 'NONE',  ( 14.33580413386840213, 42.00000000000000000, -89.41414995614803729 ) ) ;
#99395 = EDGE_CURVE ( 'NONE', #44923, #64080, #104709, .T. ) ;
#99396 = DIRECTION ( 'NONE',  ( -1.000000000000000000, 0.000000000000000000, 0.000000000000000000 ) ) ;
#99397 = CARTESIAN_POINT ( 'NONE',  ( -83.87309315678267296, -45.26105613303531783, -12.39373611433831002 ) ) ;
#99398 = CARTESIAN_POINT ( 'NONE',  ( -5.000000000000000000, -15.93202192939577344, -5.930487099830192399 ) ) ;
#99399 = VERTEX_POINT ( 'NONE', #50816 ) ;
#99400 = DIRECTION ( 'NONE',  ( 0.000000000000000000, 0.000000000000000000, 1.000000000000000000 ) ) ;
#99401 = CARTESIAN_POINT ( 'NONE',  ( 105.5720000000000312, 0.000000000000000000, 0.000000000000000000 ) ) ;
#99402 = CARTESIAN_POINT ( 'NONE',  ( 10.02677674313807366, 14.12742448687086672, -10.50839540146165696 ) ) ;
#99403 = ADVANCED_FACE ( 'NONE', ( #34694 ), #92346, .F. ) ;
#99404 = ADVANCED_FACE ( 'NONE', ( #55067 ), #2637, .T. ) ;
#99406 = AXIS2_PLACEMENT_3D ( 'NONE', #69626, #12422, #77177 ) ;
#99405 = CARTESIAN_POINT ( 'NONE',  ( -7.420756919583588009E-15, 4.501353321498349658, 60.59507871780017751 ) ) ;
#99407 = CARTESIAN_POINT ( 'NONE',  ( -35.75766626157646044, 437.8288023593529488, 4.424845182008526834 ) ) ;
#99408 = CARTESIAN_POINT ( 'NONE',  ( -42.61015704936735915, -60.00000000000002842, -41.65925318937349431 ) ) ;
#99409 = CARTESIAN_POINT ( 'NONE',  ( -76.47417906005152588, -53.37849902404385460, 138.8593508845263500 ) ) ;
#99410 = ORIENTED_EDGE ( 'NONE', *, *, #54383, .F. ) ;
#99411 = CARTESIAN_POINT ( 'NONE',  ( 74.10901235487826000, -60.00000000000013500, 189.8092491115571647 ) ) ;
#99412 = CARTESIAN_POINT ( 'NONE',  ( 7.934203308536662114, 88.86700340017800670, 1.057099537198546324 ) ) ;
#99413 = CARTESIAN_POINT ( 'NONE',  ( 94.13231147061260629, -57.67516424662597530, 3.527862659130869716 ) ) ;
#99414 = EDGE_LOOP ( 'NONE', ( #35725, #87542, #52112, #95397 ) ) ;
#99415 = CARTESIAN_POINT ( 'NONE',  ( -3.400000000000000355, 4.163799117101001052E-16, -8.000000000000000000 ) ) ;
#99417 = EDGE_CURVE ( 'NONE', #66822, #6722, #369, .T. ) ;
#99416 = AXIS2_PLACEMENT_3D ( 'NONE', #85893, #75641, #27140 ) ;
#99418 = EDGE_CURVE ( 'NONE', #550, #27751, #42296, .T. ) ;
#99419 = DIRECTION ( 'NONE',  ( 0.000000000000000000, 0.000000000000000000, -1.000000000000000000 ) ) ;
#99420 = ORIENTED_EDGE ( 'NONE', *, *, #93623, .T. ) ;
#99421 = AXIS2_PLACEMENT_3D ( 'NONE', #43260, #35193, #13529 ) ;
#99422 = DIRECTION ( 'NONE',  ( -0.000000000000000000, -1.000000000000000000, -0.000000000000000000 ) ) ;
#99423 = CARTESIAN_POINT ( 'NONE',  ( 0.000000000000000000, 0.000000000000000000, 0.000000000000000000 ) ) ;
#99424 = CARTESIAN_POINT ( 'NONE',  ( 15.39052280876485668, 44.08006356674551540, 5.263393437970842470 ) ) ;
#99425 = CARTESIAN_POINT ( 'NONE',  ( 7.188101187500001821, -11.56250000204838635, -2.977408999572650483 ) ) ;
#99426 = FACE_OUTER_BOUND ( 'NONE', #17723, .T. ) ;
#99427 = CARTESIAN_POINT ( 'NONE',  ( 2.691749510577694515, -0.5367988052720203962, 103.4277152940129412 ) ) ;
#99428 = CARTESIAN_POINT ( 'NONE',  ( 9.797174393178825657E-16, -30.00000000000000000, -8.000000000000000000 ) ) ;
#99429 = CARTESIAN_POINT ( 'NONE',  ( -9.000000000000001776, -46.00000000000000000, 42.58845726811989607 ) ) ;
#99430 = DIRECTION ( 'NONE',  ( 0.000000000000000000, 0.000000000000000000, 1.000000000000000000 ) ) ;
#99431 = PRESENTATION_STYLE_ASSIGNMENT (( #63923 ) ) ;
#99432 = EDGE_CURVE ( 'NONE', #41783, #92227, #62945, .T. ) ;
#99433 = ORIENTED_EDGE ( 'NONE', *, *, #95627, .F. ) ;
#99434 = CARTESIAN_POINT ( 'NONE',  ( -6.846597141950445220, 41.54610357434032863, -70.31839272209531089 ) ) ;
#99435 = MECHANICAL_DESIGN_GEOMETRIC_PRESENTATION_REPRESENTATION (  '', ( #102928 ), #63367 ) ;
#99436 = PRESENTATION_LAYER_ASSIGNMENT (  '', '', ( #46042 ) ) ;
#99438 = CARTESIAN_POINT ( 'NONE',  ( 29.64987082370327443, -49.90670958807863400, 34.84601124182362497 ) ) ;
#99437 = SURFACE_STYLE_USAGE ( .BOTH. , #25614 ) ;
#99439 = CARTESIAN_POINT ( 'NONE',  ( -32.80395775116956258, 487.0274233559226218, 8.980975396762143959 ) ) ;
#99440 = ORIENTED_EDGE ( 'NONE', *, *, #20790, .T. ) ;
#99441 = EDGE_CURVE ( 'NONE', #100372, #31339, #1737, .T. ) ;
#99442 = DIRECTION ( 'NONE',  ( 0.000000000000000000, 1.000000000000000000, 0.000000000000000000 ) ) ;
#99443 = VERTEX_POINT ( 'NONE', #37883 ) ;
#99444 = CIRCLE ( 'NONE', #83907, 4.000000000000001776 ) ;
#99446 = CARTESIAN_POINT ( 'NONE',  ( 1.306442393143576908, 8.377108146505385378, -7.792327460285857654 ) ) ;
#99445 = DIRECTION ( 'NONE',  ( 0.000000000000000000, 0.000000000000000000, 1.000000000000000000 ) ) ;
#99447 = AXIS2_PLACEMENT_3D ( 'NONE', #72989, #97807, #32580 ) ;
#99448 = DIRECTION ( 'NONE',  ( -1.000000000000000000, -1.224606353822377258E-16, -0.000000000000000000 ) ) ;
#99449 = CARTESIAN_POINT ( 'NONE',  ( -13.31081044356851173, 294.5490281876303698, -2.064334394374285786 ) ) ;
#99450 = VECTOR ( 'NONE', #61921, 1000.000000000000114 ) ;
#99451 = FACE_OUTER_BOUND ( 'NONE', #75412, .T. ) ;
#99452 = B_SPLINE_CURVE_WITH_KNOTS ( 'NONE', 3,
 ( #32298, #39849, #94512, #70218, #3892, #28733, #65169, #24215, #57065, #96489, #104562, #55985, #15015, #11966, #77781, #36824, #6389, #86426 ),
 .UNSPECIFIED., .F., .F.,
 ( 4, 2, 2, 2, 2, 2, 2, 2, 4 ),
 ( 0.000000000000000000, 0.06250000000000000000, 0.1250000000000000000, 0.1875000000000000000, 0.2500000000000000000, 0.3125000000000000000, 0.3750000000000000000, 0.4375000000000000000, 0.5000000000000000000 ),
 .UNSPECIFIED. ) ;
#99453 = CARTESIAN_POINT ( 'NONE',  ( 19.61638200451619696, 1.340359594676612611E-15, 0.000000000000000000 ) ) ;
#99454 = CARTESIAN_POINT ( 'NONE',  ( 0.3605712710638133145, 13.03532800917887258, -51.69843826998983616 ) ) ;
#99455 = ORIENTED_EDGE ( 'NONE', *, *, #88242, .T. ) ;
#99456 = CARTESIAN_POINT ( 'NONE',  ( 92.63360815464589848, -60.00000000000000711, -10.02160836745851924 ) ) ;
#99457 = CARTESIAN_POINT ( 'NONE',  ( 30.56153846153846132, -4.171999999999999709, 0.000000000000000000 ) ) ;
#99458 = CARTESIAN_POINT ( 'NONE',  ( 30.00000000000000355, 462.0139486977120100, 13.78583326880718829 ) ) ;
#99459 = CARTESIAN_POINT ( 'NONE',  ( 0.000000000000000000, 294.8518027762758038, -10.00000000000000355 ) ) ;
#99460 = DIRECTION ( 'NONE',  ( 0.5735764363510557073, -0.8191520442889850262, 1.003171929053516612E-16 ) ) ;
#99461 = ORIENTED_EDGE ( 'NONE', *, *, #2275, .T. ) ;
#99462 = LINE ( 'NONE', #18051, #17762 ) ;
#99463 = VERTEX_POINT ( 'NONE', #103117 ) ;
#99464 = VERTEX_POINT ( 'NONE', #4953 ) ;
#99465 = CARTESIAN_POINT ( 'NONE',  ( 7.211357414135266986, 82.98853460065558352, 3.467230644691327690 ) ) ;
#99466 = CARTESIAN_POINT ( 'NONE',  ( 5.975663821521009389, -7.000939006314210289, -0.8740179403730387042 ) ) ;
#99467 = CARTESIAN_POINT ( 'NONE',  ( -15.76179818182182224, 34.59899376685505246, -23.83662882038466080 ) ) ;
#99468 = DIRECTION ( 'NONE',  ( 1.000000000000000000, 0.000000000000000000, 0.000000000000000000 ) ) ;
#99469 = CARTESIAN_POINT ( 'NONE',  ( 85.75696656807998863, -52.74486970128089069, -6.687712918687570784 ) ) ;
#99470 = CARTESIAN_POINT ( 'NONE',  ( -39.70493663810997731, 309.1761292106233441, -6.633558359608890065 ) ) ;
#99471 = LINE ( 'NONE', #85440, #55949 ) ;
#99472 = CARTESIAN_POINT ( 'NONE',  ( 12.50000000000000533, 27.20916491834851669, -44.75057325027661648 ) ) ;
#99473 = ORIENTED_EDGE ( 'NONE', *, *, #34811, .F. ) ;
#99474 = CYLINDRICAL_SURFACE ( 'NONE', #66711, 4.999999999999999112 ) ;
#99475 = ORIENTED_EDGE ( 'NONE', *, *, #5169, .F. ) ;
#99476 = VECTOR ( 'NONE', #99460, 1000.000000000000000 ) ;
#99477 = DIRECTION ( 'NONE',  ( -1.000000000000000000, -1.224606353822377258E-16, -0.000000000000000000 ) ) ;
#99478 = CARTESIAN_POINT ( 'NONE',  ( 8.866506694866188809, 4.898587196589411843E-16, -4.000000000000000888 ) ) ;
#99480 = EDGE_LOOP ( 'NONE', ( #95466, #54409, #99370, #17774, #88828 ) ) ;
#99479 = CARTESIAN_POINT ( 'NONE',  ( 5.623226095793158130, 51.29171802761456433, 8.497680151582294172 ) ) ;
#99481 = CARTESIAN_POINT ( 'NONE',  ( 78.21122318075710211, -25.61170846490405140, 123.8332679187113570 ) ) ;
#99482 = VERTEX_POINT ( 'NONE', #44895 ) ;
#99483 = CARTESIAN_POINT ( 'NONE',  ( 17.50000000000002842, 48.98085210278581769, 64.05428188712279791 ) ) ;
#99484 = VECTOR ( 'NONE', #19955, 1000.000000000000000 ) ;
#99485 = CARTESIAN_POINT ( 'NONE',  ( 2.977408999572652260, -23.93750000204838457, 7.188101187500000044 ) ) ;
#99486 = CARTESIAN_POINT ( 'NONE',  ( -112.9456993887476415, -57.67119592114509175, 187.6412086615824535 ) ) ;
#99487 = EDGE_CURVE ( 'NONE', #32311, #80696, #61259, .T. ) ;
#99488 = VERTEX_POINT ( 'NONE', #52965 ) ;
#99489 = FILL_AREA_STYLE ('',( #67681 ) ) ;
#99490 = DIRECTION ( 'NONE',  ( -1.000000000000000000, -0.000000000000000000, -0.000000000000000000 ) ) ;
#99491 = CARTESIAN_POINT ( 'NONE',  ( 106.3494858034724473, -60.15152210362587226, 165.8936471126561116 ) ) ;
#99492 = EDGE_CURVE ( 'NONE', #53571, #14336, #77245, .T. ) ;
#99493 = ADVANCED_FACE ( 'NONE', ( #36822 ), #29788, .T. ) ;
#99494 = AXIS2_PLACEMENT_3D ( 'NONE', #51157, #84074, #50105 ) ;
#99495 = CARTESIAN_POINT ( 'NONE',  ( -34.58748436418674288, 491.1940522429816838, 12.14470207312695393 ) ) ;
#99496 = ADVANCED_FACE ( 'NONE', ( #78293 ), #93543, .T. ) ;
#99497 = DIRECTION ( 'NONE',  ( 0.000000000000000000, 0.000000000000000000, 1.000000000000000000 ) ) ;
#99498 = CARTESIAN_POINT ( 'NONE',  ( -3.313708498984765161, -26.65625000409676915, 7.999999999999998224 ) ) ;
#99499 = LINE ( 'NONE', #59605, #2016 ) ;
#99500 = DIRECTION ( 'NONE',  ( 1.000000000000000000, 0.000000000000000000, 0.000000000000000000 ) ) ;
#99501 = DIRECTION ( 'NONE',  ( -1.000000000000000000, 0.000000000000000000, 0.000000000000000000 ) ) ;
#99502 = STYLED_ITEM ( 'NONE', ( #92880 ), #67844 ) ;
#99503 = CARTESIAN_POINT ( 'NONE',  ( -6.322843063242285844, 4.034290371602571312, 5.000000000000000888 ) ) ;
#99504 = CARTESIAN_POINT ( 'NONE',  ( 62.33904886068935980, 4.898587196589294500E-16, -4.000000000000007105 ) ) ;
#99505 = DIRECTION ( 'NONE',  ( 1.000000000000000000, 0.000000000000000000, 0.000000000000000000 ) ) ;
#99506 = EDGE_LOOP ( 'NONE', ( #71430, #58186, #6749, #98324, #89912 ) ) ;
#99507 = SURFACE_STYLE_FILL_AREA ( #25682 ) ;
#99508 = EDGE_CURVE ( 'NONE', #21469, #58519, #102035, .T. ) ;
#99509 = DIRECTION ( 'NONE',  ( -1.000000000000000000, -1.224606353822377258E-16, -0.000000000000000000 ) ) ;
#99510 = CARTESIAN_POINT ( 'NONE',  ( 5.699273591081692736, -60.00000000000000711, 39.62882889116424678 ) ) ;
#99511 = CARTESIAN_POINT ( 'NONE',  ( -95.90249117390003164, -30.00000000000000000, 191.2992004980491458 ) ) ;
#99512 = B_SPLINE_CURVE_WITH_KNOTS ( 'NONE', 3,
 ( #63941, #46670, #73044, #97871, #96828, #24027, #48774, #29987, #104367, #70952 ),
 .UNSPECIFIED., .F., .F.,
 ( 4, 2, 2, 2, 4 ),
 ( 0.01051144076094937159, 0.01162027323572613000, 0.01272910571050288667, 0.01383793818527964507, 0.01494677066005640348 ),
 .UNSPECIFIED. ) ;
#99513 = ORIENTED_EDGE ( 'NONE', *, *, #7664, .F. ) ;
#99514 = CARTESIAN_POINT ( 'NONE',  ( 12.79230769230769305, 1.411358822780289120E-15, 0.000000000000000000 ) ) ;
#99515 = VECTOR ( 'NONE', #52870, 1000.000000000000000 ) ;
#99516 = CARTESIAN_POINT ( 'NONE',  ( 71.48874846803950334, -57.67964410071327563, 166.9188931464234429 ) ) ;
#99518 = CARTESIAN_POINT ( 'NONE',  ( -5.956988534971662475, 4.556784786910193397, 5.000000000000000000 ) ) ;
#99517 = PLANE ( 'NONE',  #98265 ) ;
#99519 = CARTESIAN_POINT ( 'NONE',  ( 5.356817479642971058, -21.70158312131658107, -38.54714666297098091 ) ) ;
#99520 = CARTESIAN_POINT ( 'NONE',  ( 32.17646412119353272, 464.6980787822281513, 10.84896803613063021 ) ) ;
#99521 = CYLINDRICAL_SURFACE ( 'NONE', #92531, 4.000000000000000888 ) ;
#99522 = CARTESIAN_POINT ( 'NONE',  ( -47.13330949325234087, -60.00000000000000000, 65.07896732603337853 ) ) ;
#99523 =( GEOMETRIC_REPRESENTATION_CONTEXT ( 3 ) GLOBAL_UNCERTAINTY_ASSIGNED_CONTEXT ( ( #72859 ) ) GLOBAL_UNIT_ASSIGNED_CONTEXT ( ( #77263, #102059, #86445 ) ) REPRESENTATION_CONTEXT ( 'NONE', 'WORKASPACE' ) );
#99524 = COLOUR_RGB ( '', 0.31764706, 0.68627451, 0.89019608) ;
#99525 = CIRCLE ( 'NONE', #8225, 4.000000000000001776 ) ;
#99526 = CARTESIAN_POINT ( 'NONE',  ( 0.000000000000000000, 0.000000000000000000, 4.000000000000000000 ) ) ;
#99527 = CARTESIAN_POINT ( 'NONE',  ( 5.290067270632322405, 53.47475093287481940, 8.531152949374478212 ) ) ;
#99528 = CARTESIAN_POINT ( 'NONE',  ( -86.89203889042968854, -42.78634412649035568, 189.7867230391053113 ) ) ;
#99529 = ORIENTED_EDGE ( 'NONE', *, *, #63865, .T. ) ;
#99530 = CARTESIAN_POINT ( 'NONE',  ( 9.283973715592685139, -13.34910468049023535, 16.51841009919174397 ) ) ;
#99531 = CARTESIAN_POINT ( 'NONE',  ( -6.981413442716312368, -18.58616681457634812, 26.97768225704258782 ) ) ;
#99532 = CARTESIAN_POINT ( 'NONE',  ( -5.675014839626371099, 41.92512469482201709, -59.11382255286373777 ) ) ;
#99533 = CARTESIAN_POINT ( 'NONE',  ( -5.416666666666666075, -4.378239541354687070, -5.848636054922041971 ) ) ;
#99535 = CARTESIAN_POINT ( 'NONE',  ( 4.814131498176642765, -64.23532120076806962, 13.02162479025466624 ) ) ;
#99534 = CARTESIAN_POINT ( 'NONE',  ( 0.000000000000000000, -5.000000000000002665, -75.00000000000001421 ) ) ;
#99536 = ORIENTED_EDGE ( 'NONE', *, *, #59589, .F. ) ;
#99537 = EDGE_CURVE ( 'NONE', #53305, #67639, #32728, .T. ) ;
#99538 = CARTESIAN_POINT ( 'NONE',  ( -46.00000000000000000, 488.3725375423296668, 3.127739281037489771 ) ) ;
#99539 = PRESENTATION_LAYER_ASSIGNMENT (  '', '', ( #3165 ) ) ;
#99540 = DIRECTION ( 'NONE',  ( -0.8191520442889974607, 0.000000000000000000, -0.5735764363510380548 ) ) ;
#99541 = CARTESIAN_POINT ( 'NONE',  ( -6.928203230275510549, 29.99999999999999645, -4.000000000000000000 ) ) ;
#99542 = CARTESIAN_POINT ( 'NONE',  ( 35.41928903355742619, 301.9014398045767393, -8.406339170677471273 ) ) ;
#99543 = PLANE ( 'NONE',  #38132 ) ;
#99544 = ADVANCED_FACE ( 'NONE', ( #39969 ), #105233, .T. ) ;
#99545 = DIRECTION ( 'NONE',  ( 0.000000000000000000, -1.000000000000000000, 0.000000000000000000 ) ) ;
#99546 = CARTESIAN_POINT ( 'NONE',  ( -2.499999999999998668, -30.00000000000000000, 14.79019945774903988 ) ) ;
#99547 = CONICAL_SURFACE ( 'NONE', #61634, 4.000000000000007105, 0.9599310885968835860 ) ;
#99548 = CARTESIAN_POINT ( 'NONE',  ( 106.9545358495978036, -14.21045842199422715, 174.0142581296349249 ) ) ;
#99549 = CARTESIAN_POINT ( 'NONE',  ( -81.63870341442944323, -46.45233036171202201, 168.1652440659686647 ) ) ;
#99550 = ORIENTED_EDGE ( 'NONE', *, *, #28462, .F. ) ;
#99551 = DIRECTION ( 'NONE',  ( -0.000000000000000000, -0.000000000000000000, 1.000000000000000000 ) ) ;
#99552 = CARTESIAN_POINT ( 'NONE',  ( -9.842984802582158466, 253.5906959047565294, 1.781981959250518832 ) ) ;
#99553 = DIRECTION ( 'NONE',  ( 0.000000000000000000, -6.071532165918824830E-15, 1.000000000000000000 ) ) ;
#99555 = CIRCLE ( 'NONE', #53079, 4.172000000000001485 ) ;
#99554 = CARTESIAN_POINT ( 'NONE',  ( 37.65605239364586510, 426.5628754408557484, 5.696003171475078730 ) ) ;
#99556 = ORIENTED_EDGE ( 'NONE', *, *, #71019, .T. ) ;
#99557 = CARTESIAN_POINT ( 'NONE',  ( -21.87180833870418084, 305.2301849206776865, 10.01838919985740084 ) ) ;
#99558 = VERTEX_POINT ( 'NONE', #105751 ) ;
#99559 = FACE_OUTER_BOUND ( 'NONE', #41187, .T. ) ;
#99560 = CARTESIAN_POINT ( 'NONE',  ( 4.582575694955839829, 15.00000000000000000, 9.999999999999998224 ) ) ;
#99561 = CARTESIAN_POINT ( 'NONE',  ( 32.76481181382172281, 487.6128877199117255, 8.618969267250339072 ) ) ;
#99562 = CARTESIAN_POINT ( 'NONE',  ( 60.62677696746332145, 48.00000000000000000, 24.18439665019722540 ) ) ;
#99563 = CARTESIAN_POINT ( 'NONE',  ( 33.86650669486618881, 1.474610560812782335E-15, 0.000000000000000000 ) ) ;
#99564 = B_SPLINE_CURVE_WITH_KNOTS ( 'NONE', 3,
 ( #50285, #100964, #76152, #92337, #84258 ),
 .UNSPECIFIED., .F., .F.,
 ( 4, 1, 4 ),
 ( 0.000000000000000000, 0.003752776749732568331, 0.007505553499465136662 ),
 .UNSPECIFIED. ) ;
#99566 = CARTESIAN_POINT ( 'NONE',  ( 44.21548463017017383, 435.3173990239856721, 11.13835373606124435 ) ) ;
#99565 = VECTOR ( 'NONE', #46994, 1000.000000000000000 ) ;
#99567 = ORIENTED_EDGE ( 'NONE', *, *, #5586, .T. ) ;
#99568 = CARTESIAN_POINT ( 'NONE',  ( 98.00949598672239915, -60.00000000000002132, 202.3503918769513348 ) ) ;
#99570 = CARTESIAN_POINT ( 'NONE',  ( 14.82802221756835337, -56.87755216349057719, 33.50449817620127391 ) ) ;
#99569 = CARTESIAN_POINT ( 'NONE',  ( -75.88739805180117060, -29.99999999999992895, 164.4352692622292409 ) ) ;
#99572 = DIRECTION ( 'NONE',  ( -1.000000000000000000, 0.000000000000000000, 0.000000000000000000 ) ) ;
#99571 = PRODUCT_DEFINITION_CONTEXT ( 'detailed design', #5231, 'design' ) ;
#99573 = CARTESIAN_POINT ( 'NONE',  ( 0.1695342223295464856, 53.40043206617340843, -10.24131878858624844 ) ) ;
#99574 = AXIS2_PLACEMENT_3D ( 'NONE', #96314, #6201, #48251 ) ;
#99575 = CARTESIAN_POINT ( 'NONE',  ( -41.19266119959871020, -39.52519630628623304, 39.71623854401850906 ) ) ;
#99576 = DIRECTION ( 'NONE',  ( -1.000000000000000000, -0.000000000000000000, -0.000000000000000000 ) ) ;
#99577 = ORIENTED_EDGE ( 'NONE', *, *, #16066, .F. ) ;
#99578 = CARTESIAN_POINT ( 'NONE',  ( 7.315107926653602988, 54.29845173462179986, 2.635958794940676864 ) ) ;
#99579 = CARTESIAN_POINT ( 'NONE',  ( 6.224163897435908588, -12.02839407259639337, 11.51386142893530362 ) ) ;
#99580 = AXIS2_PLACEMENT_3D ( 'NONE', #84186, #83111, #42116 ) ;
#99581 = FILL_AREA_STYLE_COLOUR ( '', #49166 ) ;
#99582 = ADVANCED_FACE ( 'NONE', ( #2135 ), #47443, .T. ) ;
#99583 = DIRECTION ( 'NONE',  ( -1.000000000000000000, 0.000000000000000000, 0.000000000000000000 ) ) ;
#99584 = CARTESIAN_POINT ( 'NONE',  ( -32.12115510384169426, 486.2840111611076281, 5.773919067741624112 ) ) ;
#99585 = ORIENTED_EDGE ( 'NONE', *, *, #79895, .F. ) ;
#99586 = FILL_AREA_STYLE ('',( #2485 ) ) ;
#99587 = DIRECTION ( 'NONE',  ( 0.000000000000000000, 0.000000000000000000, -1.000000000000000000 ) ) ;
#99588 = ORIENTED_EDGE ( 'NONE', *, *, #3666, .F. ) ;
#99589 = CARTESIAN_POINT ( 'NONE',  ( 80.60035871062690660, -30.00000000000002132, -12.85408025116223030 ) ) ;
#99590 = CARTESIAN_POINT ( 'NONE',  ( 46.92822048327062845, 13.65838325462198277, 15.00718171297847015 ) ) ;
#99591 = CARTESIAN_POINT ( 'NONE',  ( 3.340000000000000746, 0.000000000000000000, -0.4621369752184079083 ) ) ;
#99592 = DIRECTION ( 'NONE',  ( -1.000000000000000000, -1.224606353822377258E-16, -0.000000000000000000 ) ) ;
#99593 = CARTESIAN_POINT ( 'NONE',  ( 83.37423355587279161, -30.00000000000000711, 45.87345500807001741 ) ) ;
#99594 = CARTESIAN_POINT ( 'NONE',  ( -32.19491287036717608, 391.9754712875484870, 25.40006242682984094 ) ) ;
#99595 = EDGE_LOOP ( 'NONE', ( #71959, #22670, #72378, #22333, #18698 ) ) ;
#99596 = ORIENTED_EDGE ( 'NONE', *, *, #9474, .T. ) ;
#99597 = EDGE_LOOP ( 'NONE', ( #102542, #82967, #64283, #41613 ) ) ;
#99598 = VECTOR ( 'NONE', #29457, 1000.000000000000000 ) ;
#99599 = DIRECTION ( 'NONE',  ( 0.000000000000000000, 0.000000000000000000, -1.000000000000000000 ) ) ;
#99600 = CARTESIAN_POINT ( 'NONE',  ( -4.910934196423679232, 41.41789156490654733, -70.63711759939612023 ) ) ;
#99601 = AXIS2_PLACEMENT_3D ( 'NONE', #96802, #49282, #56302 ) ;
#99602 = DIRECTION ( 'NONE',  ( 0.000000000000000000, 1.000000000000000000, 0.000000000000000000 ) ) ;
#99603 = CIRCLE ( 'NONE', #99677, 4.000000000000000888 ) ;
#99604 = FACE_OUTER_BOUND ( 'NONE', #66918, .T. ) ;
#99606 = AXIS2_PLACEMENT_3D ( 'NONE', #5954, #63156, #36787 ) ;
#99605 = CARTESIAN_POINT ( 'NONE',  ( -31.36033717110301566, 339.5230286683110421, 18.44560579463051297 ) ) ;
#99607 = DIRECTION ( 'NONE',  ( 0.000000000000000000, 1.000000000000000000, 0.000000000000000000 ) ) ;
#99608 = EDGE_LOOP ( 'NONE', ( #35000, #92167 ) ) ;
#99609 = ADVANCED_FACE ( 'NONE', ( #17298 ), #84144, .T. ) ;
#99610 = FILL_AREA_STYLE ('',( #7937 ) ) ;
#99611 = ORIENTED_EDGE ( 'NONE', *, *, #96954, .T. ) ;
#99612 = DIRECTION ( 'NONE',  ( -3.552713678800500929E-15, 0.000000000000000000, 1.000000000000000000 ) ) ;
#99613 = CARTESIAN_POINT ( 'NONE',  ( 71.17493717688701338, -38.32825970135854732, 141.0574813979111752 ) ) ;
#99614 = CARTESIAN_POINT ( 'NONE',  ( 6.692588830498424457, 3.932766476276027046, -6.892929031562515796 ) ) ;
#99615 = CARTESIAN_POINT ( 'NONE',  ( 35.30318952505669472, 303.6718279376253804, 3.969031666316281459 ) ) ;
#99616 = AXIS2_PLACEMENT_3D ( 'NONE', #42731, #102021, #28181 ) ;
#99617 = CARTESIAN_POINT ( 'NONE',  ( -7.000000000000000000, 8.572527594031473190E-16, -11.82492182392400437 ) ) ;
#99618 = B_SPLINE_CURVE_WITH_KNOTS ( 'NONE', 3,
 ( #14076, #40492, #105234, #47514, #81458, #55589, #46984, #30847 ),
 .UNSPECIFIED., .F., .F.,
 ( 4, 2, 2, 4 ),
 ( 0.000000000000000000, 0.5000000000000000000, 0.7500000000000000000, 1.000000000000000000 ),
 .UNSPECIFIED. ) ;
#99619 = ORIENTED_EDGE ( 'NONE', *, *, #97472, .T. ) ;
#99620 = CARTESIAN_POINT ( 'NONE',  ( -28.31435381911579441, 34.24534108781838171, -8.450334191970046760 ) ) ;
#99621 = CARTESIAN_POINT ( 'NONE',  ( 7.317264624905434569E-15, 45.00000000000000711, -59.50000000000000000 ) ) ;
#99622 = DIRECTION ( 'NONE',  ( 0.000000000000000000, 0.000000000000000000, 1.000000000000000000 ) ) ;
#99623 = EDGE_CURVE ( 'NONE', #10104, #42316, #3093, .T. ) ;
#99624 = CARTESIAN_POINT ( 'NONE',  ( 21.19348424345033521, 294.8901562694577478, 1.945151701991110205 ) ) ;
#99625 = ORIENTED_EDGE ( 'NONE', *, *, #49313, .T. ) ;
#99626 = CIRCLE ( 'NONE', #4943, 5.000000000000002665 ) ;
#99628 = CARTESIAN_POINT ( 'NONE',  ( -23.98837369974533118, 303.9359044481634555, 10.17345894387965899 ) ) ;
#99627 =( NAMED_UNIT ( * ) PLANE_ANGLE_UNIT ( ) SI_UNIT ( $, .RADIAN. ) );
#99629 = CARTESIAN_POINT ( 'NONE',  ( 87.62222222222222001, -4.171999999999998820, 5.616230220889773285E-16 ) ) ;
#99630 = DIRECTION ( 'NONE',  ( -0.5735764363510497121, 0.8191520442889892450, 1.003171929053521665E-16 ) ) ;
#99631 = CARTESIAN_POINT ( 'NONE',  ( -8.000000000000000000, -11.74999999999999289, -9.797174393178825657E-16 ) ) ;
#99632 = DIRECTION ( 'NONE',  ( 0.000000000000000000, 0.000000000000000000, 1.000000000000000000 ) ) ;
#99633 = ADVANCED_FACE ( 'NONE', ( #59886 ), #59347, .T. ) ;
#99634 = CIRCLE ( 'NONE', #72304, 3.309500000000001663 ) ;
#99635 = CARTESIAN_POINT ( 'NONE',  ( -7.744168461338430731, 101.5374593828484109, 2.019395720771552938 ) ) ;
#99636 = ADVANCED_FACE ( 'NONE', ( #92210 ), #57712, .F. ) ;
#99637 = AXIS2_PLACEMENT_3D ( 'NONE', #46921, #46409, #37823 ) ;
#99638 = DIRECTION ( 'NONE',  ( 0.000000000000000000, 0.000000000000000000, 1.000000000000000000 ) ) ;
#99639 = CARTESIAN_POINT ( 'NONE',  ( 86.00260977355637237, -31.96737194753035993, 183.8078381457158628 ) ) ;
#99640 = CARTESIAN_POINT ( 'NONE',  ( 18.00376551885534582, 36.46870192104551478, -23.09987717863831946 ) ) ;
#99641 = CARTESIAN_POINT ( 'NONE',  ( 1.227754105814699780E-15, 67.05096163904791240, 10.02537308446410691 ) ) ;
#99642 = ORIENTED_EDGE ( 'NONE', *, *, #80092, .T. ) ;
#99643 = CARTESIAN_POINT ( 'NONE',  ( 94.59607722009114639, -57.65580962601410420, -10.11045476332422233 ) ) ;
#99644 = CARTESIAN_POINT ( 'NONE',  ( -72.06260621993654070, -38.00000000000000711, -21.47558456850402209 ) ) ;
#99645 = CARTESIAN_POINT ( 'NONE',  ( 15.76058568550410222, 34.59977121747715501, -23.83486895696631436 ) ) ;
#99646 = ADVANCED_FACE ( 'NONE', ( #10244 ), #66903, .T. ) ;
#99647 =( NAMED_UNIT ( * ) PLANE_ANGLE_UNIT ( ) SI_UNIT ( $, .RADIAN. ) );
#99648 =( BOUNDED_CURVE ( )  B_SPLINE_CURVE ( 2, ( #20848, #55259, #69876, #80072, #104902, #29967, #21885, #61808, #14271 ),
 .UNSPECIFIED., .F., .F. ) 
 B_SPLINE_CURVE_WITH_KNOTS ( ( 3, 2, 2, 2, 3 ),
 ( 0.4264705882352942123, 0.4338235294117648300, 0.4411764705882353921, 0.4485294117647060097, 0.4558823529411765718 ),
 .UNSPECIFIED. ) 
 CURVE ( )  GEOMETRIC_REPRESENTATION_ITEM ( )  RATIONAL_B_SPLINE_CURVE ( ( 0.9999999999999988898, 0.9238795325112878487, 1.000000000000000000, 0.9238795325112867385, 1.000000000000000000, 0.9238795325112867385, 1.000000000000000000, 0.9238795325112856283, 1.000000000000001110 ) ) 
 REPRESENTATION_ITEM ( '' )  );
#99649 = CARTESIAN_POINT ( 'NONE',  ( -81.29614434187884342, -30.00000000000000355, -0.4277737793982985259 ) ) ;
#99650 = AXIS2_PLACEMENT_3D ( 'NONE', #57199, #32441, #98202 ) ;
#99651 =( LENGTH_UNIT ( ) NAMED_UNIT ( * ) SI_UNIT ( .MILLI., .METRE. ) );
#99652 = CARTESIAN_POINT ( 'NONE',  ( -6.846597141950445220, 41.54610357434032863, -70.31839272209531089 ) ) ;
#99653 = FACE_OUTER_BOUND ( 'NONE', #87300, .T. ) ;
#99654 = CLOSED_SHELL ( 'NONE', ( #16277, #7853, #37977, #83469, #95420, #6315, #64108, #82778, #45279, #3886, #10508, #92066, #73803, #22488, #66937, #24760, #56276, #97074, #62053, #3855, #64164, #67118, #63566, #91858, #52510, #51627, #50486, #63298, #52434, #84617, #77775, #59141, #40131, #41549, #53370, #210, #12836, #100114, #104728, #19158, #42201, #59058, #7393, #13822, #36367, #75676, #95905, #41346, #15641, #91347, #71773, #91602, #9632, #23020, #37090, #929, #79784, #25103, #35910, #34285, #106130, #60091, #92914, #23511, #51402, #37502, #45084, #60442, #62809, #40392, #8347, #75360, #92732, #36964, #40217, #29030, #99278, #48315, #94653, #51083, #37782, #66323, #82422, #92322, #84437, #2163, #21074, #103796, #71881, #1611, #95203, #51962, #31006, #102736, #57681, #85152, #31924, #23944, #21810, #46117, #13026, #37891, #90915, #99636, #42426, #80013, #49987, #25527, #42019, #41857, #88434, #76497, #37228, #56122, #65896, #9182, #69567, #88186, #70943, #19142, #83685, #58526, #9022, #95383, #50038, #2836, #1263, #48764, #7067, #81287, #87330, #63047, #27291, #17835, #52620, #29969 ) ) ;
#99656 = CARTESIAN_POINT ( 'NONE',  ( -32.84237740334621236, 485.2251842821281116, 5.746442123025396143 ) ) ;
#99655 = DIRECTION ( 'NONE',  ( 0.000000000000000000, 1.000000000000000000, 0.000000000000000000 ) ) ;
#99657 = B_SPLINE_CURVE_WITH_KNOTS ( 'NONE', 3,
 ( #3107, #26893, #93720, #92644 ),
 .UNSPECIFIED., .F., .F.,
 ( 4, 4 ),
 ( 0.000000000000000000, 0.001861443540404501048 ),
 .UNSPECIFIED. ) ;
#99658 = CARTESIAN_POINT ( 'NONE',  ( -29.09597697838586683, 14.54318144277621982, 41.96748357178371691 ) ) ;
#99659 = CARTESIAN_POINT ( 'NONE',  ( -9.601913782316108481, -10.04478976116415012, -0.2204769333331139392 ) ) ;
#99660 = CARTESIAN_POINT ( 'NONE',  ( 5.650483388624518710, -81.54433403149616311, 2.031129859422142303 ) ) ;
#99661 = CARTESIAN_POINT ( 'NONE',  ( -69.78524612388557102, -37.99999999999998579, -22.51197996374267163 ) ) ;
#99662 = CARTESIAN_POINT ( 'NONE',  ( 19.83349330513379982, 1.593028355512270567E-15, 0.000000000000000000 ) ) ;
#99663 = CIRCLE ( 'NONE', #106515, 4.000000000000001776 ) ;
#99664 = CARTESIAN_POINT ( 'NONE',  ( -99.77890780064966236, -38.00000000000000000, 191.0086380629846872 ) ) ;
#99665 = AXIS2_PLACEMENT_3D ( 'NONE', #33891, #41414, #384 ) ;
#99666 = ORIENTED_EDGE ( 'NONE', *, *, #72556, .T. ) ;
#99667 = CARTESIAN_POINT ( 'NONE',  ( 6.481071417163344783, 9.994906101799367448, 2.652271756153596449 ) ) ;
#99668 = SURFACE_STYLE_USAGE ( .BOTH. , #41961 ) ;
#99669 = CARTESIAN_POINT ( 'NONE',  ( -7.744329845603314944, 81.53711769846543689, -2.018701143083232452 ) ) ;
#99670 = CARTESIAN_POINT ( 'NONE',  ( -55.63384620081478005, -28.59984222904408924, -26.38889157063913515 ) ) ;
#99672 = CARTESIAN_POINT ( 'NONE',  ( 37.52420368444853693, 473.1130448734259630, 17.51438724206708741 ) ) ;
#99671 = DIRECTION ( 'NONE',  ( -1.224646799147353207E-16, 1.000000000000000000, 0.000000000000000000 ) ) ;
#99673 = ORIENTED_EDGE ( 'NONE', *, *, #82549, .F. ) ;
#99674 = CARTESIAN_POINT ( 'NONE',  ( 6.291746522141169251, 1.386194408037410231, -6.829127798246559244 ) ) ;
#99675 = VERTEX_POINT ( 'NONE', #90638 ) ;
#99676 = DIRECTION ( 'NONE',  ( 1.150791560227848297E-16, -0.3420201433256725987, 0.9396926207859068736 ) ) ;
#99677 = AXIS2_PLACEMENT_3D ( 'NONE', #96271, #23453, #81114 ) ;
#99678 = VECTOR ( 'NONE', #27392, 1000.000000000000000 ) ;
#99679 = ADVANCED_FACE ( 'NONE', ( #18918, #75509 ), #10759, .T. ) ;
#99680 = CARTESIAN_POINT ( 'NONE',  ( -5.979512004945808812, 4.053280633787061937, -0.5609245978742136707 ) ) ;
#99681 = CARTESIAN_POINT ( 'NONE',  ( -81.60080408399453233, -60.00000000000000711, -26.95971957032864097 ) ) ;
#99682 = ORIENTED_EDGE ( 'NONE', *, *, #32591, .F. ) ;
#99683 = CARTESIAN_POINT ( 'NONE',  ( 33.09999999999999432, -3.309499999999999886, 4.475777889183790779E-16 ) ) ;
#99684 = CARTESIAN_POINT ( 'NONE',  ( 15.35634750254599012, 2.988828671316083430, -2.785065577016609506 ) ) ;
#99685 = AXIS2_PLACEMENT_3D ( 'NONE', #38786, #30714, #104027 ) ;
#99686 = CARTESIAN_POINT ( 'NONE',  ( 100.3941749304550228, -45.27673104686710559, 192.1863761042158103 ) ) ;
#99688 = CARTESIAN_POINT ( 'NONE',  ( -17.62428443205143580, 45.49731502040739883, 4.616218165345990165 ) ) ;
#99687 = CARTESIAN_POINT ( 'NONE',  ( 8.242617580643319286, 294.6933141679140249, -5.691011467278013214 ) ) ;
#99689 = ORIENTED_EDGE ( 'NONE', *, *, #52701, .T. ) ;
#99690 = VERTEX_POINT ( 'NONE', #76565 ) ;
#99691 = ORIENTED_EDGE ( 'NONE', *, *, #37938, .F. ) ;
#99692 = CARTESIAN_POINT ( 'NONE',  ( 30.62720677515678602, 345.4155763350589154, 19.40254811826110526 ) ) ;
#99693 = EDGE_CURVE ( 'NONE', #64080, #93305, #95755, .T. ) ;
#99694 = DIRECTION ( 'NONE',  ( 0.000000000000000000, -1.000000000000000000, 0.000000000000000000 ) ) ;
#99695 = CARTESIAN_POINT ( 'NONE',  ( 9.307364947981332293, 53.68040549777599324, 1.766710806768802877 ) ) ;
#99696 = VERTEX_POINT ( 'NONE', #36169 ) ;
#99697 = CARTESIAN_POINT ( 'NONE',  ( 16.32302039041864106, 45.99487210642904955, -4.188696036804095080 ) ) ;
#99698 =( NAMED_UNIT ( * ) PLANE_ANGLE_UNIT ( ) SI_UNIT ( $, .RADIAN. ) );
#99699 = COLOUR_RGB ( '', 0.31764706, 0.68627451, 0.89019608) ;
#99700 = CARTESIAN_POINT ( 'NONE',  ( -32.81882165182332756, 465.7334778289831547, 14.51165368403150957 ) ) ;
#99701 = CARTESIAN_POINT ( 'NONE',  ( -70.79351044798765713, -57.68242073007258597, 160.4532249112098157 ) ) ;
#99702 = CARTESIAN_POINT ( 'NONE',  ( 7.188101187500000044, -29.65625000204838813, 0.000000000000000000 ) ) ;
#99703 = LINE ( 'NONE', #25874, #35732 ) ;
#99704 = CARTESIAN_POINT ( 'NONE',  ( -35.74363442581862671, 380.1068966271811860, 4.951945592532029927 ) ) ;
#99705 = CARTESIAN_POINT ( 'NONE',  ( -6.770722853400887864, 41.58070589549304685, -58.79856860655606710 ) ) ;
#99706 = CARTESIAN_POINT ( 'NONE',  ( -86.58068678654640848, -14.21045842199428932, 15.94391106889438525 ) ) ;
#99707 = DIRECTION ( 'NONE',  ( 0.5735764363510462704, 0.8191520442889915765, 0.000000000000000000 ) ) ;
#99708 = AXIS2_PLACEMENT_3D ( 'NONE', #43240, #75599, #42166 ) ;
#99709 = CARTESIAN_POINT ( 'NONE',  ( -49.68514091287890011, -36.05463875348423386, 49.10112299445400907 ) ) ;
#99710 = VECTOR ( 'NONE', #59619, 1000.000000000000000 ) ;
#99711 = CARTESIAN_POINT ( 'NONE',  ( 4.898587196589412829E-16, -27.12499999999999645, -8.000000000000000000 ) ) ;
#99712 = ORIENTED_EDGE ( 'NONE', *, *, #26387, .T. ) ;
#99713 = CARTESIAN_POINT ( 'NONE',  ( 35.86580758070825681, 437.2863006609852050, 4.452567007867904714 ) ) ;
#99714 = EDGE_CURVE ( 'NONE', #51662, #45005, #28631, .T. ) ;
#99715 = CARTESIAN_POINT ( 'NONE',  ( -9.789044728060268596, 294.6486233851412067, -2.043184600577135690 ) ) ;
#99716 = AXIS2_PLACEMENT_3D ( 'NONE', #71447, #95221, #6179 ) ;
#99717 = ADVANCED_FACE ( 'NONE', ( #54394 ), #100443, .F. ) ;
#99718 = CARTESIAN_POINT ( 'NONE',  ( 9.805789921995232916, -0.5587250708512973008, 19.98157798524368189 ) ) ;
#99719 = ORIENTED_EDGE ( 'NONE', *, *, #82996, .F. ) ;
#99720 = CARTESIAN_POINT ( 'NONE',  ( -17.95923320562059899, 34.46585161348816229, -22.69639360600545430 ) ) ;
#99721 = CARTESIAN_POINT ( 'NONE',  ( 102.6639770615377358, -38.43513029337811560, 199.3197935500999449 ) ) ;
#99722 = CARTESIAN_POINT ( 'NONE',  ( -6.069123655689745434, 51.26876736100241772, -8.262300084537509193 ) ) ;
#99723 = CARTESIAN_POINT ( 'NONE',  ( -17.71457869773037785, 294.6047145785885846, 1.884974438337975844 ) ) ;
#99724 = CARTESIAN_POINT ( 'NONE',  ( 90.56128410203886858, 42.00000000000000000, 11.85444436786826472 ) ) ;
#99725 = CARTESIAN_POINT ( 'NONE',  ( 91.72323227205116325, -30.00000000000000355, 190.7728913354281133 ) ) ;
#99726 = EDGE_CURVE ( 'NONE', #81361, #8468, #56046, .T. ) ;
#99727 = CARTESIAN_POINT ( 'NONE',  ( 43.04469050570450150, 434.7734435962914290, 9.248231035223298591 ) ) ;
#99728 = CARTESIAN_POINT ( 'NONE',  ( -37.50813975974288184, 482.1285864697561010, 15.12809618359215946 ) ) ;
#99729 = CARTESIAN_POINT ( 'NONE',  ( 9.830769230769229594, 1.411358822780289120E-15, 0.000000000000000000 ) ) ;
#99730 = MECHANICAL_DESIGN_GEOMETRIC_PRESENTATION_REPRESENTATION (  '', ( #56600 ), #67026 ) ;
#99731 = VERTEX_POINT ( 'NONE', #106141 ) ;
#99732 = VERTEX_POINT ( 'NONE', #40361 ) ;
#99733 = CARTESIAN_POINT ( 'NONE',  ( 52.90017982257470663, -39.50313443167738825, 55.98633902596940715 ) ) ;
#99734 = CARTESIAN_POINT ( 'NONE',  ( 6.340296234547424525, 41.77218160844339678, -58.92363273660524214 ) ) ;
#99735 = CARTESIAN_POINT ( 'NONE',  ( 9.499542073392305497, 51.30140843018365615, 3.609232774367274299 ) ) ;
#99736 = VERTEX_POINT ( 'NONE', #32299 ) ;
#99737 = CARTESIAN_POINT ( 'NONE',  ( -90.94353020372604135, -38.35252991750218143, 22.60780205736431370 ) ) ;
#99738 = ORIENTED_EDGE ( 'NONE', *, *, #10199, .F. ) ;
#99739 = CARTESIAN_POINT ( 'NONE',  ( 8.000000000000000000, -29.18750000409677270, 0.000000000000000000 ) ) ;
#99740 = CARTESIAN_POINT ( 'NONE',  ( 107.3311760226882399, -38.36199077526415380, 194.2594862871855810 ) ) ;
#99741 = CARTESIAN_POINT ( 'NONE',  ( 13.02840130668396768, 21.68931673238071411, -4.976293656400714305 ) ) ;
#99742 = CARTESIAN_POINT ( 'NONE',  ( 91.04242074902893478, -60.15067329966424126, 61.63544511148911909 ) ) ;
#99743 = CARTESIAN_POINT ( 'NONE',  ( -17.62458197301598162, 43.36883309418347920, -4.616457421087988955 ) ) ;
#99745 = CIRCLE ( 'NONE', #97967, 4.172000000000009479 ) ;
#99744 = CARTESIAN_POINT ( 'NONE',  ( -1.218394774668507763, 45.86026819846987479, -17.17834643895785263 ) ) ;
#99746 = CARTESIAN_POINT ( 'NONE',  ( -35.75052666827532732, 338.6074967675372136, -1.573378144931428801 ) ) ;
#99747 = FILL_AREA_STYLE ('',( #65791 ) ) ;
#99748 = CARTESIAN_POINT ( 'NONE',  ( 73.94230384998250827, -60.00000000000001421, 171.6353201340098167 ) ) ;
#99749 = DIRECTION ( 'NONE',  ( 0.000000000000000000, -1.000000000000000000, 0.000000000000000000 ) ) ;
#99750 = DIRECTION ( 'NONE',  ( -1.000000000000000000, -1.224606353822377258E-16, -0.000000000000000000 ) ) ;
#99751 = ORIENTED_EDGE ( 'NONE', *, *, #14823, .F. ) ;
#99752 = CARTESIAN_POINT ( 'NONE',  ( 59.58870697170010544, -29.07040874811379538, 66.34822725558861123 ) ) ;
#99753 = CARTESIAN_POINT ( 'NONE',  ( -27.95499319877095701, 296.5192905871809330, -9.639268393704691462 ) ) ;
#99754 = CARTESIAN_POINT ( 'NONE',  ( 3.636386562469240082E-15, 36.30024107553216339, 29.75000000000000355 ) ) ;
#99755 = DIRECTION ( 'NONE',  ( 0.000000000000000000, 0.000000000000000000, -1.000000000000000000 ) ) ;
#99756 = DIRECTION ( 'NONE',  ( -1.000000000000000000, -1.224606353822377258E-16, -0.000000000000000000 ) ) ;
#99757 = CARTESIAN_POINT ( 'NONE',  ( -33.06942034650614914, 440.0153633844964247, 23.76350862949321296 ) ) ;
#99758 = DIRECTION ( 'NONE',  ( 1.000000000000000000, 1.224606353822377258E-16, 0.000000000000000000 ) ) ;
#99759 = SURFACE_STYLE_FILL_AREA ( #66873 ) ;
#99760 = CARTESIAN_POINT ( 'NONE',  ( -8.000000000000000000, -25.34374999999999645, -3.313708498984762496 ) ) ;
#99761 = CARTESIAN_POINT ( 'NONE',  ( -17.49999999999996447, 45.90000000000000568, 62.61746187599676716 ) ) ;
#99762 = PRESENTATION_LAYER_ASSIGNMENT (  '', '', ( #24045 ) ) ;
#99763 = AXIS2_PLACEMENT_3D ( 'NONE', #5490, #54016, #29798 ) ;
#99764 = AXIS2_PLACEMENT_3D ( 'NONE', #73864, #37971, #32378 ) ;
#99765 = CARTESIAN_POINT ( 'NONE',  ( 15.66131014786430242, 43.86972238223016518, -6.197328158278672561 ) ) ;
#99766 = ORIENTED_EDGE ( 'NONE', *, *, #54425, .F. ) ;
#99767 = CARTESIAN_POINT ( 'NONE',  ( 84.96427950620631009, -32.31981596804619983, 177.2606859094109666 ) ) ;
#99768 = CARTESIAN_POINT ( 'NONE',  ( 3.912407852882054726, -11.95585042648033003, -10.32340492114883546 ) ) ;
#99769 = CARTESIAN_POINT ( 'NONE',  ( 31.84999999999999787, 1.533819458162526451E-15, 0.000000000000000000 ) ) ;
#99770 = EDGE_LOOP ( 'NONE', ( #6125, #43707, #36218, #33197, #21395, #48766 ) ) ;
#99771 = CARTESIAN_POINT ( 'NONE',  ( -2.455508211629401138E-15, 67.05096163904791240, -10.02537308446411402 ) ) ;
#99772 = CARTESIAN_POINT ( 'NONE',  ( 4.250000000000000000, 0.000000000000000000, -10.00000000000000000 ) ) ;
#99773 = CYLINDRICAL_SURFACE ( 'NONE', #78323, 4.250000000000000000 ) ;
#99774 = CARTESIAN_POINT ( 'NONE',  ( 11.78124729766429546, -3.000000000000003109, -94.38183245066619520 ) ) ;
#99775 = EDGE_CURVE ( 'NONE', #85839, #28621, #6178, .T. ) ;
#99776 = CARTESIAN_POINT ( 'NONE',  ( -12.91373906194155730, -23.42439430174764325, -38.53824115500798086 ) ) ;
#99777 = EDGE_CURVE ( 'NONE', #22089, #13365, #33773, .T. ) ;
#99778 = FILL_AREA_STYLE_COLOUR ( '', #680 ) ;
#99779 = B_SPLINE_CURVE_WITH_KNOTS ( 'NONE', 3,
 ( #45181, #35509, #61362, #85638, #11711, #53260, #10649, #68388, #101799, #19875, #94255, #69450, #27965, #43043, #18250, #52710, #34978, #60830, #18803, #100204 ),
 .UNSPECIFIED., .F., .F.,
 ( 4, 2, 2, 2, 2, 2, 2, 2, 2, 4 ),
 ( 0.007223778813970589859, 0.007727726098206796727, 0.008231673382443002729, 0.008735620666679209598, 0.009239567950915416467, 0.009743515235151623335, 0.01024746251938783020, 0.01049943616150593451, 0.01075140980362403881, 0.01125535708786024047 ),
 .UNSPECIFIED. ) ;
#99780 = CARTESIAN_POINT ( 'NONE',  ( 47.42216474123039660, -60.00000000000000000, 65.72069959097976266 ) ) ;
#99781 = CARTESIAN_POINT ( 'NONE',  ( 7.744329845603314944, 108.4628823015345773, -2.018701143083236449 ) ) ;
#99782 = CARTESIAN_POINT ( 'NONE',  ( 19.45299894497249227, -16.87718219434115952, 31.48667012707523938 ) ) ;
#99784 = CARTESIAN_POINT ( 'NONE',  ( -14.98510621630312301, 22.22666106603950453, -3.896433925070799553 ) ) ;
#99783 = CARTESIAN_POINT ( 'NONE',  ( -16.40833728792867419, -23.49546845913443605, 36.14695687728993789 ) ) ;
#99785 = CARTESIAN_POINT ( 'NONE',  ( -3.313708498984798467, -16.53124999999999289, -7.999999999999961808 ) ) ;
#99786 = CARTESIAN_POINT ( 'NONE',  ( 2.977408999572650927, -14.37500000204838635, -7.188101187500001821 ) ) ;
#99787 = CARTESIAN_POINT ( 'NONE',  ( 30.83282128361384977, 298.3240041198961308, -1.233783556676444793 ) ) ;
#99788 = CARTESIAN_POINT ( 'NONE',  ( -6.601567268551446155, 5.319966374295964862, -7.792327460285857654 ) ) ;
#99789 = PRESENTATION_LAYER_ASSIGNMENT (  '', '', ( #55045 ) ) ;
#99790 = ORIENTED_EDGE ( 'NONE', *, *, #79227, .F. ) ;
#99791 = CARTESIAN_POINT ( 'NONE',  ( -12.50707228786319547, -23.21292011592133164, -38.54089711067194912 ) ) ;
#99792 = CARTESIAN_POINT ( 'NONE',  ( -19.50000000000017053, 49.99999999999997868, 59.86364615470554895 ) ) ;
#99793 = DIRECTION ( 'NONE',  ( 0.000000000000000000, 0.000000000000000000, 1.000000000000000000 ) ) ;
#99794 = CARTESIAN_POINT ( 'NONE',  ( 19.34999999999999787, 3.309500000000003439, 4.052968581778167743E-16 ) ) ;
#99796 = CARTESIAN_POINT ( 'NONE',  ( 15.97931424437294723, -47.40880484825536456, -34.25640142802624410 ) ) ;
#99795 = CARTESIAN_POINT ( 'NONE',  ( 5.126025408076855250, 54.24534041977454280, 6.039183340882647855 ) ) ;
#99797 = ORIENTED_EDGE ( 'NONE', *, *, #104624, .F. ) ;
#99798 = AXIS2_PLACEMENT_3D ( 'NONE', #17552, #59601, #67685 ) ;
#99799 = CARTESIAN_POINT ( 'NONE',  ( 13.97101686926742481, 20.79977776867546879, -6.270362741406088958 ) ) ;
#99800 = PRESENTATION_STYLE_ASSIGNMENT (( #66368 ) ) ;
#99801 = ORIENTED_EDGE ( 'NONE', *, *, #97228, .T. ) ;
#99802 = EDGE_CURVE ( 'NONE', #5652, #23052, #22631, .T. ) ;
#99803 = DIRECTION ( 'NONE',  ( 1.000000000000000000, 0.000000000000000000, 0.000000000000000000 ) ) ;
#99804 = CARTESIAN_POINT ( 'NONE',  ( -23.98952478535236210, 41.62026329535294877, -74.32034878064006023 ) ) ;
#99805 = CARTESIAN_POINT ( 'NONE',  ( -106.1131432879537044, -60.00000000000000711, 117.1109480045180078 ) ) ;
#99806 = DIRECTION ( 'NONE',  ( -1.000000000000000000, -1.224606353822377258E-16, -0.000000000000000000 ) ) ;
#99807 = CARTESIAN_POINT ( 'NONE',  ( 26.97491686565329161, 307.4599153070161606, -9.420584459367196573 ) ) ;
#99808 = CARTESIAN_POINT ( 'NONE',  ( 40.26058501384567023, 460.2706387420194005, 2.258779328630807548 ) ) ;
#99810 = LINE ( 'NONE', #34056, #37461 ) ;
#99809 = CARTESIAN_POINT ( 'NONE',  ( 0.000000000000000000, -5.000000000000002665, -75.00000000000001421 ) ) ;
#99811 = AXIS2_PLACEMENT_3D ( 'NONE', #14437, #95919, #23107 ) ;
#99812 = CARTESIAN_POINT ( 'NONE',  ( -84.74062074580929504, -28.95439361776484333, 169.9357238595956971 ) ) ;
#99813 = ORIENTED_EDGE ( 'NONE', *, *, #48765, .F. ) ;
#99814 = CARTESIAN_POINT ( 'NONE',  ( 6.392921707093107919, 41.54610357469336179, -70.64273453041053585 ) ) ;
#99815 = ORIENTED_EDGE ( 'NONE', *, *, #85517, .T. ) ;
#99816 = ORIENTED_EDGE ( 'NONE', *, *, #6597, .T. ) ;
#99817 = CARTESIAN_POINT ( 'NONE',  ( 16.33361799548379523, -5.000000000000000888, 6.123233995736769241E-16 ) ) ;
#99818 = EDGE_CURVE ( 'NONE', #39260, #103713, #23682, .T. ) ;
#99819 = DIRECTION ( 'NONE',  ( 0.000000000000000000, -1.000000000000000000, 0.000000000000000000 ) ) ;
#99820 = ORIENTED_EDGE ( 'NONE', *, *, #67494, .T. ) ;
#99821 = CARTESIAN_POINT ( 'NONE',  ( 68.70539558375507738, 6.856755485862130937E-15, 0.000000000000000000 ) ) ;
#99822 = DIRECTION ( 'NONE',  ( 0.000000000000000000, -1.000000000000000000, 0.000000000000000000 ) ) ;
#99823 = FACE_OUTER_BOUND ( 'NONE', #22860, .T. ) ;
#99824 = DIRECTION ( 'NONE',  ( 0.3009093847692427270, 0.4108943393899624485, 0.8605924610494111171 ) ) ;
#99825 = CARTESIAN_POINT ( 'NONE',  ( -1.484885661199817548E-13, 25.16821295365152622, -40.75000000000150635 ) ) ;
#99826 = CARTESIAN_POINT ( 'NONE',  ( -5.000000000000000000, -13.85485428919850648, 10.16324337853805204 ) ) ;
#99827 = AXIS2_PLACEMENT_3D ( 'NONE', #54796, #61875, #21944 ) ;
#99828 = CARTESIAN_POINT ( 'NONE',  ( 102.4475954893556633, -30.00000000000004263, 111.1011446524310742 ) ) ;
#99829 = CARTESIAN_POINT ( 'NONE',  ( -106.8727010878311745, -14.21045842199433373, 167.8788319932906461 ) ) ;
#99830 = CARTESIAN_POINT ( 'NONE',  ( -56.69927050699357807, -53.38582612393514637, 70.13001638502136359 ) ) ;
#99831 = ORIENTED_EDGE ( 'NONE', *, *, #100801, .T. ) ;
#99832 = CARTESIAN_POINT ( 'NONE',  ( 28.58349330513380337, 1.593028355512270962E-15, 0.000000000000000000 ) ) ;
#99833 = CARTESIAN_POINT ( 'NONE',  ( 114.4431422422120619, -60.00000000000976286, 166.1592868538951393 ) ) ;
#99834 = ORIENTED_EDGE ( 'NONE', *, *, #60292, .T. ) ;
#99835 = CARTESIAN_POINT ( 'NONE',  ( 2.999727326758741430, -29.02930189954776807, 28.72327379294769401 ) ) ;
#99836 = CARTESIAN_POINT ( 'NONE',  ( -105.1952383919716425, -60.15502232595932242, 151.5760161608686758 ) ) ;
#99837 = CARTESIAN_POINT ( 'NONE',  ( -7.188101187500000933, -15.87500000204838635, -2.977408999572651371 ) ) ;
#99838 = DIRECTION ( 'NONE',  ( 0.3934424543276984210, -0.4342828891349996834, -0.8103094515906591466 ) ) ;
#99839 = EDGE_CURVE ( 'NONE', #60981, #100031, #98206, .T. ) ;
#99840 = DIRECTION ( 'NONE',  ( 0.000000000000000000, 1.000000000000000000, 0.000000000000000000 ) ) ;
#99841 = VERTEX_POINT ( 'NONE', #57587 ) ;
#99842 = LINE ( 'NONE', #58874, #37252 ) ;
#99843 = CARTESIAN_POINT ( 'NONE',  ( -73.64671352647415858, -60.00000000000000000, 168.6311605301084455 ) ) ;
#99844 = DIRECTION ( 'NONE',  ( -1.000000000000000000, -1.224606353822377258E-16, -0.000000000000000000 ) ) ;
#99845 = CARTESIAN_POINT ( 'NONE',  ( 5.082755093536324154, -19.71875000204838457, 5.082755093536326818 ) ) ;
#99846 = CARTESIAN_POINT ( 'NONE',  ( -0.3340761435813103253, 37.19397736156746959, -27.29255811281833033 ) ) ;
#99847 = DIRECTION ( 'NONE',  ( 0.000000000000000000, 0.000000000000000000, 1.000000000000000000 ) ) ;
#99848 = CARTESIAN_POINT ( 'NONE',  ( 7.046289519167717508, -83.69408180055621926, -3.789821819998814512 ) ) ;
#99849 = CARTESIAN_POINT ( 'NONE',  ( -23.43684916743750080, 295.2641918988800285, 10.02474406024658293 ) ) ;
#99850 = CARTESIAN_POINT ( 'NONE',  ( 32.83708119314772489, 465.7129474592467773, 11.08629381895457477 ) ) ;
#99851 = EDGE_CURVE ( 'NONE', #30344, #8292, #32008, .T. ) ;
#99852 = CARTESIAN_POINT ( 'NONE',  ( -9.955499077880663350, 44.05779190055731220, -12.94048145135424299 ) ) ;
#99853 = CARTESIAN_POINT ( 'NONE',  ( -23.21751746555168339, 27.38103382803512176, 33.20617127781681432 ) ) ;
#99854 = CARTESIAN_POINT ( 'NONE',  ( 86.10036459384876650, -60.00000000000004263, 13.51756007424883599 ) ) ;
#99855 = UNCERTAINTY_MEASURE_WITH_UNIT (LENGTH_MEASURE( 1.000000000000000082E-05 ), #5081, 'distance_accuracy_value', 'NONE');
#99856 = CARTESIAN_POINT ( 'NONE',  ( -31.45780706891997269, -36.02065666347889561, 33.04706042998527238 ) ) ;
#99857 = AXIS2_PLACEMENT_3D ( 'NONE', #17601, #68267, #42382 ) ;
#99858 = CARTESIAN_POINT ( 'NONE',  ( -1.257803174857021755, -49.99999999975079845, 101.3280723981089722 ) ) ;
#99859 = CARTESIAN_POINT ( 'NONE',  ( 43.48316998106664499, -56.79513185587920532, 46.31952888274560109 ) ) ;
#99860 = CARTESIAN_POINT ( 'NONE',  ( 34.83349330513380693, 1.593028355512270962E-15, 0.000000000000000000 ) ) ;
#99861 = ORIENTED_EDGE ( 'NONE', *, *, #4269, .T. ) ;
#99862 = CARTESIAN_POINT ( 'NONE',  ( 0.000000000000000000, 0.000000000000000000, 0.000000000000000000 ) ) ;
#99863 = EDGE_CURVE ( 'NONE', #7084, #74084, #61341, .T. ) ;
#99864 = CARTESIAN_POINT ( 'NONE',  ( -80.06624740215067959, -38.78696431783050258, 193.1076717199356665 ) ) ;
#99865 = ORIENTED_EDGE ( 'NONE', *, *, #92875, .T. ) ;
#99867 = CARTESIAN_POINT ( 'NONE',  ( 40.95420997525301487, 387.0967036739339164, 27.26945002580065136 ) ) ;
#99866 = LINE ( 'NONE', #64847, #100289 ) ;
#99868 = CARTESIAN_POINT ( 'NONE',  ( 79.70884519849728633, -60.00000000000013500, 171.5327084686719274 ) ) ;
#99870 = EDGE_CURVE ( 'NONE', #53830, #23893, #71621, .T. ) ;
#99869 = CARTESIAN_POINT ( 'NONE',  ( -48.69610342378912549, 8.416294429711154379, -16.66514711139025806 ) ) ;
#99871 = CARTESIAN_POINT ( 'NONE',  ( -7.386518100075204707, 41.27037529920123404, -59.50133825707656143 ) ) ;
#99872 = DIRECTION ( 'NONE',  ( 0.000000000000000000, -1.000000000000000000, 0.000000000000000000 ) ) ;
#99873 = DIRECTION ( 'NONE',  ( 0.000000000000000000, -1.000000000000000000, 0.000000000000000000 ) ) ;
#99874 = CARTESIAN_POINT ( 'NONE',  ( 4.898587196589412829E-16, -25.81250000409677270, -8.000000000000000000 ) ) ;
#99875 =( GEOMETRIC_REPRESENTATION_CONTEXT ( 3 ) GLOBAL_UNCERTAINTY_ASSIGNED_CONTEXT ( ( #1942 ) ) GLOBAL_UNIT_ASSIGNED_CONTEXT ( ( #98006, #63001, #54877 ) ) REPRESENTATION_CONTEXT ( 'NONE', 'WORKASPACE' ) );
#99876 = CARTESIAN_POINT ( 'NONE',  ( 103.6221050402626105, -59.99999999999999289, 102.2249670950544527 ) ) ;
#99877 = CARTESIAN_POINT ( 'NONE',  ( 102.9313392694734688, 1.016364837396684119E-14, 0.000000000000000000 ) ) ;
#99878 = EDGE_CURVE ( 'NONE', #9941, #20019, #78483, .T. ) ;
#99879 = CARTESIAN_POINT ( 'NONE',  ( -38.88026246212550774, 468.9844136736957694, 0.4637902098120869065 ) ) ;
#99880 = PRESENTATION_LAYER_ASSIGNMENT (  '', '', ( #93032 ) ) ;
#99881 = ORIENTED_EDGE ( 'NONE', *, *, #49126, .F. ) ;
#99882 = CARTESIAN_POINT ( 'NONE',  ( -95.93003187330748460, -29.99999999999981526, 191.2983833983815032 ) ) ;
#99883 = EDGE_LOOP ( 'NONE', ( #22233, #19280, #40614, #48660, #80533, #67862, #78596 ) ) ;
#99884 = CIRCLE ( 'NONE', #6872, 11.00000000000000000 ) ;
#99885 = CARTESIAN_POINT ( 'NONE',  ( 26.03569976539403186, 37.04610443471195680, -9.459197729484262851 ) ) ;
#99886 = DIRECTION ( 'NONE',  ( 0.000000000000000000, 0.000000000000000000, 1.000000000000000000 ) ) ;
#99887 = CARTESIAN_POINT ( 'NONE',  ( 30.83612787059712446, 330.9523264370013180, 16.54848976118583437 ) ) ;
#99888 = CARTESIAN_POINT ( 'NONE',  ( -33.32951764101208880, 490.0033476588132544, 11.19754049617970182 ) ) ;
#99889 = CARTESIAN_POINT ( 'NONE',  ( -2.977408999572654480, -18.50000000204838457, 7.188101187499999156 ) ) ;
#99890 = DIRECTION ( 'NONE',  ( 0.000000000000000000, 0.000000000000000000, -1.000000000000000000 ) ) ;
#99891 = VECTOR ( 'NONE', #97186, 1000.000000000000000 ) ;
#99892 = DIRECTION ( 'NONE',  ( 0.000000000000000000, 0.000000000000000000, -1.000000000000000000 ) ) ;
#99893 = ORIENTED_EDGE ( 'NONE', *, *, #91354, .T. ) ;
#99894 = CARTESIAN_POINT ( 'NONE',  ( 80.64106222537829183, -56.90139274204167918, 175.6386766945464046 ) ) ;
#99895 = CIRCLE ( 'NONE', #22407, 1.999999999999999778 ) ;
#99896 = CARTESIAN_POINT ( 'NONE',  ( -63.67138272020815748, 38.95383793066860534, -8.334564508068563526 ) ) ;
#99897 = ORIENTED_EDGE ( 'NONE', *, *, #53580, .F. ) ;
#99898 = CARTESIAN_POINT ( 'NONE',  ( -50.94745919686192082, 50.00000000000000000, -37.05882352941185331 ) ) ;
#99899 = CARTESIAN_POINT ( 'NONE',  ( 16.14595037822613932, 12.99999999999999289, -8.749999999999944933 ) ) ;
#99900 = CARTESIAN_POINT ( 'NONE',  ( -7.188101187500002709, -9.312500002048382797, 2.977408999572647819 ) ) ;
#99901 = LINE ( 'NONE', #42196, #105415 ) ;
#99902 = SURFACE_STYLE_FILL_AREA ( #10875 ) ;
#99903 = CARTESIAN_POINT ( 'NONE',  ( -24.36717267311885138, 304.1505144958332494, 10.22149614222675140 ) ) ;
#99904 = CARTESIAN_POINT ( 'NONE',  ( -32.37468555527969016, 435.2081350238080404, 18.54045473102533492 ) ) ;
#99905 = EDGE_CURVE ( 'NONE', #17539, #34141, #106024, .T. ) ;
#99906 = ORIENTED_EDGE ( 'NONE', *, *, #75385, .F. ) ;
#99907 = CARTESIAN_POINT ( 'NONE',  ( 0.000000000000000000, -4.000000000000003553, 37.00000000000000000 ) ) ;
#99908 = AXIS2_PLACEMENT_3D ( 'NONE', #106401, #97260, #72971 ) ;
#99909 = ADVANCED_FACE ( 'NONE', ( #2021 ), #17698, .T. ) ;
#99910 = CARTESIAN_POINT ( 'NONE',  ( 43.00000000000000000, 461.4080316921935605, 3.462976341553817949 ) ) ;
#99911 = CARTESIAN_POINT ( 'NONE',  ( 87.19800390447835525, -46.42919513289680822, 191.1394352392929932 ) ) ;
#99912 = CARTESIAN_POINT ( 'NONE',  ( 29.68315524076959377, 13.12249633091058243, -39.60535821593525441 ) ) ;
#99913 = CARTESIAN_POINT ( 'NONE',  ( 4.401442555609581635E-16, -33.78125000204838813, -7.188101187500000044 ) ) ;
#99914 = CARTESIAN_POINT ( 'NONE',  ( 35.11650669486618170, 1.474610560812782335E-15, 0.000000000000000000 ) ) ;
#99915 = DIRECTION ( 'NONE',  ( 0.000000000000000000, 0.000000000000000000, -1.000000000000000000 ) ) ;
#99916 = ITEM_DEFINED_TRANSFORMATION ( 'NONE', 'NONE', #90352,  #10728 ) ;
#99917 = ORIENTED_EDGE ( 'NONE', *, *, #16465, .F. ) ;
#99918 = CARTESIAN_POINT ( 'NONE',  ( -35.49824309011606260, 438.0806692989499993, 4.093885194488227519 ) ) ;
#99919 = CARTESIAN_POINT ( 'NONE',  ( 22.33349330513380337, 1.593028355512270567E-15, 0.000000000000000000 ) ) ;
#99920 = CARTESIAN_POINT ( 'NONE',  ( -10.00791540606109820, 7.488695628611232280, -4.999999999999999112 ) ) ;
#99921 = FACE_OUTER_BOUND ( 'NONE', #17331, .T. ) ;
#99922 = EDGE_CURVE ( 'NONE', #52946, #57728, #83625, .T. ) ;
#99923 = AXIS2_PLACEMENT_3D ( 'NONE', #81781, #97989, #23067 ) ;
#99924 = ORIENTED_EDGE ( 'NONE', *, *, #102859, .F. ) ;
#99925 = CARTESIAN_POINT ( 'NONE',  ( -42.36808196472508570, 461.6713445545159402, 3.771400599639992635 ) ) ;
#99926 = CARTESIAN_POINT ( 'NONE',  ( 112.0387186725491091, -57.67108335773423278, 191.1994195377486108 ) ) ;
#99927 = VERTEX_POINT ( 'NONE', #83476 ) ;
#99928 = VECTOR ( 'NONE', #84028, 1000.000000000000000 ) ;
#99929 = EDGE_CURVE ( 'NONE', #12817, #24672, #25156, .T. ) ;
#99930 = CARTESIAN_POINT ( 'NONE',  ( -9.554774132531640873, 51.29119502155290178, -3.542050502601651552 ) ) ;
#99931 = CARTESIAN_POINT ( 'NONE',  ( 0.000000000000000000, 0.000000000000000000, 0.000000000000000000 ) ) ;
#99932 = CARTESIAN_POINT ( 'NONE',  ( 37.56673239365870387, 25.47613764497372557, 13.45617127780999134 ) ) ;
#99933 = CARTESIAN_POINT ( 'NONE',  ( -90.45134624145916291, -60.00000000000001421, 202.0642490602653538 ) ) ;
#99934 = DIRECTION ( 'NONE',  ( -1.000000000000000000, 0.000000000000000000, 0.000000000000000000 ) ) ;
#99935 = CARTESIAN_POINT ( 'NONE',  ( -43.31389755119099050, 487.3431498771909105, 8.040475431002969131 ) ) ;
#99936 = CARTESIAN_POINT ( 'NONE',  ( 8.000000000000000000, 9.797174393178825657E-16, -0.02540000000000007530 ) ) ;
#99937 = CARTESIAN_POINT ( 'NONE',  ( -83.55671512945748702, -53.74164608449824954, 187.8046252073974358 ) ) ;
#99938 = ORIENTED_EDGE ( 'NONE', *, *, #98376, .T. ) ;
#99939 = FACE_OUTER_BOUND ( 'NONE', #48441, .T. ) ;
#99940 = VECTOR ( 'NONE', #11115, 1000.000000000000000 ) ;
#99941 =( BOUNDED_CURVE ( )  B_SPLINE_CURVE ( 2, ( #8768, #24471, #9819, #90763, #81568 ),
 .UNSPECIFIED., .F., .F. ) 
 B_SPLINE_CURVE_WITH_KNOTS ( ( 3, 2, 3 ),
 ( 0.000000000000000000, 0.9999798024780033323, 1.000000000000000000 ),
 .UNSPECIFIED. ) 
 CURVE ( )  GEOMETRIC_REPRESENTATION_ITEM ( )  RATIONAL_B_SPLINE_CURVE ( ( 1.000000000000000666, 1.857142857142856984, 1.000000000000000000, 1.000000000000000000, 1.000000000000000000 ) ) 
 REPRESENTATION_ITEM ( '' )  );
#99942 = AXIS2_PLACEMENT_3D ( 'NONE', #16844, #15767, #48121 ) ;
#99943 = VERTEX_POINT ( 'NONE', #26360 ) ;
#99944 = CARTESIAN_POINT ( 'NONE',  ( -7.412906595240167817, -12.64188272852255324, 3.014362223629234894 ) ) ;
#99945 = EDGE_CURVE ( 'NONE', #85904, #65856, #82745, .T. ) ;
#99946 = CARTESIAN_POINT ( 'NONE',  ( 1.000000000000000000, -48.56827653475308182, 2.661071982229600064 ) ) ;
#99947 = CARTESIAN_POINT ( 'NONE',  ( -85.13337042228866380, -52.74891044688261843, -12.49663770922077255 ) ) ;
#99948 = AXIS2_PLACEMENT_3D ( 'NONE', #55584, #95546, #88522 ) ;
#99949 = CARTESIAN_POINT ( 'NONE',  ( -5.175128423392746591, -10.69566144610010028, -10.53077195007410793 ) ) ;
#99950 = CARTESIAN_POINT ( 'NONE',  ( -15.43483729484961842, 44.00314096588699897, 5.765889254525177421 ) ) ;
#99951 = CARTESIAN_POINT ( 'NONE',  ( -9.317330270139585480, -11.89270385133543506, 9.146501922081970548 ) ) ;
#99952 = CARTESIAN_POINT ( 'NONE',  ( -6.677362058809294787, -11.98847278904867508, 9.465251842568026319 ) ) ;
#99953 = CARTESIAN_POINT ( 'NONE',  ( -23.70422451874885184, 42.00000000000000000, -88.20421627933662023 ) ) ;
#99954 = CARTESIAN_POINT ( 'NONE',  ( 30.11650669486618881, -3.999999999999998224, 0.000000000000000000 ) ) ;
#99955 = DIRECTION ( 'NONE',  ( 0.3009093847692517198, -0.4108943393901564600, -0.8605924610493154159 ) ) ;
#99956 = AXIS2_PLACEMENT_3D ( 'NONE', #13629, #21771, #37432 ) ;
#99957 = CARTESIAN_POINT ( 'NONE',  ( 59.37626172009473180, -60.00000000000000000, -38.24869620007160620 ) ) ;
#99958 = B_SPLINE_CURVE_WITH_KNOTS ( 'NONE', 3,
 ( #5080, #36945, #28874, #38013, #96226, #37484, #54130, #30437, #4546, #63330 ),
 .UNSPECIFIED., .F., .F.,
 ( 4, 2, 2, 2, 4 ),
 ( 0.000000000000000000, 0.2500000000000000000, 0.5000000000000000000, 0.7500000000000000000, 1.000000000000000000 ),
 .UNSPECIFIED. ) ;
#99959 = CARTESIAN_POINT ( 'NONE',  ( -74.24640087699403068, -25.59795120301134830, 107.9182274487227602 ) ) ;
#99960 = ORIENTED_EDGE ( 'NONE', *, *, #59012, .T. ) ;
#99961 = CARTESIAN_POINT ( 'NONE',  ( 75.52921836606891759, -59.99999999999984368, 193.8580410961210134 ) ) ;
#99962 = PRESENTATION_STYLE_ASSIGNMENT (( #67079 ) ) ;
#99963 = CARTESIAN_POINT ( 'NONE',  ( 93.82677057603169146, -57.67444542026858301, 11.80858161689750752 ) ) ;
#99964 = ORIENTED_EDGE ( 'NONE', *, *, #39007, .T. ) ;
#99965 = CARTESIAN_POINT ( 'NONE',  ( 7.481431019367137836, 52.00404499236192635, -3.434350709771399224 ) ) ;
#99966 = AXIS2_PLACEMENT_3D ( 'NONE', #79792, #5387, #15048 ) ;
#99967 = DIRECTION ( 'NONE',  ( 0.000000000000000000, 0.000000000000000000, 1.000000000000000000 ) ) ;
#99968 = VERTEX_POINT ( 'NONE', #14261 ) ;
#99969 = DIRECTION ( 'NONE',  ( -0.000000000000000000, -1.000000000000000000, -0.000000000000000000 ) ) ;
#99970 = CARTESIAN_POINT ( 'NONE',  ( 72.11682663846713126, 6.975173280561618775E-15, 0.000000000000000000 ) ) ;
#99971 = FACE_OUTER_BOUND ( 'NONE', #70959, .T. ) ;
#99972 = CARTESIAN_POINT ( 'NONE',  ( 4.401442555609581635E-16, -15.78125000204838635, -7.188101187500000044 ) ) ;
#99973 = CARTESIAN_POINT ( 'NONE',  ( -48.60160210973805306, 15.38206115941372865, 14.48795722268544672 ) ) ;
#99974 = CARTESIAN_POINT ( 'NONE',  ( 6.539732759932831208, -4.285714285714297134, -24.41571844174604067 ) ) ;
#99975 = DIRECTION ( 'NONE',  ( -0.7071067811865456854, 0.000000000000000000, 0.7071067811865493491 ) ) ;
#99976 = CARTESIAN_POINT ( 'NONE',  ( -12.13034742782428310, 49.99999999999999289, -93.82352941176471006 ) ) ;
#99977 = ADVANCED_FACE ( 'NONE', ( #73021 ), #80065, .F. ) ;
#99978 = CARTESIAN_POINT ( 'NONE',  ( -12.48710243631036754, -3.525193987328853584, -13.72488916828378613 ) ) ;
#99979 = CARTESIAN_POINT ( 'NONE',  ( -5.756917790976768146, 47.99999999999999289, -98.90122916984913104 ) ) ;
#99980 = ORIENTED_EDGE ( 'NONE', *, *, #72608, .F. ) ;
#99981 = CARTESIAN_POINT ( 'NONE',  ( -7.425259529285893834, 41.08730259631308712, -69.63985907319367641 ) ) ;
#99982 = CARTESIAN_POINT ( 'NONE',  ( 32.67496446562977752, -36.02319022030835072, 33.54900523351410868 ) ) ;
#99983 = ADVANCED_FACE ( 'NONE', ( #47164 ), #81126, .T. ) ;
#99984 = CARTESIAN_POINT ( 'NONE',  ( 35.52983581801517943, 407.4223022866293604, 7.047109836617410750 ) ) ;
#99985 = ORIENTED_EDGE ( 'NONE', *, *, #68613, .T. ) ;
#99986 = ADVANCED_FACE ( 'NONE', ( #96285 ), #100875, .T. ) ;
#99987 = CARTESIAN_POINT ( 'NONE',  ( -0.5285977877722420892, 18.60303940554467772, 49.36091255612689110 ) ) ;
#99988 = CIRCLE ( 'NONE', #68988, 4.000000000000001776 ) ;
#99989 = VERTEX_POINT ( 'NONE', #88705 ) ;
#99991 = CARTESIAN_POINT ( 'NONE',  ( 0.6508621380849222149, 8.763657152406448603, -7.907633014911220393 ) ) ;
#99990 = CARTESIAN_POINT ( 'NONE',  ( 0.000000000000000000, 3.004629197474323585E-15, 8.000000000000000000 ) ) ;
#99992 = CARTESIAN_POINT ( 'NONE',  ( 1.078140322363270668E-05, -30.00000000000000000, 28.88964995960238014 ) ) ;
#99993 = DIRECTION ( 'NONE',  ( 0.000000000000000000, 0.000000000000000000, 1.000000000000000000 ) ) ;
#99994 = DIRECTION ( 'NONE',  ( -1.000000000000000000, -0.000000000000000000, -0.000000000000000000 ) ) ;
#99995 = CARTESIAN_POINT ( 'NONE',  ( 32.81762910953230516, 465.7339109553614662, 14.50750636005276384 ) ) ;
#99996 = CARTESIAN_POINT ( 'NONE',  ( 0.1551307017114974263, 12.93301843199755297, -51.74240478515310571 ) ) ;
#99997 = ORIENTED_EDGE ( 'NONE', *, *, #97472, .F. ) ;
#99998 = CARTESIAN_POINT ( 'NONE',  ( 65.89753327251730752, -60.00000000000000000, -33.92370292367453288 ) ) ;
#99999 = CARTESIAN_POINT ( 'NONE',  ( 32.93513049338609733, 465.6726574193332908, 10.66039033145344384 ) ) ;
#100000 = ADVANCED_FACE ( 'NONE', ( #39105 ), #63021, .T. ) ;
#100001 = PRESENTATION_STYLE_ASSIGNMENT (( #35307 ) ) ;
#100002 = DIRECTION ( 'NONE',  ( -0.000000000000000000, 1.000000000000000000, -0.000000000000000000 ) ) ;
#100003 = ORIENTED_EDGE ( 'NONE', *, *, #34461, .F. ) ;
#100004 = CONICAL_SURFACE ( 'NONE', #29378, 3.340000000000000746, 0.9599310885968781459 ) ;
#100005 = DIRECTION ( 'NONE',  ( -1.000000000000000000, -1.224606353822377258E-16, -0.000000000000000000 ) ) ;
#100006 = VERTEX_POINT ( 'NONE', #54718 ) ;
#100007 = ORIENTED_EDGE ( 'NONE', *, *, #56826, .F. ) ;
#100008 = AXIS2_PLACEMENT_3D ( 'NONE', #79041, #13758, #46668 ) ;
#100009 = CARTESIAN_POINT ( 'NONE',  ( 8.000000000000000000, -10.90624999999999467, -3.313708498984761164 ) ) ;
#100010 = DIRECTION ( 'NONE',  ( -0.000000000000000000, 0.1742756985702848260, 0.9846968979781743903 ) ) ;
#100011 = CARTESIAN_POINT ( 'NONE',  ( 9.349999999999997868, 1.533819458162526451E-15, 0.000000000000000000 ) ) ;
#100012 = CARTESIAN_POINT ( 'NONE',  ( 84.49694251429671965, -45.28645896664576043, -6.726666319064526611 ) ) ;
#100013 = CARTESIAN_POINT ( 'NONE',  ( -40.64764563337315195, 311.8966148236026470, -5.951010960877825440 ) ) ;
#100014 = CARTESIAN_POINT ( 'NONE',  ( 8.099999999999999645, 3.752776749732561257, -6.499999999999999112 ) ) ;
#100015 = SURFACE_STYLE_FILL_AREA ( #42309 ) ;
#100016 = ORIENTED_EDGE ( 'NONE', *, *, #1973, .F. ) ;
#100017 = LINE ( 'NONE', #59046, #90805 ) ;
#100018 = EDGE_LOOP ( 'NONE', ( #73573, #36528, #101424, #68873 ) ) ;
#100019 = DIRECTION ( 'NONE',  ( 0.000000000000000000, 0.000000000000000000, -1.000000000000000000 ) ) ;
#100020 = DIRECTION ( 'NONE',  ( 0.000000000000000000, -1.000000000000000000, 0.000000000000000000 ) ) ;
#100022 = EDGE_LOOP ( 'NONE', ( #25837, #2359 ) ) ;
#100021 = LINE ( 'NONE', #60137, #18395 ) ;
#100023 = CARTESIAN_POINT ( 'NONE',  ( 72.91780076713102687, -42.96040658466132101, 114.3445280546203122 ) ) ;
#100024 = VERTEX_POINT ( 'NONE', #22410 ) ;
#100025 = CIRCLE ( 'NONE', #26018, 3.309499999999999886 ) ;
#100026 = CARTESIAN_POINT ( 'NONE',  ( 56.90650429242290187, 38.95383793070381984, -28.99688671942671547 ) ) ;
#100027 = CARTESIAN_POINT ( 'NONE',  ( -7.188101187500000933, -24.50000000204839168, -2.977408999572651371 ) ) ;
#100028 =( GEOMETRIC_REPRESENTATION_CONTEXT ( 3 ) GLOBAL_UNCERTAINTY_ASSIGNED_CONTEXT ( ( #49481 ) ) GLOBAL_UNIT_ASSIGNED_CONTEXT ( ( #1970, #41907, #41378 ) ) REPRESENTATION_CONTEXT ( 'NONE', 'WORKASPACE' ) );
#100029 = CARTESIAN_POINT ( 'NONE',  ( -114.2271649293462445, -57.67113267762195505, 172.5270642037310722 ) ) ;
#100030 = EDGE_CURVE ( 'NONE', #44884, #59052, #84087, .T. ) ;
#100031 = VERTEX_POINT ( 'NONE', #39639 ) ;
#100032 = CONICAL_SURFACE ( 'NONE', #46606, 4.172000000000001485, 0.9599310885968750373 ) ;
#100033 = DIRECTION ( 'NONE',  ( 1.000000000000000000, 0.000000000000000000, 0.000000000000000000 ) ) ;
#100035 = CARTESIAN_POINT ( 'NONE',  ( 102.1162378120948802, -37.84850780196365605, 183.3995072184255548 ) ) ;
#100034 = VECTOR ( 'NONE', #80309, 1000.000000000000000 ) ;
#100036 = EDGE_CURVE ( 'NONE', #81483, #43496, #47520, .T. ) ;
#100037 = CARTESIAN_POINT ( 'NONE',  ( -37.24632233508901891, 27.99432795351219738, -10.98715164801380517 ) ) ;
#100038 = COLOUR_RGB ( '', 0.66274510, 0.83137255, 0.94901961) ;
#100039 = LINE ( 'NONE', #59065, #3351 ) ;
#100040 = CARTESIAN_POINT ( 'NONE',  ( 5.656854249492380582, -21.50000000409676915, -5.656854249492379694 ) ) ;
#100041 = CARTESIAN_POINT ( 'NONE',  ( -4.250000000000000000, 5.204748896376250699E-16, -10.00000000000000000 ) ) ;
#100042 = DIRECTION ( 'NONE',  ( -1.000000000000000000, -1.224606353822377258E-16, -0.000000000000000000 ) ) ;
#100043 =( LENGTH_UNIT ( ) NAMED_UNIT ( * ) SI_UNIT ( .MILLI., .METRE. ) );
#100044 = CARTESIAN_POINT ( 'NONE',  ( 0.000000000000000000, 0.000000000000000000, 0.000000000000000000 ) ) ;
#100045 = CARTESIAN_POINT ( 'NONE',  ( 13.50000000000000178, 0.000000000000000000, 0.000000000000000000 ) ) ;
#100046 = DIRECTION ( 'NONE',  ( -7.054958294834448933E-16, 0.9730768813850334542, 0.2304807647374887136 ) ) ;
#100047 = CARTESIAN_POINT ( 'NONE',  ( -3.648665620917451502, 15.00000000000000178, -9.999999999999998224 ) ) ;
#100048 = ORIENTED_EDGE ( 'NONE', *, *, #84299, .T. ) ;
#100049 = CARTESIAN_POINT ( 'NONE',  ( 44.20232540310176006, 435.2535269811378384, 14.52161920496060077 ) ) ;
#100050 = CARTESIAN_POINT ( 'NONE',  ( 17.61650669486618881, 1.474610560812782335E-15, 0.000000000000000000 ) ) ;
#100051 = DIRECTION ( 'NONE',  ( -0.2276554125553486296, 0.04124382534092855407, 0.9728679047052077866 ) ) ;
#100052 = CARTESIAN_POINT ( 'NONE',  ( -87.82931391962068801, -30.00000000000000000, 186.3420930804710736 ) ) ;
#100053 = EDGE_CURVE ( 'NONE', #11237, #54191, #7234, .T. ) ;
#100054 = AXIS2_PLACEMENT_3D ( 'NONE', #67983, #42101, #1627 ) ;
#100055 = EDGE_LOOP ( 'NONE', ( #84370, #30268 ) ) ;
#100056 = CARTESIAN_POINT ( 'NONE',  ( 0.000000000000000000, 4.898587196589413815E-16, -4.000000000000000888 ) ) ;
#100057 = CARTESIAN_POINT ( 'NONE',  ( 70.41249110440050174, -57.68249115096489987, 157.3832962191312674 ) ) ;
#100058 = AXIS2_PLACEMENT_3D ( 'NONE', #50346, #74624, #26142 ) ;
#100060 = LINE ( 'NONE', #89851, #10380 ) ;
#100059 = SURFACE_SIDE_STYLE ('',( #83344 ) ) ;
#100061 = CARTESIAN_POINT ( 'NONE',  ( 59.52453317996337745, -37.26894803123993682, -34.27940060143461665 ) ) ;
#100062 = CONICAL_SURFACE ( 'NONE', #77671, 4.000000000000001776, 0.9599310885968774798 ) ;
#100063 = DIRECTION ( 'NONE',  ( 0.000000000000000000, -1.000000000000000000, 0.000000000000000000 ) ) ;
#100064 = CARTESIAN_POINT ( 'NONE',  ( -10.28624191511820207, -1.200000000000000030E-05, 14.15779740156163946 ) ) ;
#100065 = CARTESIAN_POINT ( 'NONE',  ( -36.68252776495059919, -60.00000000000001421, 48.02914264494187080 ) ) ;
#100066 = CARTESIAN_POINT ( 'NONE',  ( 37.05595180434897173, 463.3109355731702976, 20.11755950910298196 ) ) ;
#100067 = CARTESIAN_POINT ( 'NONE',  ( -86.42980866402069751, -20.84916326163546429, 182.4270226805664663 ) ) ;
#100068 = ORIENTED_EDGE ( 'NONE', *, *, #15002, .T. ) ;
#100069 = CARTESIAN_POINT ( 'NONE',  ( 30.92841573401205579, 13.86971257847474703, 40.99043602818870369 ) ) ;
#100070 = CARTESIAN_POINT ( 'NONE',  ( -9.282201836941181838, -46.43936834299204719, 31.63261336507683552 ) ) ;
#100071 = DIRECTION ( 'NONE',  ( 0.000000000000000000, 0.000000000000000000, 1.000000000000000000 ) ) ;
#100072 = DIRECTION ( 'NONE',  ( 0.000000000000000000, -1.000000000000000000, 0.000000000000000000 ) ) ;
#100074 = CARTESIAN_POINT ( 'NONE',  ( 2.367671974756863751, -69.88010167377507287, 13.19913436203879620 ) ) ;
#100073 = DIRECTION ( 'NONE',  ( -1.000000000000000000, 0.000000000000000000, 0.000000000000000000 ) ) ;
#100075 = ORIENTED_EDGE ( 'NONE', *, *, #39111, .T. ) ;
#100076 = AXIS2_PLACEMENT_3D ( 'NONE', #51160, #26946, #20472 ) ;
#100077 = FILL_AREA_STYLE_COLOUR ( '', #50702 ) ;
#100078 = CARTESIAN_POINT ( 'NONE',  ( 0.6452404136000341461, 27.35540082825626484, 40.58352349220777455 ) ) ;
#100079 = CARTESIAN_POINT ( 'NONE',  ( -30.36467006388648926, 11.77175644674776223, -39.80053734054845904 ) ) ;
#100080 = CARTESIAN_POINT ( 'NONE',  ( 28.49755062498792668, 296.9296401919173150, -1.547493658460767696 ) ) ;
#100081 = FACE_OUTER_BOUND ( 'NONE', #24628, .T. ) ;
#100082 = DIRECTION ( 'NONE',  ( -1.000000000000000000, -1.224606353822377258E-16, -0.000000000000000000 ) ) ;
#100083 = CARTESIAN_POINT ( 'NONE',  ( 113.0845476695725864, -59.99999999999993605, 149.3435440849930842 ) ) ;
#100084 = CARTESIAN_POINT ( 'NONE',  ( -80.22109857244845443, -42.96982832339585201, 151.2315873428279076 ) ) ;
#100085 = ORIENTED_EDGE ( 'NONE', *, *, #46330, .T. ) ;
#100086 = CARTESIAN_POINT ( 'NONE',  ( 8.559508646656103892, 51.55638410492932167, -4.031152949375861105 ) ) ;
#100087 = CARTESIAN_POINT ( 'NONE',  ( 22.61650669486618526, -3.999999999999998224, 0.000000000000000000 ) ) ;
#100088 = PRESENTATION_STYLE_ASSIGNMENT (( #291 ) ) ;
#100089 = CARTESIAN_POINT ( 'NONE',  ( -7.022229286278467875, -4.221542269106504541, -17.11103215587112913 ) ) ;
#100090 = CARTESIAN_POINT ( 'NONE',  ( 45.40857607514351457, 438.4254919824014678, 6.241822647824930570 ) ) ;
#100091 = CARTESIAN_POINT ( 'NONE',  ( 44.83349330513380693, 4.000000000000002665, 0.000000000000000000 ) ) ;
#100092 = EDGE_LOOP ( 'NONE', ( #32461, #8400, #5439, #59922 ) ) ;
#100093 = UNCERTAINTY_MEASURE_WITH_UNIT (LENGTH_MEASURE( 1.000000000000000082E-05 ), #39456, 'distance_accuracy_value', 'NONE');
#100094 = CIRCLE ( 'NONE', #53604, 4.000000000000007105 ) ;
#100095 = AXIS2_PLACEMENT_3D ( 'NONE', #64356, #81034, #7150 ) ;
#100096 = CARTESIAN_POINT ( 'NONE',  ( -21.45209470218146564, 305.1036098005744748, 8.990911056619731667 ) ) ;
#100097 = ORIENTED_EDGE ( 'NONE', *, *, #60812, .T. ) ;
#100098 = CARTESIAN_POINT ( 'NONE',  ( 32.84237740334622657, 485.2251842821286800, 5.746442123025142124 ) ) ;
#100099 = CONICAL_SURFACE ( 'NONE', #7085, 4.172000000000009479, 0.9599310885968813656 ) ;
#100100 = CARTESIAN_POINT ( 'NONE',  ( 1.224646799147354440E-15, 15.00000000000000000, 9.999999999999998224 ) ) ;
#100101 = CARTESIAN_POINT ( 'NONE',  ( 32.78741055188848463, 485.3331003366708956, 5.977022408746977433 ) ) ;
#100102 = EDGE_CURVE ( 'NONE', #74232, #46481, #90571, .T. ) ;
#100103 = CARTESIAN_POINT ( 'NONE',  ( 16.84999999999999787, -3.309499999999999886, 4.475777889183790779E-16 ) ) ;
#100104 = CARTESIAN_POINT ( 'NONE',  ( 5.000000000000000000, -14.65803281199247898, 12.34559804589062537 ) ) ;
#100105 = ADVANCED_FACE ( 'NONE', ( #46643, #64952 ), #31555, .T. ) ;
#100106 = DIRECTION ( 'NONE',  ( 1.000000000000000000, 0.000000000000000000, -1.224646799147353207E-16 ) ) ;
#100107 = ORIENTED_EDGE ( 'NONE', *, *, #85360, .T. ) ;
#100108 = CARTESIAN_POINT ( 'NONE',  ( 93.04510679386291372, -60.00000000000001421, 32.83262320753426877 ) ) ;
#100109 = VECTOR ( 'NONE', #26917, 1000.000000000000000 ) ;
#100111 = CARTESIAN_POINT ( 'NONE',  ( 24.01072772857711968, -49.91340150330263725, 33.32366789474293967 ) ) ;
#100110 = CARTESIAN_POINT ( 'NONE',  ( -89.23267494088513274, -59.99999999999987921, 204.3671292578742680 ) ) ;
#100112 = CARTESIAN_POINT ( 'NONE',  ( 13.99999999999998046, 61.49999999999999289, 6.999999999999994671 ) ) ;
#100113 = CYLINDRICAL_SURFACE ( 'NONE', #94800, 4.000000000000000888 ) ;
#100114 = ADVANCED_FACE ( 'NONE', ( #97310 ), #15868, .F. ) ;
#100115 = CARTESIAN_POINT ( 'NONE',  ( -39.65982915714113233, -49.89218387423591139, 40.68439334530297202 ) ) ;
#100116 = CARTESIAN_POINT ( 'NONE',  ( -8.880059686752383996, 53.58371679781946995, -4.000342112176812570 ) ) ;
#100117 = UNCERTAINTY_MEASURE_WITH_UNIT (LENGTH_MEASURE( 1.000000000000000082E-05 ), #49829, 'distance_accuracy_value', 'NONE');
#100118 = ORIENTED_EDGE ( 'NONE', *, *, #94998, .T. ) ;
#100119 = CARTESIAN_POINT ( 'NONE',  ( -10.28624191511830155, -1.200000000000000030E-05, -14.15779740156157018 ) ) ;
#100120 = DIRECTION ( 'NONE',  ( 0.000000000000000000, 0.000000000000000000, -1.000000000000000000 ) ) ;
#100121 = CARTESIAN_POINT ( 'NONE',  ( 40.61216075948964033, 351.1469683695276558, 22.89433108575548914 ) ) ;
#100122 = DIRECTION ( 'NONE',  ( -1.000000000000000000, 0.000000000000000000, 0.000000000000000000 ) ) ;
#100123 = DIRECTION ( 'NONE',  ( -1.000000000000000000, -0.000000000000000000, -0.000000000000000000 ) ) ;
#100124 = CARTESIAN_POINT ( 'NONE',  ( -30.00000000000000355, 490.2049413377403084, 6.956578743376784502 ) ) ;
#100125 = ORIENTED_EDGE ( 'NONE', *, *, #71081, .T. ) ;
#100126 = CARTESIAN_POINT ( 'NONE',  ( -44.47534256803313468, -38.31161230092084224, 57.00189278798902137 ) ) ;
#100127 = ORIENTED_EDGE ( 'NONE', *, *, #91496, .F. ) ;
#100128 = CARTESIAN_POINT ( 'NONE',  ( 81.40593295988355749, -29.99999999999995026, -2.043119297071557039 ) ) ;
#100129 = CARTESIAN_POINT ( 'NONE',  ( 19.41543580316799122, 41.87297093669189252, -80.50253431361618084 ) ) ;
#100131 = ADVANCED_FACE ( 'NONE', ( #82729 ), #75157, .T. ) ;
#100130 = CARTESIAN_POINT ( 'NONE',  ( 23.86066917533285192, 25.16615122465923093, -33.04118181549677757 ) ) ;
#100132 = CARTESIAN_POINT ( 'NONE',  ( 14.27307692307692299, 1.411358822780289120E-15, 0.000000000000000000 ) ) ;
#100133 = CARTESIAN_POINT ( 'NONE',  ( 86.61543636280471503, -29.99999999999999645, 68.10094066095521725 ) ) ;
#100134 = CARTESIAN_POINT ( 'NONE',  ( -27.94791896389481778, 311.8549610008433319, 11.86231666168937693 ) ) ;
#100135 = ORIENTED_EDGE ( 'NONE', *, *, #67655, .F. ) ;
#100136 = B_SPLINE_CURVE_WITH_KNOTS ( 'NONE', 3,
 ( #29683, #11858, #62555, #46364, #53400, #45314, #87363, #46878, #4309, #79253, #21071, #94400, #103014, #28625, #86321, #71159, #37245, #5379, #28095, #95981, #78709, #95441, #29170, #22108, #12913, #45837, #4845, #77679, #54420, #37778, #62045, #38298, #30194, #104054 ),
 .UNSPECIFIED., .F., .F.,
 ( 4, 2, 2, 2, 2, 2, 2, 2, 2, 2, 2, 2, 2, 2, 2, 2, 4 ),
 ( 0.01263889472610566986, 0.01342810546992894566, 0.01421731621375222319, 0.01500652695757550073, 0.01579573770139877653, 0.01658494844522205233, 0.01737415918904532813, 0.01816336993286860740, 0.01895258067669188320, 0.01974179142051515901, 0.02053100216433843828, 0.02132021290816171408, 0.02210942365198498988, 0.02289863439580826568, 0.02368784513963154148, 0.02447705588345482075, 0.02526626662727809655 ),
 .UNSPECIFIED. ) ;
#100137 = AXIS2_PLACEMENT_3D ( 'NONE', #20830, #4058, #22395 ) ;
#100138 = EDGE_LOOP ( 'NONE', ( #69882, #62767, #63543, #1360 ) ) ;
#100139 = ORIENTED_EDGE ( 'NONE', *, *, #89195, .T. ) ;
#100140 = CARTESIAN_POINT ( 'NONE',  ( -4.000000000000000000, 0.000000000000000000, -2.296599999999999753 ) ) ;
#100141 = DIRECTION ( 'NONE',  ( -0.000000000000000000, -0.000000000000000000, -1.000000000000000000 ) ) ;
#100142 = CARTESIAN_POINT ( 'NONE',  ( -36.31983699975081237, 26.03207335590308347, -12.39576754523718272 ) ) ;
#100143 = AXIS2_PLACEMENT_3D ( 'NONE', #29205, #97574, #16679 ) ;
#100144 = CARTESIAN_POINT ( 'NONE',  ( 5.092539576892244568, -12.44323467208434053, 3.177249149099051984 ) ) ;
#100145 = CARTESIAN_POINT ( 'NONE',  ( 6.333820801331317973, 4.275724398227923828, -5.594228103109662342 ) ) ;
#100146 = CARTESIAN_POINT ( 'NONE',  ( 8.866506694866188809, -3.999999999999998224, 0.000000000000000000 ) ) ;
#100147 = ORIENTED_EDGE ( 'NONE', *, *, #71528, .F. ) ;
#100148 = CARTESIAN_POINT ( 'NONE',  ( -5.036189802311375807, 50.00000000000001421, -93.73786388411662074 ) ) ;
#100149 = AXIS2_PLACEMENT_3D ( 'NONE', #8523, #58139, #41426 ) ;
#100150 = ORIENTED_EDGE ( 'NONE', *, *, #66454, .F. ) ;
#100151 = FACE_OUTER_BOUND ( 'NONE', #47415, .T. ) ;
#100152 = CARTESIAN_POINT ( 'NONE',  ( 62.23204737827733624, -38.34071032238272636, 103.6626538615274313 ) ) ;
#100153 = CARTESIAN_POINT ( 'NONE',  ( 3.400000000000000355, 0.000000000000000000, -8.000000000000000000 ) ) ;
#100154 = B_SPLINE_CURVE_WITH_KNOTS ( 'NONE', 3,
 ( #55278, #22439, #47193, #30521, #14289, #23491, #97336, #57402, #89794, #32100, #48776, #73585, #16425, #6198, #96830, #15363, #56335, #89267, #81668, #104369, #5683, #104926, #14824, #90317, #6741, #24556, #39136, #32646, #72536, #63419, #48249, #63943, #72014, #64981, #31066, #22960, #81150, #7790, #96311, #65517, #55796, #105444, #88733, #7261, #40172, #73046, #79570, #105956, #97875, #24030, #56871, #99998, #35303, #50902, #101064, #41763, #33698, #75179, #100528, #18043, #60111, #9376, #1819, #91912, #67649, #26689, #18585, #25630, #68170, #66572, #34775, #42290, #84361, #10452, #8329, #83285, #59025, #82756, #59563, #41233, #92429, #49306, #51447, #58492, #43367, #76254, #57936, #83811, #16974, #42830, #74119, #67113, #75726, #2360, #33169, #8857, #49851, #27224, #9922, #26166, #92975, #74648, #206, #82215, #99456, #17511, #66041, #732, #1278, #98918, #90858, #25078, #91396, #50373, #34243, #86514, #20202, #13102, #28281, #27762, #102125, #53058, #70306, #94598, #78383, #19670, #62238, #43891, #29348, #103722, #19137, #60636, #2887, #20745, #36904, #68725, #37970, #69774, #44979, #37437, #95121, #84888, #51972, #10976, #12049, #102666, #3443, #54090, #69252, #21253, #46030, #87032, #78912, #61155, #101607, #93523, #77330, #5038, #45511, #70832, #94041, #29869, #36386, #12574, #4500, #62747, #28826, #77860, #11507, #76783, #85423, #35846, #85978, #52507, #53584, #44435, #103202, #3974, #61705, #40579, #7660, #64342, #106357, #79966, #105318, #15238, #104245, #40051, #87554, #89138, #80491, #31460, #63813, #81535, #14692, #48125, #22308, #72415, #6611, #30934, #96178, #56199, #55154, #88083, #47596, #96700, #81023, #22837, #97212, #71880, #13636, #105836, #104784, #38481, #46551, #7140, #14161, #79443, #73460, #6082, #55669, #71347, #30392, #63279, #5554, #47064, #39538, #23362, #32519, #31979, #72926, #64855, #56744, #95641, #39002, #88606, #97735, #23904, #89672, #15769, #54612, #48651, #21777, #606, #43243, #99326, #84233, #82, #92305, #66448, #57273, #50262, #49728, #41116, #50771, #73998, #33051, #83165, #34656, #49185, #18457, #99876, #58358, #16296, #66995, #65919, #9259, #67525, #75602, #26048, #16847, #100406, #42168, #51311, #58907, #10328, #57809, #82635, #91277, #9790, #34122, #91798, #25500, #17918, #1149, #83683, #42705, #26568, #41646, #76128, #8737, #1701, #17388, #65393, #59440, #2225, #98284, #24441, #75052, #90195, #98797, #24954, #90732, #82088, #8206, #74529, #33570, #78257, #103077, #43764, #44850, #2770, #28688, #27096, #52924, #61570, #70172, #19007, #101480, #35719, #94999, #77202, #84763, #76656, #93397, #29231, #94464, #4370, #11381, #100938, #68596, #69646, #28157, #92844, #36782, #27631, #20077, #37308, #45376, #102539, #19544, #60512, #20621, #62107, #86382, #12449, #53963, #86901, #12974, #52380, #59983, #53462, #102000, #21135, #77741, #45900, #78777, #35174, #44306, #68041, #85291, #51851, #61033, #10846, #3312, #36257, #69126, #93919, #85849, #11923, #3852, #87432, #13507, #37841, #4911, #56070, #14036, #47993, #72801, #46429, #14559, #96575, #46942, #97605, #6478, #64218, #70704, #79314, #5437, #104651, #5947, #47469, #22174, #55023, #29746, #87954, #72285, #38359, #71221, #63689, #79842, #38873, #39409, #71740, #62619, #15106, #30803, #54485, #95505, #105189, #104114, #21648, #56619, #96046, #22710, #89011, #80364, #97088, #30259, #80901, #63148, #55548, #89541, #7010, #23231, #39929, #105707, #48527, #88485, #31335, #31849, #64731, #23772, #15634, #103595, #7529, #40447, #16707, #74396, #73873, #33989, #57150, #25917, #57674, #73327, #8607, #42040, #50636, #81418, #49054, #90064, #17258, #66317, #16168, #106226, #99199, #475, #66859, #58773, #33444, #32388, #98149, #25363, #58223, #90597, #17786, #49597, #91670, #9655, #83554, #65259, #41509, #40984, #106768, #82505, #24301, #81950, #8075, #91149, #98669, #50128, #32914, #65792, #24822, #83038, #9129, #74922, #1005, #99748, #30071, #31143, #71550, #72621, #32182, #15444, #48335, #89876, #15983, #48860, #63493, #95850, #55364, #80703, #97413, #79652, #81230, #62954, #64547, #55877, #6820, #39218, #56955, #96909, #23573, #104455, #30603, #5763, #96391, #81753, #105001, #103924, #21980, #7347, #73131, #72093, #7875, #40256, #54835, #56420, #65064, #88293, #88812, #6279, #71033, #105523, #89353, #87763, #46758, #38685, #64031, #23040, #47798, #14906, #39740, #22521, #13845, #106035, #14368, #31663, #97961, #47277, #24111, #80175, #5369, #9160, #17291, #91702, #58256, #33474, #2126, #1047, #50165, #17817, #67430, #76030, #91183, #83067, #42071, #66346, #74956, #99231, #67950, #2666, #25949, #100307, #50670, #101381, #10231, #100831, #74430, #34021, #66893, #68493, #84133, #92204, #26467, #83583, #99780, #506, #26997, #58809, #9692, #35617, #42602, #59338, #18358, #75497, #1594, #25399, #34557, #59876, #51211, #35080, #43147, #92749, #60415, #18907, #51752, #84666, #10752, #43667, #76556, #27536, #93292, #19449, #52283, #8640, #41542, #69030, #88261, #104425, #19976, #102442, #22494, #71523, #30571, #23010, #44213, #11280, #77100, #79619, #63467, #69552, #14877, #28586, #55845, #6792, #88785, #47767, #20525, #28062, #72064, #60934, #52822, #96362, #80671, #101902, #39712, #61471, #47246, #80149, #96876, #55332, #5732, #77639, #36158, #44753, #3217, #46727, #85749, #14339, #6249, #31628, #3757, #94363, #38657, #31114, #39184, #97384, #53361, #104973, #64002, #93824, #72586, #11820, #105493, #64515, #23544, #86282, #85195, #36689, #13815, #91448, #17563, #15414, #90369, #66091, #89845, #41813, #48301, #66626, #58548, #57450, #1330, #781, #32152, #89318, #56385, #33754, #65564, #99510, #65029, #98969, #24077, #49902, #81198, #74174, #82810, #50425, #40223, #15950, #56920 ),
 .UNSPECIFIED., .F., .F.,
 ( 4, 1, 1, 1, 1, 1, 1, 2, 2, 1, 1, 2, 2, 1, 1, 1, 1, 1, 1, 1, 2, 2, 1, 1, 1, 1, 1, 1, 1, 1, 2, 2, 1, 1, 1, 1, 1, 1, 1, 1, 1, 2, 2, 1, 1, 1, 1, 1, 1, 1, 1, 1, 2, 2, 1, 1, 1, 1, 1, 1, 1, 2, 2, 1, 1, 1, 1, 2, 2, 1, 1, 1, 1, 1, 2, 2, 1, 1, 1, 1, 1, 1, 2, 2, 1, 1, 1, 1, 1, 1, 2, 2, 1, 1, 1, 1, 1, 2, 2, 1, 1, 1, 1, 1, 1, 2, 2, 1, 1, 1, 1, 1, 2, 2, 1, 1, 1, 1, 1, 2, 2, 1, 1, 1, 1, 1, 1, 2, 2, 1, 1, 1, 1, 1, 2, 2, 1, 1, 1, 1, 1, 1, 1, 2, 2, 1, 1, 1, 1, 1, 1, 1, 1, 2, 2, 1, 1, 1, 1, 1, 1, 2, 2, 1, 1, 1, 1, 1, 1, 1, 2, 2, 1, 1, 1, 1, 1, 1, 1, 1, 1, 2, 2, 1, 1, 1, 1, 1, 1, 1, 1, 1, 1, 2, 2, 1, 1, 1, 1, 2, 2, 1, 1, 1, 1, 1, 1, 1, 1, 1, 2, 2, 1, 1, 1, 1, 1, 1, 1, 1, 1, 2, 2, 1, 1, 1, 1, 1, 1, 1, 1, 2, 2, 1, 1, 1, 1, 1, 1, 1, 2, 2, 1, 1, 1, 1, 1, 1, 1, 2, 2, 1, 1, 1, 1, 1, 1, 1, 1, 1, 2, 2, 1, 1, 1, 1, 1, 1, 1, 2, 2, 1, 1, 1, 1, 1, 1, 1, 1, 2, 2, 1, 1, 1, 1, 1, 1, 1, 1, 2, 2, 1, 1, 1, 1, 1, 2, 2, 1, 1, 1, 1, 2, 2, 1, 1, 1, 1, 1, 2, 2, 1, 1, 1, 1, 1, 2, 2, 1, 1, 2, 2, 1, 2, 2, 1, 1, 1, 1, 2, 2, 1, 1, 1, 1, 2, 2, 1, 1, 1, 1, 2, 2, 1, 1, 1, 1, 1, 1, 2, 2, 1, 1, 1, 1, 1, 1, 2, 2, 1, 1, 1, 1, 1, 1, 1, 2, 2, 1, 1, 1, 1, 1, 1, 1, 2, 2, 1, 1, 1, 1, 1, 1, 1, 1, 2, 2, 1, 1, 1, 1, 2, 2, 1, 1, 1, 1, 1, 1, 1, 1, 2, 2, 1, 1, 1, 1, 1, 1, 2, 2, 1, 1, 1, 1, 1, 1, 2, 2, 1, 1, 1, 1, 1, 2, 2, 1, 1, 1, 1, 1, 1, 2, 2, 1, 1, 1, 1, 1, 1, 2, 2, 1, 1, 1, 1, 2, 2, 1, 1, 1, 1, 1, 1, 1, 2, 2, 1, 1, 1, 1, 1, 1, 1, 2, 2, 1, 1, 1, 1, 1, 1, 1, 2, 2, 1, 1, 1, 1, 1, 1, 1, 2, 2, 1, 1, 1, 1, 1, 1, 2, 2, 1, 1, 1, 1, 1, 1, 2, 2, 1, 1, 1, 1, 1, 2, 2, 1, 1, 1, 1, 2, 2, 1, 1, 1, 1, 2, 2, 1, 1, 1, 1, 1, 2, 2, 1, 1, 1, 1, 1, 1, 2, 2, 1, 1, 1, 1, 1, 1, 2, 2, 1, 1, 1, 1, 1, 1, 1, 2, 2, 1, 1, 1, 1, 1, 1, 1, 2, 2, 1, 1, 1, 1, 1, 1, 1, 2, 2, 4 ),
 ( 0.000000000000000000, 0.007812499999935031136, 0.01171874999990254497, 0.01367187499988630275, 0.01464843749987818251, 0.01513671874987412153, 0.01538085937487209190, 0.01550292968737107362, 0.01562499999987005533, 0.02343749999980482279, 0.02734374999977220652, 0.02929687499975590359, 0.03124999999973960760, 0.04687499999960928476, 0.05468749999954413549, 0.05859374999951156432, 0.06054687499949527874, 0.06152343749948713247, 0.06201171874948303853, 0.06225585937448099155, 0.06237792968697994378, 0.06249999999947890295, 0.07812499999934767458, 0.08593749999928204653, 0.08984374999924922556, 0.09179687499923282201, 0.09277343749922460636, 0.09326171874922049854, 0.09350585937421843075, 0.09362792968671740379, 0.09368896484296690419, 0.09374999999921639071, 0.1093749999990826505, 0.1171874999990158012, 0.1210937499989824112, 0.1230468749989657024, 0.1240234374989573618, 0.1245117187489531985, 0.1247558593739510890, 0.1248779296864500898, 0.1249389648426995902, 0.1249694824208242849, 0.1249999999989489935, 0.1406249999988075927, 0.1484374999987368993, 0.1523437499987015387, 0.1542968749986838584, 0.1552734374986749766, 0.1557617187486705079, 0.1560058593736682875, 0.1561279296861672328, 0.1561889648424166777, 0.1562194824205414556, 0.1562499999986662336, 0.1640624999986147747, 0.1679687499985890731, 0.1699218749985761945, 0.1708984374985696997, 0.1713867187485664523, 0.1716308593735648147, 0.1717529296860639820, 0.1718139648423135935, 0.1718749999985632049, 0.1757812499985364207, 0.1777343749985230148, 0.1787109374985162979, 0.1791992187485129118, 0.1794433593735112187, 0.1796874999985095256, 0.1835937499984822696, 0.1855468749984686416, 0.1865234374984618415, 0.1870117187484584276, 0.1872558593734567345, 0.1873779296859559018, 0.1874999999984550414, 0.1914062499984279242, 0.1933593749984143517, 0.1943359374984076071, 0.1948242187484042209, 0.1950683593734025001, 0.1951904296859016674, 0.1952514648421512511, 0.1953124999984008070, 0.1992187499983747445, 0.2011718749983617271, 0.2021484374983552046, 0.2026367187483519572, 0.2028808593733503196, 0.2030029296858494869, 0.2030639648420990984, 0.2031249999983486820, 0.2050781249983356369, 0.2060546874983291421, 0.2065429687483258669, 0.2067871093733242571, 0.2069091796858234522, 0.2069702148420730359, 0.2070312499983226473, 0.2089843749983096299, 0.2099609374983031074, 0.2104492187482998600, 0.2106933593732982501, 0.2108154296857974175, 0.2108764648420470289, 0.2109069824201718346, 0.2109374999982966403, 0.2128906249982839838, 0.2138671874982776555, 0.2143554687482744914, 0.2145996093732729093, 0.2147216796857721044, 0.2147827148420217158, 0.2148437499982712995, 0.2167968749982587262, 0.2177734374982524534, 0.2182617187482492893, 0.2185058593732477072, 0.2186279296857469301, 0.2186889648419965138, 0.2187499999982461252, 0.2226562499982208121, 0.2246093749982081278, 0.2255859374982018273, 0.2260742187481986631, 0.2263183593731970533, 0.2264404296856962762, 0.2265014648419458876, 0.2265624999981954713, 0.2304687499981701582, 0.2324218749981575016, 0.2333984374981511456, 0.2338867187481479815, 0.2341308593731463994, 0.2342529296856455945, 0.2343749999981447896, 0.2421874999980942467, 0.2460937499980689613, 0.2480468749980563326, 0.2490234374980500320, 0.2495117187480468679, 0.2497558593730452858, 0.2498779296855445087, 0.2499389648417940923, 0.2499999999980437315, 0.2656249999979469201, 0.2734374999978985699, 0.2773437499978743670, 0.2792968749978622656, 0.2802734374978562149, 0.2807617187478532172, 0.2810058593728517184, 0.2811279296853509968, 0.2811889648416006082, 0.2812499999978501641, 0.2890624999978015919, 0.2929687499977773335, 0.2949218749977651766, 0.2958984374977591258, 0.2963867187477561282, 0.2966308593727545739, 0.2967529296852537968, 0.2968749999977530196, 0.3046874999977027820, 0.3085937499976776355, 0.3105468749976650900, 0.3115234374976587617, 0.3120117187476556531, 0.3122558593726540987, 0.3123779296851532661, 0.3124389648414028775, 0.3124999999976524889, 0.3281249999975477394, 0.3359374999974953924, 0.3398437499974692466, 0.3417968749974561460, 0.3427734374974495957, 0.3432617187474463205, 0.3435058593724447107, 0.3436279296849438780, 0.3436889648411934894, 0.3437194824193182674, 0.3437499999974430454, 0.3593749999973815390, 0.3671874999973507303, 0.3710937499973353537, 0.3730468749973276932, 0.3740234374973238074, 0.3745117187473219200, 0.3747558593723210318, 0.3748779296848205322, 0.3749389648410703102, 0.3749694824191952547, 0.3749847412082576437, 0.3749999999973200882, 0.3828124999973044340, 0.3867187499972965514, 0.3886718749972926656, 0.3896484374972907783, 0.3901367187472897791, 0.3906249999972888354, 0.3984374999972733478, 0.4023437499972656317, 0.4042968749972616904, 0.4052734374972596920, 0.4057617187472586373, 0.4060058593722580267, 0.4061279296847577491, 0.4061889648410076936, 0.4062194824191325826, 0.4062347412081950271, 0.4062499999972574161, 0.4218749999971741493, 0.4296874999971324605, 0.4335937499971116438, 0.4355468749971012632, 0.4365234374970959896, 0.4370117187470933806, 0.4372558593720921039, 0.4373779296845914377, 0.4374389648408411602, 0.4374694824189659936, 0.4374999999970907716, 0.4531249999970035636, 0.4609374999969600428, 0.4648437499969382825, 0.4667968749969272912, 0.4677734374969217956, 0.4682617187469190756, 0.4685058593719177433, 0.4686279296844170217, 0.4686889648406666886, 0.4687499999969163000, 0.4765624999968729458, 0.4804687499968512410, 0.4824218749968403608, 0.4833984374968350317, 0.4838867187468323117, 0.4841308593718309794, 0.4842529296843304243, 0.4843139648405801467, 0.4843749999968298692, 0.4921874999968056663, 0.4960937499967935094, 0.4980468749967875697, 0.4990234374967845166, 0.4995117187467830178, 0.4997558593717822961, 0.4998779296842817965, 0.4999389648405315745, 0.4999999999967813524, 0.5156249999967325026, 0.5234374999967079667, 0.5273437499966957542, 0.5292968749966897590, 0.5302734374966865394, 0.5307617187466850961, 0.5310058593716844300, 0.5311279296841838748, 0.5311889648404337638, 0.5312194824185586528, 0.5312499999966834308, 0.5390624999966778796, 0.5429687499966751041, 0.5449218749966738828, 0.5458984374966732167, 0.5463867187466728836, 0.5466308593716726616, 0.5467529296841725506, 0.5468139648404225506, 0.5468749999966726616, 0.5546874999966865394, 0.5585937499966934228, 0.5605468749966969755, 0.5615234374966986408, 0.5620117187466993069, 0.5622558593716997510, 0.5623779296842000841, 0.5624389648404501951, 0.5624694824185751951, 0.5624999999967000841, 0.5703124999967056352, 0.5742187499967084108, 0.5761718749967096320, 0.5771484374967102982, 0.5776367187467107422, 0.5778808593717107422, 0.5780029296842108533, 0.5780639648404610753, 0.5780944824185860753, 0.5781249999967111863, 0.5820312499967029707, 0.5839843749966986408, 0.5849609374966965314, 0.5854492187466955322, 0.5856933593716948661, 0.5858154296841946440, 0.5859374999966944220, 0.5898437499966880937, 0.5917968749966850961, 0.5927734374966835418, 0.5932617187466827646, 0.5935058593716823205, 0.5937499999966818764, 0.5976562499966756592, 0.5996093749966725506, 0.6005859374966709963, 0.6010742187466702191, 0.6013183593716697750, 0.6014404296841695530, 0.6015624999966693309, 0.6054687499966613373, 0.6074218749966574515, 0.6083984374966554531, 0.6088867187466544539, 0.6091308593716540098, 0.6092529296841537878, 0.6093749999966534547, 0.6113281249966494579, 0.6123046874966474595, 0.6127929687466464603, 0.6132812499966455722, 0.6152343749966416864, 0.6162109374966397990, 0.6171874999966379116, 0.6210937499966301401, 0.6230468749966260322, 0.6240234374966240338, 0.6245117187466230346, 0.6247558593716224795, 0.6249999999966220354, 0.6289062499966131536, 0.6308593749966087127, 0.6318359374966064923, 0.6323242187466053821, 0.6325683593716049380, 0.6328124999966044939, 0.6367187499965958342, 0.6386718749965916153, 0.6396484374965893949, 0.6401367187465882846, 0.6403808593715877295, 0.6406249999965871744, 0.6445312499965771824, 0.6464843749965721864, 0.6474609374965697439, 0.6479492187465684117, 0.6481933593715677455, 0.6483154296840674125, 0.6483764648403171904, 0.6484374999965669684, 0.6523437499965499820, 0.6542968749965414332, 0.6552734374965371034, 0.6557617187465351050, 0.6560058593715341058, 0.6561279296840334396, 0.6561889648402831066, 0.6562499999965326625, 0.6601562499965086817, 0.6621093749964966912, 0.6630859374964906960, 0.6635742187464878095, 0.6638183593714862551, 0.6639404296839854780, 0.6640014648402351449, 0.6640319824183599229, 0.6640624999964848119, 0.6679687499964853670, 0.6699218749964857000, 0.6708984374964859221, 0.6713867187464859221, 0.6716308593714860331, 0.6717529296839860331, 0.6718139648402359221, 0.6718444824183610331, 0.6718749999964861441, 0.6757812499964886976, 0.6777343749964900299, 0.6787109374964906960, 0.6791992187464910291, 0.6794433593714912512, 0.6795654296839913622, 0.6796264648402413622, 0.6796569824183664732, 0.6796722412074290842, 0.6796874999964916952, 0.6835937499964956920, 0.6855468749964976904, 0.6865234374964988007, 0.6870117187464992448, 0.6872558593714994668, 0.6874999999964995778, 0.6914062499965030195, 0.6933593749965047959, 0.6943359374965056841, 0.6948242187465063502, 0.6950683593715065722, 0.6951904296840065722, 0.6952514648402567943, 0.6952819824183820163, 0.6952972412074446273, 0.6953124999965073494, 0.6992187499965401010, 0.7011718749965563102, 0.7021484374965644149, 0.7026367187465686337, 0.7028808593715706321, 0.7030029296840717423, 0.7030639648403224085, 0.7031249999965729636, 0.7109374999966618924, 0.7148437499967063014, 0.7167968749967285058, 0.7177734374967396080, 0.7182617187467451592, 0.7185058593717480457, 0.7186279296842494890, 0.7187499999967509323, 0.7343749999969289011, 0.7421874999970180520, 0.7460937499970626829, 0.7480468749970848874, 0.7490234374970959896, 0.7495117187471016518, 0.7499999999971072029, 0.7656249999972888354, 0.7734374999973796516, 0.7773437499974250597, 0.7792968749974478193, 0.7802734374974590326, 0.7807617187474648057, 0.7810058593724676923, 0.7812499999974704679, 0.7968749999976542098, 0.8046874999977460252, 0.8085937499977918774, 0.8105468749978148590, 0.8115234374978262943, 0.8120117187478319565, 0.8122558593728348431, 0.8124999999978376186, 0.8281249999980183629, 0.8359374999981087351, 0.8398437499981539212, 0.8417968749981765697, 0.8427734374981878940, 0.8437499999981992183, 0.8515624999982897014, 0.8554687499983348875, 0.8574218749983575361, 0.8583984374983688603, 0.8588867187483744114, 0.8591308593733772980, 0.8592529296858787413, 0.8593139648421294075, 0.8593749999983800736, 0.8671874999984743315, 0.8710937499985214050, 0.8730468749985448307, 0.8740234374985565990, 0.8745117187485624832, 0.8747558593735652588, 0.8748779296860667021, 0.8749389648423174792, 0.8749999999985681454, 0.8828124999986611821, 0.8867187499987075894, 0.8886718749987307930, 0.8896484374987423394, 0.8901367187487481125, 0.8903808593737511101, 0.8905029296862526644, 0.8905639648425033306, 0.8906249999987541077, 0.8984374999988422594, 0.9023437499988864463, 0.9042968749989085397, 0.9052734374989195310, 0.9057617187489251931, 0.9060058593739279686, 0.9061279296864293009, 0.9061889648426800781, 0.9062499999989307442, 0.9101562499989760413, 0.9121093749989985788, 0.9130859374990099031, 0.9135742187490156763, 0.9138183593740184518, 0.9139404296865198951, 0.9140014648427706723, 0.9140624999990213384, 0.9179687499990665245, 0.9199218749990891730, 0.9208984374991004973, 0.9213867187491061594, 0.9216308593741090460, 0.9217529296866104893, 0.9218139648428611554, 0.9218749999991119326, 0.9257812499991567856, 0.9277343749991792121, 0.9287109374991904254, 0.9291992187491959765, 0.9294433593741987520, 0.9295654296867001953, 0.9296874999992016386, 0.9335937499992466027, 0.9355468749992691402, 0.9365234374992804645, 0.9370117187492860156, 0.9372558593742889022, 0.9374999999992916777, 0.9414062499993371969, 0.9433593749993599564, 0.9443359374993711697, 0.9448242187493769428, 0.9450683593743798294, 0.9453124999993826050, 0.9492187499994281241, 0.9511718749994507727, 0.9521484374994620969, 0.9526367187494678701, 0.9528808593744706457, 0.9530029296869720890, 0.9531249999994735322, 0.9570312499995189404, 0.9589843749995415889, 0.9599609374995529132, 0.9604492187495586863, 0.9606933593745614619, 0.9608154296870629052, 0.9608764648433136824, 0.9609374999995643485, 0.9648437499996087574, 0.9667968749996310729, 0.9677734374996421751, 0.9682617187496477262, 0.9685058593746505018, 0.9686279296871519451, 0.9686889648434026112, 0.9687499999996533884, 0.9726562499996975752, 0.9746093749997197797, 0.9755859374997308819, 0.9760742187497363220, 0.9763183593747390976, 0.9764404296872405409, 0.9765014648434912070, 0.9765319824216165401, 0.9765624999997418731, 0.9804687499997850608, 0.9824218749998067102, 0.9833984374998175904, 0.9838867187498229194, 0.9841308593748256950, 0.9842529296873270273, 0.9843139648435776934, 0.9843444824217030265, 0.9843749999998282485, 0.9882812499998713252, 0.9902343749998927525, 0.9912109374999035216, 0.9916992187499089617, 0.9919433593749116262, 0.9920654296874129585, 0.9921264648436637357, 0.9921569824217889577, 0.9921874999999142908, 1.000000000000000000 ),
 .UNSPECIFIED. ) ;
#100155 = CARTESIAN_POINT ( 'NONE',  ( 31.51275525728127747, 299.7698742078038094, 11.04316810569213381 ) ) ;
#100156 = CARTESIAN_POINT ( 'NONE',  ( -5.477432325710314132, 246.8352046442952030, 2.459915882346695337 ) ) ;
#100157 = EDGE_LOOP ( 'NONE', ( #28414, #26688, #104819, #62675, #25351 ) ) ;
#100158 = CARTESIAN_POINT ( 'NONE',  ( 17.73948671138767352, 45.30893932440047678, -6.031879864029628280 ) ) ;
#100159 = CARTESIAN_POINT ( 'NONE',  ( 38.64013033672255659, 312.1321624020491186, 6.078733131242813670 ) ) ;
#100160 = DIRECTION ( 'NONE',  ( 0.000000000000000000, 0.000000000000000000, -1.000000000000000000 ) ) ;
#100161 = EDGE_CURVE ( 'NONE', #31268, #38217, #26140, .T. ) ;
#100162 =( NAMED_UNIT ( * ) SI_UNIT ( $, .STERADIAN. ) SOLID_ANGLE_UNIT ( ) );
#100163 = ORIENTED_EDGE ( 'NONE', *, *, #13664, .F. ) ;
#100164 = CARTESIAN_POINT ( 'NONE',  ( -22.33970404802145637, 303.2844704797087161, 10.02998793445647685 ) ) ;
#100165 = DIRECTION ( 'NONE',  ( 0.000000000000000000, 1.000000000000000000, 0.000000000000000000 ) ) ;
#100166 = UNCERTAINTY_MEASURE_WITH_UNIT (LENGTH_MEASURE( 1.000000000000000082E-05 ), #51119, 'distance_accuracy_value', 'NONE');
#100167 = CARTESIAN_POINT ( 'NONE',  ( -3.999976370155091665, -10.00072555073141167, 6.928216872919098712 ) ) ;
#100168 = CARTESIAN_POINT ( 'NONE',  ( 0.9522842513689456778, 294.8487785400556618, 1.936375222902182225 ) ) ;
#100169 = EDGE_CURVE ( 'NONE', #3854, #50065, #34749, .T. ) ;
#100170 = EDGE_CURVE ( 'NONE', #16689, #63739, #75694, .T. ) ;
#100171 = CARTESIAN_POINT ( 'NONE',  ( 53.29999999999999716, -3.309500000000000774, 0.000000000000000000 ) ) ;
#100172 = CARTESIAN_POINT ( 'NONE',  ( 86.23189122538319396, -24.68366007135474760, 181.5277984381359886 ) ) ;
#100173 = CARTESIAN_POINT ( 'NONE',  ( 17.16184658094818261, 36.31812281971417633, -24.24086490087793067 ) ) ;
#100174 = CARTESIAN_POINT ( 'NONE',  ( -8.203754751761275443, 114.5734753959365975, 5.000000000000000000 ) ) ;
#100175 = ORIENTED_EDGE ( 'NONE', *, *, #20829, .T. ) ;
#100176 = CARTESIAN_POINT ( 'NONE',  ( 93.00281210641563234, -57.65601615028951699, -17.21362402452485441 ) ) ;
#100177 = VECTOR ( 'NONE', #76054, 1000.000000000000000 ) ;
#100178 = AXIS2_PLACEMENT_3D ( 'NONE', #23647, #88893, #22056 ) ;
#100179 = CARTESIAN_POINT ( 'NONE',  ( 0.000000000000000000, -30.00000000000000000, 0.000000000000000000 ) ) ;
#100180 = CARTESIAN_POINT ( 'NONE',  ( 7.500000000000000000, 4.330127018922189208, -7.422398894150033399 ) ) ;
#100181 = CARTESIAN_POINT ( 'NONE',  ( 18.86650669486618881, 1.474610560812782335E-15, 0.000000000000000000 ) ) ;
#100182 = AXIS2_PLACEMENT_3D ( 'NONE', #96989, #367, #105086 ) ;
#100183 = CARTESIAN_POINT ( 'NONE',  ( -93.99531654986856211, -30.00000000000000355, 111.9393279711768798 ) ) ;
#100184 = EDGE_CURVE ( 'NONE', #20613, #41052, #64777, .T. ) ;
#100185 = COLOUR_RGB ( '', 0.40784314, 0.44705882, 0.49803922) ;
#100186 = CARTESIAN_POINT ( 'NONE',  ( -7.150000000000001243, 41.64999999999999147, -68.91429205801802027 ) ) ;
#100187 = DIRECTION ( 'NONE',  ( 0.000000000000000000, 0.000000000000000000, 1.000000000000000000 ) ) ;
#100189 = DIRECTION ( 'NONE',  ( 0.000000000000000000, 0.000000000000000000, 1.000000000000000000 ) ) ;
#100188 = CARTESIAN_POINT ( 'NONE',  ( -9.380894568449098969, 247.9886936688905337, -3.467341429141166387 ) ) ;
#100190 = PRESENTATION_LAYER_ASSIGNMENT (  '', '', ( #39916 ) ) ;
#100191 = PRESENTATION_STYLE_ASSIGNMENT (( #67310 ) ) ;
#100192 = CARTESIAN_POINT ( 'NONE',  ( -31.81386177463738107, 439.0024176103436275, 23.54436022379337246 ) ) ;
#100193 = CARTESIAN_POINT ( 'NONE',  ( 38.41498555331551756, 491.4234641122537823, 12.30872953874833442 ) ) ;
#100194 = CARTESIAN_POINT ( 'NONE',  ( 5.190609988845227285, -82.36077713256410959, -3.016375611400009316 ) ) ;
#100195 = DIRECTION ( 'NONE',  ( 1.000000000000000000, 0.000000000000000000, 0.000000000000000000 ) ) ;
#100196 = CARTESIAN_POINT ( 'NONE',  ( 43.49712683598065865, 471.1121331949958631, 8.167988778889762713 ) ) ;
#100197 = EDGE_CURVE ( 'NONE', #36223, #90523, #32081, .T. ) ;
#100198 = CARTESIAN_POINT ( 'NONE',  ( 13.04985325050550315, -16.80601421349662417, -34.54123526020268997 ) ) ;
#100199 = CARTESIAN_POINT ( 'NONE',  ( -25.48234102807342083, -56.87598310890427200, 34.80864869422586594 ) ) ;
#100200 = ORIENTED_EDGE ( 'NONE', *, *, #78304, .F. ) ;
#100201 = LINE ( 'NONE', #74321, #82384 ) ;
#100202 = CARTESIAN_POINT ( 'NONE',  ( -6.928203230275510549, 85.00000000000000000, -4.000000000000000000 ) ) ;
#100203 = CARTESIAN_POINT ( 'NONE',  ( -50.03090904413763695, -27.50677130059942854, -27.97160039159090772 ) ) ;
#100205 = CARTESIAN_POINT ( 'NONE',  ( 56.48317336153285595, 6.856755485862130937E-15, 0.000000000000000000 ) ) ;
#100204 = CARTESIAN_POINT ( 'NONE',  ( 4.988960626530190971E-15, 27.29656849860388235, 40.75000000000000000 ) ) ;
#100206 = ORIENTED_EDGE ( 'NONE', *, *, #90249, .T. ) ;
#100207 =( GEOMETRIC_REPRESENTATION_CONTEXT ( 3 ) GLOBAL_UNCERTAINTY_ASSIGNED_CONTEXT ( ( #59355 ) ) GLOBAL_UNIT_ASSIGNED_CONTEXT ( ( #38317, #96003, #86339 ) ) REPRESENTATION_CONTEXT ( 'NONE', 'WORKASPACE' ) );
#100208 = DIRECTION ( 'NONE',  ( 0.000000000000000000, -1.000000000000000000, 0.000000000000000000 ) ) ;
#100209 = VERTEX_POINT ( 'NONE', #25601 ) ;
#100210 = CARTESIAN_POINT ( 'NONE',  ( 0.4037800551813718331, -4.058962678540100733, 5.969670414742688003 ) ) ;
#100211 = AXIS2_PLACEMENT_3D ( 'NONE', #10696, #35560, #42011 ) ;
#100212 = CARTESIAN_POINT ( 'NONE',  ( 15.46526232232250209, 2.714356162036268838, 1.556038473651678578 ) ) ;
#100213 = CARTESIAN_POINT ( 'NONE',  ( -82.58075912419870690, -59.99999999999999289, -26.31469373492660679 ) ) ;
#100214 = ORIENTED_EDGE ( 'NONE', *, *, #7144, .F. ) ;
#100215 = CARTESIAN_POINT ( 'NONE',  ( -9.496182690454562092, 294.6569812313908869, -3.146984053371444379 ) ) ;
#100216 = CARTESIAN_POINT ( 'NONE',  ( 101.5064089130223692, -60.23311196733765627, 194.7041288308016931 ) ) ;
#100218 = CARTESIAN_POINT ( 'NONE',  ( -3.508895115992890723, -1.149532983824396615, 104.5950737443410645 ) ) ;
#100217 = CARTESIAN_POINT ( 'NONE',  ( 9.403329628528986461, 294.6596496208666167, -3.414309514541682411 ) ) ;
#100219 = ORIENTED_EDGE ( 'NONE', *, *, #79075, .T. ) ;
#100220 = EDGE_LOOP ( 'NONE', ( #106597, #24547, #3049, #104970 ) ) ;
#100221 = EDGE_LOOP ( 'NONE', ( #27057, #87822, #63769, #23221, #92931, #58058, #22659, #65713 ) ) ;
#100222 = CARTESIAN_POINT ( 'NONE',  ( 31.93152273642204619, 357.0352949535724747, 21.73667947981457971 ) ) ;
#100223 = DIRECTION ( 'NONE',  ( -1.000000000000000000, -1.224606353822377258E-16, -0.000000000000000000 ) ) ;
#100224 = CARTESIAN_POINT ( 'NONE',  ( 9.773125458951499311, 53.39756354753611589, 3.092076115194700492 ) ) ;
#100225 = ORIENTED_EDGE ( 'NONE', *, *, #49768, .F. ) ;
#100226 = ADVANCED_FACE ( 'NONE', ( #17482 ), #94114, .T. ) ;
#100227 = CARTESIAN_POINT ( 'NONE',  ( -43.59756234217317683, 434.3244621007142996, 14.55946156040369921 ) ) ;
#100228 = FACE_OUTER_BOUND ( 'NONE', #105648, .T. ) ;
#100229 = CARTESIAN_POINT ( 'NONE',  ( 7.770228158362352033, -5.000000000000000000, 0.000000000000000000 ) ) ;
#100230 = CARTESIAN_POINT ( 'NONE',  ( -11.25203090971146302, -57.67122638729478723, 41.63652355756774881 ) ) ;
#100231 = CARTESIAN_POINT ( 'NONE',  ( -43.75010090113929806, 464.8337800386750018, 11.75004750934965791 ) ) ;
#100232 = FACE_OUTER_BOUND ( 'NONE', #60559, .T. ) ;
#100233 = CARTESIAN_POINT ( 'NONE',  ( -4.966176470918042263, 41.64999999999998437, -70.47555194646970733 ) ) ;
#100234 = CARTESIAN_POINT ( 'NONE',  ( -87.78075539319912934, -14.21045842199443499, -8.620330001511526063 ) ) ;
#100235 = EDGE_CURVE ( 'NONE', #14213, #21895, #14518, .T. ) ;
#100236 = DIRECTION ( 'NONE',  ( -1.000000000000000000, -1.224606353822377258E-16, -0.000000000000000000 ) ) ;
#100237 = EDGE_CURVE ( 'NONE', #10331, #1507, #100965, .T. ) ;
#100238 = CARTESIAN_POINT ( 'NONE',  ( -49.74225373137043960, -60.29818990586195326, 57.32659193509455520 ) ) ;
#100239 = CARTESIAN_POINT ( 'NONE',  ( -25.60851123651792705, 48.00000000000000000, -75.29411764705884025 ) ) ;
#100240 = ORIENTED_EDGE ( 'NONE', *, *, #95335, .F. ) ;
#100241 = CARTESIAN_POINT ( 'NONE',  ( 12.50000000000000000, -2.999999999999996891, -14.34180675897363955 ) ) ;
#100242 = CARTESIAN_POINT ( 'NONE',  ( -8.233767125222675176, 295.9462895465074439, -10.03054565981068258 ) ) ;
#100243 = EDGE_CURVE ( 'NONE', #31268, #66339, #87206, .T. ) ;
#100244 = CARTESIAN_POINT ( 'NONE',  ( 10.15437730543717976, -0.6969019443260592306, 20.10336840207808251 ) ) ;
#100245 = ORIENTED_EDGE ( 'NONE', *, *, #67133, .F. ) ;
#100246 = CARTESIAN_POINT ( 'NONE',  ( 5.981118819178460555, 246.0281654381993803, 0.5452870891823716759 ) ) ;
#100247 = CARTESIAN_POINT ( 'NONE',  ( 87.56679391027844872, -38.57208170489048626, 199.7935100241939210 ) ) ;
#100248 = DIRECTION ( 'NONE',  ( -1.000000000000000000, -1.224606353822377258E-16, -0.000000000000000000 ) ) ;
#100249 =( GEOMETRIC_REPRESENTATION_CONTEXT ( 3 ) GLOBAL_UNCERTAINTY_ASSIGNED_CONTEXT ( ( #93096 ) ) GLOBAL_UNIT_ASSIGNED_CONTEXT ( ( #4142, #94761, #68890 ) ) REPRESENTATION_CONTEXT ( 'NONE', 'WORKASPACE' ) );
#100251 = EDGE_CURVE ( 'NONE', #18508, #21120, #32617, .T. ) ;
#100250 = CARTESIAN_POINT ( 'NONE',  ( -16.35748688301842790, 302.5696007747827707, 9.877144026384431896 ) ) ;
#100252 = ADVANCED_FACE ( 'NONE', ( #52475 ), #75557, .T. ) ;
#100253 = CARTESIAN_POINT ( 'NONE',  ( -55.65414010186720617, 42.00000000000000000, -72.41885610115910765 ) ) ;
#100254 = CARTESIAN_POINT ( 'NONE',  ( 93.38388337575746334, -30.00000000000000711, 191.1906521887401311 ) ) ;
#100255 = AXIS2_PLACEMENT_3D ( 'NONE', #1731, #74033, #83712 ) ;
#100256 = CARTESIAN_POINT ( 'NONE',  ( -10.45150921522485632, 43.95515046479253130, -12.90779740156153821 ) ) ;
#100257 = CARTESIAN_POINT ( 'NONE',  ( 27.99999999999999645, 0.000000000000000000, 0.000000000000000000 ) ) ;
#100258 = DIRECTION ( 'NONE',  ( -0.000000000000000000, 0.8660254037844388186, 0.4999999999999996114 ) ) ;
#100259 = ORIENTED_EDGE ( 'NONE', *, *, #89921, .F. ) ;
#100260 = ORIENTED_EDGE ( 'NONE', *, *, #23770, .T. ) ;
#100261 = CARTESIAN_POINT ( 'NONE',  ( 53.27090504139580673, -42.96895588525129739, 58.02480099802018287 ) ) ;
#100262 = DIRECTION ( 'NONE',  ( -0.000000000000000000, -0.000000000000000000, -1.000000000000000000 ) ) ;
#100263 = VECTOR ( 'NONE', #64067, 1000.000000000000000 ) ;
#100264 = DIRECTION ( 'NONE',  ( -1.000000000000000000, -1.224606353822377258E-16, -0.000000000000000000 ) ) ;
#100265 = VECTOR ( 'NONE', #39714, 1000.000000000000114 ) ;
#100266 = VERTEX_POINT ( 'NONE', #20174 ) ;
#100267 = CARTESIAN_POINT ( 'NONE',  ( -91.44302139157441900, -38.39068403194840329, -8.132174192228589504 ) ) ;
#100268 = B_SPLINE_CURVE_WITH_KNOTS ( 'NONE', 3,
 ( #69051, #20006, #52848, #85772 ),
 .UNSPECIFIED., .F., .F.,
 ( 4, 4 ),
 ( 0.000000000000000000, 0.001312499955570751390 ),
 .UNSPECIFIED. ) ;
#100269 = ORIENTED_EDGE ( 'NONE', *, *, #17205, .F. ) ;
#100270 = CARTESIAN_POINT ( 'NONE',  ( 9.250997389131581983, 6.123233995736770227E-16, -5.000000000000002665 ) ) ;
#100271 = CARTESIAN_POINT ( 'NONE',  ( 110.3727171012441488, -38.35605046350913483, 158.9384829488004982 ) ) ;
#100272 = CARTESIAN_POINT ( 'NONE',  ( 15.39024840373160607, 22.75717525244400008, 2.263382330767907735 ) ) ;
#100273 = CARTESIAN_POINT ( 'NONE',  ( 86.56429641673445019, -52.71572802512593370, 37.65660418523465580 ) ) ;
#100274 = CARTESIAN_POINT ( 'NONE',  ( 1.630169624183145149, -5.000000000000000000, -16.56347947974793655 ) ) ;
#100275 = DIRECTION ( 'NONE',  ( 0.000000000000000000, 0.000000000000000000, 1.000000000000000000 ) ) ;
#100276 = DIRECTION ( 'NONE',  ( -1.000000000000000000, -0.000000000000000000, -0.000000000000000000 ) ) ;
#100277 = DIRECTION ( 'NONE',  ( 0.000000000000000000, -1.000000000000000000, 0.000000000000000000 ) ) ;
#100278 = FACE_OUTER_BOUND ( 'NONE', #79413, .T. ) ;
#100280 = ORIENTED_EDGE ( 'NONE', *, *, #58352, .T. ) ;
#100279 =( BOUNDED_SURFACE ( )  B_SPLINE_SURFACE ( 3, 2, ( 
 ( #78547, #4675, #86673 ),
 ( #37608, #70471, #62388 ),
 ( #18762, #52143, #43538 ),
 ( #2527, #85061, #11138 ) ),
 .UNSPECIFIED., .F., .F., .F. ) 
 B_SPLINE_SURFACE_WITH_KNOTS ( ( 4, 4 ),
 ( 3, 3 ),
 ( 1.416401718135062993E-15, 0.001833990318203171464 ),
 ( 0.000000000000000000, 1.000000000000000000 ),
 .UNSPECIFIED. ) 
 GEOMETRIC_REPRESENTATION_ITEM ( )  RATIONAL_B_SPLINE_SURFACE ( (
 ( 1.000000000000000000, 0.7977970988452940393, 1.000000000000000000),
 ( 1.000000000000000000, 0.7897979397240406652, 1.000000000000000000),
 ( 1.000000000000000000, 0.7817839364700247540, 1.000000000000000000),
 ( 1.000000000000000000, 0.7737149417968405274, 1.000000000000000000) ) ) 
 REPRESENTATION_ITEM ( '' )  SURFACE ( )  );
#100281 = CARTESIAN_POINT ( 'NONE',  ( 59.17824404644323266, -49.90990980372215091, 74.96678020754490035 ) ) ;
#100282 = CARTESIAN_POINT ( 'NONE',  ( 0.7770801399229583240, 37.10885713635266825, 27.51745571163628412 ) ) ;
#100283 = AXIS2_PLACEMENT_3D ( 'NONE', #59265, #92678, #35008 ) ;
#100284 = CARTESIAN_POINT ( 'NONE',  ( -33.51558356630641811, 484.9916844669999705, -0.2910019615253942593 ) ) ;
#100285 = CARTESIAN_POINT ( 'NONE',  ( -33.14118366335542021, 381.7159081765646533, 24.92900331645760303 ) ) ;
#100286 = CARTESIAN_POINT ( 'NONE',  ( -0.6250000000000013323, -8.299410119600887370, -7.298562697733112614 ) ) ;
#100287 = CARTESIAN_POINT ( 'NONE',  ( 0.000000000000000000, 2.000000000000000000, 63.00000000000000000 ) ) ;
#100288 = CARTESIAN_POINT ( 'NONE',  ( -3.313708498984760720, -27.03124999999998934, -8.000000000000000000 ) ) ;
#100289 = VECTOR ( 'NONE', #41636, 1000.000000000000000 ) ;
#100290 = EDGE_CURVE ( 'NONE', #34186, #91741, #28794, .T. ) ;
#100291 = DIRECTION ( 'NONE',  ( -1.000000000000000000, 0.000000000000000000, 0.000000000000000000 ) ) ;
#100292 = VECTOR ( 'NONE', #70964, 1000.000000000000227 ) ;
#100293 = ORIENTED_EDGE ( 'NONE', *, *, #71398, .F. ) ;
#100294 = CARTESIAN_POINT ( 'NONE',  ( 84.73811181637501022, -32.38007879023361824, 175.3238245508336206 ) ) ;
#100295 = SURFACE_STYLE_FILL_AREA ( #100819 ) ;
#100296 = CARTESIAN_POINT ( 'NONE',  ( -39.41119041386610888, 438.9267638094590893, 23.32421457530460529 ) ) ;
#100297 = ORIENTED_EDGE ( 'NONE', *, *, #77308, .F. ) ;
#100298 = CARTESIAN_POINT ( 'NONE',  ( -40.73953790046564194, -18.92596047533412573, -20.36976895023281031 ) ) ;
#100299 = CARTESIAN_POINT ( 'NONE',  ( 9.499937800617230366, -5.000000000000023093, -20.18737470931553091 ) ) ;
#100300 = CARTESIAN_POINT ( 'NONE',  ( 20.19615384615384457, 1.411358822780289120E-15, 0.000000000000000000 ) ) ;
#100301 =( LENGTH_UNIT ( ) NAMED_UNIT ( * ) SI_UNIT ( .MILLI., .METRE. ) );
#100302 = CARTESIAN_POINT ( 'NONE',  ( -13.85425718576935239, -3.000000000000002665, -90.90560122694158451 ) ) ;
#100303 = CARTESIAN_POINT ( 'NONE',  ( -20.17834448772858380, -25.90226919805355266, -38.48103527270688318 ) ) ;
#100304 = CARTESIAN_POINT ( 'NONE',  ( 48.02835407290544367, -1.200000000000000030E-05, 15.60535821593427563 ) ) ;
#100305 = EDGE_CURVE ( 'NONE', #160, #60249, #92338, .T. ) ;
#100306 = SHAPE_REPRESENTATION_RELATIONSHIP ( 'NONE' , 'NONE' ,  #44072, #4890 ) ;
#100307 = CARTESIAN_POINT ( 'NONE',  ( 50.76975585573665484, -60.00000000000000711, 73.74697247292149882 ) ) ;
#100308 = CARTESIAN_POINT ( 'NONE',  ( 8.000113193197767814, 109.0002263864586212, -0.2613481123984635612 ) ) ;
#100310 = CARTESIAN_POINT ( 'NONE',  ( -13.70309997686470282, 22.84598062213630598, -1.780770408353728795 ) ) ;
#100309 = CARTESIAN_POINT ( 'NONE',  ( -27.57469521172910376, -30.80484053261712774, 39.32463195004949341 ) ) ;
#100311 = LINE ( 'NONE', #59345, #3978 ) ;
#100312 = CARTESIAN_POINT ( 'NONE',  ( 23.43684916743750080, 295.2641918988800285, 10.02474406024658293 ) ) ;
#100313 =( NAMED_UNIT ( * ) SI_UNIT ( $, .STERADIAN. ) SOLID_ANGLE_UNIT ( ) );
#100314 = LINE ( 'NONE', #59349, #58662 ) ;
#100315 = ORIENTED_EDGE ( 'NONE', *, *, #34551, .T. ) ;
#100316 = ADVANCED_FACE ( 'NONE', ( #12018 ), #12541, .T. ) ;
#100317 = CARTESIAN_POINT ( 'NONE',  ( -11.93255308427328565, 294.5886021379643580, 9.881054392645332030 ) ) ;
#100318 = PRESENTATION_LAYER_ASSIGNMENT (  '', '', ( #98550 ) ) ;
#100319 = CARTESIAN_POINT ( 'NONE',  ( -17.49999999999793587, 49.88162284957622461, 62.03084827767296616 ) ) ;
#100320 = UNCERTAINTY_MEASURE_WITH_UNIT (LENGTH_MEASURE( 1.000000000000000082E-05 ), #34411, 'distance_accuracy_value', 'NONE');
#100321 = DIRECTION ( 'NONE',  ( 0.000000000000000000, -1.000000000000000000, 0.000000000000000000 ) ) ;
#100322 = CARTESIAN_POINT ( 'NONE',  ( -39.85421124144144045, 464.8562039746861387, 17.95120812561461321 ) ) ;
#100324 = CARTESIAN_POINT ( 'NONE',  ( 54.58014935078251284, -60.22827346522726799, -31.12123911173822677 ) ) ;
#100323 = CARTESIAN_POINT ( 'NONE',  ( 4.881448269507570714, 54.28580602658091436, 6.096853558198860767 ) ) ;
#100325 = ORIENTED_EDGE ( 'NONE', *, *, #53315, .T. ) ;
#100326 = B_SPLINE_CURVE_WITH_KNOTS ( 'NONE', 3,
 ( #53492, #29260, #11954, #52957, #69679, #5469, #95031, #61607, #62141, #70733, #102576, #21686, #37875, #103629, #62660, #71256, #45416, #78288, #60542, #52411, #11415, #36293, #4406, #44341, #3352, #83464, #5980, #106671, #82407, #58674, #9565, #50549, #58125, #74305, #65696, #73772, #41942, #49501, #91051, #42471, #22209, #90500, #55060, #32288, #17160, #65156, #98054, #48955, #24203, #75369, #8509, #99104, #9035, #106129, #82937, #57052, #99649, #81852, #30295, #380, #50031, #40886, #74828, #909, #98581, #33887, #89968, #25822, #91578, #17685, #41410, #66762, #25263, #63184, #24727, #57578, #32820, #46977, #16610, #16075, #7973, #96078, #87988, #33348, #14068, #66216, #79875, #38910, #71775, #18779, #93164, #2008, #51082, #27413, #18229, #60291, #68906, #84002, #101779, #85616, #59743, #59210, #36563, #12228, #34955, #43550, #19331, #34432, #53239, #52161, #94231, #67824, #85073, #61342, #102313, #69433, #11157, #27948, #51628, #28465, #44086, #10631, #10110, #3087, #101261, #76969, #20396, #43019, #92621, #100707, #2547, #45159, #86162, #44627, #60810, #76430, #1468, #36032, #93702, #35489, #75908, #26874, #100183, #84546, #67301, #19854, #68365, #92089, #52689, #11691, #77515, #3628, #26350, #78039, #79095, #70486, #53759, #80150, #86687, #64003, #47247, #95293, #12757, #63468, #79620, #96877, #95824, #13816, #88262, #14341, #54804, #71524, #4158, #96363, #37089, #21953, #21423, #45681, #69955, #102851, #46211, #78559, #72065, #4691, #55846, #37623, #30041, #104426, #29018, #22495, #61884, #87737, #54264, #103381, #94778, #20925, #5218, #62401, #29528, #104974, #87207, #13281, #30572, #14878, #55333, #38148, #6250, #71005, #31115, #23012, #88786, #46729, #39186, #38658, #103898, #62931, #5734, #15951, #64516, #56921, #32153, #254, #6793, #39713, #24078, #66627, #57452, #106007, #82270, #81720, #65030, #32698, #48302, #97385, #73639, #23545, #106543, #8382, #56386, #41285, #25135, #33221, #105494, #82811, #58550, #81199, #89846, #65565, #80672, #99511, #98453, #33755, #7311, #24603, #782, #41814, #8912, #90370, #74175, #97927, #74702, #15415, #48827, #89319, #49363, #40752, #16485, #25685, #40225, #7845, #73093, #66093, #91449, #47768, #90914, #98970, #57994, #72587, #17027, #49903, #31631, #27284, #42884, #9428, #34296, #52560, #60165, #84415, #1331, #35360, #93033, #68230, #76305, #2948, #17564, #18640, #9981, #100052, #19723, #26220, #3499, #44495, #34833, #59079, #35903, #19192, #36438, #101123, #52032, #27818, #60687, #84943, #43424, #69308, #85484, #26744, #75782, #68779, #83336, #92490, #1875, #11032, #101660, #67702, #100584, #93575, #102183, #59620, #11564, #2417, #51500, #10510, #91966, #43949, #77383, #76841, #28332, #42348, #61208, #50426, #75235, #67171, #18095, #50956, #83870, #13155, #102721, #79499, #62802, #62282, #5610, #55211, #38535, #38022, #86031, #95689, #87609, #70357, #54141, #22365, #103253, #5089, #29399, #61754, #96235, #36955, #47122, #71941, #70881, #21304, #29915, #12625, #86565, #28884, #88136, #21833, #95171, #103775, #104296, #20798, #14218, #69823, #80019, #63341, #87081, #46084, #54672, #71397, #13690, #46602, #94652, #78965, #4557, #53630, #39061, #45562, #30447, #6130, #104845, #30986, #94098, #20262, #53108, #12103, #78431, #37494, #45033, #77918, #4027, #72466, #15824, #88657, #64395, #16351, #97269, #23415, #81082 ),
 .UNSPECIFIED., .F., .F.,
 ( 4, 1, 1, 1, 1, 1, 1, 1, 1, 2, 2, 1, 1, 1, 1, 1, 1, 2, 2, 1, 1, 1, 1, 1, 1, 1, 2, 2, 1, 1, 1, 1, 1, 1, 1, 2, 2, 1, 1, 1, 1, 1, 1, 1, 2, 2, 2, 1, 1, 1, 2, 2, 1, 1, 1, 1, 1, 2, 2, 1, 1, 1, 1, 1, 1, 1, 2, 2, 1, 1, 1, 1, 1, 1, 1, 2, 2, 1, 1, 1, 1, 1, 1, 1, 1, 2, 2, 1, 1, 1, 1, 1, 1, 1, 1, 1, 1, 2, 2, 1, 1, 1, 1, 1, 1, 1, 1, 1, 2, 2, 2, 1, 1, 1, 1, 1, 1, 1, 1, 2, 2, 1, 1, 1, 1, 1, 1, 1, 1, 1, 2, 2, 1, 1, 1, 1, 1, 1, 1, 1, 2, 2, 1, 1, 1, 1, 1, 1, 1, 1, 1, 2, 2, 1, 1, 1, 1, 1, 1, 1, 1, 1, 1, 2, 2, 1, 1, 1, 1, 1, 1, 1, 2, 2, 1, 1, 1, 1, 1, 1, 1, 2, 2, 1, 1, 1, 1, 1, 2, 2, 1, 1, 1, 2, 2, 1, 1, 1, 1, 2, 2, 1, 1, 1, 1, 1, 2, 2, 1, 1, 1, 2, 2, 1, 1, 1, 2, 2, 1, 1, 1, 1, 1, 2, 2, 1, 2, 2, 1, 1, 1, 1, 1, 2, 2, 1, 1, 1, 1, 1, 1, 1, 2, 2, 1, 1, 1, 1, 1, 1, 1, 1, 2, 2, 1, 1, 1, 1, 1, 1, 1, 1, 2, 2, 1, 1, 1, 1, 1, 1, 2, 2, 1, 1, 1, 1, 1, 1, 1, 1, 2, 2, 1, 1, 1, 1, 1, 1, 1, 2, 2, 1, 1, 1, 1, 1, 1, 2, 2, 1, 1, 1, 1, 1, 1, 1, 1, 2, 2, 1, 1, 1, 1, 1, 1, 2, 2, 1, 1, 1, 1, 1, 1, 1, 1, 2, 2, 1, 1, 1, 2, 2, 1, 1, 4 ),
 ( 0.000000000000000000, 0.007812499999918122787, 0.01171874999987713474, 0.01367187499985664072, 0.01464843749984634166, 0.01513671874984119300, 0.01538085937483866031, 0.01550292968733738355, 0.01556396484358680936, 0.01559448242171157170, 0.01562499999983633578, 0.02343749999978248996, 0.02734374999975560522, 0.02929687499974212295, 0.03027343749973534712, 0.03076171874973193318, 0.03100585937473019152, 0.03112792968722936579, 0.03124999999972853659, 0.03515624999970040632, 0.03710937499968632036, 0.03808593749967928432, 0.03857421874967577324, 0.03881835937467401770, 0.03894042968717313646, 0.03900146484342268544, 0.03903198242154746339, 0.03906249999967224135, 0.04296874999964340330, 0.04492187499962898428, 0.04589843749962177477, 0.04638671874961817349, 0.04663085937461636937, 0.04675292968711546732, 0.04681396484336501629, 0.04684448242148979424, 0.04687499999961456526, 0.05468749999955686836, 0.05859374999952800950, 0.06054687499951358354, 0.06152343749950636709, 0.06201171874950275886, 0.06225585937450096169, 0.06237792968700005963, 0.06243896484324961554, 0.06249999999949916452, 0.07031249999944196027, 0.07421874999941335815, 0.07617187499939906403, 0.07714843749939191697, 0.07763671874938833650, 0.07812499999938475603, 0.08593749999932762118, 0.08984374999929904682, 0.09179687499928476657, 0.09277343749927764727, 0.09326171874927406680, 0.09350585937427229044, 0.09374999999927050021, 0.1093749999991570909, 0.1171874999991003585, 0.1210937499990720062, 0.1230468749990578231, 0.1240234374990507316, 0.1245117187490471927, 0.1247558593740454302, 0.1248779296865445559, 0.1249999999990436816, 0.1406249999989302724, 0.1484374999988735677, 0.1523437499988452293, 0.1542968749988310739, 0.1552734374988239685, 0.1557617187488203880, 0.1560058593738185839, 0.1561279296863176957, 0.1562499999988168076, 0.1718749999987017885, 0.1796874999986442512, 0.1835937499986154964, 0.1855468749986011190, 0.1865234374985939025, 0.1870117187485903221, 0.1872558593735885457, 0.1873779296860876853, 0.1874389648423372412, 0.1874999999985867694, 0.2187499999983521515, 0.2343749999982348287, 0.2421874999981761811, 0.2460937499981468435, 0.2480468749981321608, 0.2490234374981249166, 0.2495117187481212251, 0.2497558593731193932, 0.2498779296856184773, 0.2499389648418680054, 0.2499694824199928389, 0.2499999999981176169, 0.2812499999979674037, 0.2968749999978922416, 0.3046874999978547160, 0.3085937499978359533, 0.3105468749978264609, 0.3115234374978217979, 0.3120117187478193554, 0.3122558593728181897, 0.3123779296853176346, 0.3124389648415674126, 0.3124999999978171350, 0.3437499999976899590, 0.3593749999976263987, 0.3671874999975946463, 0.3710937499975788256, 0.3730468749975709430, 0.3740234374975669462, 0.3745117187475650034, 0.3747558593725640597, 0.3748779296850636156, 0.3749389648413133380, 0.3749999999975630605, 0.4062499999974437670, 0.4218749999973840370, 0.4296874999973542830, 0.4335937499973393505, 0.4355468749973320230, 0.4365234374973284148, 0.4370117187473264719, 0.4372558593723253617, 0.4373779296848246956, 0.4374389648410741960, 0.4374999999973237519, 0.4531249999971969644, 0.4609374999971336817, 0.4648437499971019848, 0.4667968749970862197, 0.4677734374970783926, 0.4682617187470746178, 0.4685058593720728415, 0.4686279296845718423, 0.4686889648408214537, 0.4687499999970711206, 0.4843749999969746978, 0.4921874999969265141, 0.4960937499969023667, 0.4980468749968904874, 0.4990234374968843811, 0.4995117187468814390, 0.4997558593718801068, 0.4998779296843793296, 0.4999389648406289410, 0.4999694824187537190, 0.4999999999968784969, 0.5312499999966507902, 0.5468749999965369923, 0.5546874999964801489, 0.5585937499964518382, 0.5605468749964376274, 0.5615234374964305220, 0.5620117187464269692, 0.5622558593714250819, 0.5623779296839241937, 0.5624389648401738606, 0.5624694824182986386, 0.5624999999964234165, 0.5703124999963722352, 0.5742187499963464781, 0.5761718749963338215, 0.5771484374963274933, 0.5776367187463243846, 0.5778808593713228303, 0.5780029296838220532, 0.5780639648400717201, 0.5781249999963213870, 0.5820312499963147257, 0.5839843749963113950, 0.5849609374963098407, 0.5854492187463090636, 0.5856933593713085084, 0.5858154296838082864, 0.5858764648400581754, 0.5859069824181831754, 0.5859374999963080644, 0.5878906249962998487, 0.5888671874962957409, 0.5893554687462938535, 0.5895996093712928543, 0.5897216796837922992, 0.5897827148400422992, 0.5898437499962921882, 0.5908203124962911890, 0.5913085937462908559, 0.5915527343712906339, 0.5916748046837905228, 0.5917968749962905228, 0.5927734374962895236, 0.5932617187462891906, 0.5935058593712889685, 0.5936279296837888575, 0.5936889648400387465, 0.5937499999962886355, 0.5957031249962814190, 0.5966796874962778663, 0.5971679687462759789, 0.5974121093712749797, 0.5975341796837745356, 0.5975952148400242026, 0.5976562499962738695, 0.5996093749962628783, 0.6005859374962573272, 0.6010742187462545516, 0.6013183593712531083, 0.6015624999962516650, 0.6035156249962393415, 0.6044921874962332353, 0.6049804687462301267, 0.6052246093712285724, 0.6054687499962270181, 0.6074218749962153607, 0.6083984374962094765, 0.6088867187462065900, 0.6091308593712051467, 0.6092529296837044805, 0.6093139648399541475, 0.6093749999962038144, 0.6113281249961912689, 0.6123046874961850516, 0.6132812499961787234, 0.6152343749961661779, 0.6162109374961598496, 0.6166992187461567410, 0.6169433593711552977, 0.6170654296836544095, 0.6171264648399039654, 0.6171874999961536323, 0.6210937499961349806, 0.6230468749961256547, 0.6240234374961208808, 0.6245117187461185493, 0.6247558593711173280, 0.6248779296836167729, 0.6249389648398665509, 0.6249694824179915509, 0.6249999999961165509, 0.6328124999961596275, 0.6367187499961810548, 0.6386718749961918240, 0.6396484374961970421, 0.6401367187461998176, 0.6403808593712011499, 0.6405029296837018160, 0.6405639648399520381, 0.6405944824180771491, 0.6406249999962022601, 0.6484374999962930763, 0.6523437499963383734, 0.6542968749963610220, 0.6552734374963723463, 0.6557617187463781194, 0.6560058593713808950, 0.6561279296838822273, 0.6561889648401328934, 0.6562194824182582265, 0.6562499999963835595, 0.6640624999964694908, 0.6679687499965123454, 0.6699218749965338837, 0.6708984374965446529, 0.6713867187465498709, 0.6716308593715525355, 0.6717529296840539788, 0.6718749999965553110, 0.6796874999966473485, 0.6835937499966934228, 0.6855468749967164044, 0.6865234374967280617, 0.6870117187467337239, 0.6872558593717364994, 0.6873779296842381648, 0.6874389648404887199, 0.6874694824186140529, 0.6874999999967393860, 0.7031249999969233500, 0.7109374999970154985, 0.7148437499970615727, 0.7167968749970846654, 0.7177734374970963227, 0.7182617187471022069, 0.7185058593721050935, 0.7186279296846065368, 0.7187499999971078690, 0.7343749999972727371, 0.7421874999973553377, 0.7460937499973965270, 0.7480468749974170661, 0.7490234374974272802, 0.7495117187474323872, 0.7497558593724349407, 0.7499999999974373832, 0.8124999999980522247, 0.8437499999983595345, 0.8593749999985131893, 0.8671874999985900168, 0.8710937499986284305, 0.8730468749986476373, 0.8740234374986571853, 0.8745117187486619592, 0.8747558593736642907, 0.8749999999986666221, 0.8906249999988182786, 0.8984374999988939958, 0.9023437499989319655, 0.9042968749989508392, 0.9052734374989602761, 0.9057617187489650501, 0.9060058593739673816, 0.9062499999989697130, 0.9218749999991281419, 0.9296874999992073008, 0.9335937499992469357, 0.9355468749992666977, 0.9365234374992766897, 0.9370117187492815747, 0.9372558593742840172, 0.9373779296867852384, 0.9374389648430360156, 0.9374999999992866817, 0.9531249999994668709, 0.9609374999995567990, 0.9619140624995680122, 0.9624023437495735633, 0.9628906249995791145, 0.9648437499996014299, 0.9687499999996457278, 1.000000000000000000 ),
 .UNSPECIFIED. ) ;
#100327 = CARTESIAN_POINT ( 'NONE',  ( 28.19909662334077538, 36.30566500375478967, 9.434792300628540573 ) ) ;
#100328 = CARTESIAN_POINT ( 'NONE',  ( -5.290067270632216712, 52.08006895350504095, 6.031152949374556371 ) ) ;
#100330 = EDGE_LOOP ( 'NONE', ( #76530, #18858, #72725, #24358, #38635 ) ) ;
#100329 = AXIS2_PLACEMENT_3D ( 'NONE', #6476, #103594, #22709 ) ;
#100331 = CARTESIAN_POINT ( 'NONE',  ( -14.29190075645216851, 12.99999999999999289, 0.000000000000000000 ) ) ;
#100332 = CARTESIAN_POINT ( 'NONE',  ( 30.80770627799282124, 8.073552547385910216, -41.40953488888267486 ) ) ;
#100333 = CARTESIAN_POINT ( 'NONE',  ( -23.21751746555244722, -1.200000000000000030E-05, 31.95617127781060773 ) ) ;
#100334 = PRODUCT_RELATED_PRODUCT_CATEGORY ( 'part', '', ( #53642 ) ) ;
#100335 = CARTESIAN_POINT ( 'NONE',  ( -102.4273698138863722, -60.00000000000000000, 95.23766053874160775 ) ) ;
#100336 = CARTESIAN_POINT ( 'NONE',  ( 12.33349330513380693, 1.593028355512270962E-15, 0.000000000000000000 ) ) ;
#100337 = CARTESIAN_POINT ( 'NONE',  ( -16.13647630347099593, 6.334953579830782111, 5.738861489053475928 ) ) ;
#100338 = CARTESIAN_POINT ( 'NONE',  ( 31.11679462788039530, 441.4271381875185511, 23.27438508043199406 ) ) ;
#100340 = SURFACE_STYLE_USAGE ( .BOTH. , #76060 ) ;
#100339 = APPLICATION_CONTEXT ( 'automotive_design' ) ;
#100342 =( NAMED_UNIT ( * ) SI_UNIT ( $, .STERADIAN. ) SOLID_ANGLE_UNIT ( ) );
#100341 = CARTESIAN_POINT ( 'NONE',  ( -32.99999999999999289, 435.0774731480751143, 11.67986145722082902 ) ) ;
#100343 = CARTESIAN_POINT ( 'NONE',  ( -81.29675584934015831, -56.99031933536476657, 180.9625569273741519 ) ) ;
#100344 = ORIENTED_EDGE ( 'NONE', *, *, #74259, .T. ) ;
#100345 = ORIENTED_EDGE ( 'NONE', *, *, #26991, .T. ) ;
#100346 = VERTEX_POINT ( 'NONE', #101575 ) ;
#100347 = CYLINDRICAL_SURFACE ( 'NONE', #33826, 4.000000000000000000 ) ;
#100348 = CARTESIAN_POINT ( 'NONE',  ( 19.96162532426522773, 302.8116070918645164, 9.928455558879880627 ) ) ;
#100349 = ORIENTED_EDGE ( 'NONE', *, *, #80730, .F. ) ;
#100350 = COLOUR_RGB ( '', 0.08235294, 0.09019608, 0.10196078) ;
#100351 = CARTESIAN_POINT ( 'NONE',  ( 32.13672086716894682, 487.8704565892116420, 8.624753397812970235 ) ) ;
#100352 = FACE_OUTER_BOUND ( 'NONE', #85173, .T. ) ;
#100353 = DIRECTION ( 'NONE',  ( 0.5735764363510470476, -0.8191520442889911324, 1.003171929053524007E-16 ) ) ;
#100354 = CARTESIAN_POINT ( 'NONE',  ( -7.801642220026311136, -61.41203173850968966, 1.787233835843584417 ) ) ;
#100355 = CIRCLE ( 'NONE', #7343, 5.000000000000001776 ) ;
#100356 = CARTESIAN_POINT ( 'NONE',  ( 43.73399259471502631, 464.6843803606428196, 7.646783569293355676 ) ) ;
#100357 = FILL_AREA_STYLE ('',( #10803 ) ) ;
#100358 = CARTESIAN_POINT ( 'NONE',  ( -43.43869229197126458, 464.9661605157749591, 13.42065392471462637 ) ) ;
#100359 = CARTESIAN_POINT ( 'NONE',  ( 103.3501304845727873, -29.99999999999998579, 116.5671668536019610 ) ) ;
#100360 = EDGE_CURVE ( 'NONE', #81401, #96494, #49286, .T. ) ;
#100361 = CARTESIAN_POINT ( 'NONE',  ( -76.30486425386099825, -30.00000000000004619, 168.5691345232379206 ) ) ;
#100362 = CARTESIAN_POINT ( 'NONE',  ( -58.13295120765930335, -25.60580355849098311, 61.38901395099644986 ) ) ;
#100363 = ORIENTED_EDGE ( 'NONE', *, *, #77851, .T. ) ;
#100364 = CARTESIAN_POINT ( 'NONE',  ( 93.82195685172136734, -59.99999999999752731, -16.20128001769883497 ) ) ;
#100365 = VERTEX_POINT ( 'NONE', #28253 ) ;
#100366 = CARTESIAN_POINT ( 'NONE',  ( 7.105781327744331577, -35.99149389464556492, 29.87857778648328733 ) ) ;
#100367 = CARTESIAN_POINT ( 'NONE',  ( -102.7248202937925612, -52.71211498143689766, 190.6735650292727087 ) ) ;
#100368 = PLANE ( 'NONE',  #36912 ) ;
#100369 = CIRCLE ( 'NONE', #90063, 61.23540616453487218 ) ;
#100370 = CARTESIAN_POINT ( 'NONE',  ( -5.623754609091350609, 51.29168761065961490, 8.497413747174256571 ) ) ;
#100371 = CARTESIAN_POINT ( 'NONE',  ( 32.33349330513380693, 1.593028355512270962E-15, 0.000000000000000000 ) ) ;
#100372 = VERTEX_POINT ( 'NONE', #3414 ) ;
#100373 = CARTESIAN_POINT ( 'NONE',  ( 19.49236955434526308, 49.99908790945509196, 60.06985828019035267 ) ) ;
#100374 = CARTESIAN_POINT ( 'NONE',  ( -77.82043145825072372, -60.00000000000001421, 192.4616265064402114 ) ) ;
#100375 = CARTESIAN_POINT ( 'NONE',  ( -2.714483990415212045, -0.3795274241210661037, 102.8323277908853868 ) ) ;
#100376 = CARTESIAN_POINT ( 'NONE',  ( -7.188101187500000044, -21.78125000204838457, -8.802885111219163269E-16 ) ) ;
#100377 = CARTESIAN_POINT ( 'NONE',  ( -0.1682053726333464228, 36.30024107553215629, -29.75000000000000711 ) ) ;
#100379 = EDGE_CURVE ( 'NONE', #6367, #104741, #44156, .T. ) ;
#100378 = CARTESIAN_POINT ( 'NONE',  ( 45.94900261086841198, 6.123233995736772199E-16, -5.000000000000001776 ) ) ;
#100380 = CARTESIAN_POINT ( 'NONE',  ( -1.315122544340494137, 21.63948755414514125, -6.879847735748377602 ) ) ;
#100381 = LINE ( 'NONE', #10304, #106289 ) ;
#100382 = CARTESIAN_POINT ( 'NONE',  ( -6.663120783604494335, 3.846954578057034446, -6.460786012260001598 ) ) ;
#100383 = EDGE_CURVE ( 'NONE', #17567, #29960, #85947, .T. ) ;
#100384 = CARTESIAN_POINT ( 'NONE',  ( 6.903355605563677777, -12.56553646782259293, 8.191904130043296206 ) ) ;
#100385 = PRESENTATION_STYLE_ASSIGNMENT (( #67503 ) ) ;
#100386 = CARTESIAN_POINT ( 'NONE',  ( -5.121894999926677627, -2.681690743133432697, -18.64842307824732970 ) ) ;
#100387 = CARTESIAN_POINT ( 'NONE',  ( -31.02242612524658938, -39.49085496570000942, 33.50213709495920966 ) ) ;
#100388 = B_SPLINE_CURVE_WITH_KNOTS ( 'NONE', 3,
 ( #58028, #1372, #34338, #81758, #57488, #16516, #49402, #82311 ),
 .UNSPECIFIED., .F., .F.,
 ( 4, 2, 2, 4 ),
 ( 0.004673709593152165255, 0.005837709341827652942, 0.007001709090503139762, 0.009329708587854115137 ),
 .UNSPECIFIED. ) ;
#100389 = CARTESIAN_POINT ( 'NONE',  ( 6.249999999999998224, -4.618802153516998743, 7.999999999999998224 ) ) ;
#100390 = CARTESIAN_POINT ( 'NONE',  ( 46.23384880443906297, -29.15623005253502598, 42.24550313519566203 ) ) ;
#100391 = CARTESIAN_POINT ( 'NONE',  ( 3.313708498984800688, -14.28124999999998934, 7.999999999999960032 ) ) ;
#100392 = ORIENTED_EDGE ( 'NONE', *, *, #106607, .F. ) ;
#100393 = CARTESIAN_POINT ( 'NONE',  ( -7.045965687440311598, 86.30392463786034796, 3.790395326974319357 ) ) ;
#100394 = CARTESIAN_POINT ( 'NONE',  ( -78.26226481065664586, -38.60566898501981825, 189.0129437702546511 ) ) ;
#100395 = ORIENTED_EDGE ( 'NONE', *, *, #54001, .T. ) ;
#100397 = CARTESIAN_POINT ( 'NONE',  ( 40.93435977689158989, 414.3154843149413296, 27.72243992809649527 ) ) ;
#100396 = DIRECTION ( 'NONE',  ( -0.000000000000000000, -1.000000000000000000, -0.000000000000000000 ) ) ;
#100398 = CARTESIAN_POINT ( 'NONE',  ( 23.93832669066742724, -60.00000000000001421, 35.01784081144786853 ) ) ;
#100399 = DIRECTION ( 'NONE',  ( 0.000000000000000000, 1.000000000000000000, 0.000000000000000000 ) ) ;
#100400 = CARTESIAN_POINT ( 'NONE',  ( -7.395123836361360503, 40.93288475959919026, -59.01287901077084541 ) ) ;
#100401 = CARTESIAN_POINT ( 'NONE',  ( 9.852235012526417535, 15.56087475005694643, -1.749814335632526863 ) ) ;
#100402 = EDGE_CURVE ( 'NONE', #15859, #11593, #60605, .T. ) ;
#100403 = FACE_OUTER_BOUND ( 'NONE', #54582, .T. ) ;
#100404 = CARTESIAN_POINT ( 'NONE',  ( -21.16803287062261774, 305.0380828635773582, 8.976778075698762294 ) ) ;
#100405 = DIRECTION ( 'NONE',  ( 0.000000000000000000, -0.000000000000000000, 1.000000000000000000 ) ) ;
#100406 = CARTESIAN_POINT ( 'NONE',  ( 106.3883173979913437, -60.00000000000000711, 118.8213136657173266 ) ) ;
#100408 = CARTESIAN_POINT ( 'NONE',  ( 6.585468679846627538, -7.640532685286905767, -0.2337908078075620621 ) ) ;
#100407 = CIRCLE ( 'NONE', #60787, 5.000000000000001776 ) ;
#100409 = CIRCLE ( 'NONE', #50505, 5.000000000000002665 ) ;
#100410 = CARTESIAN_POINT ( 'NONE',  ( -53.08935917470201815, -30.00000000000000000, 52.21147893555080799 ) ) ;
#100411 = ORIENTED_EDGE ( 'NONE', *, *, #8547, .T. ) ;
#100412 = CARTESIAN_POINT ( 'NONE',  ( 2.230802491789472874, -49.81451076291526192, 102.4842558203777827 ) ) ;
#100413 = CARTESIAN_POINT ( 'NONE',  ( -99.23654757740681021, -30.00000000000000711, 188.2532938818355319 ) ) ;
#100414 = ORIENTED_EDGE ( 'NONE', *, *, #102318, .T. ) ;
#100415 = CARTESIAN_POINT ( 'NONE',  ( 26.12851586566475248, 36.99786746614248045, -9.591385120608638459 ) ) ;
#100416 =( NAMED_UNIT ( * ) SI_UNIT ( $, .STERADIAN. ) SOLID_ANGLE_UNIT ( ) );
#100417 = CARTESIAN_POINT ( 'NONE',  ( 19.83463548332445825, 303.8035096162420245, 9.926734387303332241 ) ) ;
#100418 = CARTESIAN_POINT ( 'NONE',  ( 24.83349330513380693, -4.000000000000000000, 4.898587196589415787E-16 ) ) ;
#100419 = CARTESIAN_POINT ( 'NONE',  ( 2.977408999572651815, -18.31250000204838457, 7.188101187500000933 ) ) ;
#100420 = EDGE_CURVE ( 'NONE', #57235, #6434, #61415, .T. ) ;
#100421 = DIRECTION ( 'NONE',  ( -1.000000000000000000, -1.224606353822377258E-16, -0.000000000000000000 ) ) ;
#100423 = EDGE_LOOP ( 'NONE', ( #79730, #44133, #55057, #41429 ) ) ;
#100422 = CARTESIAN_POINT ( 'NONE',  ( 0.000000000000000000, -1.550510257216834331, 112.0000000000000000 ) ) ;
#100424 = CARTESIAN_POINT ( 'NONE',  ( 82.17599174339494539, -39.49534644509261483, 162.1453621538301775 ) ) ;
#100425 = CARTESIAN_POINT ( 'NONE',  ( 85.31310517497098544, 1.030564683017419500E-14, 0.000000000000000000 ) ) ;
#100426 = CARTESIAN_POINT ( 'NONE',  ( -16.64348903516521005, -1.200000000000000030E-05, -5.407797401561534656 ) ) ;
#100427 = ORIENTED_EDGE ( 'NONE', *, *, #1253, .F. ) ;
#100428 = CARTESIAN_POINT ( 'NONE',  ( -20.49977525862259142, 302.8459220885798686, -10.00124997875687427 ) ) ;
#100429 = SURFACE_SIDE_STYLE ('',( #84790 ) ) ;
#100430 = CARTESIAN_POINT ( 'NONE',  ( 3.294249609603376872, -3.000000000000002665, -70.27378291343094929 ) ) ;
#100431 = CARTESIAN_POINT ( 'NONE',  ( 0.000000000000000000, 0.000000000000000000, 5.000000000000002665 ) ) ;
#100432 = LINE ( 'NONE', #76688, #12922 ) ;
#100434 = CARTESIAN_POINT ( 'NONE',  ( -31.47811980959860989, 326.9156455337226248, 15.84085572310068812 ) ) ;
#100433 = AXIS2_PLACEMENT_3D ( 'NONE', #1827, #17518, #50379 ) ;
#100435 = CARTESIAN_POINT ( 'NONE',  ( -15.05785784214673129, 3.824195276770050445, -4.604276673498571171 ) ) ;
#100436 = EDGE_CURVE ( 'NONE', #16299, #22473, #59635, .T. ) ;
#100437 = EDGE_CURVE ( 'NONE', #45306, #70963, #76221, .T. ) ;
#100438 = VERTEX_POINT ( 'NONE', #56165 ) ;
#100439 = MECHANICAL_DESIGN_GEOMETRIC_PRESENTATION_REPRESENTATION (  '', ( #66021 ), #19581 ) ;
#100440 = FILL_AREA_STYLE ('',( #67559 ) ) ;
#100441 = CIRCLE ( 'NONE', #33337, 5.000000000000000000 ) ;
#100442 = CARTESIAN_POINT ( 'NONE',  ( -1.128130203588978198, 301.8985493317088071, 9.936162350048869385 ) ) ;
#100444 = CARTESIAN_POINT ( 'NONE',  ( 11.09043181264936173, 18.64284798592871439, 36.79570967431541817 ) ) ;
#100443 =( BOUNDED_SURFACE ( )  B_SPLINE_SURFACE ( 3, 2, ( 
 ( #12889, #45813, #6928 ),
 ( #15553, #55986, #5862 ),
 ( #104563, #48444, #31764 ),
 ( #47385, #38787, #13952 ),
 ( #89980, #98066, #64645 ),
 ( #40898, #80815, #56529 ),
 ( #81335, #39850, #73240 ),
 ( #79756, #30170, #80277 ),
 ( #31250, #71656, #89459 ),
 ( #39325, #7445, #97517 ) ),
 .UNSPECIFIED., .F., .F., .F. ) 
 B_SPLINE_SURFACE_WITH_KNOTS ( ( 4, 2, 2, 2, 4 ),
 ( 3, 3 ),
 ( 0.002450517525418901676, 0.003060732775749469906, 0.003670948026080037702, 0.004891378526741174161, 0.007332239528063446213 ),
 ( 0.000000000000000000, 1.000000000000000000 ),
 .UNSPECIFIED. ) 
 GEOMETRIC_REPRESENTATION_ITEM ( )  RATIONAL_B_SPLINE_SURFACE ( (
 ( 1.000000000000000000, 0.7071067811865475727, 1.000000000000000000),
 ( 1.000000000000000000, 0.7344063550101603832, 1.000000000000000000),
 ( 1.000000000000000000, 0.7590375248711465073, 1.000000000000000000),
 ( 1.000000000000000000, 0.8038331608703648268, 1.000000000000000000),
 ( 1.000000000000000000, 0.8240352460866686712, 1.000000000000000000),
 ( 1.000000000000000000, 0.8791017378331671406, 1.000000000000000000),
 ( 1.000000000000000000, 0.9085032776981341041, 1.000000000000000000),
 ( 1.000000000000000000, 0.9784170511695907679, 1.000000000000000000),
 ( 1.000000000000000000, 0.9996598051697292986, 1.000000000000000000),
 ( 1.000000000000000000, 1.000000000000000000, 1.000000000000000000) ) ) 
 REPRESENTATION_ITEM ( '' )  SURFACE ( )  );
#100445 = CARTESIAN_POINT ( 'NONE',  ( 86.86885569288263298, -50.10510242869298736, 191.7877947622934585 ) ) ;
#100446 = DIRECTION ( 'NONE',  ( -0.000000000000000000, -0.000000000000000000, -1.000000000000000000 ) ) ;
#100447 = CARTESIAN_POINT ( 'NONE',  ( -5.082755093536326818, -27.21875000204838813, 5.082755093536325042 ) ) ;
#100448 = DIRECTION ( 'NONE',  ( -1.000000000000000000, -0.000000000000000000, -0.000000000000000000 ) ) ;
#100449 =( BOUNDED_CURVE ( )  B_SPLINE_CURVE ( 2, ( #19833, #4138, #69411 ),
 .UNSPECIFIED., .F., .T. ) 
 B_SPLINE_CURVE_WITH_KNOTS ( ( 3, 3 ),
 ( 0.000000000000000000, 1.000000000000000000 ),
 .UNSPECIFIED. ) 
 CURVE ( )  GEOMETRIC_REPRESENTATION_ITEM ( )  RATIONAL_B_SPLINE_CURVE ( ( 1.000000000000000000, 1.428571428571452584, 1.428571428571428825 ) ) 
 REPRESENTATION_ITEM ( '' )  );
#100450 = CARTESIAN_POINT ( 'NONE',  ( 7.945231034609332887, 51.78157138488628419, 3.881274660011450717 ) ) ;
#100451 = ADVANCED_FACE ( 'NONE', ( #47034 ), #89107, .T. ) ;
#100452 = FILL_AREA_STYLE ('',( #44353 ) ) ;
#100453 = ORIENTED_EDGE ( 'NONE', *, *, #8549, .T. ) ;
#100454 = CARTESIAN_POINT ( 'NONE',  ( 20.59999999999999787, 3.309500000000003439, 0.000000000000000000 ) ) ;
#100455 = LINE ( 'NONE', #2273, #94341 ) ;
#100456 = CARTESIAN_POINT ( 'NONE',  ( -9.969369542538062845, 7.546308885167836600, -5.000000000000000888 ) ) ;
#100457 = EDGE_CURVE ( 'NONE', #24323, #33529, #35562, .T. ) ;
#100458 = CARTESIAN_POINT ( 'NONE',  ( 0.000000000000000000, 0.000000000000000000, 0.000000000000000000 ) ) ;
#100459 = EDGE_LOOP ( 'NONE', ( #98924, #40609, #97594, #100200, #52780, #103821 ) ) ;
#100460 = CARTESIAN_POINT ( 'NONE',  ( -30.00000000000000355, 461.8802764867011206, 14.89328939273810093 ) ) ;
#100461 = DIRECTION ( 'NONE',  ( 0.000000000000000000, 0.000000000000000000, -1.000000000000000000 ) ) ;
#100462 = CARTESIAN_POINT ( 'NONE',  ( 32.05117072706241999, 435.5678670110675057, 16.71961908548328424 ) ) ;
#100463 = CARTESIAN_POINT ( 'NONE',  ( -8.000000000000000000, -22.43750000409676915, -9.797174393178825657E-16 ) ) ;
#100464 = LINE ( 'NONE', #90796, #37532 ) ;
#100465 = DIRECTION ( 'NONE',  ( -1.000000000000000000, -0.000000000000000000, -0.000000000000000000 ) ) ;
#100466 = CARTESIAN_POINT ( 'NONE',  ( -91.39810932065459781, -60.00000000000001421, 202.2552732027076274 ) ) ;
#100467 = VECTOR ( 'NONE', #77659, 1000.000000000000000 ) ;
#100468 = CARTESIAN_POINT ( 'NONE',  ( 9.108175880970147631, 43.74195033122234122, -14.58320101129880975 ) ) ;
#100469 = CYLINDRICAL_SURFACE ( 'NONE', #64608, 4.000000000000000000 ) ;
#100470 = CARTESIAN_POINT ( 'NONE',  ( -85.72996169165566016, -28.54324383439242752, 179.8132596535202197 ) ) ;
#100471 = CONICAL_SURFACE ( 'NONE', #53964, 3.309500000000001663, 0.9599310885968770357 ) ;
#100472 = EDGE_CURVE ( 'NONE', #17653, #59863, #79934, .T. ) ;
#100473 = AXIS2_PLACEMENT_3D ( 'NONE', #42642, #83102, #11320 ) ;
#100474 = ORIENTED_EDGE ( 'NONE', *, *, #6941, .T. ) ;
#100475 = DIRECTION ( 'NONE',  ( 0.000000000000000000, 0.000000000000000000, 1.000000000000000000 ) ) ;
#100476 = CARTESIAN_POINT ( 'NONE',  ( 3.396360046676592859, -0.8468429378662341023, 103.9790200242207021 ) ) ;
#100477 = CARTESIAN_POINT ( 'NONE',  ( -86.87225386170726438, -60.16560806864642075, -2.785716167088986506 ) ) ;
#100478 = FACE_OUTER_BOUND ( 'NONE', #23350, .T. ) ;
#100479 = CARTESIAN_POINT ( 'NONE',  ( -16.02226691200762332, 43.96107415247629291, 4.310996538645964549 ) ) ;
#100480 = CIRCLE ( 'NONE', #19558, 0.9999999999999997780 ) ;
#100481 = DIRECTION ( 'NONE',  ( 0.000000000000000000, -1.000000000000000000, 0.000000000000000000 ) ) ;
#100482 = DIRECTION ( 'NONE',  ( 0.000000000000000000, -1.000000000000000000, 0.000000000000000000 ) ) ;
#100483 = SURFACE_STYLE_FILL_AREA ( #11461 ) ;
#100484 = DIRECTION ( 'NONE',  ( 0.000000000000000000, -1.000000000000000000, 0.000000000000000000 ) ) ;
#100485 = CARTESIAN_POINT ( 'NONE',  ( 52.32017852953563164, -14.21045842199431242, 63.23906622249963760 ) ) ;
#100486 = CARTESIAN_POINT ( 'NONE',  ( -34.88259098417105974, 437.7046102974885002, 4.606877878021536254 ) ) ;
#100487 = CARTESIAN_POINT ( 'NONE',  ( -93.17098673813583787, -59.99999999999997158, -17.95829132299026298 ) ) ;
#100488 = CARTESIAN_POINT ( 'NONE',  ( -75.97434538570179541, -29.07737278147254756, 117.1882777120721073 ) ) ;
#100489 = B_SPLINE_CURVE_WITH_KNOTS ( 'NONE', 3,
 ( #29386, #77370, #19182, #94637, #103241, #93019, #52020, #3486, #36942, #27806, #13141, #11020, #102705, #43938, #37481, #35890, #36426, #76827, #68768, #93563, #62272, #20248, #4540, #19710, #28318, #70344, #45547, #12089, #53096, #21289, #101649, #69295, #102169, #77904, #52547, #61195, #60676, #69809, #95157, #45022, #4012, #85469, #87068, #46070, #78953, #28870, #94085, #86018, #20783, #35350, #53618, #86553, #68216, #21819, #71383, #97258, #31501, #6653, #54657, #5597, #89713, #63325, #89180, #88124, #15812, #6117, #32019, #56243, #15281, #23948, #14204, #39043, #72454, #23401, #64896, #40093, #105362, #38520, #47106, #104283, #7179, #48166, #87593, #30973, #13678, #81067, #72968, #30432, #71928, #39580, #104829, #105876, #97782, #56788, #63854, #96220, #80008, #64381, #22351, #96745, #46588, #48693, #5075, #22878, #38010, #70872, #103764, #79487, #29901, #55713 ),
 .UNSPECIFIED., .F., .F.,
 ( 4, 2, 2, 1, 1, 1, 1, 2, 2, 1, 2, 2, 1, 1, 1, 2, 2, 1, 2, 2, 1, 1, 1, 2, 2, 1, 2, 2, 1, 1, 1, 2, 2, 1, 2, 2, 1, 1, 2, 2, 1, 2, 2, 1, 2, 2, 1, 2, 2, 1, 1, 2, 2, 1, 2, 2, 2, 1, 1, 2, 2, 1, 1, 2, 2, 2, 2, 1, 2, 4 ),
 ( 0.000000000000000000, 0.01574254035199997015, 0.02361381052799983032, 0.02754944561599962510, 0.02951726315999962311, 0.03050117193199966895, 0.03099312631799969187, 0.03123910351099974669, 0.03136209210749976717, 0.03148508070399978764, 0.04722762105598653920, 0.05509889123197986988, 0.05903452631997656297, 0.06100234386397482278, 0.06198625263597389717, 0.06247820702197335457, 0.06272418421497306940, 0.06297016140797279116, 0.09445524211193562225, 0.1101977824639170656, 0.1180690526399078705, 0.1220046877279032521, 0.1239725052719010123, 0.1249564140438999132, 0.1254483684298993706, 0.1259403228158987864, 0.1574254035198680290, 0.1731679438718526365, 0.1810392140478448708, 0.1849748491358410019, 0.1869426666798391368, 0.1874346210658384970, 0.1879265754518378295, 0.1889104842238366333, 0.2203955649278004358, 0.2361381052797823232, 0.2440093754557732808, 0.2479450105437687457, 0.2499128280877664643, 0.2508967368597653236, 0.2518806456317641551, 0.2833657263357283740, 0.2991082666877105667, 0.3069795368637016075, 0.3109151719516971002, 0.3128829894956948743, 0.3148508070396926484, 0.3463358877436555350, 0.3620784280956369505, 0.3699496982716277138, 0.3738853333596230399, 0.3748692421316219270, 0.3753611965176212872, 0.3758531509036206475, 0.3778209684476182550, 0.4093060491515793098, 0.4250485895035597816, 0.4329198596795500453, 0.4368554947675451494, 0.4373474491535445652, 0.4378394035395440365, 0.4388233123115429235, 0.4407911298555406421, 0.4565336702075227238, 0.4644049403835138201, 0.4683405754715093128, 0.4703083930155070869, 0.4722762105595048610, 0.4880187509114868871, 0.5037612912634689133 ),
 .UNSPECIFIED. ) ;
#100490 = ORIENTED_EDGE ( 'NONE', *, *, #91017, .T. ) ;
#100491 = CARTESIAN_POINT ( 'NONE',  ( 70.80389978121282013, -30.00000000000000711, 131.5992258684728995 ) ) ;
#100492 = CARTESIAN_POINT ( 'NONE',  ( 15.48885350034982089, -60.00000000000000000, 42.17456718879848410 ) ) ;
#100493 = ORIENTED_EDGE ( 'NONE', *, *, #25364, .F. ) ;
#100494 = CARTESIAN_POINT ( 'NONE',  ( 15.80778651423128700, -3.783390974281282571, 14.51852905608714828 ) ) ;
#100495 = CARTESIAN_POINT ( 'NONE',  ( 7.188101187499999156, -22.62500000204838813, 2.977408999572654924 ) ) ;
#100496 = CARTESIAN_POINT ( 'NONE',  ( -1.012387302972281189, 27.47360406062330185, -40.25103504401613463 ) ) ;
#100497 = VERTEX_POINT ( 'NONE', #39505 ) ;
#100498 = SURFACE_STYLE_FILL_AREA ( #1792 ) ;
#100499 = DIRECTION ( 'NONE',  ( 1.000000000000000000, 1.224606353822377258E-16, 0.000000000000000000 ) ) ;
#100500 = AXIS2_PLACEMENT_3D ( 'NONE', #36547, #94762, #52672 ) ;
#100501 = CARTESIAN_POINT ( 'NONE',  ( -20.00000000000000000, 12.99999999999999289, 0.000000000000000000 ) ) ;
#100502 = CARTESIAN_POINT ( 'NONE',  ( 48.02835407290504577, -1.200000000000000030E-05, -14.35535821593549954 ) ) ;
#100503 = CARTESIAN_POINT ( 'NONE',  ( -7.188101187500000044, -13.90625000204838457, -8.802885111219163269E-16 ) ) ;
#100504 = CARTESIAN_POINT ( 'NONE',  ( -5.656854249492381470, -17.75000000409676915, 5.656854249492379694 ) ) ;
#100505 = CARTESIAN_POINT ( 'NONE',  ( 19.50000000000000000, 12.99999999999999289, 0.000000000000000000 ) ) ;
#100506 = DIRECTION ( 'NONE',  ( 0.000000000000000000, 0.000000000000000000, -1.000000000000000000 ) ) ;
#100507 = CARTESIAN_POINT ( 'NONE',  ( -11.68767211932491179, 50.00000000000000000, -81.85902538600507228 ) ) ;
#100508 = ADVANCED_FACE ( 'NONE', ( #22274 ), #9634, .T. ) ;
#100509 = CARTESIAN_POINT ( 'NONE',  ( 4.406842699996129653, -6.115962218725295330, -6.735605996566196296E-15 ) ) ;
#100510 = CIRCLE ( 'NONE', #35103, 5.000000000000011546 ) ;
#100511 = ORIENTED_EDGE ( 'NONE', *, *, #6161, .F. ) ;
#100512 = CARTESIAN_POINT ( 'NONE',  ( -7.069742149889169269, 41.66287055432060527, -69.58314084294495672 ) ) ;
#100513 = CIRCLE ( 'NONE', #9273, 4.000000000000000888 ) ;
#100515 = CARTESIAN_POINT ( 'NONE',  ( 31.81754536830298008, -42.95997511258514834, 34.45836456846625850 ) ) ;
#100514 = DIRECTION ( 'NONE',  ( -0.000000000000000000, 1.000000000000000000, -0.000000000000000000 ) ) ;
#100516 = CARTESIAN_POINT ( 'NONE',  ( -4.152276560052219345, 52.11353348511973849, -6.756903599530849291 ) ) ;
#100517 = ADVANCED_FACE ( 'NONE', ( #80990 ), #5006, .T. ) ;
#100518 = ORIENTED_EDGE ( 'NONE', *, *, #73734, .T. ) ;
#100519 = CARTESIAN_POINT ( 'NONE',  ( 0.000000000000000000, 0.000000000000000000, -3.852324522925831385 ) ) ;
#100520 = ORIENTED_EDGE ( 'NONE', *, *, #86784, .F. ) ;
#100521 = CARTESIAN_POINT ( 'NONE',  ( -26.02888215231238789, 34.91958502330739833, -9.463828569828224957 ) ) ;
#100522 = CARTESIAN_POINT ( 'NONE',  ( 18.31372175616277431, 302.6416072323730191, -10.04454203250753253 ) ) ;
#100523 = CARTESIAN_POINT ( 'NONE',  ( -44.19630675229384309, 485.6206890027647205, 3.558858865138833316 ) ) ;
#100524 = DIRECTION ( 'NONE',  ( 0.000000000000000000, -1.000000000000000000, 0.000000000000000000 ) ) ;
#100525 = CARTESIAN_POINT ( 'NONE',  ( 32.75517716563783921, 465.7432004789072266, 11.49884209862490358 ) ) ;
#100526 = CARTESIAN_POINT ( 'NONE',  ( -37.54237687662340051, 463.5961191364194178, 19.55587387183957304 ) ) ;
#100527 = ORIENTED_EDGE ( 'NONE', *, *, #33459, .T. ) ;
#100528 = CARTESIAN_POINT ( 'NONE',  ( 80.69099499396966735, -59.99999999999997868, -27.52696420757851214 ) ) ;
#100529 = DIRECTION ( 'NONE',  ( 1.000000000000000000, 1.224606353822377258E-16, 0.000000000000000000 ) ) ;
#100530 = CARTESIAN_POINT ( 'NONE',  ( 6.928203230275508773, -10.00000000000001066, -4.000000000000000000 ) ) ;
#100531 = CARTESIAN_POINT ( 'NONE',  ( -46.78679791479559213, 18.82552674760556144, -15.44534812371305144 ) ) ;
#100532 = ORIENTED_EDGE ( 'NONE', *, *, #8428, .F. ) ;
#100533 = EDGE_CURVE ( 'NONE', #45302, #49899, #104424, .T. ) ;
#100534 = AXIS2_PLACEMENT_3D ( 'NONE', #30358, #102095, #61124 ) ;
#100535 = CARTESIAN_POINT ( 'NONE',  ( -36.95390076149564607, 27.83275904791154431, 13.30708510620654472 ) ) ;
#100536 = EDGE_LOOP ( 'NONE', ( #21153, #13158, #79956, #75415, #99455, #83768, #15163, #94752 ) ) ;
#100537 = ORIENTED_EDGE ( 'NONE', *, *, #97157, .T. ) ;
#100538 = CARTESIAN_POINT ( 'NONE',  ( 7.002619243997875387, 83.94992681986181537, -3.868708944012998252 ) ) ;
#100539 = CARTESIAN_POINT ( 'NONE',  ( -16.75187969033531132, 34.25544727262101219, -24.30698433968676753 ) ) ;
#100540 = CARTESIAN_POINT ( 'NONE',  ( 10.00000000000000000, -15.00000000000000000, 10.00000000000000178 ) ) ;
#100541 = CARTESIAN_POINT ( 'NONE',  ( 83.23442963069594214, -37.80756990166215559, -8.243152359157335241 ) ) ;
#100542 = CARTESIAN_POINT ( 'NONE',  ( -33.37176405577542937, 315.0974072509098960, -7.071267840213817379 ) ) ;
#100543 = CARTESIAN_POINT ( 'NONE',  ( 0.000000000000000000, -50.00000000000000000, 119.0000000000000142 ) ) ;
#100544 = CARTESIAN_POINT ( 'NONE',  ( -18.23999450864831928, 45.00000000000000000, 62.43394949844228137 ) ) ;
#100545 = ORIENTED_EDGE ( 'NONE', *, *, #66819, .T. ) ;
#100546 = CARTESIAN_POINT ( 'NONE',  ( -48.02835407290516656, 16.78162100668608048, 14.35535821593516559 ) ) ;
#100547 = ORIENTED_EDGE ( 'NONE', *, *, #43845, .F. ) ;
#100548 = EDGE_CURVE ( 'NONE', #88217, #88418, #8030, .T. ) ;
#100549 = CARTESIAN_POINT ( 'NONE',  ( 9.686686328283677483, 51.27217407866643129, -3.328097068059955976 ) ) ;
#100550 = DIRECTION ( 'NONE',  ( 0.000000000000000000, 1.000000000000000000, -0.000000000000000000 ) ) ;
#100551 = MECHANICAL_DESIGN_GEOMETRIC_PRESENTATION_REPRESENTATION (  '', ( #36844 ), #43731 ) ;
#100553 = ORIENTED_EDGE ( 'NONE', *, *, #63596, .F. ) ;
#100552 = DIRECTION ( 'NONE',  ( -1.000000000000000000, 0.000000000000000000, 0.000000000000000000 ) ) ;
#100554 = CARTESIAN_POINT ( 'NONE',  ( 74.82255457991739434, -42.96157133918497095, 122.4742354992479108 ) ) ;
#100555 = EDGE_CURVE ( 'NONE', #31177, #37114, #83709, .T. ) ;
#100556 = AXIS2_PLACEMENT_3D ( 'NONE', #52856, #77135, #85783 ) ;
#100557 = EDGE_LOOP ( 'NONE', ( #42974, #23530, #8504, #100349 ) ) ;
#100558 = CARTESIAN_POINT ( 'NONE',  ( 3.905812579222632586, -52.93498169485550164, 40.44872036466767895 ) ) ;
#100559 = DIRECTION ( 'NONE',  ( 0.000000000000000000, 1.000000000000000000, 0.000000000000000000 ) ) ;
#100560 = STYLED_ITEM ( 'NONE', ( #99962 ), #53283 ) ;
#100561 = CARTESIAN_POINT ( 'NONE',  ( 7.188101187500000933, -26.56250000204838457, -2.977408999572650483 ) ) ;
#100562 = CARTESIAN_POINT ( 'NONE',  ( -96.68549010014578471, -57.67144976548149771, 46.95518404347522079 ) ) ;
#100563 = ADVANCED_FACE ( 'NONE', ( #104749, #55638 ), #95091, .F. ) ;
#100564 = ORIENTED_EDGE ( 'NONE', *, *, #80510, .F. ) ;
#100565 = DIRECTION ( 'NONE',  ( -0.000000000000000000, 1.000000000000000000, -0.000000000000000000 ) ) ;
#100566 = CARTESIAN_POINT ( 'NONE',  ( 104.8217955542264548, -52.71705407144827404, 181.7153123444907692 ) ) ;
#100567 = CARTESIAN_POINT ( 'NONE',  ( -36.47314689784992225, 28.20057725235767876, -11.57774245207459707 ) ) ;
#100568 = DIRECTION ( 'NONE',  ( 0.000000000000000000, -1.000000000000000000, 0.000000000000000000 ) ) ;
#100569 = CARTESIAN_POINT ( 'NONE',  ( 7.999999999999998224, -21.78125000409677980, 3.313708498984766493 ) ) ;
#100570 = CARTESIAN_POINT ( 'NONE',  ( -81.98196232622828461, -37.99999999999996447, -13.86369433938586582 ) ) ;
#100571 = DIRECTION ( 'NONE',  ( -1.000000000000000000, 0.000000000000000000, 0.000000000000000000 ) ) ;
#100572 = DIRECTION ( 'NONE',  ( 0.000000000000000000, -1.000000000000000000, 0.000000000000000000 ) ) ;
#100573 = ADVANCED_FACE ( 'NONE', ( #87522 ), #70798, .F. ) ;
#100574 = FILL_AREA_STYLE ('',( #59610 ) ) ;
#100575 = CARTESIAN_POINT ( 'NONE',  ( 8.331345277524542681, 0.000000000000000000, -7.381345277524544279 ) ) ;
#100577 = TOROIDAL_SURFACE ( 'NONE', #54055, 7.500000000000000888, 5.000000000000000000 ) ;
#100576 = DIRECTION ( 'NONE',  ( 1.000000000000000000, 0.000000000000000000, 0.000000000000000000 ) ) ;
#100578 = CARTESIAN_POINT ( 'NONE',  ( 27.33349330513380693, 4.898587196589411843E-16, -4.000000000000001776 ) ) ;
#100579 = ORIENTED_EDGE ( 'NONE', *, *, #10824, .F. ) ;
#100580 = CARTESIAN_POINT ( 'NONE',  ( 33.52307692307692122, 1.411358822780289120E-15, 0.000000000000000000 ) ) ;
#100581 = CARTESIAN_POINT ( 'NONE',  ( 0.000000000000000000, 6.123233995736770227E-16, -5.000000000000002665 ) ) ;
#100583 = CARTESIAN_POINT ( 'NONE',  ( 6.683837171061809634, -7.911893696991943337, -3.558927330633863411E-17 ) ) ;
#100582 =( BOUNDED_CURVE ( )  B_SPLINE_CURVE ( 2, ( #14657, #40546, #98250, #64310, #31947, #80991, #79935, #90162, #38971, #6045, #71844, #14133, #105807, #64828, #97707, #23872, #89637, #28248, #61670, #43857, #20710, #19099, #52470, #84852, #68690, #76748, #85391, #27184, #94560, #61118, #18547, #101030, #10420, #53548, #53017, #102087, #85942, #94007, #68136, #60075, #20168, #27727, #60600, #12012, #1788, #75689, #34745, #35810, #10935, #19637, #36350, #86479, #42797, #76215, #77829, #2322, #2856, #92398, #51411, #92937, #36870, #93488, #44945, #26653, #69738, #51939, #3407, #102631, #28788, #43334, #84323, #101569, #11471, #44399, #77296, #69220, #35266, #3938, #67617, #100495, #59530, #103689, #38446, #31426, #14650, #55116, #4463, #62202, #88046, #64301, #78343, #71312, #23320, #5523, #45993, #29833, #63774, #97173, #105280, #47027, #12535, #22797, #96662, #95601, #56159, #13598, #39500, #55632, #104206, #88569, #103168, #72374, #62710, #79929, #6566, #45471, #86994, #95087, #87517, #54578, #14126, #37404, #47560, #63242, #70265, #6038, #29311, #5001, #21741, #30350, #21219, #80455, #38963, #54049, #13064, #71837, #78872, #37932, #96134, #70793, #22268, #46511, #79408, #104743, #30895, #42130, #41609, #24398, #99291, #66407, #65353, #99837, #90155, #9222, #33535, #25467, #1111, #98243, #16260, #49690, #74492, #50226, #41, #16804, #83127, #98760, #41076, #58319, #48616, #105800, #8170, #64821, #91245, #17352, #81501, #82597, #15732, #15195, #75016, #72889, #80986, #73961, #34086, #66958, #31939, #56709, #89631, #97700, #567, #26009, #49145, #89101, #48086, #7102, #7621, #40017, #82048, #23864, #40539, #57768, #73421, #106316, #32480, #57237, #33013, #65880, #24914, #90696, #8701, #84197, #10293, #77168, #101445, #43730, #76620, #101963, #17881, #91762, #50735, #51814, #100894 ),
 .UNSPECIFIED., .F., .F. ) 
 B_SPLINE_CURVE_WITH_KNOTS ( ( 3, 2, 2, 2, 2, 2, 2, 2, 2, 2, 2, 2, 2, 2, 2, 2, 2, 2, 2, 2, 2, 2, 2, 2, 2, 2, 2, 2, 2, 2, 2, 2, 2, 2, 2, 2, 2, 2, 2, 2, 2, 2, 2, 2, 2, 2, 2, 2, 2, 2, 2, 2, 2, 2, 2, 2, 2, 2, 2, 2, 2, 2, 2, 2, 2, 2, 2, 2, 2, 2, 2, 2, 2, 2, 2, 2, 2, 2, 2, 2, 2, 2, 2, 2, 2, 2, 2, 2, 2, 2, 2, 2, 2, 2, 2, 2, 2, 2, 2, 2, 2, 2, 2, 2, 2, 2, 2, 2, 2, 2, 3 ),
 ( 0.1777496976123880690, 0.1838235294117647189, 0.1911764705882352811, 0.1985294117647058709, 0.2058823529411764608, 0.2132352941176470507, 0.2205882352941176405, 0.2279411764705882304, 0.2352941176470588203, 0.2426470588235294101, 0.2500000000000000000, 0.2573529411764705621, 0.2647058823529411797, 0.2720588235294117418, 0.2794117647058823595, 0.2867647058823529216, 0.2941176470588235392, 0.3014705882352941013, 0.3088235294117647189, 0.3161764705882352811, 0.3235294117647058987, 0.3308823529411764608, 0.3382352941176470784, 0.3455882352941176405, 0.3529411764705882582, 0.3602941176470588203, 0.3676470588235294379, 0.3750000000000000000, 0.3823529411764705621, 0.3897058823529412352, 0.3970588235294117418, 0.4044117647058823595, 0.4117647058823529216, 0.4191176470588234837, 0.4264705882352941013, 0.4338235294117647189, 0.4411764705882352811, 0.4485294117647058987, 0.4558823529411764608, 0.4632352941176470784, 0.4705882352941176405, 0.4779411764705882582, 0.4852941176470588203, 0.4926470588235294379, 0.5000000000000000000, 0.5073529411764705621, 0.5147058823529411242, 0.5220588235294117974, 0.5294117647058823595, 0.5367647058823529216, 0.5441176470588233727, 0.5514705882352941568, 0.5588235294117647189, 0.5661764705882352811, 0.5735294117647058432, 0.5808823529411765163, 0.5882352941176470784, 0.5955882352941176405, 0.6029411764705882026, 0.6102941176470588758, 0.6176470588235294379, 0.6250000000000000000, 0.6323529411764705621, 0.6397058823529411242, 0.6470588235294117974, 0.6544117647058823595, 0.6617647058823529216, 0.6691176470588233727, 0.6764705882352941568, 0.6838235294117647189, 0.6911764705882352811, 0.6985294117647058432, 0.7058823529411764053, 0.7132352941176469674, 0.7205882352941175295, 0.7279411764705880916, 0.7352941176470588758, 0.7426470588235294379, 0.7500000000000000000, 0.7573529411764705621, 0.7647058823529411242, 0.7720588235294116863, 0.7794117647058822484, 0.7867647058823528106, 0.7941176470588233727, 0.8014705882352941568, 0.8088235294117647189, 0.8161764705882352811, 0.8235294117647058432, 0.8308823529411764053, 0.8382352941176469674, 0.8455882352941175295, 0.8529411764705880916, 0.8602941176470588758, 0.8676470588235294379, 0.8750000000000000000, 0.8823529411764705621, 0.8897058823529411242, 0.8970588235294116863, 0.9044117647058822484, 0.9117647058823528106, 0.9191176470588233727, 0.9264705882352943789, 0.9338235294117647189, 0.9411764705882352811, 0.9485294117647058432, 0.9558823529411764053, 0.9632352941176471894, 0.9705882352941175295, 0.9779411764705880916, 0.9804062476879973342 ),
 .UNSPECIFIED. ) 
 CURVE ( )  GEOMETRIC_REPRESENTATION_ITEM ( )  RATIONAL_B_SPLINE_CURVE ( ( 0.9781234062028234533, 0.9371213634217746558, 1.000000000000000000, 0.9238795325112867385, 1.000000000000000000, 0.9238795325112867385, 1.000000000000000000, 0.9238795325112867385, 1.000000000000000000, 0.9238795325112867385, 1.000000000000000000, 0.9238795325112867385, 1.000000000000000000, 0.9238795325112867385, 1.000000000000000000, 0.9238795325112867385, 1.000000000000000000, 0.9238795325112867385, 1.000000000000000000, 0.9238795325112867385, 1.000000000000000000, 0.9238795325112867385, 1.000000000000000000, 0.9238795325112867385, 1.000000000000000000, 0.9238795325112867385, 1.000000000000000000, 0.9238795325112867385, 1.000000000000000000, 0.9238795325112867385, 1.000000000000000000, 0.9238795325112867385, 1.000000000000000000, 0.9238795325112867385, 1.000000000000000000, 0.9238795325112867385, 1.000000000000000000, 0.9238795325112867385, 1.000000000000000000, 0.9238795325112867385, 1.000000000000000000, 0.9238795325112867385, 1.000000000000000000, 0.9238795325112867385, 1.000000000000000000, 0.9238795325112867385, 1.000000000000000000, 0.9238795325112867385, 1.000000000000000000, 0.9238795325112867385, 1.000000000000000000, 0.9238795325112867385, 1.000000000000000000, 0.9238795325112867385, 1.000000000000000000, 0.9238795325112867385, 1.000000000000000000, 0.9238795325112867385, 1.000000000000000000, 0.9238795325112867385, 1.000000000000000000, 0.9238795325112867385, 1.000000000000000000, 0.9238795325112867385, 1.000000000000000000, 0.9238795325112867385, 1.000000000000000000, 0.9238795325112867385, 1.000000000000000000, 0.9238795325112867385, 1.000000000000000000, 0.9238795325112867385, 1.000000000000000000, 0.9238795325112867385, 1.000000000000000000, 0.9238795325112867385, 1.000000000000000000, 0.9238795325112867385, 1.000000000000000000, 0.9238795325112867385, 1.000000000000000000, 0.9238795325112867385, 1.000000000000000000, 0.9238795325112867385, 1.000000000000000000, 0.9238795325112867385, 1.000000000000000000, 0.9238795325112867385, 1.000000000000000000, 0.9238795325112867385, 1.000000000000000000, 0.9238795325112867385, 1.000000000000000000, 0.9238795325112867385, 1.000000000000000000, 0.9238795325112867385, 1.000000000000000000, 0.9238795325112867385, 1.000000000000000000, 0.9238795325112867385, 1.000000000000000000, 0.9238795325112867385, 1.000000000000000000, 0.9238795325112867385, 1.000000000000000000, 0.9238795325112867385, 1.000000000000000000, 0.9238795325112867385, 1.000000000000000000, 0.9238795325112867385, 1.000000000000000000, 0.9238795325112867385, 1.000000000000000000, 0.9238795325112867385, 1.000000000000000000, 0.9238795325112867385, 1.000000000000000000, 0.9238795325112867385, 1.000000000000000000, 0.9238795325112867385, 1.000000000000000000, 0.9238795325112867385, 1.000000000000000000, 0.9238795325112867385, 1.000000000000000000, 0.9238795325112867385, 1.000000000000000000, 0.9238795325112867385, 1.000000000000000000, 0.9238795325112867385, 1.000000000000000000, 0.9238795325112867385, 1.000000000000000000, 0.9238795325112867385, 1.000000000000000000, 0.9238795325112867385, 1.000000000000000000, 0.9238795325112867385, 1.000000000000000000, 0.9238795325112867385, 1.000000000000000000, 0.9238795325112867385, 1.000000000000000000, 0.9238795325112867385, 1.000000000000000000, 0.9238795325112867385, 1.000000000000000000, 0.9238795325112867385, 1.000000000000000000, 0.9238795325112867385, 1.000000000000000000, 0.9238795325112867385, 1.000000000000000000, 0.9238795325112867385, 1.000000000000000000, 0.9238795325112867385, 1.000000000000000000, 0.9238795325112867385, 1.000000000000000000, 0.9238795325112867385, 1.000000000000000000, 0.9238795325112867385, 1.000000000000000000, 0.9238795325112867385, 1.000000000000000000, 0.9238795325112867385, 1.000000000000000000, 0.9238795325112867385, 1.000000000000000000, 0.9238795325112867385, 1.000000000000000000, 0.9238795325112867385, 1.000000000000000000, 0.9238795325112867385, 1.000000000000000000, 0.9238795325112867385, 1.000000000000000000, 0.9238795325112867385, 1.000000000000000000, 0.9238795325112867385, 1.000000000000000000, 0.9238795325112867385, 1.000000000000000000, 0.9238795325112867385, 1.000000000000000000, 0.9238795325112867385, 1.000000000000000000, 0.9238795325112867385, 1.000000000000000000, 0.9238795325112867385, 1.000000000000000000, 0.9238795325112867385, 1.000000000000000000, 0.9238795325112867385, 1.000000000000000000, 0.9238795325112867385, 1.000000000000000000, 0.9238795325112867385, 1.000000000000000000, 0.9238795325112867385, 1.000000000000000000, 0.9238795325112867385, 1.000000000000000000, 0.9238795325112867385, 1.000000000000000000, 0.9238795325112867385, 1.000000000000000000, 0.9238795325112867385, 1.000000000000000000, 0.9238795325112867385, 1.000000000000000000, 0.9238795325112867385, 1.000000000000000000, 0.9238795325112867385, 1.000000000000000000, 0.9238795325112867385, 1.000000000000000000, 0.9238795325112867385, 1.000000000000000000, 0.9744806372091472380, 0.9660719911213342392 ) ) 
 REPRESENTATION_ITEM ( '' )  );
#100584 = CARTESIAN_POINT ( 'NONE',  ( -85.49552939016024311, -30.00000000000000000, 174.7863823751660846 ) ) ;
#100585 = EDGE_CURVE ( 'NONE', #58214, #13401, #69761, .T. ) ;
#100586 = EDGE_LOOP ( 'NONE', ( #64932, #22099, #75875, #99881 ) ) ;
#100587 = CARTESIAN_POINT ( 'NONE',  ( 38.81815223091233946, 25.18283608031790877, -12.26568976353609131 ) ) ;
#100588 = CARTESIAN_POINT ( 'NONE',  ( 70.14605380316399419, -57.68253419882464073, 155.2985699437752771 ) ) ;
#100590 = DIRECTION ( 'NONE',  ( -1.000000000000000000, -1.224606353822377258E-16, -0.000000000000000000 ) ) ;
#100589 = FILL_AREA_STYLE ('',( #91971 ) ) ;
#100591 = EDGE_CURVE ( 'NONE', #22641, #4198, #68249, .T. ) ;
#100592 = CARTESIAN_POINT ( 'NONE',  ( 29.61882069994729960, -29.43158534365355550, -38.19371325218018853 ) ) ;
#100593 = CARTESIAN_POINT ( 'NONE',  ( -14.29190075644683589, 21.26710225492821138, -5.626279437300707897 ) ) ;
#100594 = FACE_OUTER_BOUND ( 'NONE', #100220, .T. ) ;
#100595 = CARTESIAN_POINT ( 'NONE',  ( -37.39234250541336024, -60.00000000000002132, 48.78642601381413613 ) ) ;
#100596 = B_SPLINE_CURVE_WITH_KNOTS ( 'NONE', 3,
 ( #82821, #25699, #32160, #83347, #106015, #8919, #49372, #32706 ),
 .UNSPECIFIED., .F., .F.,
 ( 4, 2, 2, 4 ),
 ( 0.006061689441712471600, 0.007174127271521696381, 0.008286565101330922029, 0.01051144076094937159 ),
 .UNSPECIFIED. ) ;
#100597 = CARTESIAN_POINT ( 'NONE',  ( -33.00000000000000000, 461.8887775513397855, 11.55279652844097171 ) ) ;
#100598 = CARTESIAN_POINT ( 'NONE',  ( 23.38163988261896620, 48.00000000000000000, 60.94087333798638895 ) ) ;
#100599 = CARTESIAN_POINT ( 'NONE',  ( -86.76683669320412662, -35.44260230858979099, 187.6259941901972752 ) ) ;
#100600 = ORIENTED_EDGE ( 'NONE', *, *, #76419, .T. ) ;
#100601 = CARTESIAN_POINT ( 'NONE',  ( 30.82452621380425484, 13.29951192218422484, 41.36733700123890145 ) ) ;
#100602 = CARTESIAN_POINT ( 'NONE',  ( -4.032884956273577792, -35.99424295969529197, 29.88149843471951073 ) ) ;
#100603 = SURFACE_STYLE_USAGE ( .BOTH. , #33774 ) ;
#100604 = CARTESIAN_POINT ( 'NONE',  ( -37.45944760690750286, 486.5144608516062590, 13.75040320519661918 ) ) ;
#100605 = B_SPLINE_SURFACE_WITH_KNOTS ( 'NONE', 1, 3, ( 
 ( #65324, #96635, #105773, #98212, #22770, #24365, #105254, #71812, #49115, #73930, #57209, #16229, #32980, #72351, #63748, #14097, #47004, #31401, #59914, #27030, #83097, #92235, #50703, #26502, #100338, #540, #83616, #58287 ),
 ( #34053, #84697, #91732, #66377, #10264, #76059, #99807, #43178, #18389, #66927, #51242, #34589, #9190, #99257, #25978, #35114, #25433, #91213, #59373, #49659, #74460, #10781, #84169, #17851, #9720, #18941, #68529, #51784 ) ),
 .UNSPECIFIED., .F., .F., .F.,
 ( 2, 2 ),
 ( 4, 2, 2, 2, 2, 2, 2, 2, 2, 2, 2, 2, 2, 4 ),
 ( 0.000000000000000000, 1.000000000000000000 ),
 ( 0.08901491201581737678, 0.1032490540155679704, 0.1174831960153185778, 0.1317173380150691853, 0.1459514800148197788, 0.1744197640143299588, 0.2028880480138401388, 0.2598246160128514504, 0.3167611840118632616, 0.4306343200098861623, 0.5445074560079088410, 0.6583805920059359051, 0.7722537280039543095, 1.000000000000000000 ),
 .UNSPECIFIED. ) ;
#100607 = CARTESIAN_POINT ( 'NONE',  ( 5.413543642048970206, -66.62195522163649741, 14.08876852576774041 ) ) ;
#100606 = CARTESIAN_POINT ( 'NONE',  ( 33.77559172535807619, 464.7834715296606305, 7.192701217093271815 ) ) ;
#100608 = ORIENTED_EDGE ( 'NONE', *, *, #21037, .F. ) ;
#100609 = AXIS2_PLACEMENT_3D ( 'NONE', #10042, #75840, #34888 ) ;
#100610 = CARTESIAN_POINT ( 'NONE',  ( 0.7771955416098277336, 28.10628302878886586, 38.51754525846273225 ) ) ;
#100611 = CARTESIAN_POINT ( 'NONE',  ( 0.000000000000000000, 0.000000000000000000, 0.000000000000000000 ) ) ;
#100612 = CARTESIAN_POINT ( 'NONE',  ( 25.75971285069983807, 304.3014513131341801, -9.684463734016926395 ) ) ;
#100613 = CARTESIAN_POINT ( 'NONE',  ( 35.66932529116966322, 438.9565575286536045, 4.011496722538590909 ) ) ;
#100614 = SURFACE_STYLE_FILL_AREA ( #83900 ) ;
#100615 = CARTESIAN_POINT ( 'NONE',  ( 0.000000000000000000, 0.000000000000000000, 0.000000000000000000 ) ) ;
#100616 = CARTESIAN_POINT ( 'NONE',  ( 114.4011996162234510, -59.99999999999997158, 179.2244502532067827 ) ) ;
#100617 = CARTESIAN_POINT ( 'NONE',  ( -80.62560537530049487, -46.44214533936248301, 158.8984127742610895 ) ) ;
#100618 = CONICAL_SURFACE ( 'NONE', #73037, 5.000000000000010658, 0.9599310885968697082 ) ;
#100619 = ORIENTED_EDGE ( 'NONE', *, *, #74834, .F. ) ;
#100620 = LINE ( 'NONE', #26256, #34383 ) ;
#100621 = CARTESIAN_POINT ( 'NONE',  ( 4.903871675326597845, 252.0208580730149492, -3.461400506969868118 ) ) ;
#100622 = CARTESIAN_POINT ( 'NONE',  ( 24.28208867544860183, -57.67420315891946103, 43.01449209020211839 ) ) ;
#100623 = PRESENTATION_LAYER_ASSIGNMENT (  '', '', ( #90312 ) ) ;
#100624 = CARTESIAN_POINT ( 'NONE',  ( 6.289692432696785573, -1.240526984323783911E-13, -6.828989928337169779 ) ) ;
#100625 = CARTESIAN_POINT ( 'NONE',  ( 4.086341046824178314, 13.71216495598962304, -5.000000000000001776 ) ) ;
#100626 = FACE_OUTER_BOUND ( 'NONE', #100848, .T. ) ;
#100627 = ORIENTED_EDGE ( 'NONE', *, *, #106679, .F. ) ;
#100628 = CIRCLE ( 'NONE', #54113, 4.000000000000007105 ) ;
#100629 = CARTESIAN_POINT ( 'NONE',  ( 31.09389865030000522, 439.4630943131195977, 22.89591944113354316 ) ) ;
#100630 = ORIENTED_EDGE ( 'NONE', *, *, #52910, .T. ) ;
#100631 = SURFACE_STYLE_FILL_AREA ( #102234 ) ;
#100632 = DIRECTION ( 'NONE',  ( 1.224646799147353207E-16, 1.000000000000000000, 0.000000000000000000 ) ) ;
#100633 = CARTESIAN_POINT ( 'NONE',  ( 0.000000000000000000, 50.50000000000000000, 0.000000000000000000 ) ) ;
#100634 = EDGE_CURVE ( 'NONE', #68832, #90588, #42134, .T. ) ;
#100635 = CARTESIAN_POINT ( 'NONE',  ( -5.957442974701830707, 49.99999999999999289, 65.00000000000000000 ) ) ;
#100636 = CARTESIAN_POINT ( 'NONE',  ( 5.000000000000000000, -13.87446176118116448, 11.25142367426022538 ) ) ;
#100637 = CARTESIAN_POINT ( 'NONE',  ( 0.000000000000000000, 0.000000000000000000, 0.000000000000000000 ) ) ;
#100638 = ORIENTED_EDGE ( 'NONE', *, *, #48782, .F. ) ;
#100639 = CARTESIAN_POINT ( 'NONE',  ( 98.70648322990193435, -59.99999999999998579, 202.2230572402837367 ) ) ;
#100641 = CARTESIAN_POINT ( 'NONE',  ( 24.11997513724847408, -53.39263269948676083, 33.93311544977419913 ) ) ;
#100640 = CARTESIAN_POINT ( 'NONE',  ( -88.35884389454342625, -14.21045842199434794, 197.0605769606054594 ) ) ;
#100642 = UNCERTAINTY_MEASURE_WITH_UNIT (LENGTH_MEASURE( 1.000000000000000082E-05 ), #62140, 'distance_accuracy_value', 'NONE');
#100644 = EDGE_CURVE ( 'NONE', #16368, #40837, #99842, .T. ) ;
#100643 = CARTESIAN_POINT ( 'NONE',  ( 37.67793878171265476, 380.9275077484064127, 5.379687045508362964 ) ) ;
#100645 = CARTESIAN_POINT ( 'NONE',  ( -43.76208095016959732, -32.61856360751036021, 40.47694461062264537 ) ) ;
#100646 = CARTESIAN_POINT ( 'NONE',  ( 11.36650669486618881, 4.000000000000003553, 4.898587196589414801E-16 ) ) ;
#100647 = UNCERTAINTY_MEASURE_WITH_UNIT (LENGTH_MEASURE( 1.000000000000000082E-05 ), #64892, 'distance_accuracy_value', 'NONE');
#100648 = ORIENTED_EDGE ( 'NONE', *, *, #100290, .T. ) ;
#100649 = CARTESIAN_POINT ( 'NONE',  ( -46.00000000000000000, 461.6622277975411635, 10.18145404766348783 ) ) ;
#100650 = CARTESIAN_POINT ( 'NONE',  ( -13.87298779988979724, -57.59168965358072256, 28.89736879381397827 ) ) ;
#100651 = CARTESIAN_POINT ( 'NONE',  ( 91.09088295274877112, 1.030564683017419500E-14, 0.000000000000000000 ) ) ;
#100652 = CARTESIAN_POINT ( 'NONE',  ( 5.819846122303830249, 4.937269551422740044, 4.448398286273013369 ) ) ;
#100653 = CARTESIAN_POINT ( 'NONE',  ( -37.87024700625071461, 460.2236392396199562, 2.222911568036097574 ) ) ;
#100654 = ORIENTED_EDGE ( 'NONE', *, *, #84286, .F. ) ;
#100655 = CARTESIAN_POINT ( 'NONE',  ( -16.11359103326322995, 37.20915759416860880, -21.97891983235047775 ) ) ;
#100656 = EDGE_LOOP ( 'NONE', ( #36607, #6561, #98203, #7663, #94498 ) ) ;
#100657 = CARTESIAN_POINT ( 'NONE',  ( 76.63262662268121517, -30.00000000002306422, 171.6915798261921395 ) ) ;
#100658 = CARTESIAN_POINT ( 'NONE',  ( 42.22882555519233705, 39.53072919842792743, -49.99044811816536793 ) ) ;
#100659 = AXIS2_PLACEMENT_3D ( 'NONE', #84664, #85190, #43663 ) ;
#100660 = CARTESIAN_POINT ( 'NONE',  ( 23.97884343762943615, 25.74916088538413561, -30.95222414396502941 ) ) ;
#100661 = CARTESIAN_POINT ( 'NONE',  ( 84.07723708129948648, -30.00000000000000000, 51.17427913239208692 ) ) ;
#100662 = AXIS2_PLACEMENT_3D ( 'NONE', #93950, #54513, #20104 ) ;
#100663 = FACE_OUTER_BOUND ( 'NONE', #96527, .T. ) ;
#100664 = VERTEX_POINT ( 'NONE', #89636 ) ;
#100665 = EDGE_CURVE ( 'NONE', #17408, #68006, #47952, .T. ) ;
#100666 = AXIS2_PLACEMENT_3D ( 'NONE', #46333, #79219, #35355 ) ;
#100667 = AXIS2_PLACEMENT_3D ( 'NONE', #69010, #34003, #101885 ) ;
#100668 = ORIENTED_EDGE ( 'NONE', *, *, #104609, .T. ) ;
#100669 = ORIENTED_EDGE ( 'NONE', *, *, #39369, .F. ) ;
#100670 = CARTESIAN_POINT ( 'NONE',  ( -32.66167952489984572, 465.7843590037688273, 12.50185730157783048 ) ) ;
#100671 = DIRECTION ( 'NONE',  ( 0.000000000000000000, 0.000000000000000000, -1.000000000000000000 ) ) ;
#100672 = CARTESIAN_POINT ( 'NONE',  ( 5.856955515201468288, -13.78289058880865525, 1.326217528971456838 ) ) ;
#100673 = CARTESIAN_POINT ( 'NONE',  ( -32.09613050731442030, 439.8910643262784674, 23.54880513615299620 ) ) ;
#100674 = ORIENTED_EDGE ( 'NONE', *, *, #35352, .F. ) ;
#100675 = CARTESIAN_POINT ( 'NONE',  ( -8.737863884120026015, 49.99999999999999289, -79.96381019768847409 ) ) ;
#100676 = ORIENTED_EDGE ( 'NONE', *, *, #33140, .F. ) ;
#100677 = DIRECTION ( 'NONE',  ( 0.000000000000000000, 0.000000000000000000, -1.000000000000000000 ) ) ;
#100678 = CARTESIAN_POINT ( 'NONE',  ( 76.58278636061123734, -38.42162667129784381, 182.2336444325641480 ) ) ;
#100679 = CARTESIAN_POINT ( 'NONE',  ( 0.000000000000000000, 47.77514352166374323, -11.96035173608223090 ) ) ;
#100680 = CARTESIAN_POINT ( 'NONE',  ( 31.09148700014130640, 299.3363133847115591, 10.94160789497410313 ) ) ;
#100681 = CARTESIAN_POINT ( 'NONE',  ( -4.521127550501226722, 249.3238975947233200, 3.944701057164360147 ) ) ;
#100682 = ORIENTED_EDGE ( 'NONE', *, *, #93426, .T. ) ;
#100683 = FACE_OUTER_BOUND ( 'NONE', #72887, .T. ) ;
#100684 = CARTESIAN_POINT ( 'NONE',  ( 37.28010227714514002, 307.7308894357594795, 4.972761938079513833 ) ) ;
#100685 = CARTESIAN_POINT ( 'NONE',  ( 63.81650669486618455, 6.856755485862130937E-15, 0.000000000000000000 ) ) ;
#100686 = CARTESIAN_POINT ( 'NONE',  ( 15.47474416541426478, 2.749750016660005958, -1.674624973602916178 ) ) ;
#100687 = ORIENTED_EDGE ( 'NONE', *, *, #25730, .F. ) ;
#100688 = FACE_OUTER_BOUND ( 'NONE', #46151, .T. ) ;
#100689 = CARTESIAN_POINT ( 'NONE',  ( 9.118906730430985774E-15, 30.00000000000000000, -74.46152422706630603 ) ) ;
#100690 = DIRECTION ( 'NONE',  ( 0.000000000000000000, 0.000000000000000000, -1.000000000000000000 ) ) ;
#100691 = CARTESIAN_POINT ( 'NONE',  ( 2.503172993490694775, 294.8391969675017208, 9.934319915356635278 ) ) ;
#100692 = FILL_AREA_STYLE ('',( #83988 ) ) ;
#100693 = ORIENTED_EDGE ( 'NONE', *, *, #44045, .F. ) ;
#100694 = VECTOR ( 'NONE', #75203, 1000.000000000000227 ) ;
#100695 = FACE_OUTER_BOUND ( 'NONE', #86344, .T. ) ;
#100696 = CARTESIAN_POINT ( 'NONE',  ( 84.81970466459384284, -50.19123916470319813, 188.8545982504039102 ) ) ;
#100697 = VECTOR ( 'NONE', #3552, 1000.000000000000227 ) ;
#100698 = B_SPLINE_CURVE_WITH_KNOTS ( 'NONE', 3,
 ( #33678, #22939, #97850, #81132, #72515, #40149 ),
 .UNSPECIFIED., .F., .F.,
 ( 4, 2, 4 ),
 ( 0.000000000000000000, 0.001995463903526792284, 0.003990927807053584568 ),
 .UNSPECIFIED. ) ;
#100699 = SURFACE_SIDE_STYLE ('',( #26342 ) ) ;
#100700 = CARTESIAN_POINT ( 'NONE',  ( -7.844366129626889617, 79.51894426619178091, 0.000000000000000000 ) ) ;
#100701 = VERTEX_POINT ( 'NONE', #66963 ) ;
#100702 = VECTOR ( 'NONE', #101463, 1000.000000000000000 ) ;
#100703 = CARTESIAN_POINT ( 'NONE',  ( -72.50181434431193850, -38.00000000001091394, -21.26203725901419261 ) ) ;
#100704 = DIRECTION ( 'NONE',  ( -1.000000000000000000, -0.000000000000000000, -0.000000000000000000 ) ) ;
#100705 = DIRECTION ( 'NONE',  ( 0.000000000000000000, -1.000000000000000000, 0.000000000000000000 ) ) ;
#100706 = MECHANICAL_DESIGN_GEOMETRIC_PRESENTATION_REPRESENTATION (  '', ( #85236 ), #7694 ) ;
#100707 = CARTESIAN_POINT ( 'NONE',  ( -90.16919950005070916, -30.00000000000000000, 89.48266059237039372 ) ) ;
#100708 = EDGE_CURVE ( 'NONE', #29666, #76811, #105851, .T. ) ;
#100709 = B_SPLINE_CURVE_WITH_KNOTS ( 'NONE', 3,
 ( #103272, #7593, #29422, #40511, #7074, #89074, #53651, #70902 ),
 .UNSPECIFIED., .F., .F.,
 ( 4, 2, 2, 4 ),
 ( 0.000000000000000000, 0.4019822150283983153, 0.6029733225425960574, 0.8039644300567937441 ),
 .UNSPECIFIED. ) ;
#100710 = ADVANCED_FACE ( 'NONE', ( #106320 ), #34091, .T. ) ;
#100711 =( NAMED_UNIT ( * ) SI_UNIT ( $, .STERADIAN. ) SOLID_ANGLE_UNIT ( ) );
#100712 = CARTESIAN_POINT ( 'NONE',  ( 22.88454736421187263, 28.18015032983889867, -30.73969532942466998 ) ) ;
#100713 = CARTESIAN_POINT ( 'NONE',  ( -9.000000000000001776, 0.000000000000000000, 42.58845726811989607 ) ) ;
#100714 = EDGE_CURVE ( 'NONE', #18144, #14145, #97482, .T. ) ;
#100716 = FACE_BOUND ( 'NONE', #105052, .T. ) ;
#100715 = CARTESIAN_POINT ( 'NONE',  ( -9.989285784994832440, 246.0265757255429264, 0.5301777604595956372 ) ) ;
#100717 = EDGE_CURVE ( 'NONE', #34395, #77744, #91726, .T. ) ;
#100718 = CARTESIAN_POINT ( 'NONE',  ( 2.622924477838863844, -53.64565257674880172, 40.75381538023534489 ) ) ;
#100719 = CARTESIAN_POINT ( 'NONE',  ( 0.000000000000000000, 294.8518027762758038, -10.00000000000000178 ) ) ;
#100720 = CARTESIAN_POINT ( 'NONE',  ( 71.14984002819953446, -1.232595164407830946E-29, 4.000000000000007105 ) ) ;
#100721 = DIRECTION ( 'NONE',  ( 0.5735764363510554853, 0.8191520442889852482, 0.000000000000000000 ) ) ;
#100722 = CARTESIAN_POINT ( 'NONE',  ( 0.4037800551813753858, -7.199367570657607907, -0.5303295852573132185 ) ) ;
#100723 = CARTESIAN_POINT ( 'NONE',  ( 40.40045996829983466, -24.98508198468909924, -30.21120896785051002 ) ) ;
#100724 = CARTESIAN_POINT ( 'NONE',  ( -26.43713145984708746, -32.52648158339238904, 30.88029666580395727 ) ) ;
#100725 = EDGE_CURVE ( 'NONE', #27254, #72783, #35638, .T. ) ;
#100726 = VERTEX_POINT ( 'NONE', #57241 ) ;
#100727 = CARTESIAN_POINT ( 'NONE',  ( 5.887588022526042408, 11.68950459799316910, -3.788193301707003080 ) ) ;
#100728 = CARTESIAN_POINT ( 'NONE',  ( -9.253583916535172094, 106.2980390800503301, 3.792462592445557501 ) ) ;
#100729 = CARTESIAN_POINT ( 'NONE',  ( -17.02355309802323191, -53.40205467437851894, 33.05030794773703207 ) ) ;
#100730 = CARTESIAN_POINT ( 'NONE',  ( -63.60144037357603963, -29.63473796242592684, -23.63298369914019759 ) ) ;
#100731 = CIRCLE ( 'NONE', #99019, 3.000000000000009326 ) ;
#100733 = CARTESIAN_POINT ( 'NONE',  ( -69.08272651081071558, -34.58952494725262738, -22.16738816901018438 ) ) ;
#100732 = CYLINDRICAL_SURFACE ( 'NONE', #55126, 4.000000000000000000 ) ;
#100734 = PRODUCT_DEFINITION_FORMATION_WITH_SPECIFIED_SOURCE ( 'ANY', '', #11294, .NOT_KNOWN. ) ;
#100735 = ORIENTED_EDGE ( 'NONE', *, *, #83369, .T. ) ;
#100736 = DIRECTION ( 'NONE',  ( -0.000000000000000000, -0.000000000000000000, -1.000000000000000000 ) ) ;
#100737 = ORIENTED_EDGE ( 'NONE', *, *, #78028, .T. ) ;
#100738 = DIRECTION ( 'NONE',  ( 1.000000000000000000, 0.000000000000000000, 0.000000000000000000 ) ) ;
#100739 = CARTESIAN_POINT ( 'NONE',  ( -3.313708498984741180, -24.21875000409677625, -8.000000000000019540 ) ) ;
#100740 = VERTEX_POINT ( 'NONE', #49697 ) ;
#100741 = CARTESIAN_POINT ( 'NONE',  ( -7.350202751404733448, 54.21988909062471862, -3.137162962828702106 ) ) ;
#100742 = CARTESIAN_POINT ( 'NONE',  ( 98.76119375271832723, -37.78714592256793736, 192.0742751786086160 ) ) ;
#100744 = CARTESIAN_POINT ( 'NONE',  ( -16.64348903516521005, -1.200000000000000030E-05, -6.657797401561535544 ) ) ;
#100743 = CARTESIAN_POINT ( 'NONE',  ( 9.797174393178825657E-16, -30.00000000000000000, -8.000000000000000000 ) ) ;
#100745 = ORIENTED_EDGE ( 'NONE', *, *, #58533, .F. ) ;
#100746 = EDGE_LOOP ( 'NONE', ( #24195, #46472, #75608, #43509 ) ) ;
#100747 = ORIENTED_EDGE ( 'NONE', *, *, #39491, .T. ) ;
#100748 = CARTESIAN_POINT ( 'NONE',  ( 26.96142313735197504, 312.0022853774228793, 11.65857948192350335 ) ) ;
#100749 = CARTESIAN_POINT ( 'NONE',  ( -38.96902200852884590, 460.8405016383454722, 2.186950304199872352 ) ) ;
#100750 = CARTESIAN_POINT ( 'NONE',  ( 62.33904886068935980, 4.000000000000014211, 0.000000000000000000 ) ) ;
#100751 = EDGE_LOOP ( 'NONE', ( #48730, #62439, #61801, #24, #78275 ) ) ;
#100752 = EDGE_CURVE ( 'NONE', #18822, #40695, #9757, .T. ) ;
#100753 = CARTESIAN_POINT ( 'NONE',  ( 41.36650669486618881, 1.474610560812782335E-15, 0.000000000000000000 ) ) ;
#100754 = DIRECTION ( 'NONE',  ( 0.000000000000000000, 1.000000000000000000, 0.000000000000000000 ) ) ;
#100755 = CARTESIAN_POINT ( 'NONE',  ( -94.23463998755006799, -59.99999999999511147, 9.458815458491475425 ) ) ;
#100756 = CARTESIAN_POINT ( 'NONE',  ( 5.699988423468466792, 4.591578518468243608, -6.344710093416083829 ) ) ;
#100757 = CARTESIAN_POINT ( 'NONE',  ( -35.66932529116966322, 438.9565575286536045, 4.011496722538590909 ) ) ;
#100758 = CARTESIAN_POINT ( 'NONE',  ( -7.040774328009894667, 41.35742559143615438, -58.68913211047703982 ) ) ;
#100759 = AXIS2_PLACEMENT_3D ( 'NONE', #5814, #30117, #47331 ) ;
#100760 = CARTESIAN_POINT ( 'NONE',  ( -90.56108803656626094, -30.00000000000000711, 34.47189148671483849 ) ) ;
#100761 = EDGE_CURVE ( 'NONE', #39668, #77688, #73966, .T. ) ;
#100763 = ADVANCED_FACE ( 'NONE', ( #90161 ), #4697, .F. ) ;
#100762 = DIRECTION ( 'NONE',  ( -1.000000000000000000, 0.000000000000000000, 0.000000000000000000 ) ) ;
#100764 = CARTESIAN_POINT ( 'NONE',  ( -50.29965373618113489, -36.05105100340624347, 50.07322630481903758 ) ) ;
#100765 = ORIENTED_EDGE ( 'NONE', *, *, #90603, .F. ) ;
#100766 = DIRECTION ( 'NONE',  ( 0.5735764363510554853, 0.8191520442889852482, 0.000000000000000000 ) ) ;
#100767 = EDGE_LOOP ( 'NONE', ( #56856, #66559 ) ) ;
#100768 = DIRECTION ( 'NONE',  ( 0.000000000000000000, 0.000000000000000000, 1.000000000000000000 ) ) ;
#100769 = CIRCLE ( 'NONE', #52660, 4.000000000000000888 ) ;
#100770 = CIRCLE ( 'NONE', #97306, 3.309500000000001663 ) ;
#100771 = CARTESIAN_POINT ( 'NONE',  ( -9.482342435886300436, 294.6573797848112690, -3.183473687071290303 ) ) ;
#100772 = EDGE_CURVE ( 'NONE', #5468, #84887, #28656, .T. ) ;
#100773 = CARTESIAN_POINT ( 'NONE',  ( 14.45183933456885761, 0.5067537316480897891, 14.99274988531763775 ) ) ;
#100774 = ORIENTED_EDGE ( 'NONE', *, *, #86921, .T. ) ;
#100775 = AXIS2_PLACEMENT_3D ( 'NONE', #91123, #65764, #83530 ) ;
#100776 = CARTESIAN_POINT ( 'NONE',  ( 94.50952691389738902, -38.49070133904758251, 201.2196195639374707 ) ) ;
#100777 =( NAMED_UNIT ( * ) SI_UNIT ( $, .STERADIAN. ) SOLID_ANGLE_UNIT ( ) );
#100778 = CARTESIAN_POINT ( 'NONE',  ( -12.50000000000000711, 18.64303733123573537, -36.27143273323382999 ) ) ;
#100779 = DIRECTION ( 'NONE',  ( 0.000000000000000000, -1.000000000000000000, 0.000000000000000000 ) ) ;
#100780 = CARTESIAN_POINT ( 'NONE',  ( 90.56128410203886858, 42.00000000000000000, -11.85444436786857558 ) ) ;
#100781 = CARTESIAN_POINT ( 'NONE',  ( 94.51288522389913282, -30.00000000000000711, 191.3190572542347354 ) ) ;
#100782 = DIRECTION ( 'NONE',  ( -1.000000000000000000, -0.000000000000000000, -0.000000000000000000 ) ) ;
#100783 = ADVANCED_FACE ( 'NONE', ( #11895 ), #52841, .T. ) ;
#100784 = B_SPLINE_CURVE_WITH_KNOTS ( 'NONE', 3,
 ( #45508, #47062, #71343, #39535, #5034, #14690, #71876, #96698, #103719, #72412, #22835, #21773, #62744, #31458, #104782, #55667, #88604, #86511, #54608, #30388, #54086, #103199, #29345, #53579, #20742, #30930, #47592, #14159, #5552, #38479 ),
 .UNSPECIFIED., .F., .F.,
 ( 4, 2, 2, 2, 2, 2, 2, 2, 2, 2, 2, 2, 2, 2, 4 ),
 ( 0.01188303771272565881, 0.01280230725828810680, 0.01326194203106932298, 0.01372157680385054090, 0.01418121157663175709, 0.01441102896302235911, 0.01464084634941296287, 0.01487066373580356662, 0.01510048112219417038, 0.01556011589497537442, 0.01601975066775657847, 0.01647938544053778251, 0.01739865498610019406, 0.01831792453166260909, 0.01923719407722502064 ),
 .UNSPECIFIED. ) ;
#100785 = ORIENTED_EDGE ( 'NONE', *, *, #55553, .F. ) ;
#100786 = ORIENTED_EDGE ( 'NONE', *, *, #50996, .T. ) ;
#100787 = CARTESIAN_POINT ( 'NONE',  ( 50.73443445076901526, -60.29831178159185612, 59.32218280885512485 ) ) ;
#100788 = CARTESIAN_POINT ( 'NONE',  ( -46.00000000000000000, 437.9222508511568321, 13.74115800020528155 ) ) ;
#100789 = CARTESIAN_POINT ( 'NONE',  ( -7.500000000000007105, 42.00000000000000711, -59.28631038546422616 ) ) ;
#100790 = EDGE_CURVE ( 'NONE', #71163, #56205, #80048, .T. ) ;
#100791 = VERTEX_POINT ( 'NONE', #13475 ) ;
#100792 = CARTESIAN_POINT ( 'NONE',  ( -91.44668068905532721, -38.39006247391498050, -8.007462388528333364 ) ) ;
#100793 = ORIENTED_EDGE ( 'NONE', *, *, #31588, .T. ) ;
#100794 = SURFACE_SIDE_STYLE ('',( #17250 ) ) ;
#100795 = CARTESIAN_POINT ( 'NONE',  ( 106.9049990251340034, -38.36531872114127140, 195.0069650757791067 ) ) ;
#100796 = CARTESIAN_POINT ( 'NONE',  ( 13.56157340972956682, 22.61046526843750470, -2.795122311634720802 ) ) ;
#100797 = CARTESIAN_POINT ( 'NONE',  ( 88.36089431529551064, -37.84864422464463019, 68.44789249334731096 ) ) ;
#100798 = CARTESIAN_POINT ( 'NONE',  ( -1.102503403746643018, 45.52456777125835430, -18.11035969089068587 ) ) ;
#100799 = CARTESIAN_POINT ( 'NONE',  ( -21.71806759225283656, 305.0526565939784973, -9.957254290847345146 ) ) ;
#100800 = CARTESIAN_POINT ( 'NONE',  ( 3.216749358082111598, -8.903395928605879917, -12.12543985758794918 ) ) ;
#100801 = EDGE_CURVE ( 'NONE', #49975, #94714, #97549, .T. ) ;
#100802 = CARTESIAN_POINT ( 'NONE',  ( 0.000000000000000000, 0.000000000000000000, -13.00000000000000000 ) ) ;
#100803 = AXIS2_PLACEMENT_3D ( 'NONE', #25958, #34565, #33480 ) ;
#100804 = DIRECTION ( 'NONE',  ( -1.000000000000000000, 0.000000000000000000, 0.000000000000000000 ) ) ;
#100805 = CARTESIAN_POINT ( 'NONE',  ( 9.075140001324529138, 137.9474095044899968, 6.144345929921320785E-13 ) ) ;
#100806 = ORIENTED_EDGE ( 'NONE', *, *, #66860, .F. ) ;
#100807 = DIRECTION ( 'NONE',  ( 0.000000000000000000, -1.000000000000000000, 0.000000000000000000 ) ) ;
#100808 = FACE_OUTER_BOUND ( 'NONE', #20883, .T. ) ;
#100809 = ORIENTED_EDGE ( 'NONE', *, *, #84741, .T. ) ;
#100810 = CARTESIAN_POINT ( 'NONE',  ( -34.14470975531866515, 484.1045092577827518, 0.7158976332298593315 ) ) ;
#100811 = CARTESIAN_POINT ( 'NONE',  ( -40.95753704872183931, 390.7956291586450561, 27.40283599064078501 ) ) ;
#100812 = CARTESIAN_POINT ( 'NONE',  ( -32.84239204141412216, 485.9541550691055249, 5.517081702403281440 ) ) ;
#100813 = CARTESIAN_POINT ( 'NONE',  ( 57.45015997180046696, 6.975173280561618775E-15, 0.000000000000000000 ) ) ;
#100814 = CARTESIAN_POINT ( 'NONE',  ( -5.656854249492381470, -26.56249999999999645, 5.656854249492379694 ) ) ;
#100815 = CARTESIAN_POINT ( 'NONE',  ( 43.34664592991014587, -27.69598330275180231, 38.46056262246474944 ) ) ;
#100816 = CARTESIAN_POINT ( 'NONE',  ( 44.83349330513380693, 1.593028355512270567E-15, 0.000000000000000000 ) ) ;
#100817 = ORIENTED_EDGE ( 'NONE', *, *, #38258, .F. ) ;
#100818 = CARTESIAN_POINT ( 'NONE',  ( 82.22591555319118584, -60.76466039185579859, 188.6612029719528039 ) ) ;
#100819 = FILL_AREA_STYLE ('',( #93810 ) ) ;
#100820 = CIRCLE ( 'NONE', #54297, 4.000000000000000888 ) ;
#100821 = CARTESIAN_POINT ( 'NONE',  ( -16.02987949830368564, 45.83140534720697445, 6.508315408883771802 ) ) ;
#100822 = ORIENTED_EDGE ( 'NONE', *, *, #72195, .T. ) ;
#100823 = CARTESIAN_POINT ( 'NONE',  ( -98.38802680873801876, -45.26535420428151468, 120.6788969241506209 ) ) ;
#100824 = DIRECTION ( 'NONE',  ( 0.000000000000000000, -1.000000000000000000, 0.000000000000000000 ) ) ;
#100825 = CARTESIAN_POINT ( 'NONE',  ( 2.751706330279339863, -3.000000000000002665, -100.0000000000000000 ) ) ;
#100826 = CARTESIAN_POINT ( 'NONE',  ( -14.92100282753430562, -3.000000000000002665, -82.95543583084106842 ) ) ;
#100827 = CARTESIAN_POINT ( 'NONE',  ( -27.61666142601160701, -28.69133200283256713, -38.28075806456551788 ) ) ;
#100828 = EDGE_CURVE ( 'NONE', #12068, #56766, #53143, .T. ) ;
#100829 =( GEOMETRIC_REPRESENTATION_CONTEXT ( 3 ) GLOBAL_UNCERTAINTY_ASSIGNED_CONTEXT ( ( #50469 ) ) GLOBAL_UNIT_ASSIGNED_CONTEXT ( ( #4783, #14975, #13380 ) ) REPRESENTATION_CONTEXT ( 'NONE', 'WORKASPACE' ) );
#100830 =( LENGTH_UNIT ( ) NAMED_UNIT ( * ) SI_UNIT ( .MILLI., .METRE. ) );
#100831 = CARTESIAN_POINT ( 'NONE',  ( 50.67286391799485301, -60.00000000000000000, 73.50007806226966522 ) ) ;
#100832 =( GEOMETRIC_REPRESENTATION_CONTEXT ( 3 ) GLOBAL_UNCERTAINTY_ASSIGNED_CONTEXT ( ( #5927 ) ) GLOBAL_UNIT_ASSIGNED_CONTEXT ( ( #83278, #10967, #43881 ) ) REPRESENTATION_CONTEXT ( 'NONE', 'WORKASPACE' ) );
#100833 = CARTESIAN_POINT ( 'NONE',  ( 24.28708600688997166, -28.55405093416178630, 38.02957352212126096 ) ) ;
#100834 = DIRECTION ( 'NONE',  ( 0.000000000000000000, -1.000000000000000000, 0.000000000000000000 ) ) ;
#100835 = CARTESIAN_POINT ( 'NONE',  ( 27.01661562657338678, -20.25300179656017008, 31.73816561356836274 ) ) ;
#100836 = EDGE_CURVE ( 'NONE', #92331, #98735, #81922, .T. ) ;
#100838 = CARTESIAN_POINT ( 'NONE',  ( -13.67356607649133693, 22.79711367846607217, -2.036615685936300491 ) ) ;
#100837 = CARTESIAN_POINT ( 'NONE',  ( -42.01420664154974105, -38.13943564830498190, 52.75245923061931563 ) ) ;
#100839 = CARTESIAN_POINT ( 'NONE',  ( 6.145867760142384562, 301.8770827788400766, -10.02048593162349555 ) ) ;
#100840 = AXIS2_PLACEMENT_3D ( 'NONE', #104055, #54963, #29684 ) ;
#100841 = CARTESIAN_POINT ( 'NONE',  ( 32.35336999986095208, 300.6590557721156642, 11.25190399080426751 ) ) ;
#100842 = SURFACE_SIDE_STYLE ('',( #25406 ) ) ;
#100843 =( GEOMETRIC_REPRESENTATION_CONTEXT ( 3 ) GLOBAL_UNCERTAINTY_ASSIGNED_CONTEXT ( ( #80425 ) ) GLOBAL_UNIT_ASSIGNED_CONTEXT ( ( #32744, #90424, #65616 ) ) REPRESENTATION_CONTEXT ( 'NONE', 'WORKASPACE' ) );
#100844 = EDGE_CURVE ( 'NONE', #11929, #103169, #76947, .T. ) ;
#100845 = PRESENTATION_STYLE_ASSIGNMENT (( #75511 ) ) ;
#100846 = AXIS2_PLACEMENT_3D ( 'NONE', #91224, #17329, #50205 ) ;
#100847 = EDGE_CURVE ( 'NONE', #104577, #10763, #6696, .T. ) ;
#100848 = EDGE_LOOP ( 'NONE', ( #35736, #23707, #8631, #33512 ) ) ;
#100849 = LINE ( 'NONE', #93835, #95014 ) ;
#100850 = PRODUCT_DEFINITION_SHAPE ( 'NONE', 'NONE',  #15959 ) ;
#100851 = AXIS2_PLACEMENT_3D ( 'NONE', #95357, #87274, #13352 ) ;
#100852 = EDGE_CURVE ( 'NONE', #47541, #8878, #23738, .T. ) ;
#100853 = CARTESIAN_POINT ( 'NONE',  ( 0.000000000000000000, 0.000000000000000000, 0.000000000000000000 ) ) ;
#100854 = CIRCLE ( 'NONE', #54333, 5.000000000000002665 ) ;
#100855 = CARTESIAN_POINT ( 'NONE',  ( 37.39037644056565313, 437.8315769265258837, 4.421099621127080326 ) ) ;
#100857 = CARTESIAN_POINT ( 'NONE',  ( 15.57243583339607618, -21.77026072153822156, -30.00009859734665696 ) ) ;
#100856 = CARTESIAN_POINT ( 'NONE',  ( 9.698972129396524977, 253.1762971274193887, -2.445345647270337430 ) ) ;
#100858 = EDGE_LOOP ( 'NONE', ( #11306, #50524, #21222, #28161 ) ) ;
#100859 = CARTESIAN_POINT ( 'NONE',  ( 0.000000000000000000, 0.000000000000000000, 0.000000000000000000 ) ) ;
#100860 = CARTESIAN_POINT ( 'NONE',  ( -1.000000000001115108, -15.98025244997938721, -10.26003014047063822 ) ) ;
#100861 = VERTEX_POINT ( 'NONE', #24269 ) ;
#100862 = PLANE ( 'NONE',  #28375 ) ;
#100863 = CARTESIAN_POINT ( 'NONE',  ( 29.86026515094307854, 12.86933730193439196, -39.60535821593534678 ) ) ;
#100864 = DIRECTION ( 'NONE',  ( -1.000000000000000000, -1.224606353822377258E-16, -0.000000000000000000 ) ) ;
#100865 = CARTESIAN_POINT ( 'NONE',  ( -91.97968714158955095, -60.00000000000003553, 6.646224270140889345 ) ) ;
#100866 = DIRECTION ( 'NONE',  ( 0.000000000000000000, -1.000000000000000000, 0.000000000000000000 ) ) ;
#100867 = DIRECTION ( 'NONE',  ( 0.3420201433256622736, 0.000000000000000000, -0.9396926207859106484 ) ) ;
#100868 = CARTESIAN_POINT ( 'NONE',  ( 38.06554674067534449, 464.2394109421263693, 19.21791087872065162 ) ) ;
#100870 = FILL_AREA_STYLE ('',( #102482 ) ) ;
#100869 = CARTESIAN_POINT ( 'NONE',  ( -34.99923118634553987, 435.2190035774330568, 7.261676763235612064 ) ) ;
#100871 = CARTESIAN_POINT ( 'NONE',  ( -83.89944615507195635, -35.96775995157042871, 172.8053575196213671 ) ) ;
#100872 = ORIENTED_EDGE ( 'NONE', *, *, #68947, .F. ) ;
#100873 = FILL_AREA_STYLE ('',( #50710 ) ) ;
#100874 = ORIENTED_EDGE ( 'NONE', *, *, #334, .T. ) ;
#100875 = CONICAL_SURFACE ( 'NONE', #7864, 4.172000000000009479, 0.9599310885968813656 ) ;
#100876 = ORIENTED_EDGE ( 'NONE', *, *, #93572, .T. ) ;
#100877 = CARTESIAN_POINT ( 'NONE',  ( -13.58955859254654364, 303.5476461695370745, -10.06465166092577590 ) ) ;
#100878 = DIRECTION ( 'NONE',  ( 0.000000000000000000, -1.000000000000000000, 0.000000000000000000 ) ) ;
#100879 = FILL_AREA_STYLE ('',( #101430 ) ) ;
#100880 = VERTEX_POINT ( 'NONE', #25889 ) ;
#100881 = LINE ( 'NONE', #18956, #77126 ) ;
#100882 = CARTESIAN_POINT ( 'NONE',  ( 83.86866073052654258, -2.002967142162725287E-29, 5.000000000000011546 ) ) ;
#100883 = CARTESIAN_POINT ( 'NONE',  ( 7.551560007654696705, -13.00910351806993148, -2.648022159607832826 ) ) ;
#100884 = DIRECTION ( 'NONE',  ( 0.000000000000000000, -0.9024170203240217125, 0.4308636924011052804 ) ) ;
#100885 = CARTESIAN_POINT ( 'NONE',  ( 34.10284876471455817, 1.482358050883964840E-15, 0.000000000000000000 ) ) ;
#100886 = CARTESIAN_POINT ( 'NONE',  ( -18.00000000000000355, 12.99999999999999289, 0.000000000000000000 ) ) ;
#100887 = CARTESIAN_POINT ( 'NONE',  ( 96.14436826854903018, -60.00000000000009237, 39.43554979140174765 ) ) ;
#100888 = EDGE_CURVE ( 'NONE', #77549, #62895, #71089, .T. ) ;
#100889 = CARTESIAN_POINT ( 'NONE',  ( -92.04690998902847809, -60.00000000000008527, 204.8849370891594219 ) ) ;
#100890 = CARTESIAN_POINT ( 'NONE',  ( -56.33823149440868150, -60.33114724083395686, 72.31374845339159663 ) ) ;
#100891 = ORIENTED_EDGE ( 'NONE', *, *, #2625, .F. ) ;
#100892 = ORIENTED_EDGE ( 'NONE', *, *, #56234, .F. ) ;
#100893 = CARTESIAN_POINT ( 'NONE',  ( -103.5943349152434791, -45.26536037131153023, 181.5148655901820973 ) ) ;
#100894 = CARTESIAN_POINT ( 'NONE',  ( -3.594029361870008099, -9.531975552773349847, 6.225090491531444670 ) ) ;
#100895 = CARTESIAN_POINT ( 'NONE',  ( 5.656854249492380582, -18.50000000409676915, -5.656854249492379694 ) ) ;
#100896 = CARTESIAN_POINT ( 'NONE',  ( 3.212697619663445803, -30.00000000000000711, 6.447374205472699238 ) ) ;
#100897 = ORIENTED_EDGE ( 'NONE', *, *, #101333, .F. ) ;
#100898 = DIRECTION ( 'NONE',  ( 0.000000000000000000, 1.000000000000000000, 0.000000000000000000 ) ) ;
#100899 = CIRCLE ( 'NONE', #16522, 0.5000000000000004441 ) ;
#100900 = CARTESIAN_POINT ( 'NONE',  ( -82.28682622294347482, -60.00000000000002132, 198.2874724176148789 ) ) ;
#100901 = CARTESIAN_POINT ( 'NONE',  ( -3.352941176470593199, -1.200583151104949176, 104.5794940929807382 ) ) ;
#100902 = CARTESIAN_POINT ( 'NONE',  ( 7.188101187500000044, -22.53125000204838457, 0.000000000000000000 ) ) ;
#100903 = DIRECTION ( 'NONE',  ( 0.000000000000000000, -1.000000000000000000, 0.000000000000000000 ) ) ;
#100904 = CARTESIAN_POINT ( 'NONE',  ( 17.81438722625302518, 1.482358050883964840E-15, 0.000000000000000000 ) ) ;
#100905 = DIRECTION ( 'NONE',  ( -1.000000000000000000, 0.000000000000000000, 0.000000000000000000 ) ) ;
#100906 = CARTESIAN_POINT ( 'NONE',  ( -31.19652432992544888, 378.3327707670021027, 24.28948218791313707 ) ) ;
#100907 = DIRECTION ( 'NONE',  ( 0.000000000000000000, 0.000000000000000000, 1.000000000000000000 ) ) ;
#100908 =( BOUNDED_SURFACE ( )  B_SPLINE_SURFACE ( 3, 2, ( 
 ( #81462, #65834, #90645 ),
 ( #75517, #101401, #10767 ),
 ( #74973, #100855, #8653 ),
 ( #1062, #66362, #84150 ) ),
 .UNSPECIFIED., .F., .F., .F. ) 
 B_SPLINE_SURFACE_WITH_KNOTS ( ( 4, 4 ),
 ( 3, 3 ),
 ( -4.163336342344337027E-17, 0.001025706331908650881 ),
 ( 0.000000000000000000, 1.000000000000000000 ),
 .UNSPECIFIED. ) 
 GEOMETRIC_REPRESENTATION_ITEM ( )  RATIONAL_B_SPLINE_SURFACE ( (
 ( 1.000000000000000000, 0.9193453746270781046, 1.000000000000000000),
 ( 1.000000000000000000, 0.9180307555289033417, 1.000000000000000000),
 ( 1.000000000000000000, 0.9167125567853835477, 1.000000000000000000),
 ( 1.000000000000000000, 0.9153908114178201938, 1.000000000000000000) ) ) 
 REPRESENTATION_ITEM ( '' )  SURFACE ( )  );
#100909 = CARTESIAN_POINT ( 'NONE',  ( 4.149711973588559033, -8.980130494280730957, 13.48951460889846921 ) ) ;
#100910 = CARTESIAN_POINT ( 'NONE',  ( -1.469576158976823947E-15, -14.56250000409677092, 8.000000000000000000 ) ) ;
#100911 = CIRCLE ( 'NONE', #38945, 4.000000000000001776 ) ;
#100912 = CARTESIAN_POINT ( 'NONE',  ( -7.500000000000001776, 25.40357082213843753, -43.84441647605142123 ) ) ;
#100913 = UNCERTAINTY_MEASURE_WITH_UNIT (LENGTH_MEASURE( 1.000000000000000082E-05 ), #40443, 'distance_accuracy_value', 'NONE');
#100914 = CARTESIAN_POINT ( 'NONE',  ( -32.34892057383476072, -53.37767965076007215, 36.58595348072790188 ) ) ;
#100915 = B_SPLINE_CURVE_WITH_KNOTS ( 'NONE', 3,
 ( #92728, #67410, #74409, #99213, #98680, #24834, #8619, #100286, #75480 ),
 .UNSPECIFIED., .F., .F.,
 ( 4, 2, 1, 2, 4 ),
 ( 0.000000000000000000, 0.002165063509461097498, 0.004330127018922194995, 0.006495190528383292493, 0.008660254037844389990 ),
 .UNSPECIFIED. ) ;
#100916 = FACE_OUTER_BOUND ( 'NONE', #19942, .T. ) ;
#100917 = UNCERTAINTY_MEASURE_WITH_UNIT (LENGTH_MEASURE( 1.000000000000000082E-05 ), #53990, 'distance_accuracy_value', 'NONE');
#100918 = CARTESIAN_POINT ( 'NONE',  ( 44.50089742215685362, -25.70400728066517715, 39.42175729867503264 ) ) ;
#100919 =( GEOMETRIC_REPRESENTATION_CONTEXT ( 3 ) GLOBAL_UNCERTAINTY_ASSIGNED_CONTEXT ( ( #11361 ) ) GLOBAL_UNIT_ASSIGNED_CONTEXT ( ( #68845, #101196, #34370 ) ) REPRESENTATION_CONTEXT ( 'NONE', 'WORKASPACE' ) );
#100920 = CARTESIAN_POINT ( 'NONE',  ( -32.04854177568304152, 486.3112398708803426, 5.779390795281895699 ) ) ;
#100921 = CARTESIAN_POINT ( 'NONE',  ( 1.944839216437187431E-15, 45.30391365246044444, 18.75000000000001066 ) ) ;
#100922 = EDGE_CURVE ( 'NONE', #73080, #92577, #50433, .T. ) ;
#100923 = CARTESIAN_POINT ( 'NONE',  ( -94.07850901117426190, -38.49210041709851282, 201.1960849539863432 ) ) ;
#100924 = VECTOR ( 'NONE', #11189, 1000.000000000000000 ) ;
#100925 = VERTEX_POINT ( 'NONE', #43086 ) ;
#100927 = CARTESIAN_POINT ( 'NONE',  ( 34.95237279327285762, 304.8277712208536627, 12.26231981495593537 ) ) ;
#100926 = CARTESIAN_POINT ( 'NONE',  ( -16.13482245078207100, 21.13350007393601970, 3.415357648783710953 ) ) ;
#100928 = CARTESIAN_POINT ( 'NONE',  ( 58.87759684000966587, -59.99999999999999289, 78.92660630072694516 ) ) ;
#100929 = CARTESIAN_POINT ( 'NONE',  ( -19.07197487161970884, 49.63586355494508240, 61.78730625525749787 ) ) ;
#100930 = CARTESIAN_POINT ( 'NONE',  ( -6.907083948287215946, 41.55068305711947829, -58.85924204532966542 ) ) ;
#100931 = CIRCLE ( 'NONE', #50942, 0.9999999999999833467 ) ;
#100932 = CIRCLE ( 'NONE', #54396, 4.000000000000000888 ) ;
#100933 = CARTESIAN_POINT ( 'NONE',  ( 34.25474529525818923, 462.3053719747810533, 4.620191449216225266 ) ) ;
#100934 = FACE_OUTER_BOUND ( 'NONE', #106373, .T. ) ;
#100935 = CARTESIAN_POINT ( 'NONE',  ( 42.64966854229460580, 465.0854819100621853, 13.23715615004964086 ) ) ;
#100936 = CARTESIAN_POINT ( 'NONE',  ( 33.97359119245064818, 434.1099241184709285, 11.80501937577160732 ) ) ;
#100937 = EDGE_CURVE ( 'NONE', #3128, #47612, #11759, .T. ) ;
#100938 = CARTESIAN_POINT ( 'NONE',  ( 112.1232886518557308, -60.00000000000000000, 177.4603685517026577 ) ) ;
#100939 = CARTESIAN_POINT ( 'NONE',  ( 6.585468679846619544, -3.617797563910806868, 6.733790807807553236 ) ) ;
#100940 = AXIS2_PLACEMENT_3D ( 'NONE', #21056, #36707, #53895 ) ;
#100941 = DIRECTION ( 'NONE',  ( -1.000000000000000000, -1.224606353822377258E-16, -0.000000000000000000 ) ) ;
#100942 = VERTEX_POINT ( 'NONE', #50610 ) ;
#100943 = CARTESIAN_POINT ( 'NONE',  ( -31.35596682365705945, 438.0939828603719093, 22.55458131664414267 ) ) ;
#100944 = CARTESIAN_POINT ( 'NONE',  ( -80.84769301060788393, -30.00000000000003197, -12.29708576950179655 ) ) ;
#100945 = EDGE_LOOP ( 'NONE', ( #3610, #4190 ) ) ;
#100947 = CARTESIAN_POINT ( 'NONE',  ( 27.10511071441177222, 36.88665068479793518, -7.556984339679249985 ) ) ;
#100946 = CARTESIAN_POINT ( 'NONE',  ( -54.59759563194740650, -38.34127430065652931, 80.36034406101917682 ) ) ;
#100948 = DIRECTION ( 'NONE',  ( -0.000000000000000000, -1.000000000000000000, -0.000000000000000000 ) ) ;
#100949 = CIRCLE ( 'NONE', #13086, 5.000000000000001776 ) ;
#100950 = CARTESIAN_POINT ( 'NONE',  ( 9.380871178326122717, 27.98883620201673850, 3.467392232194197454 ) ) ;
#100951 = CARTESIAN_POINT ( 'NONE',  ( -5.082755093536325042, -17.46875000204838813, -5.082755093536325930 ) ) ;
#100952 = CARTESIAN_POINT ( 'NONE',  ( 11.99999999999999467, -5.000000000000002665, -83.42920367501479006 ) ) ;
#100953 = CARTESIAN_POINT ( 'NONE',  ( -4.250000000000000000, 5.204748896376250699E-16, -0.9215586320570148260 ) ) ;
#100955 = ORIENTED_EDGE ( 'NONE', *, *, #48127, .F. ) ;
#100954 =( NAMED_UNIT ( * ) PLANE_ANGLE_UNIT ( ) SI_UNIT ( $, .RADIAN. ) );
#100956 = CARTESIAN_POINT ( 'NONE',  ( 81.09842540489270846, -46.43962613874821699, 163.0359359564797046 ) ) ;
#100958 = CIRCLE ( 'NONE', #11403, 3.309500000000001663 ) ;
#100957 = LINE ( 'NONE', #77223, #34325 ) ;
#100959 = CARTESIAN_POINT ( 'NONE',  ( 11.31153846153846132, -4.171999999999999709, 5.616230220889763424E-16 ) ) ;
#100960 = ORIENTED_EDGE ( 'NONE', *, *, #17500, .F. ) ;
#100961 = CARTESIAN_POINT ( 'NONE',  ( 102.6464385083043283, 1.030564683017419500E-14, 0.000000000000000000 ) ) ;
#100962 = CARTESIAN_POINT ( 'NONE',  ( -46.90314054034880797, 18.02221697236581832, 16.15497048139663860 ) ) ;
#100963 = CARTESIAN_POINT ( 'NONE',  ( 5.799999999999999822, 0.000000000000000000, 0.000000000000000000 ) ) ;
#100964 = CARTESIAN_POINT ( 'NONE',  ( 5.947762761376476526, -4.378239541354667530, -5.416666666666668739 ) ) ;
#100965 = CIRCLE ( 'NONE', #52770, 0.5000000000000004441 ) ;
#100966 = CARTESIAN_POINT ( 'NONE',  ( -4.589925132946517827, 251.0652601629250285, 3.864926970398266270 ) ) ;
#100967 = CARTESIAN_POINT ( 'NONE',  ( 16.96311743595812871, 43.37158770818926001, 6.627271858056736242 ) ) ;
#100968 = CARTESIAN_POINT ( 'NONE',  ( 6.457467314873006181, -2.602085213965210642E-15, 18.85860952240310340 ) ) ;
#100969 = ORIENTED_EDGE ( 'NONE', *, *, #83668, .T. ) ;
#100970 = PRESENTATION_STYLE_ASSIGNMENT (( #68079 ) ) ;
#100971 = UNCERTAINTY_MEASURE_WITH_UNIT (LENGTH_MEASURE( 1.000000000000000082E-05 ), #35881, 'distance_accuracy_value', 'NONE');
#100972 = CARTESIAN_POINT ( 'NONE',  ( -1.128183577532071213, 300.9492746658231681, 9.936156289954721998 ) ) ;
#100973 = CARTESIAN_POINT ( 'NONE',  ( 37.46714894334161983, 18.64284798592703751, 8.551881564011154069 ) ) ;
#100974 = CARTESIAN_POINT ( 'NONE',  ( 86.53796551356465727, -57.40570272851905997, 193.5699017834150197 ) ) ;
#100975 = EDGE_CURVE ( 'NONE', #30000, #44460, #102377, .T. ) ;
#100976 = DIRECTION ( 'NONE',  ( 0.000000000000000000, 0.000000000000000000, 1.000000000000000000 ) ) ;
#100977 = EDGE_CURVE ( 'NONE', #15530, #17856, #23543, .T. ) ;
#100978 = CARTESIAN_POINT ( 'NONE',  ( -7.188101187500000044, -24.40625000204838813, -8.802885111219163269E-16 ) ) ;
#100979 = PLANE ( 'NONE',  #95667 ) ;
#100980 = APPLICATION_CONTEXT ( 'automotive_design' ) ;
#100981 = CARTESIAN_POINT ( 'NONE',  ( 81.84444444444444855, 4.172000000000019249, 5.109226446042768454E-16 ) ) ;
#100982 = CARTESIAN_POINT ( 'NONE',  ( 42.04659500829693997, 436.6121354927211087, 19.99047899505293913 ) ) ;
#100983 = ITEM_DEFINED_TRANSFORMATION ( 'NONE', 'NONE', #67948,  #10728 ) ;
#100984 = VERTEX_POINT ( 'NONE', #83527 ) ;
#100985 = CARTESIAN_POINT ( 'NONE',  ( 41.28039629891261342, 485.7122505962505556, -4.568292046900871206 ) ) ;
#100986 = ADVANCED_FACE ( 'NONE', ( #51692 ), #97590, .F. ) ;
#100987 = CARTESIAN_POINT ( 'NONE',  ( -9.969369541356423170, 7.546308884394301586, 0.000000000000000000 ) ) ;
#100988 = ADVANCED_FACE ( 'NONE', ( #86225 ), #15691, .F. ) ;
#100989 = CARTESIAN_POINT ( 'NONE',  ( 56.48317336153285595, 4.000000000000015099, 4.898587196589422689E-16 ) ) ;
#100990 = AXIS2_PLACEMENT_3D ( 'NONE', #17025, #99509, #33218 ) ;
#100991 = ORIENTED_EDGE ( 'NONE', *, *, #102543, .F. ) ;
#100992 = CARTESIAN_POINT ( 'NONE',  ( -7.466998042452497764, 52.17245120308862738, -2.150398540845605666 ) ) ;
#100993 = CARTESIAN_POINT ( 'NONE',  ( 2.354803500934599558, 48.00000000000000000, -100.0000000000000000 ) ) ;
#100994 = CONICAL_SURFACE ( 'NONE', #7975, 6.499999999999999112, 1.047197551196600296 ) ;
#100995 =( NAMED_UNIT ( * ) PLANE_ANGLE_UNIT ( ) SI_UNIT ( $, .RADIAN. ) );
#100996 = CARTESIAN_POINT ( 'NONE',  ( -1.236033772363036132, 10.15598684385509642, -50.72379936455069327 ) ) ;
#100997 = CARTESIAN_POINT ( 'NONE',  ( 26.84999999999999787, 1.533819458162526451E-15, 0.000000000000000000 ) ) ;
#100998 = VECTOR ( 'NONE', #47736, 1000.000000000000000 ) ;
#100999 = DIRECTION ( 'NONE',  ( 0.000000000000000000, 0.000000000000000000, 1.000000000000000000 ) ) ;
#101000 = CARTESIAN_POINT ( 'NONE',  ( -77.61630265161984710, -60.00000000000000711, 192.0045729689810514 ) ) ;
#101001 =( GEOMETRIC_REPRESENTATION_CONTEXT ( 3 ) GLOBAL_UNCERTAINTY_ASSIGNED_CONTEXT ( ( #27885 ) ) GLOBAL_UNIT_ASSIGNED_CONTEXT ( ( #26307, #18184, #1965 ) ) REPRESENTATION_CONTEXT ( 'NONE', 'WORKASPACE' ) );
#101002 = CARTESIAN_POINT ( 'NONE',  ( -45.33180403702434091, 464.4945808635454227, 2.178908857919817699 ) ) ;
#101003 = CARTESIAN_POINT ( 'NONE',  ( 0.000000000000000000, 4.898587196589412829E-16, -4.000000000000000000 ) ) ;
#101004 = CARTESIAN_POINT ( 'NONE',  ( -83.43097235363796926, -53.72644085999411345, 187.4685730767253915 ) ) ;
#101005 = CARTESIAN_POINT ( 'NONE',  ( -4.512569058504254826, 54.30834730652590991, -6.298727642264635662 ) ) ;
#101006 = AXIS2_PLACEMENT_3D ( 'NONE', #15731, #40538, #89100 ) ;
#101007 = AXIS2_PLACEMENT_3D ( 'NONE', #78450, #90800, #33115 ) ;
#101008 = ORIENTED_EDGE ( 'NONE', *, *, #49935, .T. ) ;
#101009 = CARTESIAN_POINT ( 'NONE',  ( -9.882762594765820197, 45.48558064014431324, -15.34364832776106979 ) ) ;
#101010 = DIRECTION ( 'NONE',  ( 0.000000000000000000, -1.000000000000000000, 0.000000000000000000 ) ) ;
#101011 = CARTESIAN_POINT ( 'NONE',  ( -82.48223426280006265, -37.83324084028321010, 8.085024656640488416 ) ) ;
#101012 = CARTESIAN_POINT ( 'NONE',  ( 32.04737116497691574, 465.7264234052258871, 15.44069434686693221 ) ) ;
#101013 = CARTESIAN_POINT ( 'NONE',  ( -35.76320840016588676, 388.4727839510825333, 5.610592865731860002 ) ) ;
#101014 = AXIS2_PLACEMENT_3D ( 'NONE', #105844, #25508, #91286 ) ;
#101015 = CARTESIAN_POINT ( 'NONE',  ( -5.747790115924391152, 4.862630607728038790, -5.000000000000000000 ) ) ;
#101016 = CARTESIAN_POINT ( 'NONE',  ( -15.37676141849992639, -5.579222135594369192, 13.92723728277131556 ) ) ;
#101017 = CARTESIAN_POINT ( 'NONE',  ( -6.073849149975423245, -15.27114203292415873, 14.38605564242085499 ) ) ;
#101018 = CARTESIAN_POINT ( 'NONE',  ( 3.351415132801500718, -0.9950411258689764171, 104.3291499688503450 ) ) ;
#101019 = CARTESIAN_POINT ( 'NONE',  ( 64.23331706704713895, -60.00000000000004263, 125.0204823638418361 ) ) ;
#101020 = CARTESIAN_POINT ( 'NONE',  ( -13.99999999999998046, 61.49999999999999289, 6.999999999999990230 ) ) ;
#101021 = EDGE_CURVE ( 'NONE', #52643, #50869, #33932, .T. ) ;
#101022 = CARTESIAN_POINT ( 'NONE',  ( -72.33650272884364085, -14.21045842199437992, -25.95337777301578797 ) ) ;
#101023 = CARTESIAN_POINT ( 'NONE',  ( -68.05384738583532567, -46.43832317692169909, 99.56375534947220274 ) ) ;
#101024 = ORIENTED_EDGE ( 'NONE', *, *, #68209, .T. ) ;
#101025 = CARTESIAN_POINT ( 'NONE',  ( 68.63284294399571195, -59.99999999999999289, 147.4025539660169954 ) ) ;
#101026 = CARTESIAN_POINT ( 'NONE',  ( 60.45578259952156941, 40.83768840997593941, 24.06212321066767501 ) ) ;
#101027 = CARTESIAN_POINT ( 'NONE',  ( 23.54848554166952823, -59.99999999999506173, 43.23155359999935143 ) ) ;
#101028 = ORIENTED_EDGE ( 'NONE', *, *, #56365, .T. ) ;
#101029 = CARTESIAN_POINT ( 'NONE',  ( 8.400757966424366785, 51.89201850070815425, -1.531152949374624317 ) ) ;
#101030 = CARTESIAN_POINT ( 'NONE',  ( 7.188101187499999156, -27.12500000204838457, 2.977408999572654924 ) ) ;
#101031 = CARTESIAN_POINT ( 'NONE',  ( -4.656390720430125363, -8.683538140394544413, 3.786082374785830762 ) ) ;
#101032 = ORIENTED_EDGE ( 'NONE', *, *, #28720, .T. ) ;
#101033 = CIRCLE ( 'NONE', #16583, 15.00000000000000000 ) ;
#101034 = ORIENTED_EDGE ( 'NONE', *, *, #85776, .F. ) ;
#101035 = CARTESIAN_POINT ( 'NONE',  ( -9.258863595255469647, 41.99999999999999289, -70.74260034492780846 ) ) ;
#101036 = DIRECTION ( 'NONE',  ( 0.000000000000000000, -1.000000000000000000, 0.000000000000000000 ) ) ;
#101037 = CARTESIAN_POINT ( 'NONE',  ( -71.30636318066278534, -59.99999999991200639, 168.8601541835865305 ) ) ;
#101038 = CARTESIAN_POINT ( 'NONE',  ( 29.25327276538528309, 308.5399522405340917, -8.932740553462334532 ) ) ;
#101039 = CARTESIAN_POINT ( 'NONE',  ( 7.188101187499999156, -11.75000000204838813, 2.977408999572654924 ) ) ;
#101040 = CARTESIAN_POINT ( 'NONE',  ( -48.02835407290515946, 14.94086294439721030, 16.85535821593516559 ) ) ;
#101041 = CIRCLE ( 'NONE', #1151, 3.309500000000007880 ) ;
#101042 = DIRECTION ( 'NONE',  ( -0.000000000000000000, -0.000000000000000000, -1.000000000000000000 ) ) ;
#101043 = CARTESIAN_POINT ( 'NONE',  ( 38.85446894546473828, 460.8903912184138676, 2.218456751109172398 ) ) ;
#101044 = CARTESIAN_POINT ( 'NONE',  ( -2.617478844990396514, 50.00000000000001421, -94.73972676610910071 ) ) ;
#101045 = EDGE_CURVE ( 'NONE', #4517, #90738, #101041, .T. ) ;
#101046 = FACE_OUTER_BOUND ( 'NONE', #54780, .T. ) ;
#101047 =( LENGTH_UNIT ( ) NAMED_UNIT ( * ) SI_UNIT ( .MILLI., .METRE. ) );
#101048 = ORIENTED_EDGE ( 'NONE', *, *, #87673, .F. ) ;
#101049 = CARTESIAN_POINT ( 'NONE',  ( 4.844458925423827722, -2.858988884354966675, 103.3760426044467380 ) ) ;
#101051 = CARTESIAN_POINT ( 'NONE',  ( 32.25262845956538627, -39.49034541401320553, 34.00867910329044719 ) ) ;
#101050 = CARTESIAN_POINT ( 'NONE',  ( -3.718188220750955786, -48.95098499554293170, 104.2423402216923591 ) ) ;
#101052 = CARTESIAN_POINT ( 'NONE',  ( 2.723397405354400211E-15, -8.673617379884035472E-16, 22.23822744035697241 ) ) ;
#101053 = ORIENTED_EDGE ( 'NONE', *, *, #72528, .F. ) ;
#101054 = CARTESIAN_POINT ( 'NONE',  ( -23.05169487621096991, 26.02509709072602817, -30.70617127781034128 ) ) ;
#101055 = EDGE_LOOP ( 'NONE', ( #6527, #87280, #29235, #52153 ) ) ;
#101056 = SURFACE_STYLE_FILL_AREA ( #75171 ) ;
#101057 = CARTESIAN_POINT ( 'NONE',  ( -10.00000000000000355, 105.0000000000000000, 0.000000000000000000 ) ) ;
#101058 = CARTESIAN_POINT ( 'NONE',  ( -34.25859903460757039, 436.5725446342189002, 6.424027449235138576 ) ) ;
#101059 = DIRECTION ( 'NONE',  ( -1.000000000000000000, 0.000000000000000000, 0.000000000000000000 ) ) ;
#101060 = DIRECTION ( 'NONE',  ( 0.000000000000000000, 0.000000000000000000, 1.000000000000000000 ) ) ;
#101061 = FILL_AREA_STYLE_COLOUR ( '', #34858 ) ;
#101062 = EDGE_LOOP ( 'NONE', ( #43575, #20097 ) ) ;
#101063 = ADVANCED_FACE ( 'NONE', ( #23077 ), #68337, .T. ) ;
#101064 = CARTESIAN_POINT ( 'NONE',  ( 73.19133291941243158, -60.00000000000002842, -31.37687942255105966 ) ) ;
#101065 = AXIS2_PLACEMENT_3D ( 'NONE', #88101, #77354, #86001 ) ;
#101066 = CARTESIAN_POINT ( 'NONE',  ( 0.000000000000000000, 0.000000000000000000, -4.147675477074182382 ) ) ;
#101067 = CARTESIAN_POINT ( 'NONE',  ( 33.49978038599233798, 465.4670364598634364, 16.54746596774596057 ) ) ;
#101068 = DIRECTION ( 'NONE',  ( -0.000000000000000000, -0.000000000000000000, -1.000000000000000000 ) ) ;
#101069 = EDGE_CURVE ( 'NONE', #36063, #5362, #22341, .T. ) ;
#101070 = CARTESIAN_POINT ( 'NONE',  ( -47.55484174478885961, 16.07433637412307803, -16.76829442854521091 ) ) ;
#101071 = ORIENTED_EDGE ( 'NONE', *, *, #11285, .T. ) ;
#101072 = CARTESIAN_POINT ( 'NONE',  ( -97.92030896840019238, -29.99999999999134914, 199.6821230727564114 ) ) ;
#101073 = ORIENTED_EDGE ( 'NONE', *, *, #17234, .T. ) ;
#101074 = ORIENTED_EDGE ( 'NONE', *, *, #27307, .F. ) ;
#101075 = CARTESIAN_POINT ( 'NONE',  ( 7.934883677559676940, 81.13160822062449995, 1.051380792122692531 ) ) ;
#101076 = FILL_AREA_STYLE_COLOUR ( '', #40723 ) ;
#101077 = CARTESIAN_POINT ( 'NONE',  ( -15.64244949893494052, 35.03874255891448541, -22.45790977275887457 ) ) ;
#101078 = CARTESIAN_POINT ( 'NONE',  ( 26.36650669486618881, 1.474610560812782335E-15, 0.000000000000000000 ) ) ;
#101080 = CARTESIAN_POINT ( 'NONE',  ( 85.63808483343134981, -52.75639776242220336, -9.610134456905338851 ) ) ;
#101079 = AXIS2_PLACEMENT_3D ( 'NONE', #68523, #101415, #80295 ) ;
#101081 = AXIS2_PLACEMENT_3D ( 'NONE', #46111, #38048, #5635 ) ;
#101082 = CARTESIAN_POINT ( 'NONE',  ( -40.05504438264630096, 310.1124923933409718, -6.399326716180240737 ) ) ;
#101083 = CARTESIAN_POINT ( 'NONE',  ( -3.412115861943773254, 304.8518027738260798, -10.00000000023261038 ) ) ;
#101084 = CARTESIAN_POINT ( 'NONE',  ( -17.55562382432310997, 45.00000000000001421, 63.27682836070874828 ) ) ;
#101085 = DIRECTION ( 'NONE',  ( -0.5735764363510497121, 0.8191520442889892450, 1.003171929053521665E-16 ) ) ;
#101086 = EDGE_LOOP ( 'NONE', ( #26272, #50639, #56105, #89524 ) ) ;
#101087 =( BOUNDED_CURVE ( )  B_SPLINE_CURVE ( 2, ( #66105, #98463, #58003 ),
 .UNSPECIFIED., .F., .F. ) 
 B_SPLINE_CURVE_WITH_KNOTS ( ( 3, 3 ),
 ( 0.000000000000000000, 1.000000000000000000 ),
 .UNSPECIFIED. ) 
 CURVE ( )  GEOMETRIC_REPRESENTATION_ITEM ( )  RATIONAL_B_SPLINE_CURVE ( ( 1.000000000000000000, 1.857142857142858317, 1.000000000000000000 ) ) 
 REPRESENTATION_ITEM ( '' )  );
#101088 = CARTESIAN_POINT ( 'NONE',  ( -43.66727438528028671, 435.6676895479261020, 17.39383282232667227 ) ) ;
#101089 = VERTEX_POINT ( 'NONE', #34903 ) ;
#101090 = FILL_AREA_STYLE ('',( #43393 ) ) ;
#101091 = VECTOR ( 'NONE', #93875, 1000.000000000000000 ) ;
#101092 =( BOUNDED_SURFACE ( )  B_SPLINE_SURFACE ( 3, 2, ( 
 ( #91215, #60452, #17853 ),
 ( #19481, #83618, #2161 ),
 ( #100869, #3253, #43180 ),
 ( #52318, #17321, #44246 ),
 ( #27032, #77138, #9722 ),
 ( #34591, #36194, #42638 ),
 ( #50196, #83098, #9192 ),
 ( #75535, #67462, #100341 ) ),
 .UNSPECIFIED., .F., .F., .F. ) 
 B_SPLINE_SURFACE_WITH_KNOTS ( ( 4, 2, 2, 4 ),
 ( 3, 3 ),
 ( -1.994931997373328159E-17, 0.003572974592251130545, 0.005359461888376705792, 0.007145949184502281039 ),
 ( 0.000000000000000000, 1.000000000000000000 ),
 .UNSPECIFIED. ) 
 GEOMETRIC_REPRESENTATION_ITEM ( )  RATIONAL_B_SPLINE_SURFACE ( (
 ( 1.000000000000000000, 0.7557288854865578109, 1.000000000000000000),
 ( 1.000000000000000000, 0.7511728107079237438, 1.000000000000000000),
 ( 1.000000000000000000, 0.7462898432665451276, 1.000000000000000000),
 ( 1.000000000000000000, 0.7384961912446853516, 1.000000000000000000),
 ( 1.000000000000000000, 0.7358197253153077044, 1.000000000000000000),
 ( 1.000000000000000000, 0.7303050827503990705, 1.000000000000000000),
 ( 1.000000000000000000, 0.7274799915864358368, 1.000000000000000000),
 ( 1.000000000000000000, 0.7246213771202483223, 1.000000000000000000) ) ) 
 REPRESENTATION_ITEM ( '' )  SURFACE ( )  );
#101094 = EDGE_LOOP ( 'NONE', ( #29329, #8994, #57000, #30892 ) ) ;
#101093 = CARTESIAN_POINT ( 'NONE',  ( 5.363597346073513350, 41.33266196706048845, -58.39526881795627844 ) ) ;
#101095 = CARTESIAN_POINT ( 'NONE',  ( 75.17581571613058600, -49.90415678964559731, 129.2185576746167897 ) ) ;
#101096 = ADVANCED_FACE ( 'NONE', ( #27893 ), #35434, .T. ) ;
#101097 = CONICAL_SURFACE ( 'NONE', #23585, 8.542937654374686218, 1.221730476396047704 ) ;
#101098 = ORIENTED_EDGE ( 'NONE', *, *, #27054, .F. ) ;
#101099 = CARTESIAN_POINT ( 'NONE',  ( 4.328822244912061912, -48.31633875694424063, 40.50747960775626666 ) ) ;
#101100 = DIRECTION ( 'NONE',  ( 1.000000000000000000, 0.000000000000000000, 0.000000000000000000 ) ) ;
#101101 = CARTESIAN_POINT ( 'NONE',  ( -7.188101187500000044, -24.40625000204838813, -8.802885111219163269E-16 ) ) ;
#101102 = CARTESIAN_POINT ( 'NONE',  ( -93.89056551065039002, -57.67583025180931600, 8.072597750090290347 ) ) ;
#101103 = ORIENTED_EDGE ( 'NONE', *, *, #33139, .F. ) ;
#101104 =( LENGTH_UNIT ( ) NAMED_UNIT ( * ) SI_UNIT ( .MILLI., .METRE. ) );
#101105 = CARTESIAN_POINT ( 'NONE',  ( 31.14131030317610538, -5.000000000000000888, 6.123233995736769241E-16 ) ) ;
#101106 = CARTESIAN_POINT ( 'NONE',  ( 105.1873821515111018, -60.15126481720113816, 187.0774076014252785 ) ) ;
#101107 = CARTESIAN_POINT ( 'NONE',  ( -9.221216839714871938, 83.95240251831026512, 3.869414262756993406 ) ) ;
#101108 = CARTESIAN_POINT ( 'NONE',  ( 48.98918515124452000, 13.11539385479792941, -16.41516879933306683 ) ) ;
#101109 = CARTESIAN_POINT ( 'NONE',  ( -1.469576158976823947E-15, -17.56250000409676915, 8.000000000000000000 ) ) ;
#101110 = CARTESIAN_POINT ( 'NONE',  ( 0.000000000000000000, 0.000000000000000000, 4.000000000000000000 ) ) ;
#101111 = DIRECTION ( 'NONE',  ( 0.000000000000000000, -1.000000000000000000, 0.000000000000000000 ) ) ;
#101112 = DIRECTION ( 'NONE',  ( 0.9737456255366201407, 0.000000000000000000, 0.2276388735438140687 ) ) ;
#101113 = CARTESIAN_POINT ( 'NONE',  ( -37.52575628270366792, 438.0832219636323543, 4.091974619433682570 ) ) ;
#101114 = DIRECTION ( 'NONE',  ( 0.000000000000000000, 0.000000000000000000, -1.000000000000000000 ) ) ;
#101115 = CARTESIAN_POINT ( 'NONE',  ( 69.88291765283142354, 183.1183258647170362, 182.1969486012845891 ) ) ;
#101116 = FACE_OUTER_BOUND ( 'NONE', #50713, .T. ) ;
#101117 = VERTEX_POINT ( 'NONE', #59153 ) ;
#101118 = CARTESIAN_POINT ( 'NONE',  ( 43.61505130863974955, 434.9783532604240008, 14.40542840455674423 ) ) ;
#101119 = DIRECTION ( 'NONE',  ( -1.000000000000000000, -1.224606353822377258E-16, -0.000000000000000000 ) ) ;
#101120 = VECTOR ( 'NONE', #70850, 1000.000000000000114 ) ;
#101121 = EDGE_CURVE ( 'NONE', #98070, #72252, #9792, .T. ) ;
#101122 = CARTESIAN_POINT ( 'NONE',  ( 0.6202535915621898432, 13.31182157833917934, 49.41091134881317970 ) ) ;
#101123 = CARTESIAN_POINT ( 'NONE',  ( -86.49196759552401659, -29.99999999999999289, 181.4671144795470639 ) ) ;
#101124 = ADVANCED_FACE ( 'NONE', ( #35976 ), #71849, .F. ) ;
#101125 = ORIENTED_EDGE ( 'NONE', *, *, #34953, .T. ) ;
#101126 = CARTESIAN_POINT ( 'NONE',  ( 2.819467257040595420, -49.57152905888915484, 44.39875113217646430 ) ) ;
#101127 = CARTESIAN_POINT ( 'NONE',  ( 83.50137569068580490, -57.54076335939706155, 201.4680290845222999 ) ) ;
#101128 = ADVANCED_FACE ( 'NONE', ( #85563 ), #25395, .T. ) ;
#101130 = CARTESIAN_POINT ( 'NONE',  ( 46.08349330513379982, 1.593028355512270567E-15, 0.000000000000000000 ) ) ;
#101129 = CARTESIAN_POINT ( 'NONE',  ( -15.50532557111765541, 2.637300882401473867, 0.8493220884279345517 ) ) ;
#101131 = CARTESIAN_POINT ( 'NONE',  ( 70.17982293570671004, -38.22781381422611702, -31.10776116069777331 ) ) ;
#101132 = CARTESIAN_POINT ( 'NONE',  ( -43.00000000000000000, 435.1719937645106029, 7.191579780910007713 ) ) ;
#101133 = DIRECTION ( 'NONE',  ( 1.000000000000000000, 0.000000000000000000, 0.000000000000000000 ) ) ;
#101134 = CARTESIAN_POINT ( 'NONE',  ( -39.40759530360957541, -59.99999999999999289, 51.27385300903834775 ) ) ;
#101135 = TOROIDAL_SURFACE ( 'NONE', #101230, 12.00000000000000711, 3.000000000000000000 ) ;
#101136 = DIRECTION ( 'NONE',  ( 0.000000000000000000, 1.000000000000000000, 0.000000000000000000 ) ) ;
#101137 = CARTESIAN_POINT ( 'NONE',  ( 58.90678327789231616, 48.00000000000000000, -28.11551192221969941 ) ) ;
#101138 = TOROIDAL_SURFACE ( 'NONE', #102916, 8.499999999999992895, 0.5000000000000000000 ) ;
#101139 = CARTESIAN_POINT ( 'NONE',  ( -85.78283469545968387, -57.45526895688682600, 192.9326975944933054 ) ) ;
#101140 = ORIENTED_EDGE ( 'NONE', *, *, #104273, .F. ) ;
#101141 = CARTESIAN_POINT ( 'NONE',  ( 30.93190593211533823, 14.41219003788192587, 40.70233947780381101 ) ) ;
#101142 = CARTESIAN_POINT ( 'NONE',  ( -1.987691155308321189, -25.54942359938841889, 28.14570803181489822 ) ) ;
#101143 = CARTESIAN_POINT ( 'NONE',  ( -41.58444704644840328, 481.6528781813217961, 13.64578380398117829 ) ) ;
#101145 = SURFACE_SIDE_STYLE ('',( #12125 ) ) ;
#101144 = CARTESIAN_POINT ( 'NONE',  ( -37.25380483576834934, 307.7259701645078280, 4.972132598451335816 ) ) ;
#101146 = EDGE_LOOP ( 'NONE', ( #101074, #16567, #28517, #97168, #6531 ) ) ;
#101147 =( NAMED_UNIT ( * ) SI_UNIT ( $, .STERADIAN. ) SOLID_ANGLE_UNIT ( ) );
#101148 = DIRECTION ( 'NONE',  ( 0.000000000000000000, -1.000000000000000000, 0.000000000000000000 ) ) ;
#101149 = CARTESIAN_POINT ( 'NONE',  ( 31.86888217434322712, 485.1577972469718816, 5.527887721099247642 ) ) ;
#101150 = AXIS2_PLACEMENT_3D ( 'NONE', #15571, #8004, #40914 ) ;
#101151 = VECTOR ( 'NONE', #31539, 1000.000000000000000 ) ;
#101152 = CARTESIAN_POINT ( 'NONE',  ( 23.12331641935568527, 303.3400345184521143, -9.895296368007924670 ) ) ;
#101153 = CARTESIAN_POINT ( 'NONE',  ( 35.96492786661492858, 302.4488314805894902, -8.278427239162008178 ) ) ;
#101154 = FACE_OUTER_BOUND ( 'NONE', #79174, .T. ) ;
#101155 = CARTESIAN_POINT ( 'NONE',  ( 9.805911699687639427, 53.43740237845030094, -2.589507950532081271 ) ) ;
#101156 = EDGE_CURVE ( 'NONE', #31749, #90543, #41588, .T. ) ;
#101157 = CARTESIAN_POINT ( 'NONE',  ( 90.94603201905546541, -14.21045842199432663, 57.96280492189741551 ) ) ;
#101158 = CARTESIAN_POINT ( 'NONE',  ( -81.28725701646312984, -36.03165964993199566, 150.3997114263125070 ) ) ;
#101159 = ORIENTED_EDGE ( 'NONE', *, *, #97953, .F. ) ;
#101160 = DIRECTION ( 'NONE',  ( 0.000000000000000000, -1.000000000000000000, 0.000000000000000000 ) ) ;
#101161 = FACE_OUTER_BOUND ( 'NONE', #45711, .T. ) ;
#101162 = STYLED_ITEM ( 'NONE', ( #18480 ), #24760 ) ;
#101163 = AXIS2_PLACEMENT_3D ( 'NONE', #94104, #4036, #61219 ) ;
#101164 = AXIS2_PLACEMENT_3D ( 'NONE', #77402, #3518, #20281 ) ;
#101165 = PRESENTATION_LAYER_ASSIGNMENT (  '', '', ( #25432 ) ) ;
#101166 = DIRECTION ( 'NONE',  ( 1.000000000000000000, 0.000000000000000000, 0.000000000000000000 ) ) ;
#101167 = CARTESIAN_POINT ( 'NONE',  ( 41.96862382816240711, 327.9039392355280711, 6.054989524861565720 ) ) ;
#101168 = CARTESIAN_POINT ( 'NONE',  ( 12.61650669486618881, 1.474610560812782335E-15, 0.000000000000000000 ) ) ;
#101169 = EDGE_LOOP ( 'NONE', ( #43404, #9608 ) ) ;
#101170 = UNCERTAINTY_MEASURE_WITH_UNIT (LENGTH_MEASURE( 1.000000000000000082E-05 ), #4930, 'distance_accuracy_value', 'NONE');
#101171 = CARTESIAN_POINT ( 'NONE',  ( -12.19423397773156736, 304.5852035401753710, 9.880331998383338643 ) ) ;
#101173 = CIRCLE ( 'NONE', #7565, 4.999999999999998224 ) ;
#101172 = CARTESIAN_POINT ( 'NONE',  ( 31.52580585160177051, 438.9871292739251771, 23.28495454672928489 ) ) ;
#101174 = ORIENTED_EDGE ( 'NONE', *, *, #24121, .F. ) ;
#101175 = CARTESIAN_POINT ( 'NONE',  ( 25.21823338009918203, 3.851859888774471706E-31, 5.000000000000001776 ) ) ;
#101176 = LINE ( 'NONE', #93624, #32614 ) ;
#101177 = CARTESIAN_POINT ( 'NONE',  ( 6.057904175366207511, 41.61856606260997893, -70.65344123640606711 ) ) ;
#101178 = EDGE_CURVE ( 'NONE', #37313, #91522, #51777, .T. ) ;
#101179 = CARTESIAN_POINT ( 'NONE',  ( -57.09426686934756390, 50.00000000000000000, -27.25041924766811618 ) ) ;
#101180 = DIRECTION ( 'NONE',  ( 0.000000000000000000, -1.000000000000000000, 0.000000000000000000 ) ) ;
#101181 = DIRECTION ( 'NONE',  ( -1.000000000000000000, -1.224606353822377258E-16, -0.000000000000000000 ) ) ;
#101182 = ORIENTED_EDGE ( 'NONE', *, *, #24425, .T. ) ;
#101183 = LINE ( 'NONE', #27344, #102326 ) ;
#101185 = CARTESIAN_POINT ( 'NONE',  ( 20.76647212221055483, -18.59340802667270864, 27.55324192485566570 ) ) ;
#101184 = CARTESIAN_POINT ( 'NONE',  ( -92.04690998902847809, -60.00000000000008527, 204.8849370891594219 ) ) ;
#101186 = CARTESIAN_POINT ( 'NONE',  ( -4.088397730506703845E-15, 46.03420836107012093, 33.38430095398285147 ) ) ;
#101187 = CARTESIAN_POINT ( 'NONE',  ( 0.000000000000000000, 0.000000000000000000, 0.000000000000000000 ) ) ;
#101188 = CARTESIAN_POINT ( 'NONE',  ( -35.05813823911775984, -46.43391309501947717, 36.68683573906173478 ) ) ;
#101189 = AXIS2_PLACEMENT_3D ( 'NONE', #33991, #25918, #64858 ) ;
#101190 = CARTESIAN_POINT ( 'NONE',  ( -16.64348903516517098, 45.60392139269950462, 6.657797401561654560 ) ) ;
#101191 = UNCERTAINTY_MEASURE_WITH_UNIT (LENGTH_MEASURE( 1.000000000000000082E-05 ), #94021, 'distance_accuracy_value', 'NONE');
#101192 = ORIENTED_EDGE ( 'NONE', *, *, #39626, .F. ) ;
#101193 = DIRECTION ( 'NONE',  ( -1.000000000000000000, -0.000000000000000000, -0.000000000000000000 ) ) ;
#101194 = CYLINDRICAL_SURFACE ( 'NONE', #7758, 10.00000000000000000 ) ;
#101195 = CARTESIAN_POINT ( 'NONE',  ( -13.95266368664216294, -57.79432512081118034, 25.82453759514263680 ) ) ;
#101196 =( NAMED_UNIT ( * ) PLANE_ANGLE_UNIT ( ) SI_UNIT ( $, .RADIAN. ) );
#101197 = CARTESIAN_POINT ( 'NONE',  ( 7.344505440741523117, -62.55381072701295153, -3.175463080953004447 ) ) ;
#101199 = ORIENTED_EDGE ( 'NONE', *, *, #22161, .F. ) ;
#101198 = AXIS2_PLACEMENT_3D ( 'NONE', #94964, #72254, #4874 ) ;
#101200 = DIRECTION ( 'NONE',  ( 0.000000000000000000, 0.000000000000000000, 1.000000000000000000 ) ) ;
#101201 = ORIENTED_EDGE ( 'NONE', *, *, #26863, .T. ) ;
#101202 = CARTESIAN_POINT ( 'NONE',  ( 98.58235770902466300, -29.99999999999995737, 189.7049926379953888 ) ) ;
#101203 = CARTESIAN_POINT ( 'NONE',  ( 82.70911704725124025, 1.016364837396684119E-14, 0.000000000000000000 ) ) ;
#101204 = UNCERTAINTY_MEASURE_WITH_UNIT (LENGTH_MEASURE( 1.000000000000000082E-05 ), #14337, 'distance_accuracy_value', 'NONE');
#101205 = DIRECTION ( 'NONE',  ( 0.000000000000000000, -1.000000000000000000, 0.000000000000000000 ) ) ;
#101206 = CIRCLE ( 'NONE', #78778, 1.000000000000000888 ) ;
#101207 = CARTESIAN_POINT ( 'NONE',  ( 81.06425680110626786, -30.00000000000000000, 22.12711938399802847 ) ) ;
#101208 = EDGE_CURVE ( 'NONE', #32538, #92197, #83949, .T. ) ;
#101209 = CARTESIAN_POINT ( 'NONE',  ( -28.84069063680069434, 315.3197465396486905, 12.73806496493308593 ) ) ;
#101210 = ORIENTED_EDGE ( 'NONE', *, *, #91556, .F. ) ;
#101211 = ORIENTED_EDGE ( 'NONE', *, *, #6869, .T. ) ;
#101212 = ORIENTED_EDGE ( 'NONE', *, *, #87375, .T. ) ;
#101214 = EDGE_LOOP ( 'NONE', ( #41713, #36111, #71332, #3873 ) ) ;
#101213 = CARTESIAN_POINT ( 'NONE',  ( -32.65869381073711253, 465.0820644893343001, 12.85946116547015983 ) ) ;
#101215 = DIRECTION ( 'NONE',  ( 1.000000000000000000, 0.000000000000000000, 0.000000000000000000 ) ) ;
#101216 = CARTESIAN_POINT ( 'NONE',  ( -19.01441297883930304, 303.6984617652402676, 9.904405537397884984 ) ) ;
#101217 =( NAMED_UNIT ( * ) SI_UNIT ( $, .STERADIAN. ) SOLID_ANGLE_UNIT ( ) );
#101218 = CARTESIAN_POINT ( 'NONE',  ( -31.42155219348691375, 380.7461170327588320, 23.45653096014077477 ) ) ;
#101219 = CARTESIAN_POINT ( 'NONE',  ( 10.51296777078104050, 50.00000000000000000, -92.64705882352942012 ) ) ;
#101220 = STYLED_ITEM ( 'NONE', ( #10820 ), #1568 ) ;
#101221 = ORIENTED_EDGE ( 'NONE', *, *, #99418, .T. ) ;
#101222 = CARTESIAN_POINT ( 'NONE',  ( -6.043427762773251111, 50.00000000000000000, -95.48543666094653304 ) ) ;
#101224 = EDGE_CURVE ( 'NONE', #40289, #84395, #47335, .T. ) ;
#101223 = EDGE_LOOP ( 'NONE', ( #43048, #83303, #52833, #5407, #31130, #9999 ) ) ;
#101225 = CARTESIAN_POINT ( 'NONE',  ( -4.165977904505308693, 16.00000000000000000, -9.090909090909089940 ) ) ;
#101226 = CARTESIAN_POINT ( 'NONE',  ( 75.26362525057788844, -38.34453862111913480, 172.0622010566955851 ) ) ;
#101227 = CARTESIAN_POINT ( 'NONE',  ( -1.469576158976823947E-15, -11.56250000409677092, 8.000000000000000000 ) ) ;
#101228 = ADVANCED_FACE ( 'NONE', ( #6880 ), #44307, .T. ) ;
#101229 = CARTESIAN_POINT ( 'NONE',  ( 29.82401586680403938, 298.2086656657758681, 10.68039305417390139 ) ) ;
#101230 = AXIS2_PLACEMENT_3D ( 'NONE', #95304, #39196, #104983 ) ;
#101231 = DIRECTION ( 'NONE',  ( -1.000000000000000000, -0.000000000000000000, -0.000000000000000000 ) ) ;
#101232 = AXIS2_PLACEMENT_3D ( 'NONE', #19179, #67153, #28314 ) ;
#101233 = EDGE_CURVE ( 'NONE', #13709, #72287, #40832, .T. ) ;
#101234 = EDGE_LOOP ( 'NONE', ( #89364, #30113, #24911, #5966, #26441 ) ) ;
#101235 = CARTESIAN_POINT ( 'NONE',  ( -8.737863883542573262, -3.000000000000002665, -90.03618980370899294 ) ) ;
#101236 = CARTESIAN_POINT ( 'NONE',  ( 17.88133836625030426, 45.34897204669927362, -5.215214262617966945 ) ) ;
#101237 = CARTESIAN_POINT ( 'NONE',  ( 104.3757837139179117, 1.016364837396684119E-14, 0.000000000000000000 ) ) ;
#101238 =( BOUNDED_CURVE ( )  B_SPLINE_CURVE ( 2, ( #19525, #103057, #27078, #29214, #93373, #84211, #3293, #2745, #100910 ),
 .UNSPECIFIED., .F., .F. ) 
 B_SPLINE_CURVE_WITH_KNOTS ( ( 3, 2, 2, 2, 3 ),
 ( 0.7205882352941176405, 0.7279411764705882026, 0.7352941176470588758, 0.7426470588235294379, 0.7500000000000000000 ),
 .UNSPECIFIED. ) 
 CURVE ( )  GEOMETRIC_REPRESENTATION_ITEM ( )  RATIONAL_B_SPLINE_CURVE ( ( 1.000000000000000000, 0.9238795325112867385, 1.000000000000000000, 0.9238795325112867385, 1.000000000000000000, 0.9238795325112867385, 1.000000000000000000, 0.9238795325112867385, 1.000000000000000000 ) ) 
 REPRESENTATION_ITEM ( '' )  );
#101239 = CARTESIAN_POINT ( 'NONE',  ( 0.000000000000000000, 0.000000000000000000, 0.000000000000000000 ) ) ;
#101240 = CARTESIAN_POINT ( 'NONE',  ( 14.61305944212074692, 1.672740767018813024, 3.460733717104720331 ) ) ;
#101241 = VERTEX_POINT ( 'NONE', #55934 ) ;
#101242 = CARTESIAN_POINT ( 'NONE',  ( 7.744168461338430731, -88.46254061715157491, 2.019395720771552050 ) ) ;
#101243 = DIRECTION ( 'NONE',  ( -0.000000000000000000, 1.000000000000000000, -0.000000000000000000 ) ) ;
#101244 = DIRECTION ( 'NONE',  ( 0.000000000000000000, -1.000000000000000000, 0.000000000000000000 ) ) ;
#101245 = CARTESIAN_POINT ( 'NONE',  ( 4.250000000000000000, 0.000000000000000000, -0.5505556536572887572 ) ) ;
#101247 = CARTESIAN_POINT ( 'NONE',  ( 33.94429683799095443, 489.7044232353788971, 10.92862313927360596 ) ) ;
#101246 = AXIS2_PLACEMENT_3D ( 'NONE', #65863, #98742, #90677 ) ;
#101248 = CARTESIAN_POINT ( 'NONE',  ( 42.61140200160144786, 465.9030374194822457, 13.21253569360410829 ) ) ;
#101249 = PRESENTATION_LAYER_ASSIGNMENT (  '', '', ( #40945 ) ) ;
#101250 = AXIS2_PLACEMENT_3D ( 'NONE', #8011, #66800, #90005 ) ;
#101251 = DIRECTION ( 'NONE',  ( 0.000000000000000000, 0.000000000000000000, 1.000000000000000000 ) ) ;
#101252 = PRESENTATION_LAYER_ASSIGNMENT (  '', '', ( #32354 ) ) ;
#101253 = CARTESIAN_POINT ( 'NONE',  ( 86.57521083124422034, -42.81237575202452916, 189.2799081440977602 ) ) ;
#101254 = CARTESIAN_POINT ( 'NONE',  ( 17.37779721166321778, 36.93489020264718192, -21.96297318349786210 ) ) ;
#101255 = CARTESIAN_POINT ( 'NONE',  ( -3.750717479518892006, 132.2449738128835577, 5.000000000000000888 ) ) ;
#101256 = ORIENTED_EDGE ( 'NONE', *, *, #39246, .F. ) ;
#101257 = CARTESIAN_POINT ( 'NONE',  ( 69.25544739171029107, -57.67106767548779089, -34.92408972481134555 ) ) ;
#101258 = FILL_AREA_STYLE ('',( #20922 ) ) ;
#101259 = CARTESIAN_POINT ( 'NONE',  ( -3.250000000000016431, 5.629165124598842773, 1.734723475976807094E-15 ) ) ;
#101260 = CYLINDRICAL_SURFACE ( 'NONE', #16611, 1.250000000000001110 ) ;
#101261 = CARTESIAN_POINT ( 'NONE',  ( -88.91012085090163453, -30.00000000000000355, 82.06472925106058369 ) ) ;
#101262 = ADVANCED_FACE ( 'NONE', ( #6334 ), #13366, .T. ) ;
#101263 = B_SPLINE_CURVE_WITH_KNOTS ( 'NONE', 3,
 ( #103993, #71624, #20498, #5832 ),
 .UNSPECIFIED., .F., .F.,
 ( 4, 4 ),
 ( 0.000000000000000000, 1.000000000000000000 ),
 .UNSPECIFIED. ) ;
#101264 = VECTOR ( 'NONE', #39974, 1000.000000000000114 ) ;
#101265 = LINE ( 'NONE', #1470, #41680 ) ;
#101266 = CARTESIAN_POINT ( 'NONE',  ( -4.599534470795829222, 6.460478697738384568, -7.590212325761545031 ) ) ;
#101267 = EDGE_CURVE ( 'NONE', #93631, #42388, #87820, .T. ) ;
#101269 = FACE_OUTER_BOUND ( 'NONE', #88243, .T. ) ;
#101268 = CARTESIAN_POINT ( 'NONE',  ( -7.897836333153806621, -1.530409084195007985, -7.633857274177629826 ) ) ;
#101270 = AXIS2_PLACEMENT_3D ( 'NONE', #6583, #21758, #95615 ) ;
#101271 = FACE_OUTER_BOUND ( 'NONE', #32644, .T. ) ;
#101272 = DIRECTION ( 'NONE',  ( -0.000000000000000000, 1.000000000000000000, -0.000000000000000000 ) ) ;
#101273 = CARTESIAN_POINT ( 'NONE',  ( 6.928203230275509661, 30.00000000000000000, 4.000000000000000000 ) ) ;
#101274 = CARTESIAN_POINT ( 'NONE',  ( 61.09210413872295931, -29.38834330421657270, -24.58964298202642595 ) ) ;
#101275 =( GEOMETRIC_REPRESENTATION_CONTEXT ( 3 ) GLOBAL_UNCERTAINTY_ASSIGNED_CONTEXT ( ( #61272 ) ) GLOBAL_UNIT_ASSIGNED_CONTEXT ( ( #14401, #80210, #12294 ) ) REPRESENTATION_CONTEXT ( 'NONE', 'WORKASPACE' ) );
#101276 = CARTESIAN_POINT ( 'NONE',  ( -25.97158367243803667, -36.00318411789499606, 31.37728892077313603 ) ) ;
#101277 = ORIENTED_EDGE ( 'NONE', *, *, #20474, .T. ) ;
#101278 = CARTESIAN_POINT ( 'NONE',  ( 6.981089760825446078, 9.033170731678344723, 0.5312715680615406333 ) ) ;
#101279 = FILL_AREA_STYLE_COLOUR ( '', #2144 ) ;
#101280 = CARTESIAN_POINT ( 'NONE',  ( -16.63618056918942045, -32.51365049520764217, 29.53634284231671714 ) ) ;
#101281 = DIRECTION ( 'NONE',  ( 1.000000000000000000, 0.000000000000000000, -0.000000000000000000 ) ) ;
#101282 = CARTESIAN_POINT ( 'NONE',  ( 0.6421581498681602218, 36.36120089367192065, -29.57562450428436662 ) ) ;
#101283 = EDGE_CURVE ( 'NONE', #84625, #14056, #47751, .T. ) ;
#101284 = ORIENTED_EDGE ( 'NONE', *, *, #21996, .T. ) ;
#101285 = CIRCLE ( 'NONE', #22075, 4.000000000000000888 ) ;
#101286 = CARTESIAN_POINT ( 'NONE',  ( -35.45036406932566564, 436.3203772529605544, 5.179456583033978490 ) ) ;
#101287 = EDGE_LOOP ( 'NONE', ( #32652, #38513, #63530, #102489, #12263 ) ) ;
#101288 = FILL_AREA_STYLE_COLOUR ( '', #77425 ) ;
#101289 = CIRCLE ( 'NONE', #85753, 0.9999999999999994449 ) ;
#101290 =( NAMED_UNIT ( * ) SI_UNIT ( $, .STERADIAN. ) SOLID_ANGLE_UNIT ( ) );
#101291 = ADVANCED_FACE ( 'NONE', ( #21001 ), #18460, .T. ) ;
#101292 = DIRECTION ( 'NONE',  ( 1.000000000000000000, 1.224606353822377258E-16, 0.000000000000000000 ) ) ;
#101293 = VERTEX_POINT ( 'NONE', #63550 ) ;
#101294 = CARTESIAN_POINT ( 'NONE',  ( 100.9578779286414800, -52.74261186640906374, 193.4183224279464071 ) ) ;
#101296 = FACE_OUTER_BOUND ( 'NONE', #93734, .T. ) ;
#101295 =( NAMED_UNIT ( * ) SI_UNIT ( $, .STERADIAN. ) SOLID_ANGLE_UNIT ( ) );
#101297 = VECTOR ( 'NONE', #8641, 1000.000000000000000 ) ;
#101298 = EDGE_LOOP ( 'NONE', ( #1177, #57600 ) ) ;
#101299 = ORIENTED_EDGE ( 'NONE', *, *, #49670, .T. ) ;
#101300 = ORIENTED_EDGE ( 'NONE', *, *, #43077, .F. ) ;
#101301 = CARTESIAN_POINT ( 'NONE',  ( 24.02573244599213353, 306.3041407548990946, 9.258542674397354233 ) ) ;
#101302 = B_SPLINE_CURVE_WITH_KNOTS ( 'NONE', 3,
 ( #13885, #55405, #46802, #79695, #5804, #38727 ),
 .UNSPECIFIED., .F., .F.,
 ( 4, 2, 4 ),
 ( 0.02753256083616405225, 0.02987018135583073206, 0.03220780187549741186 ),
 .UNSPECIFIED. ) ;
#101303 = DIRECTION ( 'NONE',  ( 0.000000000000000000, -1.000000000000000000, 0.000000000000000000 ) ) ;
#101304 = DIRECTION ( 'NONE',  ( 0.000000000000000000, -1.000000000000000000, 0.000000000000000000 ) ) ;
#101306 = EDGE_CURVE ( 'NONE', #7894, #15446, #1219, .T. ) ;
#101305 = ORIENTED_EDGE ( 'NONE', *, *, #64871, .T. ) ;
#101307 = DIRECTION ( 'NONE',  ( 0.000000000000000000, -0.000000000000000000, 1.000000000000000000 ) ) ;
#101308 = DIRECTION ( 'NONE',  ( 0.000000000000000000, 0.000000000000000000, 1.000000000000000000 ) ) ;
#101309 = CARTESIAN_POINT ( 'NONE',  ( -83.96692933907711165, -60.00000000000971312, -28.23229891493929600 ) ) ;
#101310 = CARTESIAN_POINT ( 'NONE',  ( 43.21667697146742881, 434.4554196591589630, 16.17972000939166222 ) ) ;
#101311 = CONICAL_SURFACE ( 'NONE', #20382, 4.000000000000001776, 0.9599310885968808105 ) ;
#101312 = CARTESIAN_POINT ( 'NONE',  ( 1.040949779275250140E-15, -15.00000000000000000, 8.500000000000000000 ) ) ;
#101313 = CARTESIAN_POINT ( 'NONE',  ( -7.026865645360749646, 41.28180592973833285, -58.57603972943267934 ) ) ;
#101314 = TOROIDAL_SURFACE ( 'NONE', #63454, 7.999999999999998224, 2.000000000000000000 ) ;
#101315 = CARTESIAN_POINT ( 'NONE',  ( -87.76943268072510307, -14.21045842199432307, -6.547605000374890238 ) ) ;
#101316 = CARTESIAN_POINT ( 'NONE',  ( -43.51765957956997966, 464.6235667276147296, 9.550596550081237979 ) ) ;
#101317 = CARTESIAN_POINT ( 'NONE',  ( -50.52341832492433582, -25.65870449059931957, 46.96528990739796683 ) ) ;
#101318 = VERTEX_POINT ( 'NONE', #14963 ) ;
#101319 = CARTESIAN_POINT ( 'NONE',  ( -12.50000000000000533, 152.0000000000000000, 0.000000000000000000 ) ) ;
#101320 = ORIENTED_EDGE ( 'NONE', *, *, #22621, .T. ) ;
#101321 = CARTESIAN_POINT ( 'NONE',  ( -3.313708498984837547, -13.53124999999998934, -7.999999999999923617 ) ) ;
#101322 = STYLED_ITEM ( 'NONE', ( #65942 ), #39165 ) ;
#101323 = CARTESIAN_POINT ( 'NONE',  ( -7.886225517035546417, 296.0473068317272123, -10.02775466922440195 ) ) ;
#101324 = CARTESIAN_POINT ( 'NONE',  ( 16.65484354297773351, 6.123233995736770227E-16, -5.000000000000002665 ) ) ;
#101325 = ORIENTED_EDGE ( 'NONE', *, *, #20690, .F. ) ;
#101326 = CARTESIAN_POINT ( 'NONE',  ( 109.5798523967376497, -30.00000000001343992, 175.3446974936682068 ) ) ;
#101327 = CARTESIAN_POINT ( 'NONE',  ( 48.59987877357390573, 15.38663336896927447, 14.48702310944051419 ) ) ;
#101328 = DIRECTION ( 'NONE',  ( -1.000000000000000000, -1.224606353822377258E-16, -0.000000000000000000 ) ) ;
#101329 = CARTESIAN_POINT ( 'NONE',  ( -1.221766272017100308, -5.532494385104715917, -13.95387042840530256 ) ) ;
#101330 = CARTESIAN_POINT ( 'NONE',  ( 10.04205104292330475, 18.64316884715076839, 37.36680950592799633 ) ) ;
#101331 = CARTESIAN_POINT ( 'NONE',  ( 87.06498138213956395, -30.00000000000000355, 183.9578833979254568 ) ) ;
#101332 = CARTESIAN_POINT ( 'NONE',  ( -11.24782996177939332, 43.18746564262799126, -14.96095123926246373 ) ) ;
#101333 = EDGE_CURVE ( 'NONE', #100365, #90212, #4667, .T. ) ;
#101334 = CARTESIAN_POINT ( 'NONE',  ( 6.400000000000000355, -4.618802153517009401, -8.000000000000001776 ) ) ;
#101335 = ORIENTED_EDGE ( 'NONE', *, *, #71742, .T. ) ;
#101336 = EDGE_LOOP ( 'NONE', ( #87521, #37806, #58293, #20593, #18124 ) ) ;
#101337 = CARTESIAN_POINT ( 'NONE',  ( 51.03706583455220880, -49.90368789440714892, 56.18858338209947334 ) ) ;
#101338 = LINE ( 'NONE', #77053, #38732 ) ;
#101339 = DIRECTION ( 'NONE',  ( 0.000000000000000000, 0.000000000000000000, 1.000000000000000000 ) ) ;
#101340 = EDGE_CURVE ( 'NONE', #50908, #20242, #44087, .T. ) ;
#101341 = ORIENTED_EDGE ( 'NONE', *, *, #94820, .F. ) ;
#101342 = CARTESIAN_POINT ( 'NONE',  ( -90.37755454089685259, -38.40153146471335788, -14.95169647791086653 ) ) ;
#101343 = TOROIDAL_SURFACE ( 'NONE', #6630, 11.00000000000000000, 2.000000000000000000 ) ;
#101344 = ORIENTED_EDGE ( 'NONE', *, *, #49733, .F. ) ;
#101345 = CARTESIAN_POINT ( 'NONE',  ( 108.2541020591300907, -38.35772930560278127, 192.2632853830203032 ) ) ;
#101346 = CARTESIAN_POINT ( 'NONE',  ( 11.23676242740048892, 17.72229746334734202, 8.838879072636887102 ) ) ;
#101347 = CARTESIAN_POINT ( 'NONE',  ( 83.25917025631360957, -37.85102771844027814, 29.52673368758545536 ) ) ;
#101348 = CARTESIAN_POINT ( 'NONE',  ( -26.46282106933370315, 307.1428501120792021, -8.492241753587084219 ) ) ;
#101349 = FILL_AREA_STYLE ('',( #35049 ) ) ;
#101350 = CARTESIAN_POINT ( 'NONE',  ( 6.692428679880670472, -4.002209756868618129, 6.852332176615682613 ) ) ;
#101351 = ADVANCED_FACE ( 'NONE', ( #58642 ), #30861, .F. ) ;
#101352 = DIRECTION ( 'NONE',  ( -3.469446951953614189E-16, 1.000000000000000000, 0.000000000000000000 ) ) ;
#101353 = CARTESIAN_POINT ( 'NONE',  ( 8.763463954874110229, 132.4016268868458326, 5.000000000000000888 ) ) ;
#101354 = EDGE_LOOP ( 'NONE', ( #67260, #27979, #86844, #50585 ) ) ;
#101355 = DIRECTION ( 'NONE',  ( 0.000000000000000000, 0.000000000000000000, 1.000000000000000000 ) ) ;
#101356 = ADVANCED_BREP_SHAPE_REPRESENTATION ( '', ( #88119, #10728 ), #90114 ) ;
#101357 = CARTESIAN_POINT ( 'NONE',  ( 7.493262089825916128, 40.00000000068802564, -69.66935728187972643 ) ) ;
#101358 = CARTESIAN_POINT ( 'NONE',  ( 33.09999999999999432, 1.533819458162526451E-15, 0.000000000000000000 ) ) ;
#101359 = VERTEX_POINT ( 'NONE', #57017 ) ;
#101360 = CARTESIAN_POINT ( 'NONE',  ( -30.47697434215580259, 313.1714974985160325, -7.033864211245149711 ) ) ;
#101361 = CIRCLE ( 'NONE', #68651, 9.999999999999998224 ) ;
#101362 = CARTESIAN_POINT ( 'NONE',  ( -35.82079281205172805, 304.5878133820737617, 4.193256625072890209 ) ) ;
#101363 = CARTESIAN_POINT ( 'NONE',  ( 1.666670260708756013, -30.00000000000001066, 28.88807923168612746 ) ) ;
#101364 = CARTESIAN_POINT ( 'NONE',  ( -1.469576158976823947E-15, -23.37499999999999289, 8.000000000000000000 ) ) ;
#101365 = CARTESIAN_POINT ( 'NONE',  ( -8.000000000000000000, -20.74999999999999289, -9.797174393178825657E-16 ) ) ;
#101366 = CARTESIAN_POINT ( 'NONE',  ( -52.00049474763441992, -30.00000000000002132, 50.03028121960383601 ) ) ;
#101367 = STYLED_ITEM ( 'NONE', ( #69256 ), #2836 ) ;
#101368 = CARTESIAN_POINT ( 'NONE',  ( 99.75754961941544252, 1.030564683017419500E-14, 0.000000000000000000 ) ) ;
#101369 = AXIS2_PLACEMENT_3D ( 'NONE', #29064, #18832, #53804 ) ;
#101370 = ORIENTED_EDGE ( 'NONE', *, *, #31985, .F. ) ;
#101371 = CARTESIAN_POINT ( 'NONE',  ( 84.21780330469050568, -46.56204000551604594, 185.3552051814339166 ) ) ;
#101372 = CARTESIAN_POINT ( 'NONE',  ( 0.000000000000000000, 0.000000000000000000, 1.734723475976807094E-15 ) ) ;
#101373 = CARTESIAN_POINT ( 'NONE',  ( 5.947762761376474749, 6.880090707843042885, -1.083333333333333037 ) ) ;
#101374 = ORIENTED_EDGE ( 'NONE', *, *, #26991, .F. ) ;
#101375 = CARTESIAN_POINT ( 'NONE',  ( -85.41117724271114753, -45.26541568431846230, 38.51296887745267128 ) ) ;
#101376 = CARTESIAN_POINT ( 'NONE',  ( 0.000000000000000000, 0.000000000000000000, -4.874849604647447876 ) ) ;
#101377 = DIRECTION ( 'NONE',  ( -0.5000000000000025535, 0.8660254037844371533, 0.000000000000000000 ) ) ;
#101378 = CARTESIAN_POINT ( 'NONE',  ( 19.73463816634110657, 304.7971333121958537, 8.925379062039144884 ) ) ;
#101379 = CARTESIAN_POINT ( 'NONE',  ( -14.01098147192283783, -23.76418724810895000, -38.53464035791351705 ) ) ;
#101380 = EDGE_CURVE ( 'NONE', #96063, #52601, #35720, .T. ) ;
#101381 = CARTESIAN_POINT ( 'NONE',  ( 50.69148081940352313, -60.00000000000004263, 73.54746023732971594 ) ) ;
#101382 = MECHANICAL_DESIGN_GEOMETRIC_PRESENTATION_REPRESENTATION (  '', ( #94474 ), #23885 ) ;
#101383 = CARTESIAN_POINT ( 'NONE',  ( 29.74370370787013584, -32.27977560020801207, 40.42837052529171871 ) ) ;
#101384 =( GEOMETRIC_REPRESENTATION_CONTEXT ( 3 ) GLOBAL_UNCERTAINTY_ASSIGNED_CONTEXT ( ( #79734 ) ) GLOBAL_UNIT_ASSIGNED_CONTEXT ( ( #92927, #28239, #10410 ) ) REPRESENTATION_CONTEXT ( 'NONE', 'WORKASPACE' ) );
#101385 = CARTESIAN_POINT ( 'NONE',  ( 7.551560007654694928, 108.0091035180699350, -2.648022159607841708 ) ) ;
#101386 = CARTESIAN_POINT ( 'NONE',  ( 10.53029844143175531, -13.89981288703387641, 31.86682902241898319 ) ) ;
#101387 = CONICAL_SURFACE ( 'NONE', #44587, 5.000000000000001776, 0.9599310885968803664 ) ;
#101388 = ADVANCED_FACE ( 'NONE', ( #91544 ), #70849, .T. ) ;
#101390 = CARTESIAN_POINT ( 'NONE',  ( -10.35489345913581616, 16.95138009610748497, 9.903898274887804831 ) ) ;
#101389 = CARTESIAN_POINT ( 'NONE',  ( -2.499999999999996447, -17.75175104828353057, -25.82778608236962015 ) ) ;
#101391 = CARTESIAN_POINT ( 'NONE',  ( 2.569942032970752077, 295.6515237735611095, -10.00266688365501544 ) ) ;
#101392 = CARTESIAN_POINT ( 'NONE',  ( 36.91281931599076671, 303.7809130842520631, -7.959270006439831846 ) ) ;
#101393 = VECTOR ( 'NONE', #78566, 1000.000000000000000 ) ;
#101394 = DIRECTION ( 'NONE',  ( -1.000000000000000000, -0.000000000000000000, -0.000000000000000000 ) ) ;
#101395 = VERTEX_POINT ( 'NONE', #45647 ) ;
#101396 = FACE_OUTER_BOUND ( 'NONE', #92847, .T. ) ;
#101397 = FILL_AREA_STYLE ('',( #54818 ) ) ;
#101398 = EDGE_LOOP ( 'NONE', ( #1239, #36201, #103339, #27448 ) ) ;
#101399 = DIRECTION ( 'NONE',  ( 0.000000000000000000, -1.000000000000000000, 0.000000000000000000 ) ) ;
#101400 = CARTESIAN_POINT ( 'NONE',  ( 46.00000000000000000, 488.0336798547363628, -0.8984331811833941028 ) ) ;
#101401 = CARTESIAN_POINT ( 'NONE',  ( 37.06599482039754889, 437.8929527013448819, 4.336831230556377648 ) ) ;
#101403 = CARTESIAN_POINT ( 'NONE',  ( 25.91305494270541843, -60.22838175289183482, -35.60186180949625623 ) ) ;
#101402 = CARTESIAN_POINT ( 'NONE',  ( 9.165151389911702751, 250.2631950629487960, 4.000000000000000000 ) ) ;
#101404 = ORIENTED_EDGE ( 'NONE', *, *, #62779, .T. ) ;
#101405 = CIRCLE ( 'NONE', #41120, 1.000000000000002442 ) ;
#101406 = CYLINDRICAL_SURFACE ( 'NONE', #54941, 8.000000000000000000 ) ;
#101407 = DIRECTION ( 'NONE',  ( -0.000000000000000000, 1.000000000000000000, -0.000000000000000000 ) ) ;
#101408 = AXIS2_PLACEMENT_3D ( 'NONE', #7567, #57706, #39964 ) ;
#101409 = ORIENTED_EDGE ( 'NONE', *, *, #4552, .F. ) ;
#101410 = EDGE_CURVE ( 'NONE', #88641, #20459, #79065, .T. ) ;
#101411 = CARTESIAN_POINT ( 'NONE',  ( 80.97977184163765685, -5.000000000000000888, 6.123233995736779101E-16 ) ) ;
#101412 = AXIS2_PLACEMENT_3D ( 'NONE', #36254, #27093, #75049 ) ;
#101413 = CARTESIAN_POINT ( 'NONE',  ( -6.492510984469592294, 41.78432685485347520, -59.03546988472429291 ) ) ;
#101414 = STYLED_ITEM ( 'NONE', ( #27145 ), #43529 ) ;
#101415 = DIRECTION ( 'NONE',  ( 1.000000000000000000, 0.000000000000000000, 0.000000000000000000 ) ) ;
#101416 = CARTESIAN_POINT ( 'NONE',  ( -94.39869318582654500, -60.00000000000000711, 44.50543556059614048 ) ) ;
#101417 = DIRECTION ( 'NONE',  ( -0.5735764363510497121, 0.8191520442889892450, 1.003171929053521665E-16 ) ) ;
#101418 = CARTESIAN_POINT ( 'NONE',  ( 46.36650669486618881, 4.000000000000003553, 4.898587196589414801E-16 ) ) ;
#101419 = CARTESIAN_POINT ( 'NONE',  ( 41.59697046779439233, 465.5819587124576628, 15.80766635430880918 ) ) ;
#101421 = PRESENTATION_STYLE_ASSIGNMENT (( #3789 ) ) ;
#101420 = CARTESIAN_POINT ( 'NONE',  ( 0.000000000000000000, -3.000000000000002665, -75.00000000000001421 ) ) ;
#101422 = STYLED_ITEM ( 'NONE', ( #97971 ), #31256 ) ;
#101423 = CARTESIAN_POINT ( 'NONE',  ( -82.21114147848552989, -49.99081894097567158, 178.5515362787500635 ) ) ;
#101424 = ORIENTED_EDGE ( 'NONE', *, *, #97312, .T. ) ;
#101425 = CARTESIAN_POINT ( 'NONE',  ( -44.20228413058327277, 435.2535421915627012, 14.52187095974274911 ) ) ;
#101426 = VERTEX_POINT ( 'NONE', #47212 ) ;
#101427 = ORIENTED_EDGE ( 'NONE', *, *, #88739, .T. ) ;
#101428 = DIRECTION ( 'NONE',  ( -0.000000000000000000, 1.000000000000000000, 0.000000000000000000 ) ) ;
#101429 = CARTESIAN_POINT ( 'NONE',  ( -7.549954993183457752, -4.999999999999999112, -15.49602501671512833 ) ) ;
#101430 = FILL_AREA_STYLE_COLOUR ( '', #90470 ) ;
#101431 = VERTEX_POINT ( 'NONE', #37590 ) ;
#101432 = CARTESIAN_POINT ( 'NONE',  ( -113.9602498558271719, -57.67115345197749576, 163.9892394128282262 ) ) ;
#101433 = CARTESIAN_POINT ( 'NONE',  ( 6.944371705245976578, -10.53899691424551222, -3.972324460300563409 ) ) ;
#101434 = DIRECTION ( 'NONE',  ( -0.8191520442889909104, 0.000000000000000000, -0.5735764363510472696 ) ) ;
#101435 = CARTESIAN_POINT ( 'NONE',  ( -9.918512371096300129, 101.2071700772945064, -1.297150762882696817 ) ) ;
#101436 = CARTESIAN_POINT ( 'NONE',  ( -16.52732684424165654, 43.98685724163156863, -87.77868211029610279 ) ) ;
#101437 = DIRECTION ( 'NONE',  ( 0.000000000000000000, 1.000000000000000000, 0.000000000000000000 ) ) ;
#101438 = CARTESIAN_POINT ( 'NONE',  ( 95.66379843407523254, -59.99999999999997158, 35.18487050012404893 ) ) ;
#101439 = CARTESIAN_POINT ( 'NONE',  ( -82.63253876390992048, -60.00000000000011369, 201.7050754921980911 ) ) ;
#101440 = CARTESIAN_POINT ( 'NONE',  ( -59.77475626106946294, -39.49178998087817405, 71.62854156836660025 ) ) ;
#101441 = ORIENTED_EDGE ( 'NONE', *, *, #78040, .F. ) ;
#101442 = CARTESIAN_POINT ( 'NONE',  ( 6.879789419156629116, 16.78666415220166996, 1.315101155215614437 ) ) ;
#101443 = ORIENTED_EDGE ( 'NONE', *, *, #43951, .F. ) ;
#101444 = CARTESIAN_POINT ( 'NONE',  ( -104.7020446980512958, -52.71019846712929535, 182.7859787390149222 ) ) ;
#101445 = CARTESIAN_POINT ( 'NONE',  ( 4.401442555609581635E-16, -10.15625000204838457, -7.188101187500000044 ) ) ;
#101446 = CARTESIAN_POINT ( 'NONE',  ( -29.77292113577844646, 13.34857726707550007, -42.10535821593474282 ) ) ;
#101448 = CARTESIAN_POINT ( 'NONE',  ( 14.63429600766766114, 41.99999999961375607, -88.44473994942086392 ) ) ;
#101447 = CIRCLE ( 'NONE', #54924, 10.00000000000000000 ) ;
#101449 = ORIENTED_EDGE ( 'NONE', *, *, #18511, .F. ) ;
#101450 = CARTESIAN_POINT ( 'NONE',  ( 19.49546873405769887, 49.99968197754504473, 60.00409861388182264 ) ) ;
#101451 = CARTESIAN_POINT ( 'NONE',  ( -40.66005888438434823, -59.99999999999998579, 53.02551035700262361 ) ) ;
#101452 = CARTESIAN_POINT ( 'NONE',  ( -1.560777554885082852, -0.03795747330964680671, 101.5963436445145476 ) ) ;
#101453 = CARTESIAN_POINT ( 'NONE',  ( 7.188101187500001821, -11.93750000204838457, -2.977408999572650483 ) ) ;
#101454 = DIRECTION ( 'NONE',  ( 0.000000000000000000, 0.000000000000000000, -1.000000000000000000 ) ) ;
#101455 = DIRECTION ( 'NONE',  ( 0.000000000000000000, 0.000000000000000000, -1.000000000000000000 ) ) ;
#101456 = CARTESIAN_POINT ( 'NONE',  ( 2.220657265734799157, -0.000000000000000000, -16.90652009647985565 ) ) ;
#101457 = CARTESIAN_POINT ( 'NONE',  ( -24.60488647473181345, 306.9835580411500473, 10.41807558718820914 ) ) ;
#101458 = CARTESIAN_POINT ( 'NONE',  ( 9.165151389911679658, 105.0000000000000142, -4.000000000000001776 ) ) ;
#101459 = CARTESIAN_POINT ( 'NONE',  ( 7.000000000000000000, 0.000000000000000000, -8.574621033218877031 ) ) ;
#101460 = EDGE_CURVE ( 'NONE', #17102, #31486, #42598, .T. ) ;
#101461 = CARTESIAN_POINT ( 'NONE',  ( -7.500000000007254641, 42.38482959929934424, -59.14603436866633501 ) ) ;
#101462 = CARTESIAN_POINT ( 'NONE',  ( -30.90958803885418504, -25.60400391790700425, 30.93804380000945287 ) ) ;
#101463 = DIRECTION ( 'NONE',  ( -0.8191520442889924647, 1.003171929053525486E-16, 0.5735764363510451602 ) ) ;
#101464 = CARTESIAN_POINT ( 'NONE',  ( 44.68940265413235835, -36.07226461998735090, 42.37193160774957335 ) ) ;
#101465 = CARTESIAN_POINT ( 'NONE',  ( 5.947762761376472973, 4.378239541354660425, 5.416666666666664298 ) ) ;
#101466 = VECTOR ( 'NONE', #102027, 1000.000000000000000 ) ;
#101467 = CARTESIAN_POINT ( 'NONE',  ( -7.002641335706728754, 86.05087262680835636, 3.868676264653293284 ) ) ;
#101468 = CARTESIAN_POINT ( 'NONE',  ( -89.65333812297674854, -38.52081078200126285, 200.4790887592579054 ) ) ;
#101469 = VERTEX_POINT ( 'NONE', #96850 ) ;
#101471 = CARTESIAN_POINT ( 'NONE',  ( -43.00000000000000000, 436.0987441542287115, 7.567257455462746307 ) ) ;
#101470 = CARTESIAN_POINT ( 'NONE',  ( -16.10099529212900649, 21.87266829489404785, 0.2127561331495561314 ) ) ;
#101472 = CARTESIAN_POINT ( 'NONE',  ( 14.61174433364459802, -59.99999999999999289, 34.00541122474304245 ) ) ;
#101473 = DIRECTION ( 'NONE',  ( 0.000000000000000000, -1.000000000000000000, 0.000000000000000000 ) ) ;
#101474 = CARTESIAN_POINT ( 'NONE',  ( 42.23079339798724163, 460.7352525929352964, 2.726051457480600515 ) ) ;
#101475 = CIRCLE ( 'NONE', #8450, 1.000000000000000888 ) ;
#101476 = CARTESIAN_POINT ( 'NONE',  ( 4.933292146132942868, 41.54835750584369691, -70.57172791956975288 ) ) ;
#101477 = CARTESIAN_POINT ( 'NONE',  ( -18.99999999999999645, -4.000000000000000000, -1.500000000000000000 ) ) ;
#101478 = CARTESIAN_POINT ( 'NONE',  ( -23.05315642362847584, 305.6756567056184508, 9.116243019785128965 ) ) ;
#101479 = CARTESIAN_POINT ( 'NONE',  ( 32.15496997666741663, 435.6577922786089516, 19.42935975044838415 ) ) ;
#101480 = CARTESIAN_POINT ( 'NONE',  ( 112.1766375600363403, -60.00000000000000711, 169.0515973596464221 ) ) ;
#101481 = EDGE_CURVE ( 'NONE', #1725, #20836, #98131, .T. ) ;
#101482 = CARTESIAN_POINT ( 'NONE',  ( 30.00000000000000000, 0.000000000000000000, 4.999999999999999112 ) ) ;
#101483 = ORIENTED_EDGE ( 'NONE', *, *, #233, .T. ) ;
#101484 = CARTESIAN_POINT ( 'NONE',  ( 2.122576366385977575, -49.78385856110771357, 102.5552564100475763 ) ) ;
#101485 = B_SPLINE_CURVE_WITH_KNOTS ( 'NONE', 3,
 ( #51861, #93408, #26059, #36271, #10859, #18468, #76668, #2781 ),
 .UNSPECIFIED., .F., .F.,
 ( 4, 2, 2, 4 ),
 ( 0.000000000000000000, 0.5000000000000000000, 0.7500000000000000000, 1.000000000000000000 ),
 .UNSPECIFIED. ) ;
#101486 = CIRCLE ( 'NONE', #54951, 3.000000000000000000 ) ;
#101487 = CARTESIAN_POINT ( 'NONE',  ( -88.84843115600412489, -30.00000000000000711, 82.20554073122355021 ) ) ;
#101488 = ORIENTED_EDGE ( 'NONE', *, *, #24682, .F. ) ;
#101490 = DIRECTION ( 'NONE',  ( -1.000000000000000000, -1.224606353822377258E-16, -0.000000000000000000 ) ) ;
#101489 = CARTESIAN_POINT ( 'NONE',  ( -79.70867639164802654, -38.76023424625122260, 192.4775466185992627 ) ) ;
#101491 = CARTESIAN_POINT ( 'NONE',  ( 44.46823338009918558, 3.851859888774471706E-31, 5.000000000000001776 ) ) ;
#101492 = CARTESIAN_POINT ( 'NONE',  ( -6.397334739185442487, -2.999999999999999556, 4.916373759799318677 ) ) ;
#101493 = CARTESIAN_POINT ( 'NONE',  ( -33.70427618943709547, 490.4072845429053586, 11.54254722977865733 ) ) ;
#101494 = CARTESIAN_POINT ( 'NONE',  ( 2.977408999572650927, -20.75000000204839523, -7.188101187500001821 ) ) ;
#101495 = CARTESIAN_POINT ( 'NONE',  ( 9.349999999999997868, 3.309500000000003439, 4.052968581778167743E-16 ) ) ;
#101496 = B_SPLINE_CURVE_WITH_KNOTS ( 'NONE', 3,
 ( #18436, #18982, #101976, #51828, #44831, #43223, #36234, #77718, #51291, #76105, #10826, #35700, #2206, #61016, #69106, #28137, #11358, #3829, #69630, #102524 ),
 .UNSPECIFIED., .F., .F.,
 ( 4, 2, 2, 2, 2, 2, 2, 2, 2, 4 ),
 ( 0.002921171163060748248, 0.003426533276933608693, 0.003931895390806470006, 0.004184576447742896325, 0.004437257504679322645, 0.004942619618552173549, 0.005447981732425023586, 0.005953343846297873623, 0.006458705960170724528, 0.006964068074043574565 ),
 .UNSPECIFIED. ) ;
#101497 = CARTESIAN_POINT ( 'NONE',  ( 7.770228158362351145, 1.340359594676612611E-15, 0.000000000000000000 ) ) ;
#101498 = AXIS2_PLACEMENT_3D ( 'NONE', #18147, #52607, #26267 ) ;
#101499 = VERTEX_POINT ( 'NONE', #70453 ) ;
#101500 = CARTESIAN_POINT ( 'NONE',  ( 84.80004317470192632, -22.09711215687178765, 158.8498095341223859 ) ) ;
#101501 = DIRECTION ( 'NONE',  ( -0.7071067811865315855, 0.000000000000000000, 0.7071067811865634489 ) ) ;
#101502 = ORIENTED_EDGE ( 'NONE', *, *, #103875, .T. ) ;
#101503 = DIRECTION ( 'NONE',  ( 0.000000000000000000, 0.000000000000000000, 1.000000000000000000 ) ) ;
#101504 = DIRECTION ( 'NONE',  ( 0.000000000000000000, -0.9137523047315411207, 0.4062717386156671773 ) ) ;
#101505 = DIRECTION ( 'NONE',  ( 0.3048027540951617209, 0.4519649026962606064, 0.8383453988820862568 ) ) ;
#101506 = DIRECTION ( 'NONE',  ( 0.000000000000000000, 1.000000000000000000, -0.000000000000000000 ) ) ;
#101507 = LINE ( 'NONE', #27126, #101466 ) ;
#101508 = PRODUCT ( 'plain washer hardened small grade a_din_Washer DIN 433 - 17 - 300HV', 'plain washer hardened small grade a_din_Washer DIN 433 - 17 - 300HV', '', ( #103767 ) ) ;
#101509 = ORIENTED_EDGE ( 'NONE', *, *, #19652, .T. ) ;
#101510 = EDGE_CURVE ( 'NONE', #63888, #29217, #5488, .T. ) ;
#101511 = LINE ( 'NONE', #68635, #40582 ) ;
#101512 = CARTESIAN_POINT ( 'NONE',  ( -8.786988139152953468E-15, 18.64300841652315910, 38.36521369532682257 ) ) ;
#101513 = CARTESIAN_POINT ( 'NONE',  ( 87.03219043533479748, -39.08529333260427308, 189.1299867071195422 ) ) ;
#101514 = ADVANCED_FACE ( 'NONE', ( #32666 ), #49446, .T. ) ;
#101515 = EDGE_CURVE ( 'NONE', #347, #45425, #40249, .T. ) ;
#101517 = DIRECTION ( 'NONE',  ( 0.000000000000000000, -1.000000000000000000, 0.000000000000000000 ) ) ;
#101516 = CARTESIAN_POINT ( 'NONE',  ( 42.69811214730273718, 434.9611672192513652, 18.34625614733207399 ) ) ;
#101518 = CIRCLE ( 'NONE', #58481, 8.000000000000000000 ) ;
#101519 = CARTESIAN_POINT ( 'NONE',  ( 7.188101187499999156, -25.25000000204839523, 2.977408999572654924 ) ) ;
#101520 = LINE ( 'NONE', #60548, #69800 ) ;
#101521 = DIRECTION ( 'NONE',  ( -0.3893994694819514213, 0.000000000000000000, 0.9210689730781157492 ) ) ;
#101522 = CIRCLE ( 'NONE', #68818, 7.500000000000003553 ) ;
#101523 = SURFACE_SIDE_STYLE ('',( #10890 ) ) ;
#101524 = CONTEXT_DEPENDENT_SHAPE_REPRESENTATION ( #96891, #19992 ) ;
#101525 = ORIENTED_EDGE ( 'NONE', *, *, #60812, .F. ) ;
#101526 = CARTESIAN_POINT ( 'NONE',  ( -34.84618260875176787, 489.9833681528637044, 11.97975507378787619 ) ) ;
#101527 = CARTESIAN_POINT ( 'NONE',  ( 72.85555555555556850, 3.309500000000014541, 0.000000000000000000 ) ) ;
#101528 = CARTESIAN_POINT ( 'NONE',  ( -9.999342726577260976, 7.500940813888675507, 0.000000000000000000 ) ) ;
#101529 = FILL_AREA_STYLE ('',( #77253 ) ) ;
#101530 = EDGE_CURVE ( 'NONE', #66067, #9858, #82235, .T. ) ;
#101531 = ORIENTED_EDGE ( 'NONE', *, *, #106081, .T. ) ;
#101532 = FACE_BOUND ( 'NONE', #34930, .T. ) ;
#101533 = CARTESIAN_POINT ( 'NONE',  ( -4.080003621823601989, 50.00000000000000000, -97.51073764065985472 ) ) ;
#101534 = AXIS2_PLACEMENT_3D ( 'NONE', #83859, #66616, #59070 ) ;
#101535 = ADVANCED_FACE ( 'NONE', ( #74665 ), #99474, .T. ) ;
#101536 = CARTESIAN_POINT ( 'NONE',  ( 32.21158651034458131, 436.2407106940943322, 19.11433863909860875 ) ) ;
#101537 = CARTESIAN_POINT ( 'NONE',  ( -0.5361375818286260309, 8.011584859334254460, -51.63592075595909137 ) ) ;
#101538 = CARTESIAN_POINT ( 'NONE',  ( -34.49859336299155643, 464.8458904554828450, 18.22488476268509316 ) ) ;
#101539 = SURFACE_STYLE_USAGE ( .BOTH. , #52989 ) ;
#101540 = CARTESIAN_POINT ( 'NONE',  ( -102.3495297225788931, -60.00000000000001421, 200.9636531052911721 ) ) ;
#101541 = FILL_AREA_STYLE_COLOUR ( '', #41037 ) ;
#101542 = DIRECTION ( 'NONE',  ( -0.000000000000000000, -0.000000000000000000, -1.000000000000000000 ) ) ;
#101543 = FACE_OUTER_BOUND ( 'NONE', #73736, .T. ) ;
#101544 = EDGE_CURVE ( 'NONE', #96494, #81401, #52925, .T. ) ;
#101545 = DIRECTION ( 'NONE',  ( 0.3934424543256375140, 0.4342828891348778364, 0.8103094515917250718 ) ) ;
#101546 = CARTESIAN_POINT ( 'NONE',  ( -83.34365347161629245, -57.34364429206465275, 189.3595448663711807 ) ) ;
#101547 = ORIENTED_EDGE ( 'NONE', *, *, #57222, .F. ) ;
#101548 = CARTESIAN_POINT ( 'NONE',  ( -10.28624191511829977, 46.12099395432375104, -12.90779740156156841 ) ) ;
#101549 =( BOUNDED_SURFACE ( )  B_SPLINE_SURFACE ( 3, 2, ( 
 ( #12576, #68171, #102127 ),
 ( #94043, #3444, #53060 ),
 ( #101067, #52509, #60112 ),
 ( #44437, #36387, #45512 ) ),
 .UNSPECIFIED., .F., .F., .F. ) 
 B_SPLINE_SURFACE_WITH_KNOTS ( ( 4, 4 ),
 ( 3, 3 ),
 ( -8.673617379884035472E-19, 0.002473307515803177190 ),
 ( 0.000000000000000000, 1.000000000000000000 ),
 .UNSPECIFIED. ) 
 GEOMETRIC_REPRESENTATION_ITEM ( )  RATIONAL_B_SPLINE_SURFACE ( (
 ( 1.000000000000000000, 0.8138888783289754958, 1.000000000000000000),
 ( 1.000000000000000000, 0.8083744009271378594, 1.000000000000000000),
 ( 1.000000000000000000, 0.7997328579908555835, 1.000000000000000000),
 ( 1.000000000000000000, 0.7904469216848438728, 1.000000000000000000) ) ) 
 REPRESENTATION_ITEM ( '' )  SURFACE ( )  );
#101550 = CARTESIAN_POINT ( 'NONE',  ( 1.000000000000000222, -40.48763664057447187, -0.7135409870748585792 ) ) ;
#101551 = CARTESIAN_POINT ( 'NONE',  ( -86.30673588546420660, -60.13456697820941343, 5.314161181627422792 ) ) ;
#101552 = CONICAL_SURFACE ( 'NONE', #80827, 8.000000000000000000, 0.9599310885968911355 ) ;
#101553 = DIRECTION ( 'NONE',  ( 0.000000000000000000, -0.3420201433256725987, -0.9396926207859068736 ) ) ;
#101554 = CARTESIAN_POINT ( 'NONE',  ( -3.547914663864637497, 24.63190979035525885, -5.000000000000000000 ) ) ;
#101555 = CARTESIAN_POINT ( 'NONE',  ( 19.96162532426522773, 302.8116070918645164, 9.928455558879877074 ) ) ;
#101556 = CARTESIAN_POINT ( 'NONE',  ( -5.964242399901850789, -13.95070288504640743, 13.91433285878926007 ) ) ;
#101557 = CARTESIAN_POINT ( 'NONE',  ( -7.754160006507099467, 42.00000000000000711, -59.23741894013591036 ) ) ;
#101558 = CARTESIAN_POINT ( 'NONE',  ( 74.04755006654457361, -14.21045842199432307, 133.5027151116648838 ) ) ;
#101559 =( GEOMETRIC_REPRESENTATION_CONTEXT ( 3 ) GLOBAL_UNCERTAINTY_ASSIGNED_CONTEXT ( ( #37557 ) ) GLOBAL_UNIT_ASSIGNED_CONTEXT ( ( #24732, #58681, #33894 ) ) REPRESENTATION_CONTEXT ( 'NONE', 'WORKASPACE' ) );
#101560 = CARTESIAN_POINT ( 'NONE',  ( -1.446302031375384395E-15, 60.76237703744687479, 11.80995232570204045 ) ) ;
#101561 = CARTESIAN_POINT ( 'NONE',  ( -95.18184656059791848, -59.99999999999997158, -7.511930356246473650 ) ) ;
#101562 = CARTESIAN_POINT ( 'NONE',  ( -75.68663096329835582, -32.54935148169148817, 118.5104710783690791 ) ) ;
#101563 = ORIENTED_EDGE ( 'NONE', *, *, #74402, .F. ) ;
#101564 = CARTESIAN_POINT ( 'NONE',  ( 83.90815637317848541, -29.99999999999993605, 196.6622986253035208 ) ) ;
#101565 = CARTESIAN_POINT ( 'NONE',  ( -43.66105921549289093, 40.83721605545716216, 48.52424057032921212 ) ) ;
#101566 = CARTESIAN_POINT ( 'NONE',  ( 36.29725819348360716, -57.67119622293918013, -42.14310373887633432 ) ) ;
#101567 = ORIENTED_EDGE ( 'NONE', *, *, #72208, .T. ) ;
#101568 = DIRECTION ( 'NONE',  ( 0.000000000000000000, -1.000000000000000000, 0.000000000000000000 ) ) ;
#101569 = CARTESIAN_POINT ( 'NONE',  ( -7.188101187500000933, -23.37500000204838813, -2.977408999572651371 ) ) ;
#101570 = MECHANICAL_DESIGN_GEOMETRIC_PRESENTATION_REPRESENTATION (  '', ( #92938 ), #79157 ) ;
#101571 = CARTESIAN_POINT ( 'NONE',  ( -4.904566723942686224, -7.977572975292544832, 3.460360782932702328 ) ) ;
#101572 = ORIENTED_EDGE ( 'NONE', *, *, #42553, .F. ) ;
#101573 = CARTESIAN_POINT ( 'NONE',  ( -16.14595037822608603, 7.274337365584598203, -6.616591826375523233 ) ) ;
#101574 = EDGE_LOOP ( 'NONE', ( #39855, #66725, #51050, #14167, #66243 ) ) ;
#101575 = CARTESIAN_POINT ( 'NONE',  ( 16.75187969033571989, 34.25544727262119693, 24.30698433968583316 ) ) ;
#101576 = CARTESIAN_POINT ( 'NONE',  ( 47.14730021652958669, 17.20087926883151752, -16.50246546963092698 ) ) ;
#101577 = CARTESIAN_POINT ( 'NONE',  ( -74.75441323975938701, -60.00000000000489564, 191.7171422206980367 ) ) ;
#101578 = DIRECTION ( 'NONE',  ( -0.000000000000000000, -1.000000000000000000, -0.000000000000000000 ) ) ;
#101579 = CARTESIAN_POINT ( 'NONE',  ( -1.320432766682874540E-15, -33.40625000204838813, 7.188101187500000044 ) ) ;
#101580 = CARTESIAN_POINT ( 'NONE',  ( 80.00000000000000000, -60.00000000000000000, -21.09707704303352926 ) ) ;
#101581 = CARTESIAN_POINT ( 'NONE',  ( 1.544427540536530710E-15, -4.285714285714290916, -25.22241582816893057 ) ) ;
#101582 =( LENGTH_UNIT ( ) NAMED_UNIT ( * ) SI_UNIT ( .MILLI., .METRE. ) );
#101583 =( GEOMETRIC_REPRESENTATION_CONTEXT ( 3 ) GLOBAL_UNCERTAINTY_ASSIGNED_CONTEXT ( ( #57036 ) ) GLOBAL_UNIT_ASSIGNED_CONTEXT ( ( #22561, #22014, #39255 ) ) REPRESENTATION_CONTEXT ( 'NONE', 'WORKASPACE' ) );
#101584 = CARTESIAN_POINT ( 'NONE',  ( 7.374560640985523996, 50.00000000000000000, -75.40399789250294305 ) ) ;
#101585 = CARTESIAN_POINT ( 'NONE',  ( -8.000000000000001776, -14.65624999999999467, 3.313708498984759387 ) ) ;
#101587 = EDGE_CURVE ( 'NONE', #26114, #57008, #102891, .T. ) ;
#101586 = UNCERTAINTY_MEASURE_WITH_UNIT (LENGTH_MEASURE( 1.000000000000000082E-05 ), #85448, 'distance_accuracy_value', 'NONE');
#101588 = CONICAL_SURFACE ( 'NONE', #10254, 4.000000000000001776, 0.9599310885968808105 ) ;
#101589 = ORIENTED_EDGE ( 'NONE', *, *, #13782, .F. ) ;
#101590 = PRESENTATION_STYLE_ASSIGNMENT (( #85959 ) ) ;
#101592 = CARTESIAN_POINT ( 'NONE',  ( 33.33570294487471841, -60.30676322309119541, 38.33902022564197409 ) ) ;
#101591 = CARTESIAN_POINT ( 'NONE',  ( 4.523357435794008730, 51.56555634218408812, -8.281338046071601511 ) ) ;
#101593 = CARTESIAN_POINT ( 'NONE',  ( -12.70248734011669356, -4.285714285715063632, 22.03900363279318597 ) ) ;
#101594 = ORIENTED_EDGE ( 'NONE', *, *, #38965, .T. ) ;
#101595 = ADVANCED_FACE ( 'NONE', ( #58512 ), #23942, .F. ) ;
#101596 = CARTESIAN_POINT ( 'NONE',  ( -6.145467199749144349, 47.99999999999998579, -92.99666842398180222 ) ) ;
#101597 = EDGE_CURVE ( 'NONE', #60873, #18742, #100017, .T. ) ;
#101598 = CIRCLE ( 'NONE', #55065, 7.999999999999986677 ) ;
#101600 = CARTESIAN_POINT ( 'NONE',  ( 6.890281281981907924, 41.03680257675737408, -70.85895802599645776 ) ) ;
#101599 =( NAMED_UNIT ( * ) PLANE_ANGLE_UNIT ( ) SI_UNIT ( $, .RADIAN. ) );
#101601 = FACE_OUTER_BOUND ( 'NONE', #83956, .T. ) ;
#101602 = CARTESIAN_POINT ( 'NONE',  ( -43.56126634772117967, 484.2986656255091589, 0.7800160315439713665 ) ) ;
#101603 = CARTESIAN_POINT ( 'NONE',  ( 32.12958771267400948, 464.7275665249413237, 11.12424126545885628 ) ) ;
#101604 = CARTESIAN_POINT ( 'NONE',  ( 0.000000000000000000, -48.44948974278317877, 112.0000000000000000 ) ) ;
#101605 = ORIENTED_EDGE ( 'NONE', *, *, #30692, .T. ) ;
#101606 = AXIS2_PLACEMENT_3D ( 'NONE', #105397, #7745, #64423 ) ;
#101607 = CARTESIAN_POINT ( 'NONE',  ( 92.02827674427864224, -60.00000000000000000, 5.649209357253974773 ) ) ;
#101608 = CARTESIAN_POINT ( 'NONE',  ( 15.59999999999999787, 3.309500000000003439, 4.052968581778167743E-16 ) ) ;
#101609 = ADVANCED_FACE ( 'NONE', ( #2908 ), #8773, .F. ) ;
#101610 = CARTESIAN_POINT ( 'NONE',  ( -36.64547244151101069, 438.4340776271736217, 4.169367496923826799 ) ) ;
#101611 = ADVANCED_FACE ( 'NONE', ( #101628 ), #18063, .F. ) ;
#101612 = CARTESIAN_POINT ( 'NONE',  ( -6.716519851531634444, 41.04202961696241658, -70.96212009813095278 ) ) ;
#101613 = CARTESIAN_POINT ( 'NONE',  ( -46.89590902281747731, 18.03207604453001167, -16.16381118462896183 ) ) ;
#101614 = ORIENTED_EDGE ( 'NONE', *, *, #17456, .T. ) ;
#101615 = CARTESIAN_POINT ( 'NONE',  ( -109.4266139821181838, -29.99999999998669153, 164.9709206702354152 ) ) ;
#101616 = ORIENTED_EDGE ( 'NONE', *, *, #93374, .T. ) ;
#101617 = CARTESIAN_POINT ( 'NONE',  ( 37.56673239365870387, 25.75719283951018923, 10.95617127780998956 ) ) ;
#101618 = SURFACE_SIDE_STYLE ('',( #35858 ) ) ;
#101619 = FACE_OUTER_BOUND ( 'NONE', #36150, .T. ) ;
#101620 = DIRECTION ( 'NONE',  ( 0.000000000000000000, -1.000000000000000000, 0.000000000000000000 ) ) ;
#101621 = CARTESIAN_POINT ( 'NONE',  ( 85.03385216039647787, -52.75405561412956246, -12.86923322555876581 ) ) ;
#101622 = CARTESIAN_POINT ( 'NONE',  ( -30.96957840895870362, 309.3457195621996334, -8.501950603266685391 ) ) ;
#101623 = CARTESIAN_POINT ( 'NONE',  ( -18.61215960593760244, 304.6205012219655828, -10.04916466315146906 ) ) ;
#101624 = AXIS2_PLACEMENT_3D ( 'NONE', #11554, #101651, #54659 ) ;
#101625 = CARTESIAN_POINT ( 'NONE',  ( -17.63720921189712953, 45.00000000000000711, 62.98367185064536500 ) ) ;
#101626 = CARTESIAN_POINT ( 'NONE',  ( 9.646320399536545409, 46.21287003049852871, -13.08069908581829388 ) ) ;
#101627 = ORIENTED_EDGE ( 'NONE', *, *, #86606, .T. ) ;
#101628 = FACE_OUTER_BOUND ( 'NONE', #17608, .T. ) ;
#101629 = ORIENTED_EDGE ( 'NONE', *, *, #75666, .T. ) ;
#101630 = PRESENTATION_STYLE_ASSIGNMENT (( #92999 ) ) ;
#101631 = CARTESIAN_POINT ( 'NONE',  ( 14.34999999999999787, 3.309500000000003439, 0.000000000000000000 ) ) ;
#101633 = ORIENTED_EDGE ( 'NONE', *, *, #42908, .F. ) ;
#101632 = CARTESIAN_POINT ( 'NONE',  ( 35.59999999999999432, 3.309500000000003439, 4.052968581778167743E-16 ) ) ;
#101634 = CARTESIAN_POINT ( 'NONE',  ( 75.82183472299138316, -60.31256542882874072, 141.6087927635422830 ) ) ;
#101635 = ORIENTED_EDGE ( 'NONE', *, *, #48711, .T. ) ;
#101636 = CARTESIAN_POINT ( 'NONE',  ( 1.192997108011318863, -53.99999999871816669, 40.95527494392581502 ) ) ;
#101637 = CARTESIAN_POINT ( 'NONE',  ( -30.00000000000000000, 500.0000000000002274, 0.000000000000000000 ) ) ;
#101638 = CARTESIAN_POINT ( 'NONE',  ( 7.188101187499999156, -23.75000000204838813, 2.977408999572654924 ) ) ;
#101639 = CARTESIAN_POINT ( 'NONE',  ( -72.53004918620850106, -57.66488672193313647, 177.2532351053191348 ) ) ;
#101640 = ORIENTED_EDGE ( 'NONE', *, *, #36564, .T. ) ;
#101641 = AXIS2_PLACEMENT_3D ( 'NONE', #20455, #79681, #13873 ) ;
#101642 = FILL_AREA_STYLE_COLOUR ( '', #86821 ) ;
#101643 = CARTESIAN_POINT ( 'NONE',  ( 104.0197026221604659, -45.28274691081462322, 170.3665903025353430 ) ) ;
#101644 = VECTOR ( 'NONE', #4564, 1000.000000000000000 ) ;
#101645 = CARTESIAN_POINT ( 'NONE',  ( 101.4868948250290259, 5.000000000000023093, 6.123233995736781074E-16 ) ) ;
#101646 = EDGE_CURVE ( 'NONE', #65096, #25050, #87350, .T. ) ;
#101647 = DIRECTION ( 'NONE',  ( 0.000000000000000000, -1.000000000000000000, 0.000000000000000000 ) ) ;
#101648 = CARTESIAN_POINT ( 'NONE',  ( 4.898587196589412829E-16, -19.81250000409677270, -8.000000000000000000 ) ) ;
#101649 = CARTESIAN_POINT ( 'NONE',  ( -46.03754588423731064, -28.64604925653195977, 41.20450600710818634 ) ) ;
#101650 = CARTESIAN_POINT ( 'NONE',  ( 9.177080501238327415, 249.4665305714572696, -3.972956046786645601 ) ) ;
#101651 = DIRECTION ( 'NONE',  ( -1.000000000000000000, -1.224606353822377258E-16, -0.000000000000000000 ) ) ;
#101652 = CARTESIAN_POINT ( 'NONE',  ( 97.24367771952604755, -45.35429863921569904, 193.9807169920567560 ) ) ;
#101653 = DIRECTION ( 'NONE',  ( 0.000000000000000000, 0.000000000000000000, 1.000000000000000000 ) ) ;
#101654 = CARTESIAN_POINT ( 'NONE',  ( 56.22793774957824553, 4.898587196589294500E-16, -4.000000000000007105 ) ) ;
#101655 = ORIENTED_EDGE ( 'NONE', *, *, #40700, .F. ) ;
#101656 = CARTESIAN_POINT ( 'NONE',  ( -3.000704772616793026, -49.56994904094584342, 40.82253472268489958 ) ) ;
#101657 = DIRECTION ( 'NONE',  ( -0.000000000000000000, -1.000000000000000000, -0.000000000000000000 ) ) ;
#101658 = CARTESIAN_POINT ( 'NONE',  ( 0.2960823612032095764, 13.62269841106403589, 49.28347290955902338 ) ) ;
#101659 = VECTOR ( 'NONE', #62235, 1000.000000000000000 ) ;
#101660 = CARTESIAN_POINT ( 'NONE',  ( -85.50673915265689118, -30.00000000000000000, 174.8803046632957034 ) ) ;
#101661 = VERTEX_POINT ( 'NONE', #83833 ) ;
#101662 = AXIS2_PLACEMENT_3D ( 'NONE', #4410, #94504, #12485 ) ;
#101663 = CARTESIAN_POINT ( 'NONE',  ( 83.69418490561940871, -57.54334727501766622, 201.5786063079811186 ) ) ;
#101664 = CARTESIAN_POINT ( 'NONE',  ( 8.737863883542576815, 47.99999999999999289, -90.03618980370899294 ) ) ;
#101666 = CARTESIAN_POINT ( 'NONE',  ( 28.38348711115560263, -28.97649890655438654, -38.24913939007272745 ) ) ;
#101665 = CIRCLE ( 'NONE', #87885, 5.000000000000002665 ) ;
#101667 = CARTESIAN_POINT ( 'NONE',  ( -15.74121454705215051, 22.21713694095602420, -3.427215416360654743 ) ) ;
#101668 = DIRECTION ( 'NONE',  ( 0.000000000000000000, 0.000000000000000000, -1.000000000000000000 ) ) ;
#101669 = CARTESIAN_POINT ( 'NONE',  ( -53.06927891376064821, -60.00000000000000711, 79.84214154986403855 ) ) ;
#101670 = CARTESIAN_POINT ( 'NONE',  ( -1.908195823574487804E-14, -8.660254037844390851, -0.9999999999999974465 ) ) ;
#101671 = EDGE_CURVE ( 'NONE', #102690, #11593, #67201, .T. ) ;
#101672 = AXIS2_PLACEMENT_3D ( 'NONE', #25739, #9480, #58594 ) ;
#101673 = CARTESIAN_POINT ( 'NONE',  ( 64.32759900504497352, 48.00000000000000000, -11.06576400629120549 ) ) ;
#101674 = CARTESIAN_POINT ( 'NONE',  ( -86.30437896728759029, -50.15100290326923016, 191.1588917352661383 ) ) ;
#101675 = ORIENTED_EDGE ( 'NONE', *, *, #15436, .T. ) ;
#101676 = FACE_OUTER_BOUND ( 'NONE', #33719, .T. ) ;
#101677 = CARTESIAN_POINT ( 'NONE',  ( -1.974527876150213856, -18.58613712976008614, 26.98527037229319347 ) ) ;
#101678 = CARTESIAN_POINT ( 'NONE',  ( -37.46539295237194978, 482.0432618190212111, 15.05095727675832684 ) ) ;
#101680 = CARTESIAN_POINT ( 'NONE',  ( 0.000000000000000000, 0.9999999999999943379, 0.000000000000000000 ) ) ;
#101679 = CARTESIAN_POINT ( 'NONE',  ( -31.26587727109280479, 298.8769331254652570, 2.831021014789372625 ) ) ;
#101681 = VERTEX_POINT ( 'NONE', #100546 ) ;
#101682 = B_SPLINE_CURVE_WITH_KNOTS ( 'NONE', 3,
 ( #194, #82742, #16413, #50360, #83795, #67100, #99984, #34764, #26671, #33158, #42815, #41218, #75711, #42276, #1806, #66027, #59550, #25065, #74638, #66558, #83273, #98905, #26155, #15885, #48761, #9362, #7779, #59011, #40684, #18025, #58477, #73571, #90843, #91382, #33686, #106473, #32631, #91900, #41750, #25616, #16960, #49837 ),
 .UNSPECIFIED., .F., .F.,
 ( 4, 2, 2, 2, 2, 2, 2, 2, 2, 2, 2, 2, 2, 2, 2, 2, 2, 2, 2, 2, 4 ),
 ( 0.001097384766869235941, 0.009808348211478244358, 0.01851931165608725061, 0.03594123854530526657, 0.05336316543452327560, 0.06207412887913228011, 0.07078509232374130544, 0.08820701921295932835, 0.1056289461021773235, 0.1143399095467863419, 0.1186953912690908441, 0.1230508729913953325, 0.1274063547136998487, 0.1295840955748520373, 0.1317618364360041983, 0.1328507068665802926, 0.1339395772971563869, 0.1350284477277324813, 0.1361173181583085756, 0.1382950590194607643, 0.1404727998806129252 ),
 .UNSPECIFIED. ) ;
#101683 = CARTESIAN_POINT ( 'NONE',  ( 38.97459859895755585, 491.1625636263767092, 12.12552269506736913 ) ) ;
#101684 = DIRECTION ( 'NONE',  ( -1.000000000000000000, -1.224606353822377258E-16, -0.000000000000000000 ) ) ;
#101685 = CARTESIAN_POINT ( 'NONE',  ( 14.27307692307692299, 1.411358822780289120E-15, 0.000000000000000000 ) ) ;
#101686 = CIRCLE ( 'NONE', #13820, 5.000000000000010658 ) ;
#101687 = CARTESIAN_POINT ( 'NONE',  ( 25.85345068545198544, 295.8771030381062133, -1.779349931180276512 ) ) ;
#101688 = CARTESIAN_POINT ( 'NONE',  ( 45.50145573691759182, 405.2496736015978627, 8.430338687477670234 ) ) ;
#101689 = DIRECTION ( 'NONE',  ( -1.000000000000000000, 0.000000000000000000, 0.000000000000000000 ) ) ;
#101690 = CARTESIAN_POINT ( 'NONE',  ( 10.11650669486618881, 1.474610560812782335E-15, 0.000000000000000000 ) ) ;
#101691 = CARTESIAN_POINT ( 'NONE',  ( 92.03798523278891253, -30.00000000000002842, 46.84723268580137301 ) ) ;
#101692 = CONICAL_SURFACE ( 'NONE', #1809, 3.309500000000007880, 0.9599310885968770357 ) ;
#101693 = CARTESIAN_POINT ( 'NONE',  ( -84.18899188864789096, -18.67328967961437414, 149.2220349266904407 ) ) ;
#101694 = ORIENTED_EDGE ( 'NONE', *, *, #25381, .F. ) ;
#101695 = CARTESIAN_POINT ( 'NONE',  ( 42.79914298582033894, 484.2777690190574162, -1.375851118309875387 ) ) ;
#101696 = CARTESIAN_POINT ( 'NONE',  ( 5.858881034796415754, 253.7858632400298404, 1.317748741875953034 ) ) ;
#101697 = CARTESIAN_POINT ( 'NONE',  ( 53.63544537906832232, -57.67554562530587958, 87.33806224458429313 ) ) ;
#101698 = DIRECTION ( 'NONE',  ( -1.000000000000000000, 0.000000000000000000, 0.000000000000000000 ) ) ;
#101699 = CARTESIAN_POINT ( 'NONE',  ( 40.75098415788840356, 318.6269542384334841, 3.769023074406288476 ) ) ;
#101700 = CARTESIAN_POINT ( 'NONE',  ( 43.72375837489602191, 464.7599263999839536, 7.850687543234091237 ) ) ;
#101701 = ORIENTED_EDGE ( 'NONE', *, *, #25927, .F. ) ;
#101702 = DIRECTION ( 'NONE',  ( 0.000000000000000000, 0.000000000000000000, 1.000000000000000000 ) ) ;
#101703 = CARTESIAN_POINT ( 'NONE',  ( 32.02768009620982070, 439.4026772796270848, 23.60435309139906579 ) ) ;
#101704 = CARTESIAN_POINT ( 'NONE',  ( -2.977408999572650039, -29.18750000204839523, -7.188101187500001821 ) ) ;
#101705 = ORIENTED_EDGE ( 'NONE', *, *, #68360, .T. ) ;
#101706 = DIRECTION ( 'NONE',  ( -1.000000000000000000, -0.000000000000000000, -0.000000000000000000 ) ) ;
#101707 = CARTESIAN_POINT ( 'NONE',  ( 6.914762299961043190, 41.79847487255189264, -69.55926079108232329 ) ) ;
#101708 = CARTESIAN_POINT ( 'NONE',  ( 50.94745919686198476, 50.00000000000000000, -37.05882352941176094 ) ) ;
#101709 = CARTESIAN_POINT ( 'NONE',  ( 6.697918543062176155, -13.04454418786335701, -7.429595805581659107 ) ) ;
#101710 = VECTOR ( 'NONE', #59140, 1000.000000000000000 ) ;
#101711 = ORIENTED_EDGE ( 'NONE', *, *, #87628, .F. ) ;
#101712 = CARTESIAN_POINT ( 'NONE',  ( 27.75240500599559113, -60.00000000000001421, -41.15272815132448869 ) ) ;
#101714 = CARTESIAN_POINT ( 'NONE',  ( 22.40106687016081111, -35.99523339415899414, 30.71253893013516745 ) ) ;
#101713 = CARTESIAN_POINT ( 'NONE',  ( -51.40736910322219444, -29.99999999999990052, 68.09419600167673536 ) ) ;
#101715 = CARTESIAN_POINT ( 'NONE',  ( -6.949531687764044400E-15, 14.17434517210798184, 56.74723269274520021 ) ) ;
#101716 = CARTESIAN_POINT ( 'NONE',  ( -34.86660559149834171, -42.96819926141629509, 35.91443906510038175 ) ) ;
#101717 = UNCERTAINTY_MEASURE_WITH_UNIT (LENGTH_MEASURE( 1.000000000000000082E-05 ), #35068, 'distance_accuracy_value', 'NONE');
#101718 = EDGE_LOOP ( 'NONE', ( #94163, #37007, #22700, #83291, #4870 ) ) ;
#101719 = CARTESIAN_POINT ( 'NONE',  ( -4.551587301587297851, -48.79941684889506348, 104.4018401814738013 ) ) ;
#101720 = CARTESIAN_POINT ( 'NONE',  ( -13.59360248487383771, -56.00807882655470138, 23.64795065864135637 ) ) ;
#101721 = LINE ( 'NONE', #42416, #7827 ) ;
#101722 = CARTESIAN_POINT ( 'NONE',  ( 6.692588830498428898, 7.935834885954428763, -0.04058884017440173020 ) ) ;
#101723 = CARTESIAN_POINT ( 'NONE',  ( 0.5805565836007664515, -7.505553499465142053, -1.357586595304856736E-16 ) ) ;
#101724 = ORIENTED_EDGE ( 'NONE', *, *, #63984, .T. ) ;
#101725 = CARTESIAN_POINT ( 'NONE',  ( -15.51166181318948567, 36.90500793569740523, -23.41746243165360042 ) ) ;
#101726 = VERTEX_POINT ( 'NONE', #26710 ) ;
#101727 = CARTESIAN_POINT ( 'NONE',  ( 92.67046874064129725, -29.99999999999975486, 191.0464373490836749 ) ) ;
#101728 = CARTESIAN_POINT ( 'NONE',  ( 38.73813457942127059, 39.95935930601281427, -54.64964148907081665 ) ) ;
#101730 = CARTESIAN_POINT ( 'NONE',  ( 0.000000000000000000, 0.000000000000000000, 0.000000000000000000 ) ) ;
#101729 = AXIS2_PLACEMENT_3D ( 'NONE', #63431, #7273, #48788 ) ;
#101731 = ADVANCED_FACE ( 'NONE', ( #92449 ), #18605, .T. ) ;
#101732 = CARTESIAN_POINT ( 'NONE',  ( 80.38962007328909465, -30.00000000000000000, -13.30899004357461912 ) ) ;
#101733 = PRESENTATION_LAYER_ASSIGNMENT (  '', '', ( #36327 ) ) ;
#101734 = EDGE_CURVE ( 'NONE', #82760, #92683, #96196, .T. ) ;
#101735 = ORIENTED_EDGE ( 'NONE', *, *, #77384, .F. ) ;
#101736 = ORIENTED_EDGE ( 'NONE', *, *, #104014, .F. ) ;
#101737 = ORIENTED_EDGE ( 'NONE', *, *, #78742, .T. ) ;
#101738 = LINE ( 'NONE', #19809, #19904 ) ;
#101739 = CARTESIAN_POINT ( 'NONE',  ( -34.92499999999994742, 0.000000000000000000, 8.500000000000000000 ) ) ;
#101740 = DIRECTION ( 'NONE',  ( 0.000000000000000000, 0.000000000000000000, 1.000000000000000000 ) ) ;
#101741 = LINE ( 'NONE', #82501, #4563 ) ;
#101742 = DIRECTION ( 'NONE',  ( -1.000000000000000000, -1.224606353822377258E-16, -0.000000000000000000 ) ) ;
#101743 = DIRECTION ( 'NONE',  ( -0.000000000000000000, -1.000000000000000000, -0.000000000000000000 ) ) ;
#101744 = ORIENTED_EDGE ( 'NONE', *, *, #89056, .T. ) ;
#101745 = CARTESIAN_POINT ( 'NONE',  ( -11.99999999999999467, 50.00000000000000000, -86.57079632497432442 ) ) ;
#101746 = AXIS2_PLACEMENT_3D ( 'NONE', #84118, #43129, #2113 ) ;
#101747 = EDGE_LOOP ( 'NONE', ( #7760, #67672, #40388, #11909, #94299 ) ) ;
#101748 = CARTESIAN_POINT ( 'NONE',  ( 75.47013347569310326, -38.35162841314899396, 173.9377833191998661 ) ) ;
#101749 = DIRECTION ( 'NONE',  ( -0.6505632072693953161, 0.6639782930160468277, 0.3686466326319209341 ) ) ;
#101750 = CARTESIAN_POINT ( 'NONE',  ( 23.16176619586232732, 303.5563662793418871, 10.08948326321344524 ) ) ;
#101751 = B_SPLINE_CURVE_WITH_KNOTS ( 'NONE', 3,
 ( #78614, #86221, #71066, #37686, #103438, #71583, #4746, #29589, #62458, #104490, #95350, #30637, #54321, #13877, #87266, #55396, #79685, #13344, #63525, #96424, #88327, #36622, #44688, #77576, #3695, #69487, #102373, #28521 ),
 .UNSPECIFIED., .F., .F.,
 ( 4, 2, 2, 2, 2, 2, 2, 2, 2, 2, 2, 2, 2, 4 ),
 ( 0.006869492556767144154, 0.007098556943535802230, 0.007327621330304460306, 0.007785750103841772123, 0.008702007650916396622, 0.009618265197991021989, 0.01053452274506564736, 0.01145078029214027099, 0.01236703783921489636, 0.01282516661275220730, 0.01328329538628951825, 0.01374142415982682920, 0.01397048854659548381, 0.01419955293336414015 ),
 .UNSPECIFIED. ) ;
#101752 =( GEOMETRIC_REPRESENTATION_CONTEXT ( 3 ) GLOBAL_UNCERTAINTY_ASSIGNED_CONTEXT ( ( #8427 ) ) GLOBAL_UNIT_ASSIGNED_CONTEXT ( ( #25031, #57887, #102490 ) ) REPRESENTATION_CONTEXT ( 'NONE', 'WORKASPACE' ) );
#101753 = CARTESIAN_POINT ( 'NONE',  ( -4.478476647430157165, 249.7264792081795690, 3.992942460563209117 ) ) ;
#101754 = PRODUCT_DEFINITION_SHAPE ( 'NONE', 'NONE',  #106786 ) ;
#101755 = ORIENTED_EDGE ( 'NONE', *, *, #8679, .F. ) ;
#101756 = CARTESIAN_POINT ( 'NONE',  ( 14.54015256618498775, 9.738273119607207207, 5.000000000000000000 ) ) ;
#101757 = CARTESIAN_POINT ( 'NONE',  ( 0.000000000000000000, 50.00000000000000000, 0.000000000000000000 ) ) ;
#101758 = CARTESIAN_POINT ( 'NONE',  ( 5.799999999999999822, -9.237604307034013473, 7.924929828396943928E-16 ) ) ;
#101759 = DIRECTION ( 'NONE',  ( 0.000000000000000000, 0.000000000000000000, -1.000000000000000000 ) ) ;
#101760 = ORIENTED_EDGE ( 'NONE', *, *, #36297, .T. ) ;
#101762 = CARTESIAN_POINT ( 'NONE',  ( 8.000113193197767814, -89.00022638645864959, -0.2613481123984638943 ) ) ;
#101761 = FILL_AREA_STYLE ('',( #36014 ) ) ;
#101763 = CYLINDRICAL_SURFACE ( 'NONE', #29543, 4.000000000000000000 ) ;
#101764 = FACE_OUTER_BOUND ( 'NONE', #82765, .T. ) ;
#101765 = CARTESIAN_POINT ( 'NONE',  ( 4.238124563102311448, 302.8058401784392117, 9.927349086999059935 ) ) ;
#101766 = AXIS2_PLACEMENT_3D ( 'NONE', #44540, #86610, #77430 ) ;
#101767 = CARTESIAN_POINT ( 'NONE',  ( -7.744329845603313167, 101.5371176984654085, -2.018701143083234228 ) ) ;
#101768 = EDGE_CURVE ( 'NONE', #85839, #83401, #102685, .T. ) ;
#101769 = CARTESIAN_POINT ( 'NONE',  ( 2.075968632161881544, 6.306992450856642840, -6.056431503345442557 ) ) ;
#101770 =( REPRESENTATION_RELATIONSHIP ('NONE','NONE', #69581, #7490 ) REPRESENTATION_RELATIONSHIP_WITH_TRANSFORMATION ( #11967 )SHAPE_REPRESENTATION_RELATIONSHIP( ) );
#101771 = CARTESIAN_POINT ( 'NONE',  ( 86.39827197653144708, -17.11905348657290915, 182.3887232808949932 ) ) ;
#101772 = CARTESIAN_POINT ( 'NONE',  ( 16.75187969033515145, 37.11970326878314808, -21.80698433968624528 ) ) ;
#101773 = CARTESIAN_POINT ( 'NONE',  ( -3.422569409892814551, 123.4621055364969919, 5.000000000000000888 ) ) ;
#101774 = VERTEX_POINT ( 'NONE', #12593 ) ;
#101775 =( LENGTH_UNIT ( ) NAMED_UNIT ( * ) SI_UNIT ( .MILLI., .METRE. ) );
#101776 = DIRECTION ( 'NONE',  ( -1.000000000000000000, -0.000000000000000000, -0.000000000000000000 ) ) ;
#101777 = CARTESIAN_POINT ( 'NONE',  ( 13.86650669486618881, 1.474610560812782335E-15, 0.000000000000000000 ) ) ;
#101778 = CARTESIAN_POINT ( 'NONE',  ( 5.000000000000000000, -14.29896967480689440, 12.05578540490725103 ) ) ;
#101779 = CARTESIAN_POINT ( 'NONE',  ( -82.75356297445279097, -30.00000000000000711, 40.85445903543622137 ) ) ;
#101780 = EDGE_CURVE ( 'NONE', #55329, #57292, #92488, .T. ) ;
#101781 = EDGE_CURVE ( 'NONE', #18381, #59052, #79461, .T. ) ;
#101782 = CIRCLE ( 'NONE', #46653, 10.00000000000000178 ) ;
#101783 = FACE_OUTER_BOUND ( 'NONE', #31587, .T. ) ;
#101784 = CARTESIAN_POINT ( 'NONE',  ( 16.75933443583691584, -57.67153105735553709, 41.87489785921763996 ) ) ;
#101786 = DIRECTION ( 'NONE',  ( -0.000000000000000000, 1.000000000000000000, -0.000000000000000000 ) ) ;
#101785 = CARTESIAN_POINT ( 'NONE',  ( 0.000000000000000000, -100.0000000000000000, 0.000000000000000000 ) ) ;
#101787 = CARTESIAN_POINT ( 'NONE',  ( 0.7777777777777741264, -54.00000000000000711, 40.97837836547555668 ) ) ;
#101788 = CARTESIAN_POINT ( 'NONE',  ( -36.26183010482215252, -33.57661459365222356, 34.86165481847040581 ) ) ;
#101789 = CARTESIAN_POINT ( 'NONE',  ( -19.49122775093939808, 50.00000000000002132, 59.91448273658983226 ) ) ;
#101790 = DIRECTION ( 'NONE',  ( 0.5735764363510468256, 0.8191520442889913545, 0.000000000000000000 ) ) ;
#101791 = CARTESIAN_POINT ( 'NONE',  ( 47.78548586219075389, -26.97685489492021205, -28.53356913460428856 ) ) ;
#101792 = ADVANCED_FACE ( 'NONE', ( #70323 ), #3034, .F. ) ;
#101793 = CARTESIAN_POINT ( 'NONE',  ( -26.57524688902023868, -36.00438821441548498, 31.51423073511094941 ) ) ;
#101794 = ORIENTED_EDGE ( 'NONE', *, *, #36130, .F. ) ;
#101795 = CARTESIAN_POINT ( 'NONE',  ( 38.79307744977586481, 485.8212363931093591, -4.896981067619740280 ) ) ;
#101796 = CARTESIAN_POINT ( 'NONE',  ( -15.95769171998673919, -56.88368443177520106, 33.57075391308669765 ) ) ;
#101797 = AXIS2_PLACEMENT_3D ( 'NONE', #15381, #72554, #39152 ) ;
#101798 = ADVANCED_FACE ( 'NONE', ( #62765 ), #26776, .T. ) ;
#101800 = CARTESIAN_POINT ( 'NONE',  ( -43.00000000000000000, 436.5989882784185170, 19.94133085611150591 ) ) ;
#101799 = CARTESIAN_POINT ( 'NONE',  ( -1.249969396200062199, 27.80191114808519615, 39.34173072747167765 ) ) ;
#101801 = ORIENTED_EDGE ( 'NONE', *, *, #80811, .T. ) ;
#101802 = COLOUR_RGB ( '', 0.72549020, 0.75294118, 0.79215686) ;
#101803 = CARTESIAN_POINT ( 'NONE',  ( 20.59999999999999787, 1.533819458162526451E-15, 0.000000000000000000 ) ) ;
#101804 = ORIENTED_EDGE ( 'NONE', *, *, #57500, .F. ) ;
#101805 = CARTESIAN_POINT ( 'NONE',  ( 30.00000000000000000, 0.000000000000000000, 0.000000000000000000 ) ) ;
#101806 = AXIS2_PLACEMENT_3D ( 'NONE', #16062, #106660, #56509 ) ;
#101807 = CARTESIAN_POINT ( 'NONE',  ( 15.20081118350077176, 3.404146808184774997, 3.872164105970431258 ) ) ;
#101808 = CARTESIAN_POINT ( 'NONE',  ( -8.000000000000001776, -23.84375000409677270, 3.313708498984759387 ) ) ;
#101809 = ORIENTED_EDGE ( 'NONE', *, *, #34331, .T. ) ;
#101810 = CARTESIAN_POINT ( 'NONE',  ( 48.02835407290544367, 9.771516447483593382, 16.85535821593427386 ) ) ;
#101811 = FACE_OUTER_BOUND ( 'NONE', #61949, .T. ) ;
#101812 = CARTESIAN_POINT ( 'NONE',  ( 101.3166947854019924, -37.84832686624076103, 187.1998071382763271 ) ) ;
#101813 = CARTESIAN_POINT ( 'NONE',  ( -7.744168461338432508, -6.537459382848431311, 2.019395720771551161 ) ) ;
#101814 = ORIENTED_EDGE ( 'NONE', *, *, #49242, .F. ) ;
#101815 = EDGE_CURVE ( 'NONE', #478, #70516, #85997, .T. ) ;
#101816 = ORIENTED_EDGE ( 'NONE', *, *, #33785, .T. ) ;
#101817 = VERTEX_POINT ( 'NONE', #39018 ) ;
#101818 = CARTESIAN_POINT ( 'NONE',  ( 23.16208212304022851, 304.6450008528781837, 10.10914924364463907 ) ) ;
#101819 = CARTESIAN_POINT ( 'NONE',  ( 7.500000000000007105, 39.99999999999998579, -68.91429205785453860 ) ) ;
#101820 = CARTESIAN_POINT ( 'NONE',  ( -15.05785784214673129, 3.824195276770050445, -4.604276673498571171 ) ) ;
#101821 = VERTEX_POINT ( 'NONE', #5054 ) ;
#101822 = CARTESIAN_POINT ( 'NONE',  ( 101.2019940638598854, 1.030564683017419500E-14, 0.000000000000000000 ) ) ;
#101823 = CARTESIAN_POINT ( 'NONE',  ( -6.458627570771506399, 41.53001914901422964, -70.63868815569685466 ) ) ;
#101824 = CARTESIAN_POINT ( 'NONE',  ( 7.500000000000006217, 39.99999999999998579, -62.89165061482851371 ) ) ;
#101826 = CARTESIAN_POINT ( 'NONE',  ( -80.19169983686356318, -59.99999999999025846, -30.56219965566434738 ) ) ;
#101825 = AXIS2_PLACEMENT_3D ( 'NONE', #73672, #82840, #40253 ) ;
#101827 = DIRECTION ( 'NONE',  ( -1.000000000000000000, -1.224606353822377258E-16, -0.000000000000000000 ) ) ;
#101828 = DIRECTION ( 'NONE',  ( 0.000000000000000000, 0.000000000000000000, -1.000000000000000000 ) ) ;
#101829 = CARTESIAN_POINT ( 'NONE',  ( -5.383907111441308402, 41.54392591541395063, -58.58678640223104139 ) ) ;
#101830 = VECTOR ( 'NONE', #89513, 999.9999999999998863 ) ;
#101831 = CARTESIAN_POINT ( 'NONE',  ( -93.17098673813583787, -59.99999999999997158, -17.95829132299026298 ) ) ;
#101832 = CARTESIAN_POINT ( 'NONE',  ( -8.397840381921547248, 51.60961829421124492, 4.031152949374568806 ) ) ;
#101833 = CARTESIAN_POINT ( 'NONE',  ( -48.81468002507525483, -29.13763464560829419, 45.59164195770564021 ) ) ;
#101834 = AXIS2_PLACEMENT_3D ( 'NONE', #8881, #40718, #100019 ) ;
#101835 = EDGE_LOOP ( 'NONE', ( #13452, #5835, #80022, #99691, #80477, #93576 ) ) ;
#101836 = CARTESIAN_POINT ( 'NONE',  ( 34.83349330513379982, 4.000000000000002665, 0.000000000000000000 ) ) ;
#101837 = PRODUCT ( 'hex bolt gradeab_iso_ISO 4014 - M10 x 100 x 26-S', 'hex bolt gradeab_iso_ISO 4014 - M10 x 100 x 26-S', '', ( #48172 ) ) ;
#101838 = ORIENTED_EDGE ( 'NONE', *, *, #43997, .T. ) ;
#101839 = CARTESIAN_POINT ( 'NONE',  ( -93.93607513590077929, -37.67500921297137495, 192.9510021341835966 ) ) ;
#101840 = CARTESIAN_POINT ( 'NONE',  ( -4.691302026902953948, 301.0269659577480752, -10.01286862727976867 ) ) ;
#101841 = LINE ( 'NONE', #3154, #5198 ) ;
#101842 = VERTEX_POINT ( 'NONE', #102148 ) ;
#101843 = CARTESIAN_POINT ( 'NONE',  ( 4.905018583967742707, 247.9764001432031364, -3.459768807258305490 ) ) ;
#101844 = ORIENTED_EDGE ( 'NONE', *, *, #61667, .T. ) ;
#101845 = CARTESIAN_POINT ( 'NONE',  ( 89.66286304382025207, -29.99999999999339195, -12.38401627152031637 ) ) ;
#101846 = CARTESIAN_POINT ( 'NONE',  ( 48.90276556242013584, 14.54846953981844315, 14.70164374843103339 ) ) ;
#101847 = DIRECTION ( 'NONE',  ( 0.000000000000000000, -0.5000000000000008882, 0.8660254037844381525 ) ) ;
#101848 = CARTESIAN_POINT ( 'NONE',  ( -3.912401218062240282, -11.95583337082086572, -10.32341866952809006 ) ) ;
#101849 = CARTESIAN_POINT ( 'NONE',  ( 47.37019975555959661, 42.00000000000001421, -36.40416150955741870 ) ) ;
#101850 = CARTESIAN_POINT ( 'NONE',  ( 87.02385573829870680, -30.00000000000000000, 183.8029085475771183 ) ) ;
#101851 =( BOUNDED_SURFACE ( )  B_SPLINE_SURFACE ( 3, 2, ( 
 ( #16971, #82752, #8854 ),
 ( #34239, #67110, #99995 ),
 ( #7258, #1816, #102663 ),
 ( #51969, #102122, #19667 ),
 ( #51443, #94038, #75722 ),
 ( #28822, #50899, #59559 ),
 ( #52504, #68721, #100525 ),
 ( #101603, #76781, #69249 ) ),
 .UNSPECIFIED., .F., .F., .F. ) 
 B_SPLINE_SURFACE_WITH_KNOTS ( ( 4, 2, 2, 4 ),
 ( 3, 3 ),
 ( 1.821459649775647449E-17, 0.002244734355330710134, 0.003367101532996056093, 0.004489468710661402052 ),
 ( 0.000000000000000000, 1.000000000000000000 ),
 .UNSPECIFIED. ) 
 GEOMETRIC_REPRESENTATION_ITEM ( )  RATIONAL_B_SPLINE_SURFACE ( (
 ( 1.000000000000000000, 0.8138888783289954798, 1.000000000000000000),
 ( 1.000000000000000000, 0.8201127045485649969, 1.000000000000000000),
 ( 1.000000000000000000, 0.8211215022261788565, 1.000000000000000000),
 ( 1.000000000000000000, 0.8168533336260839217, 1.000000000000000000),
 ( 1.000000000000000000, 0.8144062529165223552, 1.000000000000000000),
 ( 1.000000000000000000, 0.8072737967807479542, 1.000000000000000000),
 ( 1.000000000000000000, 0.8026171117809203226, 1.000000000000000000),
 ( 1.000000000000000000, 0.7964893136846624699, 1.000000000000000000) ) ) 
 REPRESENTATION_ITEM ( '' )  SURFACE ( )  );
#101852 = CARTESIAN_POINT ( 'NONE',  ( -11.04491272560624182, 43.74903401048490537, -13.15179640090838298 ) ) ;
#101853 = EDGE_CURVE ( 'NONE', #21929, #83020, #37573, .T. ) ;
#101854 = CARTESIAN_POINT ( 'NONE',  ( -1.219694214448577840, 36.63054784644727846, 28.81676271875494066 ) ) ;
#101855 = AXIS2_PLACEMENT_3D ( 'NONE', #30529, #20349, #102804 ) ;
#101856 = ORIENTED_EDGE ( 'NONE', *, *, #63976, .F. ) ;
#101857 = ORIENTED_EDGE ( 'NONE', *, *, #60992, .T. ) ;
#101858 = CARTESIAN_POINT ( 'NONE',  ( 54.05082700138242302, -22.16248697930777567, 51.66267588704993585 ) ) ;
#101859 = CARTESIAN_POINT ( 'NONE',  ( 5.971401237478955792, 41.34845901557833514, -58.36201559607086153 ) ) ;
#101860 = EDGE_CURVE ( 'NONE', #49975, #10091, #34096, .T. ) ;
#101861 = CARTESIAN_POINT ( 'NONE',  ( 8.000000000000000000, 9.797174393178825657E-16, -7.424942857142857733 ) ) ;
#101862 = EDGE_LOOP ( 'NONE', ( #43726, #70097, #21889, #97216 ) ) ;
#101863 = CARTESIAN_POINT ( 'NONE',  ( -91.44417391070038548, -38.39049349820264467, -8.093955909943030491 ) ) ;
#101864 = ORIENTED_EDGE ( 'NONE', *, *, #5532, .F. ) ;
#101865 = CARTESIAN_POINT ( 'NONE',  ( 0.5805565836007667846, -3.752776749732578132, -6.500000000000000888 ) ) ;
#101866 = CARTESIAN_POINT ( 'NONE',  ( 109.9455632978033890, -38.35592182039783182, 186.4162405044224613 ) ) ;
#101867 = CARTESIAN_POINT ( 'NONE',  ( 10.43259654054523899, 17.30095377175555527, 9.783482319262313709 ) ) ;
#101868 = CARTESIAN_POINT ( 'NONE',  ( 85.24673747113007494, -52.71308823531107635, 2.599026173514388471 ) ) ;
#101869 = CARTESIAN_POINT ( 'NONE',  ( 41.79722565532031098, 337.2140685331145278, 12.11318237481769877 ) ) ;
#101870 = CARTESIAN_POINT ( 'NONE',  ( 16.52731600354976393, 43.98685737190850631, -87.77869701378344303 ) ) ;
#101871 = CARTESIAN_POINT ( 'NONE',  ( 1.574031687329273232, -6.039084736203306214, -13.77476369213296259 ) ) ;
#101872 = CARTESIAN_POINT ( 'NONE',  ( 6.449804269883600227, -2.701269212709792367, 6.840189325177430391 ) ) ;
#101873 = CONICAL_SURFACE ( 'NONE', #27865, 4.000000000000001776, 0.9599310885968808105 ) ;
#101874 = CARTESIAN_POINT ( 'NONE',  ( -44.26374899283617026, 435.3115877954970188, 11.30001004034635770 ) ) ;
#101875 = CARTESIAN_POINT ( 'NONE',  ( 8.167412539206976518, 112.7208733012430741, 4.999999999998771649 ) ) ;
#101876 = ORIENTED_EDGE ( 'NONE', *, *, #17436, .F. ) ;
#101877 = CARTESIAN_POINT ( 'NONE',  ( 1.125013611802090141, 36.97869928123036942, 27.86412292502800980 ) ) ;
#101878 = CARTESIAN_POINT ( 'NONE',  ( 7.286131463487275362, 40.29425637570631125, -70.75304884496938485 ) ) ;
#101879 = CARTESIAN_POINT ( 'NONE',  ( -32.39662675564067484, 439.6664204692525573, 24.00562780833886123 ) ) ;
#101880 = AXIS2_PLACEMENT_3D ( 'NONE', #91597, #65181, #17708 ) ;
#101881 = VERTEX_POINT ( 'NONE', #53075 ) ;
#101882 = CARTESIAN_POINT ( 'NONE',  ( 0.4964154566687890013, 4.996589667937374912, 7.345652830558757174 ) ) ;
#101883 = CARTESIAN_POINT ( 'NONE',  ( -31.25520399608259936, 324.6763390771653235, 15.30305406351194186 ) ) ;
#101884 = CARTESIAN_POINT ( 'NONE',  ( 33.86650669486618881, 1.474610560812782335E-15, 0.000000000000000000 ) ) ;
#101885 = DIRECTION ( 'NONE',  ( 0.000000000000000000, -1.000000000000000000, 0.000000000000000000 ) ) ;
#101886 = CARTESIAN_POINT ( 'NONE',  ( -8.000000000000001776, -23.65624999999999645, 3.313708498984758943 ) ) ;
#101887 = AXIS2_PLACEMENT_3D ( 'NONE', #70528, #3132, #2585 ) ;
#101888 = VECTOR ( 'NONE', #102839, 1000.000000000000227 ) ;
#101889 = EDGE_CURVE ( 'NONE', #7556, #88346, #101206, .T. ) ;
#101890 = CARTESIAN_POINT ( 'NONE',  ( 38.38188837495465577, 437.9257690784075407, 4.300778830038875178 ) ) ;
#101891 = VERTEX_POINT ( 'NONE', #41131 ) ;
#101892 = CARTESIAN_POINT ( 'NONE',  ( 84.33144613566925329, -42.97469618036930683, 183.3463168981145657 ) ) ;
#101893 = FACE_OUTER_BOUND ( 'NONE', #10939, .T. ) ;
#101894 = ORIENTED_EDGE ( 'NONE', *, *, #89523, .T. ) ;
#101895 = CARTESIAN_POINT ( 'NONE',  ( -98.81514710444544392, -52.71022382344329316, 115.6151661280325840 ) ) ;
#101896 = DIRECTION ( 'NONE',  ( 0.000000000000000000, 0.1409055682474881777, -0.9900230405585784821 ) ) ;
#101897 = CARTESIAN_POINT ( 'NONE',  ( 13.73780227957584898, -5.000000000000002665, -78.37846873787442803 ) ) ;
#101898 = CARTESIAN_POINT ( 'NONE',  ( 19.29515645702225868, 1.482358050883964840E-15, 0.000000000000000000 ) ) ;
#101899 = CARTESIAN_POINT ( 'NONE',  ( -8.929954440217160894, -22.36709864391503544, -38.54354848803745170 ) ) ;
#101900 = ADVANCED_FACE ( 'NONE', ( #32534 ), #48669, .T. ) ;
#101901 = VECTOR ( 'NONE', #10804, 999.9999999999998863 ) ;
#101902 = CARTESIAN_POINT ( 'NONE',  ( 29.47384080531130124, -60.00000000000000711, 42.78219204235330153 ) ) ;
#101903 = CIRCLE ( 'NONE', #64130, 10.00000000000000178 ) ;
#101904 = CARTESIAN_POINT ( 'NONE',  ( 33.03637614824300073, -34.39509796229107508, 42.57305433018176188 ) ) ;
#101905 = CARTESIAN_POINT ( 'NONE',  ( 2.230802491789480424, -0.1854892370859804462, 102.4842558203776974 ) ) ;
#101906 = CARTESIAN_POINT ( 'NONE',  ( 52.01278122997629794, -29.95930541098613631, 50.12252116197368679 ) ) ;
#101908 = CARTESIAN_POINT ( 'NONE',  ( -13.03669973157214557, 19.28101993133772041, 7.786058856550787333 ) ) ;
#101907 = CARTESIAN_POINT ( 'NONE',  ( -34.19577669012690535, -35.06686992932695546, 43.52267011995650137 ) ) ;
#101909 = AXIS2_PLACEMENT_3D ( 'NONE', #76805, #85447, #69278 ) ;
#101910 = CARTESIAN_POINT ( 'NONE',  ( 4.598202642359287218, 296.0917469168782077, -10.00877229851196404 ) ) ;
#101911 = CARTESIAN_POINT ( 'NONE',  ( 5.082755093536325930, -9.968750002048384573, -5.082755093536325042 ) ) ;
#101912 = CARTESIAN_POINT ( 'NONE',  ( 42.68131856673817026, 337.5603479645903917, 8.268498401259357422 ) ) ;
#101913 = DIRECTION ( 'NONE',  ( 0.8191520442889884679, 0.000000000000000000, 0.5735764363510508224 ) ) ;
#101914 = ORIENTED_EDGE ( 'NONE', *, *, #36499, .F. ) ;
#101915 = CARTESIAN_POINT ( 'NONE',  ( -19.07845090537422550, 294.6331628770684574, 9.890526070132905190 ) ) ;
#101916 = CARTESIAN_POINT ( 'NONE',  ( -17.49999999999997513, 51.99978697404923622, 59.99316026186820494 ) ) ;
#101917 = ORIENTED_EDGE ( 'NONE', *, *, #103398, .F. ) ;
#101918 =( NAMED_UNIT ( * ) PLANE_ANGLE_UNIT ( ) SI_UNIT ( $, .RADIAN. ) );
#101919 = DIRECTION ( 'NONE',  ( 0.000000000000000000, -1.000000000000000000, -0.000000000000000000 ) ) ;
#101920 = ADVANCED_FACE ( 'NONE', ( #49202 ), #104148, .T. ) ;
#101921 = CARTESIAN_POINT ( 'NONE',  ( 1.540719842239331561, -21.77031602692093060, -30.51804812785477594 ) ) ;
#101922 = EDGE_LOOP ( 'NONE', ( #72355, #30115, #55780 ) ) ;
#101923 = CARTESIAN_POINT ( 'NONE',  ( 27.72595153895140996, 36.41251212665846282, 9.903912806810659220 ) ) ;
#101924 = CARTESIAN_POINT ( 'NONE',  ( 1.000000000000000444, -5.000000000000000000, -14.14213562373095101 ) ) ;
#101925 = VERTEX_POINT ( 'NONE', #12331 ) ;
#101926 = EDGE_CURVE ( 'NONE', #59443, #11535, #42677, .T. ) ;
#101927 =( NAMED_UNIT ( * ) SI_UNIT ( $, .STERADIAN. ) SOLID_ANGLE_UNIT ( ) );
#101928 = LINE ( 'NONE', #92776, #100177 ) ;
#101929 = FACE_OUTER_BOUND ( 'NONE', #88425, .T. ) ;
#101930 = CARTESIAN_POINT ( 'NONE',  ( -91.95502790194899490, -60.00000000000000000, 7.220182617842619166 ) ) ;
#101931 = ORIENTED_EDGE ( 'NONE', *, *, #50288, .F. ) ;
#101932 = CARTESIAN_POINT ( 'NONE',  ( -8.000000000000000000, -25.34374999999999645, -3.313708498984762496 ) ) ;
#101933 = DIRECTION ( 'NONE',  ( 0.000000000000000000, 0.000000000000000000, -1.000000000000000000 ) ) ;
#101934 = LINE ( 'NONE', #64029, #36440 ) ;
#101935 = CARTESIAN_POINT ( 'NONE',  ( -3.867083106916794133, -48.81750179905139220, 103.9715359882822270 ) ) ;
#101937 = FACE_OUTER_BOUND ( 'NONE', #73895, .T. ) ;
#101936 = CARTESIAN_POINT ( 'NONE',  ( -5.036189802311206165, -3.000000000000002665, -76.26213611587844809 ) ) ;
#101938 = CARTESIAN_POINT ( 'NONE',  ( -81.85053211555002406, -46.45651121556473839, 170.1952362726539150 ) ) ;
#101939 = VERTEX_POINT ( 'NONE', #53338 ) ;
#101940 = CARTESIAN_POINT ( 'NONE',  ( -7.540179673743359068, -0.000000000000000000, -15.29468310208057602 ) ) ;
#101942 = EDGE_CURVE ( 'NONE', #45881, #106169, #27511, .T. ) ;
#101941 = CIRCLE ( 'NONE', #22753, 5.000000000000011546 ) ;
#101943 = ORIENTED_EDGE ( 'NONE', *, *, #27739, .F. ) ;
#101944 = AXIS2_PLACEMENT_3D ( 'NONE', #17400, #97751, #99890 ) ;
#101945 = ORIENTED_EDGE ( 'NONE', *, *, #55874, .T. ) ;
#101946 = CARTESIAN_POINT ( 'NONE',  ( 14.99896353599399923, -4.999999999999999112, 9.191463535713378263 ) ) ;
#101947 = CARTESIAN_POINT ( 'NONE',  ( 33.86879232827773478, 484.1347737343853623, 1.564974661443952364 ) ) ;
#101948 = DIRECTION ( 'NONE',  ( -0.000000000000000000, 1.000000000000000000, 0.000000000000000000 ) ) ;
#101949 = ORIENTED_EDGE ( 'NONE', *, *, #50056, .F. ) ;
#101950 = CARTESIAN_POINT ( 'NONE',  ( -57.15598917327103834, -57.67115757216583205, -38.38010944898898202 ) ) ;
#101951 = CARTESIAN_POINT ( 'NONE',  ( -4.813555570991610466, -66.79473796517321205, -3.584128953194789968 ) ) ;
#101952 = CARTESIAN_POINT ( 'NONE',  ( 5.510910596163103361E-16, 200.0000000000000000, -2.000000000000011102 ) ) ;
#101953 = CARTESIAN_POINT ( 'NONE',  ( -13.72589306172073442, -50.98891492079946630, 29.76321791924474525 ) ) ;
#101954 = VECTOR ( 'NONE', #66971, 1000.000000000000227 ) ;
#101955 = CARTESIAN_POINT ( 'NONE',  ( 90.56091889802806350, -29.99999999999993960, 34.47026654395114775 ) ) ;
#101956 = MECHANICAL_DESIGN_GEOMETRIC_PRESENTATION_REPRESENTATION (  '', ( #65844 ), #60655 ) ;
#101957 = CARTESIAN_POINT ( 'NONE',  ( -81.96434049221993234, -29.99999999999993250, 194.6677479149438454 ) ) ;
#101958 = CARTESIAN_POINT ( 'NONE',  ( -55.22263546528215272, -49.91236510178273988, 65.08345786281854828 ) ) ;
#101959 = ORIENTED_EDGE ( 'NONE', *, *, #60766, .F. ) ;
#101960 = DIRECTION ( 'NONE',  ( 1.000000000000000000, 0.000000000000000000, 0.000000000000000000 ) ) ;
#101961 = ORIENTED_EDGE ( 'NONE', *, *, #1086, .F. ) ;
#101962 = CARTESIAN_POINT ( 'NONE',  ( -102.3679167227413700, -37.82050009904918397, 181.3159907740166830 ) ) ;
#101963 = CARTESIAN_POINT ( 'NONE',  ( -7.188101187500000933, -9.875000002048388126, -2.977408999572651371 ) ) ;
#101964 = CARTESIAN_POINT ( 'NONE',  ( 7.999999999999998224, -18.78125000409677270, 3.313708498984766049 ) ) ;
#101965 = CARTESIAN_POINT ( 'NONE',  ( 4.404050688260422675, -29.99999999999999289, 5.685839403562723327 ) ) ;
#101966 = ORIENTED_EDGE ( 'NONE', *, *, #899, .T. ) ;
#101967 = CARTESIAN_POINT ( 'NONE',  ( 5.693345023037156949, -5.000000000005900169, -71.09407786877757474 ) ) ;
#101968 = CARTESIAN_POINT ( 'NONE',  ( 8.000000000000000000, 0.000000000000000000, 3.469446951953614189E-15 ) ) ;
#101969 = CARTESIAN_POINT ( 'NONE',  ( -3.352941176470596307, -1.200583151104958279, 104.5794940929807524 ) ) ;
#101970 = CARTESIAN_POINT ( 'NONE',  ( -1.320432766682874540E-15, -16.90625000204838813, 7.188101187500000044 ) ) ;
#101971 = CARTESIAN_POINT ( 'NONE',  ( 0.000000000000000000, 47.00000000000000000, 0.000000000000000000 ) ) ;
#101972 = FACE_OUTER_BOUND ( 'NONE', #47366, .T. ) ;
#101973 = CARTESIAN_POINT ( 'NONE',  ( -11.51551999166614060, -4.933705119235564318, -12.56689034858084497 ) ) ;
#101974 = FACE_OUTER_BOUND ( 'NONE', #25651, .T. ) ;
#101975 = CARTESIAN_POINT ( 'NONE',  ( -9.613206415764745216, 8.856620616597396634, 0.000000000000000000 ) ) ;
#101976 = CARTESIAN_POINT ( 'NONE',  ( -16.32527301256094177, 45.99414959098179168, -4.187920679398874135 ) ) ;
#101977 = EDGE_CURVE ( 'NONE', #82359, #9383, #102973, .T. ) ;
#101978 = DIRECTION ( 'NONE',  ( 0.000000000000000000, 1.000000000000000000, 0.000000000000000000 ) ) ;
#101979 = UNCERTAINTY_MEASURE_WITH_UNIT (LENGTH_MEASURE( 1.000000000000000082E-05 ), #13568, 'distance_accuracy_value', 'NONE');
#101980 = CARTESIAN_POINT ( 'NONE',  ( -29.54167733814598407, -22.11927707116958075, 29.86409302364821627 ) ) ;
#101981 = AXIS2_PLACEMENT_3D ( 'NONE', #18287, #76486, #82462 ) ;
#101982 = CARTESIAN_POINT ( 'NONE',  ( 104.0908829527487711, 1.030564683017419500E-14, 0.000000000000000000 ) ) ;
#101983 = CARTESIAN_POINT ( 'NONE',  ( 48.50725277660750834, -53.36040862114389682, 52.77151552700934189 ) ) ;
#101984 = CARTESIAN_POINT ( 'NONE',  ( -7.500000000000000000, -4.330127018922201643, -10.00000000000000000 ) ) ;
#101985 = EDGE_CURVE ( 'NONE', #62254, #77573, #20346, .T. ) ;
#101986 = FACE_OUTER_BOUND ( 'NONE', #96853, .T. ) ;
#101987 = VECTOR ( 'NONE', #66641, 1000.000000000000000 ) ;
#101988 = CARTESIAN_POINT ( 'NONE',  ( -100.6822085231046344, -38.46011006933861864, 200.2742388691330291 ) ) ;
#101989 = ORIENTED_EDGE ( 'NONE', *, *, #15999, .F. ) ;
#101991 = CARTESIAN_POINT ( 'NONE',  ( -28.28142067734527032, 36.39280011943776572, 8.376232292823662107 ) ) ;
#101990 = DIRECTION ( 'NONE',  ( -1.000000000000000000, -1.224606353822377258E-16, -0.000000000000000000 ) ) ;
#101992 = PRESENTATION_STYLE_ASSIGNMENT (( #37299 ) ) ;
#101993 = CARTESIAN_POINT ( 'NONE',  ( -19.24979913086533756, 49.81992999154532242, 61.45847795212542763 ) ) ;
#101994 = CARTESIAN_POINT ( 'NONE',  ( 41.50820411079195793, 461.5963371455320612, 2.703439750996331270 ) ) ;
#101995 = CARTESIAN_POINT ( 'NONE',  ( 6.238189707152653973, 40.55825190858245577, -71.19044262412266733 ) ) ;
#101996 = CARTESIAN_POINT ( 'NONE',  ( 85.31310517497098544, -2.002967142162725287E-29, 5.000000000000011546 ) ) ;
#101997 = DIRECTION ( 'NONE',  ( -1.000000000000000000, -0.000000000000000000, -0.000000000000000000 ) ) ;
#101999 = COLOUR_RGB ( '', 0.08235294, 0.09019608, 0.10196078) ;
#101998 = CARTESIAN_POINT ( 'NONE',  ( -9.970195021759442611, 302.6460196488377505, -10.04373974541436887 ) ) ;
#102000 = CARTESIAN_POINT ( 'NONE',  ( 108.8655680065974423, -60.00000000000000711, 193.9842112700635539 ) ) ;
#102001 = CARTESIAN_POINT ( 'NONE',  ( -7.619701877737479201, -68.17442159532767221, -2.447562251315981374 ) ) ;
#102002 = ORIENTED_EDGE ( 'NONE', *, *, #28265, .F. ) ;
#102003 = EDGE_CURVE ( 'NONE', #58472, #44553, #94338, .T. ) ;
#102004 = CARTESIAN_POINT ( 'NONE',  ( 0.9999999999999940048, -50.00000000000000000, 101.0455488498966758 ) ) ;
#102005 = CARTESIAN_POINT ( 'NONE',  ( -79.26773016923658588, -29.99999999999997868, -14.68326225543056829 ) ) ;
#102006 = VERTEX_POINT ( 'NONE', #621 ) ;
#102008 = CARTESIAN_POINT ( 'NONE',  ( 5.296353609480505931, 19.09562013799879310, -38.40621394496536567 ) ) ;
#102007 = SURFACE_SIDE_STYLE ('',( #20629 ) ) ;
#102009 = FACE_OUTER_BOUND ( 'NONE', #83294, .T. ) ;
#102010 = CARTESIAN_POINT ( 'NONE',  ( 1.589967640017929007, -5.000000000000000000, -16.33935305251328884 ) ) ;
#102011 = CARTESIAN_POINT ( 'NONE',  ( 5.082755093536324154, -15.21875000204838457, 5.082755093536326818 ) ) ;
#102012 = CARTESIAN_POINT ( 'NONE',  ( -7.374560640982810611, -5.000000000000002665, -94.59600210748614302 ) ) ;
#102013 = CARTESIAN_POINT ( 'NONE',  ( 11.84999999999999787, 1.533819458162526451E-15, 0.000000000000000000 ) ) ;
#102015 = EDGE_LOOP ( 'NONE', ( #1164, #33560 ) ) ;
#102014 = CARTESIAN_POINT ( 'NONE',  ( -33.21587117934102196, 465.5376285004398937, 9.463823683521015440 ) ) ;
#102016 = CARTESIAN_POINT ( 'NONE',  ( 81.30317062471358724, -53.43848046224103143, 176.1350280067906624 ) ) ;
#102017 = CARTESIAN_POINT ( 'NONE',  ( 45.36923076923077502, 1.411358822780289120E-15, 0.000000000000000000 ) ) ;
#102018 = CARTESIAN_POINT ( 'NONE',  ( 10.00004721872059932, 89.00011804681153649, -0.2617599822266505338 ) ) ;
#102019 = ORIENTED_EDGE ( 'NONE', *, *, #40608, .T. ) ;
#102020 = STYLED_ITEM ( 'NONE', ( #34549 ), #83037 ) ;
#102021 = DIRECTION ( 'NONE',  ( 1.000000000000000000, 1.224606353822377258E-16, 0.000000000000000000 ) ) ;
#102022 = CARTESIAN_POINT ( 'NONE',  ( 0.000000000000000000, 50.00000000000000000, -97.00000000000000000 ) ) ;
#102023 = DIRECTION ( 'NONE',  ( -1.000000000000000000, -0.000000000000000000, -0.000000000000000000 ) ) ;
#102024 =( LENGTH_UNIT ( ) NAMED_UNIT ( * ) SI_UNIT ( .MILLI., .METRE. ) );
#102025 = MECHANICAL_DESIGN_GEOMETRIC_PRESENTATION_REPRESENTATION (  '', ( #31383 ), #62400 ) ;
#102026 = DIRECTION ( 'NONE',  ( 0.000000000000000000, -1.000000000000000000, 0.000000000000000000 ) ) ;
#102027 = DIRECTION ( 'NONE',  ( -0.000000000000000000, -0.000000000000000000, 1.000000000000000000 ) ) ;
#102028 = CARTESIAN_POINT ( 'NONE',  ( 7.386188840451400672, -0.04421783097938639107, 19.15859931866217636 ) ) ;
#102029 = ORIENTED_EDGE ( 'NONE', *, *, #78695, .F. ) ;
#102030 = SURFACE_STYLE_USAGE ( .BOTH. , #85329 ) ;
#102032 = CARTESIAN_POINT ( 'NONE',  ( -5.715859758579841632, 297.8165492175919553, 8.222449063051152862 ) ) ;
#102031 = AXIS2_PLACEMENT_3D ( 'NONE', #99042, #83942, #25210 ) ;
#102033 = DIRECTION ( 'NONE',  ( 0.000000000000000000, -1.000000000000000000, 0.000000000000000000 ) ) ;
#102034 = CARTESIAN_POINT ( 'NONE',  ( 14.62354047171442772, 22.28742650378891810, 3.920645538799723884 ) ) ;
#102035 = B_SPLINE_CURVE_WITH_KNOTS ( 'NONE', 3,
 ( #104693, #24345, #38780, #81994, #81457, #7571, #87997, #64771, #73368, #79881, #98190, #56659, #57187, #90103, #63731, #14075, #64258, #8112 ),
 .UNSPECIFIED., .F., .F.,
 ( 4, 2, 2, 2, 2, 2, 2, 2, 4 ),
 ( 0.000000000000000000, 0.06250000000001418310, 0.1250000000000283662, 0.1875000000000425493, 0.2500000000000567324, 0.3125000000000709433, 0.3750000000000852096, 0.4375000000000994205, 0.5000000000001136868 ),
 .UNSPECIFIED. ) ;
#102037 = CARTESIAN_POINT ( 'NONE',  ( -14.04769764157139988, 4.430073480882096071, -5.212240267777101366 ) ) ;
#102036 = FACE_OUTER_BOUND ( 'NONE', #24327, .T. ) ;
#102038 = CARTESIAN_POINT ( 'NONE',  ( -7.188101187500002709, -27.31250000204838457, 2.977408999572648707 ) ) ;
#102039 = DIRECTION ( 'NONE',  ( 0.000000000000000000, 0.000000000000000000, 1.000000000000000000 ) ) ;
#102040 = DIRECTION ( 'NONE',  ( -1.000000000000000000, -1.224606353822377258E-16, -0.000000000000000000 ) ) ;
#102041 = CARTESIAN_POINT ( 'NONE',  ( 14.95520043898952345, 4.194724623210972503, 5.164345506890690274 ) ) ;
#102042 = ORIENTED_EDGE ( 'NONE', *, *, #55610, .T. ) ;
#102043 = CARTESIAN_POINT ( 'NONE',  ( -37.38583316527437717, 490.8443774175583485, 12.40598127368437531 ) ) ;
#102044 = CARTESIAN_POINT ( 'NONE',  ( -8.824767335732170537, 18.31512251393273161, -4.999999999999364952 ) ) ;
#102045 = COLOUR_RGB ( '', 0.40784314, 0.44705882, 0.49803922) ;
#102046 = CARTESIAN_POINT ( 'NONE',  ( 0.000000000000000000, 38.19193163660327173, 24.55262289886175964 ) ) ;
#102047 = ADVANCED_FACE ( 'NONE', ( #58371 ), #45957, .F. ) ;
#102048 = PRESENTATION_LAYER_ASSIGNMENT (  '', '', ( #10796 ) ) ;
#102049 = EDGE_LOOP ( 'NONE', ( #104142, #47437, #87013, #76262, #94849 ) ) ;
#102050 = EDGE_CURVE ( 'NONE', #8349, #81897, #46828, .T. ) ;
#102051 = CARTESIAN_POINT ( 'NONE',  ( 34.89131925218347874, 463.6463204812255867, 18.89898487466263077 ) ) ;
#102052 = CARTESIAN_POINT ( 'NONE',  ( -12.13034742782427955, 48.00000000000000000, -93.82352941176471006 ) ) ;
#102053 = AXIS2_PLACEMENT_3D ( 'NONE', #26678, #36379, #3964 ) ;
#102054 = ORIENTED_EDGE ( 'NONE', *, *, #32843, .F. ) ;
#102055 = EDGE_CURVE ( 'NONE', #61410, #100984, #104540, .T. ) ;
#102056 = CARTESIAN_POINT ( 'NONE',  ( 31.80017143950496106, 436.0492156885775330, 18.01770255577284630 ) ) ;
#102057 = DIRECTION ( 'NONE',  ( -1.000000000000000000, -1.224606353822377258E-16, -0.000000000000000000 ) ) ;
#102058 = CARTESIAN_POINT ( 'NONE',  ( 9.948513602187993854, 101.1302205665614053, 1.045942665286139439 ) ) ;
#102059 =( NAMED_UNIT ( * ) PLANE_ANGLE_UNIT ( ) SI_UNIT ( $, .RADIAN. ) );
#102060 = UNCERTAINTY_MEASURE_WITH_UNIT (LENGTH_MEASURE( 1.000000000000000082E-05 ), #23306, 'distance_accuracy_value', 'NONE');
#102061 = CARTESIAN_POINT ( 'NONE',  ( -111.3761741217465300, -60.00000000000000711, 185.3197500022033068 ) ) ;
#102062 = CARTESIAN_POINT ( 'NONE',  ( 19.45524037106658355, 49.98193815142445118, 60.61134026581003553 ) ) ;
#102063 = CIRCLE ( 'NONE', #55547, 3.000000000000000000 ) ;
#102064 = SURFACE_SIDE_STYLE ('',( #35237 ) ) ;
#102065 = CARTESIAN_POINT ( 'NONE',  ( -86.34263362178202783, -18.09246414803421033, 171.9745557676415615 ) ) ;
#102066 = SURFACE_STYLE_USAGE ( .BOTH. , #61096 ) ;
#102067 = EDGE_CURVE ( 'NONE', #99464, #23643, #38758, .T. ) ;
#102068 = ORIENTED_EDGE ( 'NONE', *, *, #47265, .F. ) ;
#102069 = CARTESIAN_POINT ( 'NONE',  ( -9.088913997560085889, 46.11732115646235286, -13.78939345329818877 ) ) ;
#102070 = CARTESIAN_POINT ( 'NONE',  ( 32.33349330513379982, 4.000000000000002665, 0.000000000000000000 ) ) ;
#102071 = CARTESIAN_POINT ( 'NONE',  ( -83.93095737769149878, -45.26970912266205005, 3.740156994664543877 ) ) ;
#102072 = DIRECTION ( 'NONE',  ( -1.000000000000000000, -1.224606353822377258E-16, -0.000000000000000000 ) ) ;
#102073 = CARTESIAN_POINT ( 'NONE',  ( 9.075061003900238177, 137.9460510617556679, -5.000000000000000888 ) ) ;
#102074 = CARTESIAN_POINT ( 'NONE',  ( -5.960000261375883568, -13.79916237020877112, 13.82526581198430016 ) ) ;
#102075 = CARTESIAN_POINT ( 'NONE',  ( -45.60838156032659896, 42.00000000000000000, 79.13121736029036413 ) ) ;
#102076 = CARTESIAN_POINT ( 'NONE',  ( 66.64731328016637235, -30.00000000000005684, 114.0820693445010363 ) ) ;
#102077 = CARTESIAN_POINT ( 'NONE',  ( -23.61990465140407380, 60.76237703744687479, -11.80995232570204223 ) ) ;
#102078 = CARTESIAN_POINT ( 'NONE',  ( -73.46108764834735894, -30.00000000000002132, -28.33320811291743269 ) ) ;
#102079 = CARTESIAN_POINT ( 'NONE',  ( -67.57911227637399065, -53.38914766505263998, 101.9919822544095638 ) ) ;
#102080 = ORIENTED_EDGE ( 'NONE', *, *, #26631, .F. ) ;
#102081 = CARTESIAN_POINT ( 'NONE',  ( 97.75109942996037660, -59.99999999999985789, 204.9114775063931120 ) ) ;
#102082 = CARTESIAN_POINT ( 'NONE',  ( 5.937976208022995195, 40.83857947417038758, 64.79749893865751176 ) ) ;
#102083 = VERTEX_POINT ( 'NONE', #29626 ) ;
#102084 = CARTESIAN_POINT ( 'NONE',  ( 80.91739486121119285, -57.67116913187329885, -29.69084684708537125 ) ) ;
#102085 = ORIENTED_EDGE ( 'NONE', *, *, #56141, .F. ) ;
#102086 = CARTESIAN_POINT ( 'NONE',  ( 13.90377727273328645, -57.59477087426256503, 25.34355585267129740 ) ) ;
#102087 = CARTESIAN_POINT ( 'NONE',  ( 2.977408999572650927, -26.75000000204838457, -7.188101187500000933 ) ) ;
#102088 = CIRCLE ( 'NONE', #98685, 4.000000000000001776 ) ;
#102089 = CARTESIAN_POINT ( 'NONE',  ( -5.092539576892243680, -7.556765327915675456, 3.177249149099054204 ) ) ;
#102090 = EDGE_LOOP ( 'NONE', ( #623, #53194, #81183, #86198, #90676, #10544 ) ) ;
#102091 = FACE_OUTER_BOUND ( 'NONE', #45291, .T. ) ;
#102092 = ORIENTED_EDGE ( 'NONE', *, *, #85360, .F. ) ;
#102093 = DIRECTION ( 'NONE',  ( 0.000000000000000000, 0.000000000000000000, 1.000000000000000000 ) ) ;
#102094 = PRESENTATION_LAYER_ASSIGNMENT (  '', '', ( #69404 ) ) ;
#102095 = DIRECTION ( 'NONE',  ( -1.000000000000000000, -0.000000000000000000, -0.000000000000000000 ) ) ;
#102096 = CARTESIAN_POINT ( 'NONE',  ( -92.21698522519400854, -60.00000000000001421, -12.99394316321618703 ) ) ;
#102097 = CARTESIAN_POINT ( 'NONE',  ( -11.38818291378892056, 43.57520507334620419, 13.48712730654634662 ) ) ;
#102098 = CARTESIAN_POINT ( 'NONE',  ( -7.188101187500000044, -33.78125000204838813, -8.802885111219163269E-16 ) ) ;
#102099 = CARTESIAN_POINT ( 'NONE',  ( 31.84999999999999787, -3.309499999999999886, 0.000000000000000000 ) ) ;
#102100 =( GEOMETRIC_REPRESENTATION_CONTEXT ( 3 ) GLOBAL_UNCERTAINTY_ASSIGNED_CONTEXT ( ( #6356 ) ) GLOBAL_UNIT_ASSIGNED_CONTEXT ( ( #52707, #102868, #61360 ) ) REPRESENTATION_CONTEXT ( 'NONE', 'WORKASPACE' ) );
#102101 = DIRECTION ( 'NONE',  ( 0.000000000000000000, 0.000000000000000000, 1.000000000000000000 ) ) ;
#102102 = CARTESIAN_POINT ( 'NONE',  ( 63.81650669486618455, 6.856755485862130937E-15, 0.000000000000000000 ) ) ;
#102103 =( NAMED_UNIT ( * ) SI_UNIT ( $, .STERADIAN. ) SOLID_ANGLE_UNIT ( ) );
#102104 = CARTESIAN_POINT ( 'NONE',  ( -7.999912353029506207, 108.9998247060309069, -0.2691822806795004519 ) ) ;
#102105 = CARTESIAN_POINT ( 'NONE',  ( 38.55706197333972085, 437.0914394628474611, 4.833655886047981909 ) ) ;
#102106 = EDGE_CURVE ( 'NONE', #38679, #16973, #18308, .T. ) ;
#102107 = ORIENTED_EDGE ( 'NONE', *, *, #8530, .F. ) ;
#102108 = CARTESIAN_POINT ( 'NONE',  ( 4.051286199644066777, -1.398729870307594547, 103.8758286790405094 ) ) ;
#102109 = STYLED_ITEM ( 'NONE', ( #97211 ), #20943 ) ;
#102111 = CARTESIAN_POINT ( 'NONE',  ( 33.78548833840188337, -56.83387574824190835, 37.94913980780508211 ) ) ;
#102110 = FACE_OUTER_BOUND ( 'NONE', #47885, .T. ) ;
#102112 = EDGE_LOOP ( 'NONE', ( #83250, #42110, #30400, #85654 ) ) ;
#102113 = EDGE_CURVE ( 'NONE', #7306, #76519, #75390, .T. ) ;
#102114 = EDGE_CURVE ( 'NONE', #75855, #4655, #9290, .T. ) ;
#102115 = CARTESIAN_POINT ( 'NONE',  ( 35.04348997865178461, 484.2371297655228091, -0.9829126381495068010 ) ) ;
#102117 = CARTESIAN_POINT ( 'NONE',  ( -32.11411341898570981, 317.7919323371296514, -6.873671351699469412 ) ) ;
#102116 = CARTESIAN_POINT ( 'NONE',  ( -25.88429648623745649, 35.08523104449947283, -8.490101697507606460 ) ) ;
#102118 = CARTESIAN_POINT ( 'NONE',  ( 28.58349330513380337, 1.593028355512270962E-15, 0.000000000000000000 ) ) ;
#102119 = CARTESIAN_POINT ( 'NONE',  ( 8.113285044351216187E-15, 80.00000000000000000, 66.00000000000000000 ) ) ;
#102120 = SURFACE_STYLE_FILL_AREA ( #46024 ) ;
#102121 = DIRECTION ( 'NONE',  ( 0.000000000000000000, -1.000000000000000000, 0.000000000000000000 ) ) ;
#102122 = CARTESIAN_POINT ( 'NONE',  ( 32.65869381073299138, 465.0820644893343569, 12.85946116546466200 ) ) ;
#102123 = DIRECTION ( 'NONE',  ( 0.02699252395738975518, -0.001721171576548164101, 0.9996341536876447442 ) ) ;
#102124 = ORIENTED_EDGE ( 'NONE', *, *, #57377, .F. ) ;
#102125 = CARTESIAN_POINT ( 'NONE',  ( 92.68197952148119612, -59.99999999999999289, -4.372387793708037762 ) ) ;
#102126 = CARTESIAN_POINT ( 'NONE',  ( -11.49350100829453325, 45.59260286365996961, -13.79671030421808098 ) ) ;
#102127 = CARTESIAN_POINT ( 'NONE',  ( 32.28552837373270279, 464.7648866755952213, 15.30384310833110462 ) ) ;
#102128 = CARTESIAN_POINT ( 'NONE',  ( -35.68994829237247757, 432.5459415766960092, 4.686749143785717386 ) ) ;
#102129 = VECTOR ( 'NONE', #61349, 1000.000000000000000 ) ;
#102130 = CARTESIAN_POINT ( 'NONE',  ( -6.870940789805455751, 40.00000000008640200, -71.15487332242412322 ) ) ;
#102131 = CARTESIAN_POINT ( 'NONE',  ( -11.59786760126457139, 15.72211884272761750, -9.649684760468234757 ) ) ;
#102132 = ORIENTED_EDGE ( 'NONE', *, *, #58479, .T. ) ;
#102133 = EDGE_CURVE ( 'NONE', #68169, #77582, #79727, .T. ) ;
#102134 = STYLED_ITEM ( 'NONE', ( #12604 ), #38340 ) ;
#102135 = CARTESIAN_POINT ( 'NONE',  ( -109.6056691518176649, -30.00000000000000000, 173.1093856131147959 ) ) ;
#102136 = ORIENTED_EDGE ( 'NONE', *, *, #41694, .F. ) ;
#102137 = CARTESIAN_POINT ( 'NONE',  ( -9.822490609848976817, -57.47042247602874454, 25.11095637839896000 ) ) ;
#102138 = SURFACE_SIDE_STYLE ('',( #54101 ) ) ;
#102139 = DIRECTION ( 'NONE',  ( -1.000000000000000000, -0.000000000000000000, -0.000000000000000000 ) ) ;
#102140 = CARTESIAN_POINT ( 'NONE',  ( 16.13469797932767946, 21.10829079392559393, -3.392296823476807610 ) ) ;
#102141 = CARTESIAN_POINT ( 'NONE',  ( 85.09962800393060434, -60.19390250260627084, -15.90040431203298255 ) ) ;
#102142 = TOROIDAL_SURFACE ( 'NONE', #36670, 11.00000000000000000, 2.000000000000000000 ) ;
#102143 = CARTESIAN_POINT ( 'NONE',  ( -1.320432766682874540E-15, -28.90625000204838813, 7.188101187500000044 ) ) ;
#102144 = CARTESIAN_POINT ( 'NONE',  ( -17.77115019406404173, 34.18919163712646281, 23.80020659827771112 ) ) ;
#102145 = CARTESIAN_POINT ( 'NONE',  ( 9.041225629235734473, 45.95386998337555440, -14.35441598012803510 ) ) ;
#102146 = ORIENTED_EDGE ( 'NONE', *, *, #36786, .T. ) ;
#102147 = EDGE_CURVE ( 'NONE', #41373, #104078, #92982, .T. ) ;
#102148 = CARTESIAN_POINT ( 'NONE',  ( -33.74271564777242816, 484.1802673187708592, 2.058285076122308155 ) ) ;
#102149 = ORIENTED_EDGE ( 'NONE', *, *, #22873, .T. ) ;
#102150 = CARTESIAN_POINT ( 'NONE',  ( 17.50000000000002842, 45.00000000000000711, 64.09953197936602010 ) ) ;
#102151 = FILL_AREA_STYLE_COLOUR ( '', #12844 ) ;
#102153 = EDGE_CURVE ( 'NONE', #57881, #84797, #53674, .T. ) ;
#102152 = B_SPLINE_CURVE_WITH_KNOTS ( 'NONE', 3,
 ( #55464, #392, #98591, #75380, #91588, #75919, #919, #25832, #100194, #26359, #66772, #83475, #16083, #1479, #89979, #33899, #33359, #57586, #48963, #81861, #58136, #59220, #99660, #17170, #34443, #8519, #84014, #10120, #43030, #58686, #9574, #50557, #67313, #50041, #82951, #91062 ),
 .UNSPECIFIED., .F., .F.,
 ( 4, 2, 2, 2, 2, 2, 2, 2, 2, 2, 2, 2, 2, 2, 2, 2, 2, 4 ),
 ( 0.000000000000000000, 0.0008074604767267243646, 0.001614920953453448729, 0.002422381430180173094, 0.003229841906906897459, 0.004037302383633621823, 0.004844762860360346188, 0.005652223337087070552, 0.006459683813813794917, 0.007267144290540519282, 0.008074604767267243646, 0.008882065243993968878, 0.009689525720720692376, 0.01049698619744741587, 0.01130444667417414110, 0.01211190715090086634, 0.01251563738926422809, 0.01291936762762758983 ),
 .UNSPECIFIED. ) ;
#102155 = ORIENTED_EDGE ( 'NONE', *, *, #103458, .F. ) ;
#102154 = CARTESIAN_POINT ( 'NONE',  ( 29.66054107240687543, 1.482358050883964840E-15, 0.000000000000000000 ) ) ;
#102156 = CARTESIAN_POINT ( 'NONE',  ( 79.60872795848992212, -29.08772644578209210, 133.2594084639777634 ) ) ;
#102157 = ORIENTED_EDGE ( 'NONE', *, *, #20017, .F. ) ;
#102158 = CARTESIAN_POINT ( 'NONE',  ( 4.408087643829541769, -52.50239862025969018, 40.28907920670494036 ) ) ;
#102159 = CARTESIAN_POINT ( 'NONE',  ( 7.188101187499999156, -19.25000000204838457, 2.977408999572654924 ) ) ;
#102160 =( BOUNDED_CURVE ( )  B_SPLINE_CURVE ( 3, ( #75074, #33592, #73480, #48674, #106379, #9281, #103, #67015, #81558, #99896, #33072, #7685, #90752, #83702 ),
 .UNSPECIFIED., .F., .T. ) 
 B_SPLINE_CURVE_WITH_KNOTS ( ( 4, 2, 2, 2, 2, 2, 4 ),
 ( 0.5000000000031382674, 0.5892633092116352778, 0.6785266184232030540, 0.7677899276347708302, 0.8570532368463388284, 0.9463165460579068267, 1.000000000000000000 ),
 .UNSPECIFIED. ) 
 CURVE ( )  GEOMETRIC_REPRESENTATION_ITEM ( )  RATIONAL_B_SPLINE_CURVE ( ( 1.420262811277154924, 1.420262811277154924, 1.420262811277154924, 1.420262811277154924, 1.420262811277154924, 1.420262811277154924, 1.420262811277154924, 1.420262811277154924, 1.420262811277154924, 1.420262811277154924, 1.420262811277154924, 1.420262811277154924, 1.420262811277154924, 1.420262811277154924 ) ) 
 REPRESENTATION_ITEM ( '' )  );
#102161 = CARTESIAN_POINT ( 'NONE',  ( -111.5786317092108533, -57.67087409935591324, 192.6842770035980834 ) ) ;
#102162 = ORIENTED_EDGE ( 'NONE', *, *, #16463, .T. ) ;
#102163 = FILL_AREA_STYLE_COLOUR ( '', #36738 ) ;
#102164 = CARTESIAN_POINT ( 'NONE',  ( -4.478476647430159829, -10.27352079182045941, 3.992942460563206009 ) ) ;
#102165 = CARTESIAN_POINT ( 'NONE',  ( -36.35727881789110683, 28.12781631794103276, -12.56218724973182255 ) ) ;
#102166 = EDGE_CURVE ( 'NONE', #46319, #40774, #35789, .T. ) ;
#102167 = CARTESIAN_POINT ( 'NONE',  ( 49.03498469565151652, 14.13689777146936422, -14.86104782056310114 ) ) ;
#102168 = CARTESIAN_POINT ( 'NONE',  ( 5.656854249492380582, -18.50000000409676915, -5.656854249492379694 ) ) ;
#102169 = CARTESIAN_POINT ( 'NONE',  ( -45.45765750525109183, -28.45291710252894646, 40.56146669681922390 ) ) ;
#102170 = FILL_AREA_STYLE ('',( #70345 ) ) ;
#102171 = CIRCLE ( 'NONE', #17801, 12.00000000000000711 ) ;
#102172 = DIRECTION ( 'NONE',  ( 1.150791560227848051E-16, -0.3420201433256733758, 0.9396926207859066515 ) ) ;
#102173 = DIRECTION ( 'NONE',  ( 0.000000000000000000, 0.000000000000000000, 1.000000000000000000 ) ) ;
#102174 = AXIS2_PLACEMENT_3D ( 'NONE', #26739, #43944, #36948 ) ;
#102175 = PRODUCT_CONTEXT ( 'NONE', #1077, 'mechanical' ) ;
#102176 = CARTESIAN_POINT ( 'NONE',  ( 33.88461414431416330, 464.6055380068779073, 6.798187872881690019 ) ) ;
#102177 = ORIENTED_EDGE ( 'NONE', *, *, #86141, .T. ) ;
#102178 = CARTESIAN_POINT ( 'NONE',  ( -3.478182438133638588, -49.25293460592492067, 40.73187655623500092 ) ) ;
#102179 = CARTESIAN_POINT ( 'NONE',  ( 11.64553472616179342, -4.906298272857039677, -12.56112232304452370 ) ) ;
#102180 = MECHANICAL_DESIGN_GEOMETRIC_PRESENTATION_REPRESENTATION (  '', ( #22989 ), #16027 ) ;
#102181 = CYLINDRICAL_SURFACE ( 'NONE', #10097, 8.000000000000000000 ) ;
#102182 = CARTESIAN_POINT ( 'NONE',  ( -23.46280628704403171, -21.90278913687860651, -37.56245478017753214 ) ) ;
#102183 = CARTESIAN_POINT ( 'NONE',  ( -85.49286042444410327, -30.00000000000000711, 174.7639661085288481 ) ) ;
#102184 = EDGE_CURVE ( 'NONE', #21850, #23846, #19245, .T. ) ;
#102185 = ORIENTED_EDGE ( 'NONE', *, *, #35758, .F. ) ;
#102186 = DIRECTION ( 'NONE',  ( 0.000000000000000000, 0.000000000000000000, 1.000000000000000000 ) ) ;
#102187 = AXIS2_PLACEMENT_3D ( 'NONE', #88360, #29109, #39284 ) ;
#102188 = CARTESIAN_POINT ( 'NONE',  ( 75.44058859636598413, -57.56160405487426601, 191.8524245654686240 ) ) ;
#102189 = LINE ( 'NONE', #84950, #34540 ) ;
#102190 = ADVANCED_FACE ( 'NONE', ( #78480 ), #4073, .T. ) ;
#102191 = ADVANCED_FACE ( 'NONE', ( #62321 ), #77958, .T. ) ;
#102192 = CARTESIAN_POINT ( 'NONE',  ( 39.31863996099055214, -32.72901781786905673, -37.51093992367277963 ) ) ;
#102193 = SURFACE_STYLE_FILL_AREA ( #3507 ) ;
#102194 = CARTESIAN_POINT ( 'NONE',  ( 8.737863883542576815, -3.000000000000002665, -79.96381019629100706 ) ) ;
#102195 = CARTESIAN_POINT ( 'NONE',  ( -64.60151486236289031, -60.00000000000001421, 116.7762116740196063 ) ) ;
#102196 = ADVANCED_FACE ( 'NONE', ( #12147 ), #10179, .F. ) ;
#102197 = CARTESIAN_POINT ( 'NONE',  ( -86.41237560483617131, -46.49691307358666137, 190.1354165495773714 ) ) ;
#102199 = ORIENTED_EDGE ( 'NONE', *, *, #32651, .T. ) ;
#102198 = CIRCLE ( 'NONE', #45404, 4.000000000000000000 ) ;
#102200 = CARTESIAN_POINT ( 'NONE',  ( -42.36808196472509280, 461.6713445545159971, 3.771400599640011286 ) ) ;
#102201 = CARTESIAN_POINT ( 'NONE',  ( -4.019156803245598653, -32.51259995193562702, 29.30134738771553415 ) ) ;
#102202 = EDGE_CURVE ( 'NONE', #74698, #75985, #44539, .T. ) ;
#102203 = EDGE_CURVE ( 'NONE', #30000, #81108, #30616, .T. ) ;
#102204 = CARTESIAN_POINT ( 'NONE',  ( -6.849721783289899335, 41.84384191736015168, -59.83401399873645232 ) ) ;
#102205 = CARTESIAN_POINT ( 'NONE',  ( 37.18119764941855721, 491.8021068614486921, 12.56169729800603463 ) ) ;
#102206 = CARTESIAN_POINT ( 'NONE',  ( -7.461489502270862495, 54.13514019874089200, 3.459350134084382855 ) ) ;
#102207 = ORIENTED_EDGE ( 'NONE', *, *, #48393, .T. ) ;
#102208 = CARTESIAN_POINT ( 'NONE',  ( -1.829579891623863134E-15, 10.71892156097790583, -14.93965356295127478 ) ) ;
#102209 = AXIS2_PLACEMENT_3D ( 'NONE', #47117, #32028, #72461 ) ;
#102210 = CARTESIAN_POINT ( 'NONE',  ( 33.00000000000000000, 450.0000000000002274, 13.20242257375370976 ) ) ;
#102211 = CARTESIAN_POINT ( 'NONE',  ( -30.00000000000000000, 500.0000000000002274, 0.000000000000000000 ) ) ;
#102212 = DIRECTION ( 'NONE',  ( 0.5000000000000011102, -0.8660254037844380415, 0.000000000000000000 ) ) ;
#102213 = VECTOR ( 'NONE', #73751, 1000.000000000000000 ) ;
#102214 = EDGE_LOOP ( 'NONE', ( #93189, #12298, #65346, #39444 ) ) ;
#102215 = CARTESIAN_POINT ( 'NONE',  ( 17.58100359019471526, 50.00000000000000000, 62.76922408379542873 ) ) ;
#102216 = CARTESIAN_POINT ( 'NONE',  ( 21.23684446602553777, 304.9566545053270943, -9.977713076987676288 ) ) ;
#102217 = CARTESIAN_POINT ( 'NONE',  ( 15.50035291838848472, -4.285714285715568117, -20.16952962162309859 ) ) ;
#102218 = CARTESIAN_POINT ( 'NONE',  ( 9.166999376131622412, 53.73590836252315484, -1.685805968339065819 ) ) ;
#102219 = CARTESIAN_POINT ( 'NONE',  ( 94.42187179517443951, -29.99999999999998934, 63.29523499578382228 ) ) ;
#102220 = CARTESIAN_POINT ( 'NONE',  ( -83.08186369656709758, -25.62021722390013068, 150.1200563151912775 ) ) ;
#102221 = EDGE_LOOP ( 'NONE', ( #36929, #43706, #1606, #79285 ) ) ;
#102222 = LINE ( 'NONE', #19763, #20626 ) ;
#102223 = CARTESIAN_POINT ( 'NONE',  ( 40.11650669486618881, 4.000000000000003553, 4.898587196589414801E-16 ) ) ;
#102224 = CARTESIAN_POINT ( 'NONE',  ( 5.689865212206615119, -57.67123513422165360, 41.59068566848854687 ) ) ;
#102225 = DIRECTION ( 'NONE',  ( 0.8086898285216187476, 0.000000000000000000, -0.5882352941176471894 ) ) ;
#102226 = CARTESIAN_POINT ( 'NONE',  ( 41.04411817078318592, 313.2288094300998296, -5.615143661017929055 ) ) ;
#102227 = CARTESIAN_POINT ( 'NONE',  ( 43.54570344706467466, 464.5919001250003362, 9.427857144828974967 ) ) ;
#102228 = ORIENTED_EDGE ( 'NONE', *, *, #5485, .F. ) ;
#102229 = UNCERTAINTY_MEASURE_WITH_UNIT (LENGTH_MEASURE( 1.000000000000000082E-05 ), #7662, 'distance_accuracy_value', 'NONE');
#102230 = DIRECTION ( 'NONE',  ( 0.000000000000000000, 1.000000000000000000, 0.000000000000000000 ) ) ;
#102231 = FACE_BOUND ( 'NONE', #8865, .T. ) ;
#102232 = CARTESIAN_POINT ( 'NONE',  ( -7.188101187500002709, -25.81250000204838457, 2.977408999572648707 ) ) ;
#102233 = ORIENTED_EDGE ( 'NONE', *, *, #54405, .F. ) ;
#102234 = FILL_AREA_STYLE ('',( #73145 ) ) ;
#102235 = CARTESIAN_POINT ( 'NONE',  ( -2.797297131808754944, 15.83452282593334282, 9.607612890400021755 ) ) ;
#102236 = CARTESIAN_POINT ( 'NONE',  ( 6.491942738476094377, 41.63185016724582965, -70.49544021083930545 ) ) ;
#102237 = CARTESIAN_POINT ( 'NONE',  ( -22.66220480930539338, 50.00000000000000000, 59.06576954297837290 ) ) ;
#102238 = CARTESIAN_POINT ( 'NONE',  ( -5.656854249492379694, -17.93749999999999645, -5.656854249492380582 ) ) ;
#102239 = DIRECTION ( 'NONE',  ( -1.000000000000000000, 0.000000000000000000, 0.000000000000000000 ) ) ;
#102240 = ORIENTED_EDGE ( 'NONE', *, *, #9605, .T. ) ;
#102241 = CARTESIAN_POINT ( 'NONE',  ( 85.64840212452983792, -60.00000000000000000, -23.98298676833077181 ) ) ;
#102243 = CARTESIAN_POINT ( 'NONE',  ( 22.70406402036928739, -46.43430815227275588, 32.52211750540141111 ) ) ;
#102242 = CARTESIAN_POINT ( 'NONE',  ( -59.93215762506982713, -30.00000000000009592, 91.51900601851320971 ) ) ;
#102244 = CARTESIAN_POINT ( 'NONE',  ( 66.76860190796568872, 46.03420836107012093, -33.38430095398283726 ) ) ;
#102245 = ADVANCED_FACE ( 'NONE', ( #73945 ), #90890, .T. ) ;
#102246 = CARTESIAN_POINT ( 'NONE',  ( -33.88291765572438408, -25.63420728696120676, 32.08181795506389733 ) ) ;
#102247 = UNCERTAINTY_MEASURE_WITH_UNIT (LENGTH_MEASURE( 1.000000000000000082E-05 ), #54432, 'distance_accuracy_value', 'NONE');
#102248 = ORIENTED_EDGE ( 'NONE', *, *, #74585, .F. ) ;
#102249 = CARTESIAN_POINT ( 'NONE',  ( -23.93420880016848074, -4.285714285714295357, -8.127057321558261549 ) ) ;
#102250 = FILL_AREA_STYLE ('',( #5159 ) ) ;
#102251 = CARTESIAN_POINT ( 'NONE',  ( -13.38090213880806978, -54.00000000000000711, 31.11721482942554928 ) ) ;
#102252 = AXIS2_PLACEMENT_3D ( 'NONE', #71949, #28891, #88145 ) ;
#102253 =( NAMED_UNIT ( * ) SI_UNIT ( $, .STERADIAN. ) SOLID_ANGLE_UNIT ( ) );
#102254 = CARTESIAN_POINT ( 'NONE',  ( 0.3760805802986251778, 300.0000000000000000, 9.936999415321508877 ) ) ;
#102255 = CARTESIAN_POINT ( 'NONE',  ( 11.84572884306312979, -1.963608633182635232, 20.63449361704874718 ) ) ;
#102256 = ORIENTED_EDGE ( 'NONE', *, *, #73725, .T. ) ;
#102257 = CARTESIAN_POINT ( 'NONE',  ( -73.92728128053286696, -38.32663353633068226, 159.7396587626866449 ) ) ;
#102258 = CARTESIAN_POINT ( 'NONE',  ( 43.51330286016530380, 435.7669547662781042, 8.554287073368662675 ) ) ;
#102259 = CARTESIAN_POINT ( 'NONE',  ( 97.91342610505886057, -29.99999999999999289, 190.6140529371372452 ) ) ;
#102260 = CARTESIAN_POINT ( 'NONE',  ( 33.03967949176340113, 40.70416129926884707, -62.21519284123854021 ) ) ;
#102261 = AXIS2_PLACEMENT_3D ( 'NONE', #13849, #97966, #96395 ) ;
#102262 = CARTESIAN_POINT ( 'NONE',  ( -4.595881407952572495, -83.93374566798678416, -3.857520671226066789 ) ) ;
#102263 = CARTESIAN_POINT ( 'NONE',  ( 81.33594675399758955, -30.00000000000000355, -1.021767529535129171 ) ) ;
#102264 = AXIS2_PLACEMENT_3D ( 'NONE', #36728, #62560, #79787 ) ;
#102265 = DIRECTION ( 'NONE',  ( -1.160749806054361473E-16, 0.000000000000000000, -1.000000000000000000 ) ) ;
#102266 = ORIENTED_EDGE ( 'NONE', *, *, #27433, .T. ) ;
#102267 = ORIENTED_EDGE ( 'NONE', *, *, #41286, .T. ) ;
#102268 = ORIENTED_EDGE ( 'NONE', *, *, #50642, .T. ) ;
#102269 = CARTESIAN_POINT ( 'NONE',  ( 0.000000000000000000, 50.00000000000000000, -60.00000000000000000 ) ) ;
#102270 = CARTESIAN_POINT ( 'NONE',  ( 28.55297524992865377, 43.39596580573108753, -71.24614888030039594 ) ) ;
#102271 = CARTESIAN_POINT ( 'NONE',  ( 26.36650669486618881, 1.474610560812782335E-15, 0.000000000000000000 ) ) ;
#102272 = CARTESIAN_POINT ( 'NONE',  ( 36.36650669486618881, -3.999999999999998224, 0.000000000000000000 ) ) ;
#102273 = CARTESIAN_POINT ( 'NONE',  ( -31.34146884395068966, 438.6798339901752115, 22.89183309451972548 ) ) ;
#102274 = CARTESIAN_POINT ( 'NONE',  ( -7.212408192734265810, -87.01517089320367404, -3.465038817813880456 ) ) ;
#102275 = CARTESIAN_POINT ( 'NONE',  ( 4.898587196589412829E-16, -13.62499999999999112, -8.000000000000000000 ) ) ;
#102276 = ORIENTED_EDGE ( 'NONE', *, *, #79589, .T. ) ;
#102277 = CARTESIAN_POINT ( 'NONE',  ( 3.140974613991526887, 50.00000000000000000, -73.31232788067644890 ) ) ;
#102278 = ORIENTED_EDGE ( 'NONE', *, *, #42584, .T. ) ;
#102279 =( NAMED_UNIT ( * ) PLANE_ANGLE_UNIT ( ) SI_UNIT ( $, .RADIAN. ) );
#102280 = LINE ( 'NONE', #21396, #5670 ) ;
#102281 = CARTESIAN_POINT ( 'NONE',  ( 5.656854249492380582, -11.00000000409677092, -5.656854249492379694 ) ) ;
#102282 = CARTESIAN_POINT ( 'NONE',  ( 26.04978609391949718, 296.0924368275842653, 10.20507325036795443 ) ) ;
#102283 = ADVANCED_FACE ( 'NONE', ( #65864, #100352 ), #17866, .F. ) ;
#102284 = PLANE ( 'NONE',  #2812 ) ;
#102285 = CARTESIAN_POINT ( 'NONE',  ( 59.69857829083183987, -53.38500049141745052, 78.06181712156276831 ) ) ;
#102286 = PRESENTATION_LAYER_ASSIGNMENT (  '', '', ( #47140 ) ) ;
#102287 = ORIENTED_EDGE ( 'NONE', *, *, #77181, .T. ) ;
#102288 = CARTESIAN_POINT ( 'NONE',  ( 29.59213159313616970, 8.427504962981444692, -42.10535821593531125 ) ) ;
#102289 = CARTESIAN_POINT ( 'NONE',  ( 7.899999792244755348, -11.02739026146943857, -12.99999999999998934 ) ) ;
#102290 = CARTESIAN_POINT ( 'NONE',  ( -6.013174582917088173, 11.20780250015804391, -3.585507868043892987 ) ) ;
#102291 = CONICAL_SURFACE ( 'NONE', #16199, 4.000000000000007105, 0.9599310885968835860 ) ;
#102292 = CARTESIAN_POINT ( 'NONE',  ( -9.559820589950547287, 51.28889575324969741, 3.548930410621208953 ) ) ;
#102293 = COLOUR_RGB ( '', 0.66274510, 0.83137255, 0.94901961) ;
#102295 = ORIENTED_EDGE ( 'NONE', *, *, #63165, .F. ) ;
#102294 = CONICAL_SURFACE ( 'NONE', #64420, 3.309500000000001663, 0.9599310885968770357 ) ;
#102296 = CARTESIAN_POINT ( 'NONE',  ( -4.781335833249819700, -2.669875467129551261, 102.4226025779373401 ) ) ;
#102297 = CARTESIAN_POINT ( 'NONE',  ( 0.000000000000000000, -46.00000000000000000, 112.0000000000000000 ) ) ;
#102298 = DIRECTION ( 'NONE',  ( 0.000000000000000000, 0.000000000000000000, 1.000000000000000000 ) ) ;
#102299 = AXIS2_PLACEMENT_3D ( 'NONE', #55049, #30285, #72310 ) ;
#102300 = CARTESIAN_POINT ( 'NONE',  ( -6.928203230275507885, 105.0000000000000000, -4.000000000000001776 ) ) ;
#102301 = PRODUCT_DEFINITION ( 'UNKNOWN', '', #35343, #56449 ) ;
#102302 = CARTESIAN_POINT ( 'NONE',  ( -4.844944557854277199E-15, -0.1944580884125578779, -19.78098730681987405 ) ) ;
#102303 = CARTESIAN_POINT ( 'NONE',  ( 9.852211596319799369, 15.56091200510340045, 1.749942564367552356 ) ) ;
#102304 = CARTESIAN_POINT ( 'NONE',  ( 85.92109966458600923, -53.81464801703884149, 191.8547092607505817 ) ) ;
#102305 = CARTESIAN_POINT ( 'NONE',  ( -5.248814467633681424, 10.38896636856183520, -30.54266839283955193 ) ) ;
#102306 = CARTESIAN_POINT ( 'NONE',  ( -4.248277208370227598, 140.2847170224943056, 4.999999999999997335 ) ) ;
#102307 = ORIENTED_EDGE ( 'NONE', *, *, #59267, .T. ) ;
#102308 = B_SPLINE_CURVE_WITH_KNOTS ( 'NONE', 3,
 ( #65434, #30436, #40096, #81582, #7181, #40617, #80537, #15814, #64384, #48169, #39049, #22354, #64901, #97783, #39583, #89715, #30976, #23950, #24484, #104832 ),
 .UNSPECIFIED., .F., .F.,
 ( 4, 2, 2, 2, 2, 2, 2, 2, 2, 4 ),
 ( 0.003044366697538010598, 0.003296264436757893445, 0.003548162175977776726, 0.004051957654417542853, 0.005059548611297080313, 0.005563344089736851211, 0.006067139568176622977, 0.006319037307396508860, 0.006570935046616394742, 0.007074730525056170845 ),
 .UNSPECIFIED. ) ;
#102309 = CARTESIAN_POINT ( 'NONE',  ( 65.37306859926557934, -29.78427825893012582, -22.92028099111634631 ) ) ;
#102310 = LINE ( 'NONE', #60806, #24597 ) ;
#102311 = FACE_OUTER_BOUND ( 'NONE', #48741, .T. ) ;
#102312 = LINE ( 'NONE', #4157, #11192 ) ;
#102313 = CARTESIAN_POINT ( 'NONE',  ( -86.38235237773579911, -29.99999999999999645, 66.63133496844396575 ) ) ;
#102314 = CARTESIAN_POINT ( 'NONE',  ( -4.466912950640278268E-14, -7.505553499465147382, -0.7999999999999977129 ) ) ;
#102315 = CARTESIAN_POINT ( 'NONE',  ( 28.07782961039620417, -57.67952082435122918, 44.31659357402789823 ) ) ;
#102317 = CARTESIAN_POINT ( 'NONE',  ( 13.82057366821712030, 304.5462546222179299, 9.872053150317878334 ) ) ;
#102316 = CARTESIAN_POINT ( 'NONE',  ( 37.26719918006427434, 490.8904285930220226, 12.42640642751123714 ) ) ;
#102318 = EDGE_CURVE ( 'NONE', #54844, #2515, #11645, .T. ) ;
#102319 = CARTESIAN_POINT ( 'NONE',  ( 5.163300830990278811, -51.69768845676519931, 40.01618609069083732 ) ) ;
#102320 = LINE ( 'NONE', #28471, #102129 ) ;
#102321 = CARTESIAN_POINT ( 'NONE',  ( -19.16726914849938979, 50.00000000000000000, 60.35899421978155743 ) ) ;
#102322 = PLANE ( 'NONE',  #89051 ) ;
#102323 = FACE_OUTER_BOUND ( 'NONE', #25077, .T. ) ;
#102324 = AXIS2_PLACEMENT_3D ( 'NONE', #58832, #51776, #76052 ) ;
#102325 = CARTESIAN_POINT ( 'NONE',  ( 39.39455998684030646, -24.68490879047467956, -30.41947531785933734 ) ) ;
#102326 = VECTOR ( 'NONE', #19260, 1000.000000000000000 ) ;
#102327 = CARTESIAN_POINT ( 'NONE',  ( -21.68992718180131618, -53.40044820062799857, 33.52570783747689376 ) ) ;
#102328 = ORIENTED_EDGE ( 'NONE', *, *, #95372, .T. ) ;
#102329 = CARTESIAN_POINT ( 'NONE',  ( 40.34962789288341867, 485.8327705809480221, -4.928685277743327653 ) ) ;
#102330 = DIRECTION ( 'NONE',  ( -0.000000000000000000, 1.000000000000000000, -0.000000000000000000 ) ) ;
#102331 = CARTESIAN_POINT ( 'NONE',  ( -17.53032627728494575, -22.07011661811088032, 27.84778146757210138 ) ) ;
#102332 = ADVANCED_FACE ( 'NONE', ( #59389 ), #90678, .T. ) ;
#102333 = EDGE_CURVE ( 'NONE', #33830, #54910, #54669, .T. ) ;
#102335 = CARTESIAN_POINT ( 'NONE',  ( 39.42064391485031649, 485.2093941173905023, -4.368290657543239419 ) ) ;
#102334 =( LENGTH_UNIT ( ) NAMED_UNIT ( * ) SI_UNIT ( .MILLI., .METRE. ) );
#102336 = VERTEX_POINT ( 'NONE', #17334 ) ;
#102337 = EDGE_CURVE ( 'NONE', #71240, #75630, #8181, .T. ) ;
#102338 =( NAMED_UNIT ( * ) PLANE_ANGLE_UNIT ( ) SI_UNIT ( $, .RADIAN. ) );
#102339 = VERTEX_POINT ( 'NONE', #100882 ) ;
#102340 = CARTESIAN_POINT ( 'NONE',  ( -10.51296777078104050, 50.00000000000000000, -92.64705882352942012 ) ) ;
#102341 =( NAMED_UNIT ( * ) PLANE_ANGLE_UNIT ( ) SI_UNIT ( $, .RADIAN. ) );
#102342 = B_SPLINE_CURVE_WITH_KNOTS ( 'NONE', 3,
 ( #21958, #4162, #54809, #87741, #13821, #79624, #71529, #63472, #96368, #16488, #31637, #98456, #89326, #96882, #8388, #25139, #57457, #15419, #74708, #49367, #15955, #31120, #81202, #74178, #89850, #24608 ),
 .UNSPECIFIED., .F., .F.,
 ( 4, 2, 2, 2, 2, 2, 2, 2, 2, 2, 2, 2, 4 ),
 ( 0.007354091942747225871, 0.007606081946708171705, 0.007858071950669117539, 0.008362051958591010942, 0.008614041962551966317, 0.008866031966512921692, 0.009370011974434832441, 0.009873991982356743191, 0.01037797199027865394, 0.01062996199423960758, 0.01088195199820056296, 0.01113394200216151660, 0.01138593200612247024 ),
 .UNSPECIFIED. ) ;
#102343 = CARTESIAN_POINT ( 'NONE',  ( -10.78860715609207865, -60.00000000000000000, -42.38218987242183289 ) ) ;
#102344 = ORIENTED_EDGE ( 'NONE', *, *, #19193, .T. ) ;
#102345 = SURFACE_STYLE_USAGE ( .BOTH. , #29048 ) ;
#102346 = CARTESIAN_POINT ( 'NONE',  ( 102.6487958908516589, -45.28275320593341036, 187.0266445405623017 ) ) ;
#102348 = DIRECTION ( 'NONE',  ( 0.000000000000000000, -1.000000000000000000, 0.000000000000000000 ) ) ;
#102347 = CARTESIAN_POINT ( 'NONE',  ( 38.09999999999998721, 0.000000000000000000, 3.309499999999999886 ) ) ;
#102349 = EDGE_LOOP ( 'NONE', ( #83776, #75643, #101071, #3941 ) ) ;
#102350 = VERTEX_POINT ( 'NONE', #9206 ) ;
#102351 = ORIENTED_EDGE ( 'NONE', *, *, #4690, .F. ) ;
#102352 = CARTESIAN_POINT ( 'NONE',  ( 23.28067972821365217, 305.8297143474431437, 10.15087365266885122 ) ) ;
#102353 = VECTOR ( 'NONE', #10873, 1000.000000000000227 ) ;
#102354 = FACE_OUTER_BOUND ( 'NONE', #73141, .T. ) ;
#102355 = VERTEX_POINT ( 'NONE', #67474 ) ;
#102356 = AXIS2_PLACEMENT_3D ( 'NONE', #12617, #4547, #87601 ) ;
#102357 = DIRECTION ( 'NONE',  ( -1.000000000000000000, -1.224606353822377258E-16, -0.000000000000000000 ) ) ;
#102358 = CARTESIAN_POINT ( 'NONE',  ( -5.500000000458552307, 41.99999999999999289, -68.91429205817152592 ) ) ;
#102359 = AXIS2_PLACEMENT_3D ( 'NONE', #84650, #26449, #42581 ) ;
#102360 = CARTESIAN_POINT ( 'NONE',  ( -57.24587099102581078, -60.00000000000970601, -38.75777265976601882 ) ) ;
#102361 = CARTESIAN_POINT ( 'NONE',  ( 7.934996450857313199, -68.86862456472532301, -1.050865690281774123 ) ) ;
#102362 = CARTESIAN_POINT ( 'NONE',  ( 30.71235692075721602, -60.00000000000002132, 43.40817750810721520 ) ) ;
#102363 = CARTESIAN_POINT ( 'NONE',  ( -12.86716125047998993, -4.999999999999999112, -10.20667643956625525 ) ) ;
#102364 = CARTESIAN_POINT ( 'NONE',  ( -14.33580413386536812, 42.00000000000000000, -89.41414995615788541 ) ) ;
#102366 = CARTESIAN_POINT ( 'NONE',  ( 3.991493828809749456, -25.54818830820175890, 28.14084830479718491 ) ) ;
#102365 = CARTESIAN_POINT ( 'NONE',  ( -113.0839934364197887, -60.00000000000005684, 149.3435297534686299 ) ) ;
#102367 = DIRECTION ( 'NONE',  ( -1.000000000000000000, -1.224606353822377258E-16, -0.000000000000000000 ) ) ;
#102368 = ADVANCED_FACE ( 'NONE', ( #84183 ), #79034, .T. ) ;
#102369 = CARTESIAN_POINT ( 'NONE',  ( -49.48822239264870859, -29.13117794537824423, 46.55600149492851614 ) ) ;
#102370 = ORIENTED_EDGE ( 'NONE', *, *, #50201, .T. ) ;
#102371 = PLANE ( 'NONE',  #5706 ) ;
#102372 = VERTEX_POINT ( 'NONE', #78745 ) ;
#102373 = CARTESIAN_POINT ( 'NONE',  ( 0.07719627998383862821, 7.746009256456144243, -51.75000000000014921 ) ) ;
#102374 = CARTESIAN_POINT ( 'NONE',  ( 16.14595037822608603, 7.274337365584589321, 6.616591826375515240 ) ) ;
#102375 = CARTESIAN_POINT ( 'NONE',  ( 5.855777637195783925, -6.218935032415544129, -1.331220292256673154 ) ) ;
#102376 = VERTEX_POINT ( 'NONE', #37279 ) ;
#102377 = LINE ( 'NONE', #52763, #8015 ) ;
#102378 = VERTEX_POINT ( 'NONE', #101968 ) ;
#102379 = CARTESIAN_POINT ( 'NONE',  ( 90.09087589920459038, -29.99999999999832667, -7.510710023258664769 ) ) ;
#102380 = DIRECTION ( 'NONE',  ( 1.000000000000000000, -0.000000000000000000, 1.224646799147353207E-16 ) ) ;
#102381 = SURFACE_SIDE_STYLE ('',( #28533 ) ) ;
#102382 = CARTESIAN_POINT ( 'NONE',  ( 6.738100180926640093, 41.71798714554645215, -59.05424661244425266 ) ) ;
#102383 = CARTESIAN_POINT ( 'NONE',  ( -59.23741894013591036, 42.00000000000000711, 7.754160006507077263 ) ) ;
#102384 = CARTESIAN_POINT ( 'NONE',  ( 97.54756622113360720, -30.00000000000000711, 190.8661322625956700 ) ) ;
#102385 = B_SPLINE_SURFACE_WITH_KNOTS ( 'NONE', 1, 3, ( 
 ( #80117, #80643, #57421, #33193, #16447, #89292, #15921, #6765 ),
 ( #40719, #39686, #66063, #105465, #98428, #63967, #7285, #39157 ) ),
 .UNSPECIFIED., .F., .F., .F.,
 ( 2, 2 ),
 ( 4, 2, 2, 4 ),
 ( 0.000000000000000000, 1.000000000000000000 ),
 ( 0.000000000000000000, 0.04450745600790868145, 0.06676118401186306728, 0.08901491201581737678 ),
 .UNSPECIFIED. ) ;
#102386 = ADVANCED_FACE ( 'NONE', ( #37815 ), #75657, .T. ) ;
#102387 = CARTESIAN_POINT ( 'NONE',  ( 57.45015997180046696, 4.898587196589294500E-16, -4.000000000000007105 ) ) ;
#102388 = B_SPLINE_CURVE_WITH_KNOTS ( 'NONE', 3,
 ( #32279, #105605, #62655, #49493 ),
 .UNSPECIFIED., .F., .F.,
 ( 4, 4 ),
 ( 0.000000000000000000, 0.002847824002212423055 ),
 .UNSPECIFIED. ) ;
#102389 = ORIENTED_EDGE ( 'NONE', *, *, #33349, .T. ) ;
#102390 = CIRCLE ( 'NONE', #31732, 0.5000000000000004441 ) ;
#102391 = VERTEX_POINT ( 'NONE', #70674 ) ;
#102392 = VERTEX_POINT ( 'NONE', #78228 ) ;
#102393 = CARTESIAN_POINT ( 'NONE',  ( 53.04775056965937807, -60.30987783887891851, 64.32335167159055800 ) ) ;
#102394 = CARTESIAN_POINT ( 'NONE',  ( 6.453254806564252988, 41.48539221478000627, -58.52372623101098981 ) ) ;
#102395 = DIRECTION ( 'NONE',  ( -1.000000000000000000, -1.224606353822377258E-16, -0.000000000000000000 ) ) ;
#102396 = VERTEX_POINT ( 'NONE', #94967 ) ;
#102397 = CARTESIAN_POINT ( 'NONE',  ( -90.43472293642049920, -38.40210348684055219, -14.77404530433802243 ) ) ;
#102398 = ORIENTED_EDGE ( 'NONE', *, *, #26452, .T. ) ;
#102399 = FILL_AREA_STYLE_COLOUR ( '', #87914 ) ;
#102400 = CARTESIAN_POINT ( 'NONE',  ( 89.10629083803385697, -38.53219886314418829, 200.3222450649632833 ) ) ;
#102401 = CARTESIAN_POINT ( 'NONE',  ( 10.68792165862781296, 15.17596856234630920, 9.765698129339666522 ) ) ;
#102402 = VECTOR ( 'NONE', #60658, 1000.000000000000000 ) ;
#102403 = CARTESIAN_POINT ( 'NONE',  ( 83.77118831961728063, -45.28417051351964773, 6.938750227302574736 ) ) ;
#102404 = AXIS2_PLACEMENT_3D ( 'NONE', #51827, #41623, #33549 ) ;
#102405 = FACE_OUTER_BOUND ( 'NONE', #101223, .T. ) ;
#102406 = AXIS2_PLACEMENT_3D ( 'NONE', #16925, #7742, #32595 ) ;
#102407 = CARTESIAN_POINT ( 'NONE',  ( 4.837657582856586203, -12.04835165414415066, -8.962574246966335423 ) ) ;
#102408 = APPLICATION_CONTEXT ( 'automotive_design' ) ;
#102409 =( GEOMETRIC_REPRESENTATION_CONTEXT ( 3 ) GLOBAL_UNCERTAINTY_ASSIGNED_CONTEXT ( ( #40865 ) ) GLOBAL_UNIT_ASSIGNED_CONTEXT ( ( #88312, #72638, #30623 ) ) REPRESENTATION_CONTEXT ( 'NONE', 'WORKASPACE' ) );
#102410 = ADVANCED_FACE ( 'NONE', ( #71192 ), #61086, .T. ) ;
#102411 = CARTESIAN_POINT ( 'NONE',  ( 20.00000000000001066, -4.000000000000000000, 25.00000000000000000 ) ) ;
#102412 = CIRCLE ( 'NONE', #9378, 5.000000000000010658 ) ;
#102413 = CARTESIAN_POINT ( 'NONE',  ( -43.79395675348489192, 434.3550296691299195, 12.19643612485312190 ) ) ;
#102414 = CARTESIAN_POINT ( 'NONE',  ( 8.588478090850260926, 128.2033481600911955, 6.133923549007229389E-13 ) ) ;
#102415 = ORIENTED_EDGE ( 'NONE', *, *, #78369, .F. ) ;
#102416 = EDGE_CURVE ( 'NONE', #54959, #16922, #82523, .T. ) ;
#102417 = CARTESIAN_POINT ( 'NONE',  ( -8.000000000000001776, -10.34375000409677092, 3.313708498984759387 ) ) ;
#102419 = B_SPLINE_CURVE_WITH_KNOTS ( 'NONE', 3,
 ( #52541, #77364, #105221, #103625, #38907, #19176, #60148, #63179, #52012, #22204, #87459, #87984, #84927, #85461, #3479, #79867, #54515, #46456, #11013, #36419, #21681, #5975, #43932, #71769, #104682, #30833, #98180, #66344, #40475, #74427, #502, #33470, #41013, #56649, #23258, #48021, #99227, #64761, #24850, #56102, #98696, #39958, #25394, #65817, #106256, #73898, #41537, #97636, #58250, #8102, #49626, #80102 ),
 .UNSPECIFIED., .F., .F.,
 ( 4, 1, 1, 1, 1, 1, 1, 2, 2, 1, 1, 1, 1, 1, 1, 1, 1, 1, 1, 2, 2, 1, 1, 1, 1, 1, 1, 1, 1, 2, 2, 1, 1, 1, 1, 1, 1, 1, 1, 2, 2, 4 ),
 ( 0.000000000000000000, 0.1250000000000170974, 0.1875000000000253686, 0.2187500000000295597, 0.2343750000000313916, 0.2421875000000320022, 0.2460937500000320854, 0.2480468750000324463, 0.2500000000000328071, 0.3750000000000618394, 0.4375000000000762723, 0.4687500000000834888, 0.4843750000000871525, 0.4921875000000889289, 0.4960937500000900391, 0.4980468750000908162, 0.4990234375000915379, 0.4995117187500917599, 0.4997558593750915934, 0.4998779296875914824, 0.5000000000000913714, 0.5625000000001059153, 0.5937500000001132427, 0.6093750000001169065, 0.6171875000001185718, 0.6210937500001195710, 0.6230468750001201261, 0.6240234375001204592, 0.6245117187501205702, 0.6247558593751206812, 0.6250000000001206812, 0.6875000000001317835, 0.7187500000001374456, 0.7343750000001403322, 0.7421875000001415534, 0.7460937500001423306, 0.7480468750001427747, 0.7490234375001427747, 0.7495117187501424416, 0.7497558593751425526, 0.7500000000001425526, 1.000000000000000000 ),
 .UNSPECIFIED. ) ;
#102418 = CARTESIAN_POINT ( 'NONE',  ( 15.52419239919875693, 37.09839268680908475, -22.76866006007180587 ) ) ;
#102420 = FACE_OUTER_BOUND ( 'NONE', #11490, .T. ) ;
#102421 = EDGE_LOOP ( 'NONE', ( #74773, #84487, #19678, #36099 ) ) ;
#102422 = DIRECTION ( 'NONE',  ( -0.6505632072693978696, 0.6639782930160472718, -0.3686466326319159381 ) ) ;
#102423 = CARTESIAN_POINT ( 'NONE',  ( -40.03675158195893147, 318.9422692625357740, 7.795136733933277995 ) ) ;
#102424 = CARTESIAN_POINT ( 'NONE',  ( 13.09999999999999787, -3.309499999999999886, 4.475777889183790779E-16 ) ) ;
#102425 = CARTESIAN_POINT ( 'NONE',  ( -14.01509096962760736, 42.58675651153940578, -91.23243542799710326 ) ) ;
#102426 = CARTESIAN_POINT ( 'NONE',  ( 3.313708498984762496, -20.28124999999999289, 7.999999999999998224 ) ) ;
#102427 = CARTESIAN_POINT ( 'NONE',  ( -31.60541874544299645, -33.50245859134227544, 41.55280622130048584 ) ) ;
#102428 = CARTESIAN_POINT ( 'NONE',  ( -8.559508646656370345, -1.200000000000000030E-05, 4.031152949374564365 ) ) ;
#102429 = ORIENTED_EDGE ( 'NONE', *, *, #50073, .F. ) ;
#102430 = CARTESIAN_POINT ( 'NONE',  ( 84.53399812488744658, -42.96929415438898303, 184.1428513560889542 ) ) ;
#102431 = CARTESIAN_POINT ( 'NONE',  ( 6.249999999999998224, 4.618802153517001408, -8.000000000000000000 ) ) ;
#102432 = CARTESIAN_POINT ( 'NONE',  ( 0.000000000000000000, -1.200000000000000030E-05, -17.50000000000000000 ) ) ;
#102433 = ORIENTED_EDGE ( 'NONE', *, *, #8662, .T. ) ;
#102434 = ADVANCED_FACE ( 'NONE', ( #6742 ), #70520, .T. ) ;
#102435 = CARTESIAN_POINT ( 'NONE',  ( -86.84743696432029481, -37.82102094881744847, 58.81972901610166815 ) ) ;
#102436 = CARTESIAN_POINT ( 'NONE',  ( 0.2573354458087823704, -6.889406814520509847, 1.067197363239225760 ) ) ;
#102437 = CARTESIAN_POINT ( 'NONE',  ( 12.76706325321343094, -5.000000000000002665, -81.58101990455240582 ) ) ;
#102438 = DIRECTION ( 'NONE',  ( -1.000000000000000000, -1.224606353822377258E-16, -0.000000000000000000 ) ) ;
#102439 = DIRECTION ( 'NONE',  ( 0.000000000000000000, 1.000000000000000000, 0.000000000000000000 ) ) ;
#102440 = AXIS2_PLACEMENT_3D ( 'NONE', #42873, #91955, #76296 ) ;
#102441 = CARTESIAN_POINT ( 'NONE',  ( 81.92741076442609938, -53.50746804662570355, 180.9159421606091200 ) ) ;
#102442 = CARTESIAN_POINT ( 'NONE',  ( 38.67627001412847676, -59.99999999999999289, 50.31928010676779195 ) ) ;
#102443 = CARTESIAN_POINT ( 'NONE',  ( 16.26197166262537763, -23.40186626609153109, 36.11761830283866459 ) ) ;
#102444 = PRESENTATION_STYLE_ASSIGNMENT (( #70611 ) ) ;
#102445 = CARTESIAN_POINT ( 'NONE',  ( 51.42506870373882322, -29.90362599224476980, 49.04348699933098032 ) ) ;
#102447 = CARTESIAN_POINT ( 'NONE',  ( -13.29977836103240030, 22.16549982817352316, 4.028575465788259535 ) ) ;
#102446 = DIRECTION ( 'NONE',  ( 1.000000000000000000, 1.224606353822377258E-16, 0.000000000000000000 ) ) ;
#102448 = CARTESIAN_POINT ( 'NONE',  ( 6.549255471752022828, 294.7416366638802856, -7.570647764325297402 ) ) ;
#102449 = CARTESIAN_POINT ( 'NONE',  ( -2.977408999572650039, -9.687500002048384573, -7.188101187500001821 ) ) ;
#102450 = ORIENTED_EDGE ( 'NONE', *, *, #102460, .T. ) ;
#102451 =( LENGTH_UNIT ( ) NAMED_UNIT ( * ) SI_UNIT ( .MILLI., .METRE. ) );
#102452 = CARTESIAN_POINT ( 'NONE',  ( 0.000000000000000000, 0.000000000000000000, 0.000000000000000000 ) ) ;
#102453 = LINE ( 'NONE', #94374, #67289 ) ;
#102454 = ORIENTED_EDGE ( 'NONE', *, *, #27166, .T. ) ;
#102455 = DIRECTION ( 'NONE',  ( 0.000000000000000000, -1.000000000000000000, 0.000000000000000000 ) ) ;
#102456 = CARTESIAN_POINT ( 'NONE',  ( -17.49999999999997158, 51.85440564192673918, 61.62473156926974838 ) ) ;
#102457 = ORIENTED_EDGE ( 'NONE', *, *, #96025, .T. ) ;
#102458 = CARTESIAN_POINT ( 'NONE',  ( -9.922755624444706157, -3.234633340497464982, 15.16391852634635562 ) ) ;
#102459 = FILL_AREA_STYLE_COLOUR ( '', #59149 ) ;
#102460 = EDGE_CURVE ( 'NONE', #45219, #34210, #79571, .T. ) ;
#102461 = CARTESIAN_POINT ( 'NONE',  ( 66.74444444444444002, 6.915964383211875250E-15, 0.000000000000000000 ) ) ;
#102462 = EDGE_CURVE ( 'NONE', #41320, #88738, #76158, .T. ) ;
#102464 = CARTESIAN_POINT ( 'NONE',  ( 4.765530066358713235, -47.40889156923955028, -34.73460941772712118 ) ) ;
#102463 = CARTESIAN_POINT ( 'NONE',  ( 9.842473135306434529, 253.5893181711358295, 1.785129593756250355 ) ) ;
#102465 = CIRCLE ( 'NONE', #35283, 4.000000000000000888 ) ;
#102466 = ORIENTED_EDGE ( 'NONE', *, *, #75972, .F. ) ;
#102467 = FACE_OUTER_BOUND ( 'NONE', #45564, .T. ) ;
#102468 = CARTESIAN_POINT ( 'NONE',  ( 0.000000000000000000, 0.000000000000000000, -1.581124522925831499 ) ) ;
#102469 = VERTEX_POINT ( 'NONE', #7791 ) ;
#102470 = EDGE_CURVE ( 'NONE', #78182, #28854, #27521, .T. ) ;
#102471 = CARTESIAN_POINT ( 'NONE',  ( 6.333820801330125150, 4.275724398227219503, 5.594228103108966010 ) ) ;
#102472 = AXIS2_PLACEMENT_3D ( 'NONE', #9207, #8687, #18405 ) ;
#102473 = CARTESIAN_POINT ( 'NONE',  ( -91.96800439629041080, -60.00000000000000000, 6.911253661384300528 ) ) ;
#102474 = ORIENTED_EDGE ( 'NONE', *, *, #99878, .F. ) ;
#102475 = CARTESIAN_POINT ( 'NONE',  ( 1.843592604519097344, 42.00000000000000000, -60.21617040573095636 ) ) ;
#102476 = CARTESIAN_POINT ( 'NONE',  ( 0.000000000000000000, 32.68727484027578356, -33.82893434829263413 ) ) ;
#102477 = AXIS2_PLACEMENT_3D ( 'NONE', #95450, #37789, #70650 ) ;
#102478 = DIRECTION ( 'NONE',  ( -1.000000000000000000, 0.000000000000000000, 0.000000000000000000 ) ) ;
#102479 = CARTESIAN_POINT ( 'NONE',  ( -3.801077171203065319, -48.88909605940821734, 104.1059035333590828 ) ) ;
#102480 = CIRCLE ( 'NONE', #31812, 4.000000000000001776 ) ;
#102482 = FILL_AREA_STYLE_COLOUR ( '', #102862 ) ;
#102481 = CARTESIAN_POINT ( 'NONE',  ( -8.000000000000000000, -26.74999999999999645, -9.797174393178825657E-16 ) ) ;
#102483 = CARTESIAN_POINT ( 'NONE',  ( -82.93554783337889091, -39.48948165585812831, 169.2715108827067354 ) ) ;
#102484 = ORIENTED_EDGE ( 'NONE', *, *, #68492, .T. ) ;
#102485 = VECTOR ( 'NONE', #47321, 1000.000000000000000 ) ;
#102486 = CARTESIAN_POINT ( 'NONE',  ( -8.521464936451071281, -0.000000000000000000, 14.76977913854606506 ) ) ;
#102487 = ORIENTED_EDGE ( 'NONE', *, *, #28831, .F. ) ;
#102488 = CIRCLE ( 'NONE', #16326, 5.000000000000002665 ) ;
#102489 = ORIENTED_EDGE ( 'NONE', *, *, #67903, .F. ) ;
#102491 =( BOUNDED_CURVE ( )  B_SPLINE_CURVE ( 2, ( #97729, #56739, #64336 ),
 .UNSPECIFIED., .F., .F. ) 
 B_SPLINE_CURVE_WITH_KNOTS ( ( 3, 3 ),
 ( 0.000000000000000000, 1.000000000000000000 ),
 .UNSPECIFIED. ) 
 CURVE ( )  GEOMETRIC_REPRESENTATION_ITEM ( )  RATIONAL_B_SPLINE_CURVE ( ( 1.000000000000000000, 1.857142857142858317, 1.000000000000000000 ) ) 
 REPRESENTATION_ITEM ( '' )  );
#102490 =( NAMED_UNIT ( * ) SI_UNIT ( $, .STERADIAN. ) SOLID_ANGLE_UNIT ( ) );
#102492 = CARTESIAN_POINT ( 'NONE',  ( -5.000000000000000000, -12.54465221550630183, 8.223849511754982800 ) ) ;
#102493 = DIRECTION ( 'NONE',  ( -1.000000000000000000, 0.000000000000000000, 0.000000000000000000 ) ) ;
#102494 = ORIENTED_EDGE ( 'NONE', *, *, #987, .T. ) ;
#102495 = CARTESIAN_POINT ( 'NONE',  ( -94.14808112328414325, -57.65316219711669987, -13.38331396264917394 ) ) ;
#102496 = CARTESIAN_POINT ( 'NONE',  ( -4.472135954999577834, -65.27411850998326770, -4.000000000000002665 ) ) ;
#102497 = LINE ( 'NONE', #10800, #1404 ) ;
#102498 = CARTESIAN_POINT ( 'NONE',  ( 23.85899507165746414, 27.29461519911105682, 33.04201830783504334 ) ) ;
#102499 = CARTESIAN_POINT ( 'NONE',  ( -13.99657022045423282, -50.02530620882281198, 26.59685899168112400 ) ) ;
#102500 = CARTESIAN_POINT ( 'NONE',  ( 4.034557488804384917, 15.07443463110268134, -9.151133496029480341 ) ) ;
#102501 = CARTESIAN_POINT ( 'NONE',  ( 82.73925898424661796, -14.21045842199433373, -19.52984640694043250 ) ) ;
#102502 = CARTESIAN_POINT ( 'NONE',  ( -74.10870907870054225, -60.00000000000004974, 189.8079394841834073 ) ) ;
#102503 = EDGE_CURVE ( 'NONE', #100209, #81828, #58493, .T. ) ;
#102504 = CARTESIAN_POINT ( 'NONE',  ( -54.64099352351128402, -53.38243350366994378, 65.16998337476768199 ) ) ;
#102505 = ORIENTED_EDGE ( 'NONE', *, *, #31850, .T. ) ;
#102506 = CARTESIAN_POINT ( 'NONE',  ( 6.705175466950450414, 16.46052391487621591, -2.022930269817424076 ) ) ;
#102507 = ORIENTED_EDGE ( 'NONE', *, *, #47375, .F. ) ;
#102508 = CARTESIAN_POINT ( 'NONE',  ( -103.9834764852472517, -52.71019089480785880, 186.8325922579311680 ) ) ;
#102509 = DIRECTION ( 'NONE',  ( 0.000000000000000000, 0.000000000000000000, 1.000000000000000000 ) ) ;
#102510 = ADVANCED_FACE ( 'NONE', ( #98919 ), #90050, .F. ) ;
#102511 = ORIENTED_EDGE ( 'NONE', *, *, #52449, .F. ) ;
#102512 = CARTESIAN_POINT ( 'NONE',  ( 7.230783190336673272, -4.999999999999994671, -70.90935357140938322 ) ) ;
#102513 = FILL_AREA_STYLE ('',( #45349 ) ) ;
#102514 =( LENGTH_UNIT ( ) NAMED_UNIT ( * ) SI_UNIT ( .MILLI., .METRE. ) );
#102515 = CARTESIAN_POINT ( 'NONE',  ( -2.977408999572650039, -14.56250000204838457, -7.188101187500001821 ) ) ;
#102516 = CARTESIAN_POINT ( 'NONE',  ( 30.55228927099183522, 298.7536840786443690, 10.80461237140096209 ) ) ;
#102517 = DIRECTION ( 'NONE',  ( -1.000000000000000000, -1.224606353822377258E-16, -0.000000000000000000 ) ) ;
#102518 = VECTOR ( 'NONE', #85890, 1000.000000000000227 ) ;
#102519 = DIRECTION ( 'NONE',  ( 0.000000000000000000, -1.000000000000000000, 0.000000000000000000 ) ) ;
#102520 = CARTESIAN_POINT ( 'NONE',  ( 66.85002385057480012, -29.99999999999999645, 85.60483471394741173 ) ) ;
#102521 = DIRECTION ( 'NONE',  ( 1.000000000000000000, 1.224606353822377258E-16, 0.000000000000000000 ) ) ;
#102522 = CARTESIAN_POINT ( 'NONE',  ( -9.826266471807617364, 7.906979468790463095, -0.000000000000000000 ) ) ;
#102523 = EDGE_CURVE ( 'NONE', #85798, #50509, #31317, .T. ) ;
#102524 = CARTESIAN_POINT ( 'NONE',  ( -16.64348903516496136, 45.60392139269943357, -6.657797401562710604 ) ) ;
#102525 = CARTESIAN_POINT ( 'NONE',  ( -26.98668602709024356, -46.43780309524522210, 33.41811407250219901 ) ) ;
#102526 = CARTESIAN_POINT ( 'NONE',  ( 47.78329097220170496, -18.76695584851968235, 41.09799256819893287 ) ) ;
#102527 = ORIENTED_EDGE ( 'NONE', *, *, #84159, .T. ) ;
#102528 = DIRECTION ( 'NONE',  ( 0.000000000000000000, 0.000000000000000000, 1.000000000000000000 ) ) ;
#102529 = CARTESIAN_POINT ( 'NONE',  ( -6.928203230275510549, 85.00000000000000000, 4.000000000000000000 ) ) ;
#102530 = CARTESIAN_POINT ( 'NONE',  ( -93.74606775496390298, -38.49331479316243332, 201.1767005034121780 ) ) ;
#102531 = ORIENTED_EDGE ( 'NONE', *, *, #35079, .T. ) ;
#102532 = DIRECTION ( 'NONE',  ( -1.000000000000000000, -1.224606353822377258E-16, -0.000000000000000000 ) ) ;
#102533 = CARTESIAN_POINT ( 'NONE',  ( 15.78881369299498694, 4.458650427774422553, -5.229507541793314118 ) ) ;
#102534 = CARTESIAN_POINT ( 'NONE',  ( -18.92291927219337921, 48.92936808311021935, 62.13088862737573237 ) ) ;
#102535 = SURFACE_STYLE_FILL_AREA ( #4905 ) ;
#102536 = CARTESIAN_POINT ( 'NONE',  ( 6.592082458585389659, 40.00000000377368536, -71.20206342450474324 ) ) ;
#102537 = CARTESIAN_POINT ( 'NONE',  ( -31.88369140427094806, 435.8716523888044208, 17.58732034368808073 ) ) ;
#102538 = CARTESIAN_POINT ( 'NONE',  ( 2.761899744546835519E-15, 36.79151656018385097, 22.55262289886175964 ) ) ;
#102539 = CARTESIAN_POINT ( 'NONE',  ( 111.2827313485384479, -60.00000000000000000, 185.7785520166476090 ) ) ;
#102540 = VECTOR ( 'NONE', #56798, 1000.000000000000000 ) ;
#102541 = DIRECTION ( 'NONE',  ( 0.000000000000000000, -1.000000000000000000, 0.000000000000000000 ) ) ;
#102542 = ORIENTED_EDGE ( 'NONE', *, *, #44750, .F. ) ;
#102543 = EDGE_CURVE ( 'NONE', #41735, #59443, #8858, .T. ) ;
#102544 = CARTESIAN_POINT ( 'NONE',  ( 7.213352437320216914, 32.01836473007681860, -3.463014597543476736 ) ) ;
#102545 = CARTESIAN_POINT ( 'NONE',  ( -73.50846916961513955, -30.00000000000000711, -18.85481956966018302 ) ) ;
#102546 = ORIENTED_EDGE ( 'NONE', *, *, #17544, .T. ) ;
#102548 = FACE_OUTER_BOUND ( 'NONE', #17001, .T. ) ;
#102547 = CARTESIAN_POINT ( 'NONE',  ( -75.93393509941148523, -38.37291240018149097, 177.9364027747577381 ) ) ;
#102549 = B_SPLINE_CURVE_WITH_KNOTS ( 'NONE', 3,
 ( #7465, #80834, #48988, #8541, #98610, #24761, #66254, #99136 ),
 .UNSPECIFIED., .F., .F.,
 ( 4, 2, 2, 4 ),
 ( 0.003797433802554463656, 0.004743183970586255238, 0.005688934138618048121, 0.007580434474681636489 ),
 .UNSPECIFIED. ) ;
#102550 = DIRECTION ( 'NONE',  ( 0.000000000000000000, 1.000000000000000000, 0.000000000000000000 ) ) ;
#102551 = LINE ( 'NONE', #28701, #67398 ) ;
#102552 = CARTESIAN_POINT ( 'NONE',  ( 5.082755093536324154, -12.21875000204838635, 5.082755093536326818 ) ) ;
#102553 = CIRCLE ( 'NONE', #55998, 3.309500000000001663 ) ;
#102554 = CARTESIAN_POINT ( 'NONE',  ( -43.61212006920826667, 434.3223099624050292, 14.49719201759458898 ) ) ;
#102555 = VECTOR ( 'NONE', #46365, 1000.000000000000000 ) ;
#102556 = AXIS2_PLACEMENT_3D ( 'NONE', #8322, #41226, #66035 ) ;
#102557 = AXIS2_PLACEMENT_3D ( 'NONE', #16242, #72875, #90675 ) ;
#102558 = CARTESIAN_POINT ( 'NONE',  ( 0.000000000000000000, 0.000000000000000000, -8.000000000000000000 ) ) ;
#102559 = AXIS2_PLACEMENT_3D ( 'NONE', #96385, #38167, #5757 ) ;
#102561 = ORIENTED_EDGE ( 'NONE', *, *, #14296, .F. ) ;
#102560 = CARTESIAN_POINT ( 'NONE',  ( -7.500000000000007105, 39.99999999999999289, -65.90297133634224735 ) ) ;
#102562 = CARTESIAN_POINT ( 'NONE',  ( 84.54726099131491424, -28.98982865470740933, 167.9107454418049770 ) ) ;
#102563 = LINE ( 'NONE', #43787, #49762 ) ;
#102564 = AXIS2_PLACEMENT_3D ( 'NONE', #58647, #1978, #17657 ) ;
#102565 = CARTESIAN_POINT ( 'NONE',  ( 6.815830331203682313, -0.6610623347507985637, -6.171384342982605631 ) ) ;
#102566 = ORIENTED_EDGE ( 'NONE', *, *, #40335, .T. ) ;
#102567 = CARTESIAN_POINT ( 'NONE',  ( -32.17606763901869016, 486.0066785907575877, 5.076925403390320390 ) ) ;
#102568 = EDGE_CURVE ( 'NONE', #93742, #32720, #81669, .T. ) ;
#102569 = CARTESIAN_POINT ( 'NONE',  ( -48.02835407290516656, 16.78162100668608048, 14.35535821593516559 ) ) ;
#102570 = CARTESIAN_POINT ( 'NONE',  ( 8.000000000000000000, -28.99999999999999289, 0.000000000000000000 ) ) ;
#102571 = SURFACE_STYLE_FILL_AREA ( #38387 ) ;
#102572 = DIRECTION ( 'NONE',  ( -1.000000000000000000, -1.224606353822377258E-16, -0.000000000000000000 ) ) ;
#102573 = DIRECTION ( 'NONE',  ( -1.000000000000000000, -0.000000000000000000, -0.000000000000000000 ) ) ;
#102574 = CARTESIAN_POINT ( 'NONE',  ( 10.29956429353439873, 2.626117177127659463, 14.76850153968369916 ) ) ;
#102575 = ORIENTED_EDGE ( 'NONE', *, *, #10243, .T. ) ;
#102576 = CARTESIAN_POINT ( 'NONE',  ( -76.71780263312517434, -30.00000000000000355, -16.85326244919820482 ) ) ;
#102577 = CARTESIAN_POINT ( 'NONE',  ( -5.000000000000000888, -4.607398061199006634, -14.28094137034753608 ) ) ;
#102578 = CARTESIAN_POINT ( 'NONE',  ( 4.000000000000000000, 4.898587196589412829E-16, -5.703399999999999359 ) ) ;
#102580 = FACE_OUTER_BOUND ( 'NONE', #72770, .T. ) ;
#102579 = CARTESIAN_POINT ( 'NONE',  ( 30.00000000000000000, 0.000000000000000000, 0.000000000000000000 ) ) ;
#102581 = CARTESIAN_POINT ( 'NONE',  ( 5.082755093536325930, -24.96875000204838813, -5.082755093536325042 ) ) ;
#102582 = DIRECTION ( 'NONE',  ( 0.000000000000000000, 0.000000000000000000, 1.000000000000000000 ) ) ;
#102583 = DIRECTION ( 'NONE',  ( -1.000000000000000000, -1.224606353822377258E-16, -0.000000000000000000 ) ) ;
#102584 = DIRECTION ( 'NONE',  ( -0.5735764363510510444, -0.8191520442889883569, 0.000000000000000000 ) ) ;
#102585 = CONTEXT_DEPENDENT_SHAPE_REPRESENTATION ( #81732, #56321 ) ;
#102586 = ORIENTED_EDGE ( 'NONE', *, *, #93204, .T. ) ;
#102587 = B_SPLINE_CURVE_WITH_KNOTS ( 'NONE', 3,
 ( #63809, #14158, #45507, #21249 ),
 .UNSPECIFIED., .F., .F.,
 ( 4, 4 ),
 ( 0.000000000000000000, 0.01132019266528281470 ),
 .UNSPECIFIED. ) ;
#102588 = CARTESIAN_POINT ( 'NONE',  ( 40.33183555103128271, 485.8341092017946039, -4.932519190553093402 ) ) ;
#102589 = CARTESIAN_POINT ( 'NONE',  ( 7.500000000000000000, -3.202733125952014426, -7.213074474936427727 ) ) ;
#102590 = CARTESIAN_POINT ( 'NONE',  ( -3.475980472679373268, 26.84355119020046132, -5.000000000000000000 ) ) ;
#102591 = DIRECTION ( 'NONE',  ( 0.000000000000000000, 0.000000000000000000, -1.000000000000000000 ) ) ;
#102592 = EDGE_CURVE ( 'NONE', #26726, #6732, #89170, .T. ) ;
#102593 = B_SPLINE_CURVE_WITH_KNOTS ( 'NONE', 3,
 ( #91614, #68401, #9598, #41976, #10664, #26384, #50069, #66799, #17721, #1504, #51660, #85103, #99687, #60324, #18268, #100217, #27444, #51122, #25857, #83498 ),
 .UNSPECIFIED., .F., .F.,
 ( 4, 2, 2, 2, 2, 2, 2, 2, 2, 4 ),
 ( 0.000000000000000000, 0.001698246576620752709, 0.003396493153241505417, 0.005094739729862258343, 0.006792986306483010835, 0.008491232883103763326, 0.01018947945972451322, 0.01188772603634526658, 0.01273684932465564239, 0.01358597261296601820 ),
 .UNSPECIFIED. ) ;
#102594 = ORIENTED_EDGE ( 'NONE', *, *, #75268, .T. ) ;
#102595 = FACE_OUTER_BOUND ( 'NONE', #5062, .T. ) ;
#102596 = VERTEX_POINT ( 'NONE', #53585 ) ;
#102597 = ADVANCED_FACE ( 'NONE', ( #1820 ), #48085, .T. ) ;
#102598 = DIRECTION ( 'NONE',  ( 0.000000000000000000, -1.000000000000000000, 0.000000000000000000 ) ) ;
#102599 = CARTESIAN_POINT ( 'NONE',  ( -3.313708498984746065, -22.15625000409677625, 8.000000000000017764 ) ) ;
#102600 = CARTESIAN_POINT ( 'NONE',  ( 9.165151389911677882, 104.7326484439288237, -4.000000000000001776 ) ) ;
#102601 = CARTESIAN_POINT ( 'NONE',  ( -17.99842623603809244, 36.44670248777274679, 23.18063615129680954 ) ) ;
#102602 = CARTESIAN_POINT ( 'NONE',  ( -112.0514578880708285, -59.99999999999998579, 178.8323363711955665 ) ) ;
#102603 =( NAMED_UNIT ( * ) SI_UNIT ( $, .STERADIAN. ) SOLID_ANGLE_UNIT ( ) );
#102604 = CARTESIAN_POINT ( 'NONE',  ( 0.7145311798163234140, -9.237604307034013473, 6.198474679904167468E-16 ) ) ;
#102605 = CARTESIAN_POINT ( 'NONE',  ( 5.455323569189487465, 53.44305311210484888, -8.531152949374620320 ) ) ;
#102606 = SURFACE_SIDE_STYLE ('',( #12513 ) ) ;
#102607 = CARTESIAN_POINT ( 'NONE',  ( -86.11088107305231176, -21.49943172053022522, 175.3779314699612542 ) ) ;
#102608 = STYLED_ITEM ( 'NONE', ( #89723 ), #64886 ) ;
#102609 = CARTESIAN_POINT ( 'NONE',  ( 51.21652843344448769, 40.83886418554102704, -40.08891448626480525 ) ) ;
#102610 = ORIENTED_EDGE ( 'NONE', *, *, #50404, .T. ) ;
#102611 = CARTESIAN_POINT ( 'NONE',  ( 7.000000000000000000, -14.05766640829038039, -5.232782735144291486 ) ) ;
#102612 = ADVANCED_FACE ( 'NONE', ( #84889 ), #77861, .F. ) ;
#102613 = SURFACE_STYLE_FILL_AREA ( #69721 ) ;
#102614 = CARTESIAN_POINT ( 'NONE',  ( -86.74535326754120490, -60.15511608754272288, -0.9989608454956866446 ) ) ;
#102615 = DIRECTION ( 'NONE',  ( -0.000000000000000000, -0.000000000000000000, -1.000000000000000000 ) ) ;
#102616 = CARTESIAN_POINT ( 'NONE',  ( -3.454139446565478888, 27.54133855866839653, -5.000000000000000000 ) ) ;
#102617 = CARTESIAN_POINT ( 'NONE',  ( 8.763392006801380418, 132.4000990056166529, -4.999999999999999112 ) ) ;
#102618 = CARTESIAN_POINT ( 'NONE',  ( 15.50526908259248593, 42.00000000004113332, 57.69562748392037577 ) ) ;
#102619 = CARTESIAN_POINT ( 'NONE',  ( 72.58683006904378487, -60.00000000000011369, 181.3898877100950244 ) ) ;
#102620 = CARTESIAN_POINT ( 'NONE',  ( -89.32121524059635931, -30.00000000000006750, 17.90039431539770121 ) ) ;
#102621 = EDGE_CURVE ( 'NONE', #79056, #24576, #41258, .T. ) ;
#102622 = CARTESIAN_POINT ( 'NONE',  ( -64.47158722768480743, -32.53199268566179825, 81.05542600198782566 ) ) ;
#102623 = ORIENTED_EDGE ( 'NONE', *, *, #21610, .T. ) ;
#102624 = CARTESIAN_POINT ( 'NONE',  ( 80.78816237064734196, -29.99999999999997513, 192.9482874834278903 ) ) ;
#102625 = CARTESIAN_POINT ( 'NONE',  ( 31.45128802944020663, 39.42551091560301302, 56.96251755607489287 ) ) ;
#102626 = CARTESIAN_POINT ( 'NONE',  ( 35.58387498457056353, -60.00000000000000000, 50.27079091460490901 ) ) ;
#102627 = CIRCLE ( 'NONE', #14760, 7.000000000000000000 ) ;
#102629 = ORIENTED_EDGE ( 'NONE', *, *, #102055, .T. ) ;
#102628 = VECTOR ( 'NONE', #80720, 1000.000000000000114 ) ;
#102630 = LINE ( 'NONE', #20709, #45901 ) ;
#102632 = AXIS2_PLACEMENT_3D ( 'NONE', #7087, #39999, #72873 ) ;
#102631 = CARTESIAN_POINT ( 'NONE',  ( 2.977408999572650927, -23.75000000204838813, -7.188101187500000933 ) ) ;
#102633 = CARTESIAN_POINT ( 'NONE',  ( -5.646888413699862497, -6.550258440296117257, 2.040714635159913470 ) ) ;
#102634 = ORIENTED_EDGE ( 'NONE', *, *, #3266, .F. ) ;
#102635 = DIRECTION ( 'NONE',  ( 0.5735764363510466035, -0.8191520442889914655, 1.003171929053524500E-16 ) ) ;
#102636 = ORIENTED_EDGE ( 'NONE', *, *, #77466, .F. ) ;
#102637 = CARTESIAN_POINT ( 'NONE',  ( -7.135888613855453144, 41.99999999999999289, -71.74865085751117988 ) ) ;
#102638 =( LENGTH_UNIT ( ) NAMED_UNIT ( * ) SI_UNIT ( .MILLI., .METRE. ) );
#102640 = VECTOR ( 'NONE', #2855, 1000.000000000000341 ) ;
#102639 = CARTESIAN_POINT ( 'NONE',  ( -82.04894669109339134, -60.00000000000000000, -26.67549837306723504 ) ) ;
#102641 = DIRECTION ( 'NONE',  ( -1.000000000000000000, -1.224606353822377258E-16, -0.000000000000000000 ) ) ;
#102642 = CARTESIAN_POINT ( 'NONE',  ( -5.082755093536325042, -33.96875000204838813, -5.082755093536325930 ) ) ;
#102643 = DIRECTION ( 'NONE',  ( -1.000000000000000000, -0.000000000000000000, -0.000000000000000000 ) ) ;
#102644 = CONICAL_SURFACE ( 'NONE', #57811, 4.171999999999999709, 0.7853981633974708165 ) ;
#102645 = CARTESIAN_POINT ( 'NONE',  ( -9.596002107494335576, 50.00000000000000000, -77.62543935900903591 ) ) ;
#102646 = CARTESIAN_POINT ( 'NONE',  ( -45.99999999999999289, 438.0740625310870087, 11.26011362676991467 ) ) ;
#102647 = EDGE_CURVE ( 'NONE', #77299, #59177, #68726, .T. ) ;
#102648 = CARTESIAN_POINT ( 'NONE',  ( 0.000000000000000000, 6.123233995736767268E-16, -5.000000000000000888 ) ) ;
#102649 = ORIENTED_EDGE ( 'NONE', *, *, #64245, .F. ) ;
#102650 = CARTESIAN_POINT ( 'NONE',  ( -7.500000000000006217, 40.28748324523081692, -68.91429205787007106 ) ) ;
#102651 = CIRCLE ( 'NONE', #92318, 1.000000000000000888 ) ;
#102653 = CARTESIAN_POINT ( 'NONE',  ( 35.62089395783882395, -56.82290754243824438, 39.01274798168336133 ) ) ;
#102652 = FACE_OUTER_BOUND ( 'NONE', #72694, .T. ) ;
#102654 = CARTESIAN_POINT ( 'NONE',  ( -24.56594385547996140, -4.285714285713227767, 6.601913983196856073 ) ) ;
#102655 = ORIENTED_EDGE ( 'NONE', *, *, #53722, .T. ) ;
#102656 = CARTESIAN_POINT ( 'NONE',  ( -42.51086551946191605, 484.3281707585954337, -1.915972276551850095 ) ) ;
#102657 = B_SPLINE_CURVE_WITH_KNOTS ( 'NONE', 3,
 ( #95679, #39050, #20252, #103766 ),
 .UNSPECIFIED., .F., .F.,
 ( 4, 4 ),
 ( 5.028454403087268254E-17, 0.001025896622541378790 ),
 .UNSPECIFIED. ) ;
#102659 = CARTESIAN_POINT ( 'NONE',  ( -10.39117206796836435, 1.272551561242683961E-15, -8.500000000000000000 ) ) ;
#102658 = CARTESIAN_POINT ( 'NONE',  ( -25.85821479973299120, 35.03516150445064881, -8.996769488741277243 ) ) ;
#102660 = CARTESIAN_POINT ( 'NONE',  ( -12.50000000000000533, -3.000000000000000888, -55.91956093573308806 ) ) ;
#102661 = CARTESIAN_POINT ( 'NONE',  ( -43.51067860848499436, 485.4417974898086641, 3.909400899866716461 ) ) ;
#102662 = DIRECTION ( 'NONE',  ( -1.000000000000000000, -1.224606353822377258E-16, -0.000000000000000000 ) ) ;
#102663 = CARTESIAN_POINT ( 'NONE',  ( 32.70701262248892505, 465.7750753107771970, 13.84670167513632144 ) ) ;
#102664 = CARTESIAN_POINT ( 'NONE',  ( -7.499999999999999112, 1.443375672974058110, -7.063244554130000630 ) ) ;
#102665 = ORIENTED_EDGE ( 'NONE', *, *, #57170, .T. ) ;
#102666 = CARTESIAN_POINT ( 'NONE',  ( 92.28783886427984839, -60.00000000000001421, 1.681624045158784719 ) ) ;
#102667 = CARTESIAN_POINT ( 'NONE',  ( -10.45249458729210090, 46.08328249563463430, -12.90779740156156663 ) ) ;
#102668 = CARTESIAN_POINT ( 'NONE',  ( 5.947762761376479190, -6.880090707843049103, 1.083333333333333259 ) ) ;
#102669 = CARTESIAN_POINT ( 'NONE',  ( -35.45332598873516616, 373.5548271054980773, 5.144531785461577300 ) ) ;
#102670 = CARTESIAN_POINT ( 'NONE',  ( -6.686882633394676034, 40.00000000008991918, -71.19596940281091690 ) ) ;
#102671 = CARTESIAN_POINT ( 'NONE',  ( -12.01037645372310791, 17.07677055236747421, -9.138074232161729427 ) ) ;
#102672 = ORIENTED_EDGE ( 'NONE', *, *, #58682, .F. ) ;
#102673 = EDGE_CURVE ( 'NONE', #59491, #94655, #10217, .T. ) ;
#102674 = CARTESIAN_POINT ( 'NONE',  ( -96.30420021061665636, -29.99999999998855316, 199.8843319236383138 ) ) ;
#102675 = EDGE_LOOP ( 'NONE', ( #75724, #87645, #69016, #105136 ) ) ;
#102676 = CARTESIAN_POINT ( 'NONE',  ( -9.864331116128868260, -57.59319873990106231, 25.34043079474438898 ) ) ;
#102677 = SURFACE_STYLE_USAGE ( .BOTH. , #36399 ) ;
#102678 = CARTESIAN_POINT ( 'NONE',  ( 58.18888888888888999, 6.915964383211875250E-15, 0.000000000000000000 ) ) ;
#102679 = CARTESIAN_POINT ( 'NONE',  ( 15.76925030630952485, 22.49347711646982262, 2.473099622756875338 ) ) ;
#102680 = CARTESIAN_POINT ( 'NONE',  ( 0.000000000000000000, 34.00000000000000711, -11.18527996897366528 ) ) ;
#102681 = CARTESIAN_POINT ( 'NONE',  ( 5.082755093536324154, -33.21875000204838813, 5.082755093536326818 ) ) ;
#102682 = CARTESIAN_POINT ( 'NONE',  ( -17.59489243402637371, 34.17351006103357491, 23.98382166917486558 ) ) ;
#102683 = CARTESIAN_POINT ( 'NONE',  ( 0.000000000000000000, 0.000000000000000000, 0.000000000000000000 ) ) ;
#102684 = VERTEX_POINT ( 'NONE', #12575 ) ;
#102686 = EDGE_CURVE ( 'NONE', #101241, #89169, #12050, .T. ) ;
#102685 = LINE ( 'NONE', #95658, #78692 ) ;
#102687 = EDGE_LOOP ( 'NONE', ( #464, #98237, #47311, #89815, #82007, #58170 ) ) ;
#102688 = CARTESIAN_POINT ( 'NONE',  ( 48.02835407290504577, 9.771516447483525880, -16.85535821593549954 ) ) ;
#102690 = VERTEX_POINT ( 'NONE', #76255 ) ;
#102689 = CYLINDRICAL_SURFACE ( 'NONE', #25331, 5.000000000000002665 ) ;
#102691 = CARTESIAN_POINT ( 'NONE',  ( 79.60604231873648473, -42.96535285804148430, 147.0936545434987579 ) ) ;
#102692 = CIRCLE ( 'NONE', #56135, 5.000000000000011546 ) ;
#102693 = ORIENTED_EDGE ( 'NONE', *, *, #39102, .T. ) ;
#102694 = EDGE_CURVE ( 'NONE', #40108, #66555, #94042, .T. ) ;
#102695 = CARTESIAN_POINT ( 'NONE',  ( 2.751717838649724079, -49.70119617224028730, 40.86150536811170753 ) ) ;
#102696 = CARTESIAN_POINT ( 'NONE',  ( 7.188101187500000933, -17.56250000204838457, -2.977408999572650483 ) ) ;
#102697 = CARTESIAN_POINT ( 'NONE',  ( -75.26480569136067800, -57.56533996972894585, 191.5310976926263322 ) ) ;
#102698 = CIRCLE ( 'NONE', #33804, 2.999999999999999112 ) ;
#102699 = ORIENTED_EDGE ( 'NONE', *, *, #58880, .F. ) ;
#102700 = B_SPLINE_CURVE_WITH_KNOTS ( 'NONE', 3,
 ( #93846, #38680, #80169, #71546, #30599, #62950, #104450, #39212, #72087, #104994, #31138, #25161, #33245, #59107, #91475, #33779, #17590, #66655, #106570, #32721 ),
 .UNSPECIFIED., .F., .F.,
 ( 4, 2, 2, 2, 2, 2, 2, 2, 2, 4 ),
 ( 0.007841668765295708304, 0.008346380259883516214, 0.008851091754471324125, 0.009103447501765230682, 0.009355803249059137239, 0.009860514743646950353, 0.01036522623823476347, 0.01086993773282257658, 0.01137464922741038970, 0.01187936072199820281 ),
 .UNSPECIFIED. ) ;
#102701 = CARTESIAN_POINT ( 'NONE',  ( -5.982126593009819970, -13.97334227892932290, 0.5333292889181908691 ) ) ;
#102702 = FACE_OUTER_BOUND ( 'NONE', #61273, .T. ) ;
#102703 = DIRECTION ( 'NONE',  ( 0.000000000000000000, 1.000000000000000000, 0.000000000000000000 ) ) ;
#102704 = CARTESIAN_POINT ( 'NONE',  ( -5.656854249492381470, -16.25000000409677270, 5.656854249492379694 ) ) ;
#102705 = CARTESIAN_POINT ( 'NONE',  ( -51.39279124642569485, -29.89994363668846589, 48.98449833262483821 ) ) ;
#102706 = CIRCLE ( 'NONE', #25205, 2.000000000000001776 ) ;
#102707 = SURFACE_STYLE_USAGE ( .BOTH. , #45548 ) ;
#102708 =( GEOMETRIC_REPRESENTATION_CONTEXT ( 3 ) GLOBAL_UNCERTAINTY_ASSIGNED_CONTEXT ( ( #70946 ) ) GLOBAL_UNIT_ASSIGNED_CONTEXT ( ( #38052, #49807, #89755 ) ) REPRESENTATION_CONTEXT ( 'NONE', 'WORKASPACE' ) );
#102709 = CARTESIAN_POINT ( 'NONE',  ( 5.700000000000000178, 0.000000000000000000, -4.400000000000000355 ) ) ;
#102710 = CARTESIAN_POINT ( 'NONE',  ( 7.500000000000003553, 7.934965735923709573, -31.00258070019285839 ) ) ;
#102711 = CARTESIAN_POINT ( 'NONE',  ( 4.189287965499270072, 52.12930734542786126, 6.683032746053408246 ) ) ;
#102712 = DIRECTION ( 'NONE',  ( 0.9241844797253264687, 0.000000000000000000, 0.3819463934046607445 ) ) ;
#102713 = CARTESIAN_POINT ( 'NONE',  ( 0.8498388482167839042, -29.99999999999998934, -7.699168385716881780 ) ) ;
#102714 = EDGE_LOOP ( 'NONE', ( #6058, #39672, #2659 ) ) ;
#102716 = CIRCLE ( 'NONE', #23523, 0.4000000000000001887 ) ;
#102715 = CARTESIAN_POINT ( 'NONE',  ( -4.140888306088402970, -48.57836392318088059, 40.56393780175194763 ) ) ;
#102717 = SURFACE_SIDE_STYLE ('',( #36435 ) ) ;
#102718 = CIRCLE ( 'NONE', #50954, 4.000000000000001776 ) ;
#102719 = CARTESIAN_POINT ( 'NONE',  ( 8.021436534415164826E-15, 80.00000000000000000, 65.50000000000000000 ) ) ;
#102720 = CARTESIAN_POINT ( 'NONE',  ( -44.85365888377566534, -27.62284328472143002, -35.79871730042521705 ) ) ;
#102721 = CARTESIAN_POINT ( 'NONE',  ( -84.24606464348262591, -30.00000000000000000, 163.2190891219070465 ) ) ;
#102722 = CARTESIAN_POINT ( 'NONE',  ( 96.28888888888889142, 1.023464760207051730E-14, 0.000000000000000000 ) ) ;
#102723 = EDGE_CURVE ( 'NONE', #89178, #78936, #26690, .T. ) ;
#102724 = ORIENTED_EDGE ( 'NONE', *, *, #41088, .F. ) ;
#102725 = AXIS2_PLACEMENT_3D ( 'NONE', #9798, #42714, #51320 ) ;
#102726 = DIRECTION ( 'NONE',  ( 1.000000000000000000, 0.000000000000000000, -0.000000000000000000 ) ) ;
#102727 = CARTESIAN_POINT ( 'NONE',  ( 77.69090662619261423, -57.51539192374901432, 196.1345721221005931 ) ) ;
#102728 = VECTOR ( 'NONE', #72282, 1000.000000000000000 ) ;
#102729 = CARTESIAN_POINT ( 'NONE',  ( 44.03912857151497917, 435.2850055576267323, 15.29440791315701098 ) ) ;
#102730 = ADVANCED_FACE ( 'NONE', ( #92976 ), #32672, .T. ) ;
#102731 = EDGE_CURVE ( 'NONE', #64937, #71316, #20746, .T. ) ;
#102732 = DIRECTION ( 'NONE',  ( 0.000000000000000000, 1.000000000000000000, 0.000000000000000000 ) ) ;
#102733 = CARTESIAN_POINT ( 'NONE',  ( -14.37769637068204709, 21.52932494089419180, -5.240976541736561245 ) ) ;
#102734 = CARTESIAN_POINT ( 'NONE',  ( 9.349999999999997868, -3.309499999999999886, 4.475777889183790779E-16 ) ) ;
#102735 = CARTESIAN_POINT ( 'NONE',  ( -53.51261712237818813, -59.99999999999999289, 81.06700852216475539 ) ) ;
#102736 = ADVANCED_FACE ( 'NONE', ( #67650 ), #51448, .F. ) ;
#102737 = CIRCLE ( 'NONE', #73459, 4.000000000000001776 ) ;
#102738 = CARTESIAN_POINT ( 'NONE',  ( -84.23439574659690265, -57.43960185101178695, 191.0516973466356490 ) ) ;
#102739 = ORIENTED_EDGE ( 'NONE', *, *, #53322, .T. ) ;
#102740 = CARTESIAN_POINT ( 'NONE',  ( 35.70858988364064146, 426.6102125256102227, 5.236736094956324195 ) ) ;
#102741 = CARTESIAN_POINT ( 'NONE',  ( -1.010379499472258136, -46.43937201709040608, 31.62954529578411567 ) ) ;
#102742 = CARTESIAN_POINT ( 'NONE',  ( -6.951447413152006760, 41.73217189154441087, -59.36631701933645644 ) ) ;
#102743 = CARTESIAN_POINT ( 'NONE',  ( 0.000000000000000000, 0.000000000000000000, 0.000000000000000000 ) ) ;
#102744 = EDGE_CURVE ( 'NONE', #48691, #87871, #61919, .T. ) ;
#102745 = CARTESIAN_POINT ( 'NONE',  ( 3.659159783247726268E-15, 10.71892156097790583, 14.93965356295127478 ) ) ;
#102746 = CARTESIAN_POINT ( 'NONE',  ( 25.53945892759312031, 0.000000000000000000, 5.000000000000002665 ) ) ;
#102747 = FILL_AREA_STYLE ('',( #20287 ) ) ;
#102748 = CARTESIAN_POINT ( 'NONE',  ( 33.86650669486618881, -3.999999999999998224, 0.000000000000000000 ) ) ;
#102749 = ORIENTED_EDGE ( 'NONE', *, *, #38224, .F. ) ;
#102750 = CARTESIAN_POINT ( 'NONE',  ( 17.72825544378323315, 50.00000000000000711, 62.31995822720367073 ) ) ;
#102751 = DIRECTION ( 'NONE',  ( 1.000000000000000000, -0.000000000000000000, -0.000000000000000000 ) ) ;
#102752 = EDGE_CURVE ( 'NONE', #34646, #79234, #106685, .T. ) ;
#102753 = CARTESIAN_POINT ( 'NONE',  ( -12.70248734011669356, -4.285714285715063632, 22.03900363279318597 ) ) ;
#102754 = DIRECTION ( 'NONE',  ( -1.000000000000000000, -0.000000000000000000, -0.000000000000000000 ) ) ;
#102755 = CARTESIAN_POINT ( 'NONE',  ( 101.8005042720997864, -59.99999999999995026, 77.51357286062189189 ) ) ;
#102756 = CARTESIAN_POINT ( 'NONE',  ( -81.82631429444417392, -22.15562358550804589, 138.5281546227773504 ) ) ;
#102757 = ORIENTED_EDGE ( 'NONE', *, *, #44800, .T. ) ;
#102758 = SURFACE_STYLE_FILL_AREA ( #95729 ) ;
#102759 = CARTESIAN_POINT ( 'NONE',  ( 4.497431761510343406, 250.5409812425103837, -3.972160586670077542 ) ) ;
#102760 = DIRECTION ( 'NONE',  ( -1.000000000000000000, -0.000000000000000000, -0.000000000000000000 ) ) ;
#102761 = CARTESIAN_POINT ( 'NONE',  ( 45.18811156849615429, 356.2875363396749435, 4.031983282298342353 ) ) ;
#102762 = CARTESIAN_POINT ( 'NONE',  ( 33.78214696664169736, 461.9283422808849764, 7.821959642284836534 ) ) ;
#102763 = ORIENTED_EDGE ( 'NONE', *, *, #8754, .T. ) ;
#102764 = PRESENTATION_LAYER_ASSIGNMENT (  '', '', ( #80331 ) ) ;
#102765 = CARTESIAN_POINT ( 'NONE',  ( -32.46316046841231184, 488.6793347432158043, 9.801212136597996505 ) ) ;
#102766 = CARTESIAN_POINT ( 'NONE',  ( 31.13400694707459238, 439.5192420142489027, 23.00466474004402073 ) ) ;
#102767 = CARTESIAN_POINT ( 'NONE',  ( 5.082755093536325930, -23.46875000204838457, -5.082755093536325042 ) ) ;
#102768 = VERTEX_POINT ( 'NONE', #106214 ) ;
#102769 = CYLINDRICAL_SURFACE ( 'NONE', #29265, 65.00000000000000000 ) ;
#102770 = CARTESIAN_POINT ( 'NONE',  ( 0.000000000000000000, 0.000000000000000000, 0.000000000000000000 ) ) ;
#102771 = CARTESIAN_POINT ( 'NONE',  ( 6.302263272061760624, 41.90661423598773894, -70.03646374312130263 ) ) ;
#102772 = AXIS2_PLACEMENT_3D ( 'NONE', #73637, #24600, #38656 ) ;
#102773 = CARTESIAN_POINT ( 'NONE',  ( -16.64348903516496136, 45.60392139269943357, -6.657797401562710604 ) ) ;
#102774 = CARTESIAN_POINT ( 'NONE',  ( 6.138844529812615747, -12.09084599930882931, -8.896264339907997254 ) ) ;
#102775 =( NAMED_UNIT ( * ) PLANE_ANGLE_UNIT ( ) SI_UNIT ( $, .RADIAN. ) );
#102776 = VERTEX_POINT ( 'NONE', #15626 ) ;
#102777 = CARTESIAN_POINT ( 'NONE',  ( 1.405425598185054066E-06, -60.00000000000000711, -42.63907915653317104 ) ) ;
#102778 = AXIS2_PLACEMENT_3D ( 'NONE', #45308, #1623, #34585 ) ;
#102779 = VECTOR ( 'NONE', #38681, 1000.000000000000000 ) ;
#102781 = CARTESIAN_POINT ( 'NONE',  ( 29.17015437932591126, -53.38279045855296090, 35.28568588006530860 ) ) ;
#102780 = CARTESIAN_POINT ( 'NONE',  ( -72.31573431813527009, -14.21045842199431064, 125.5062215401438266 ) ) ;
#102782 = CYLINDRICAL_SURFACE ( 'NONE', #97219, 4.000000000000001776 ) ;
#102783 = ORIENTED_EDGE ( 'NONE', *, *, #48925, .F. ) ;
#102784 = CARTESIAN_POINT ( 'NONE',  ( -35.65114319003946264, -36.04324675791306021, 35.00216631688633129 ) ) ;
#102785 = ORIENTED_EDGE ( 'NONE', *, *, #93560, .T. ) ;
#102786 = PRODUCT_DEFINITION_SHAPE ( 'NONE', 'NONE',  #106803 ) ;
#102787 = STYLED_ITEM ( 'NONE', ( #94608 ), #23974 ) ;
#102788 = CIRCLE ( 'NONE', #73418, 3.309500000000001663 ) ;
#102789 = PRESENTATION_STYLE_ASSIGNMENT (( #28401 ) ) ;
#102790 = CARTESIAN_POINT ( 'NONE',  ( -13.77150638301485941, -57.01344421731529621, 24.47399976921181519 ) ) ;
#102791 = STYLED_ITEM ( 'NONE', ( #19743 ), #3575 ) ;
#102792 = CIRCLE ( 'NONE', #94169, 18.00000000000000000 ) ;
#102793 = DIRECTION ( 'NONE',  ( 0.000000000000000000, 0.000000000000000000, 1.000000000000000000 ) ) ;
#102794 = CARTESIAN_POINT ( 'NONE',  ( 6.943482370013978944, -64.47151629739275336, 3.973876482044369940 ) ) ;
#102795 = CARTESIAN_POINT ( 'NONE',  ( 11.46095665410260267, -1.517388566600422539, 20.53707809498644821 ) ) ;
#102796 = ORIENTED_EDGE ( 'NONE', *, *, #1218, .T. ) ;
#102797 = CARTESIAN_POINT ( 'NONE',  ( -69.38341510186705818, -38.33187031249859444, 131.7580717154634726 ) ) ;
#102798 = CARTESIAN_POINT ( 'NONE',  ( 101.1080780491627991, -29.99999999999998224, 175.1557127305151198 ) ) ;
#102799 = CARTESIAN_POINT ( 'NONE',  ( 62.59428447264396311, 6.856755485862130937E-15, 0.000000000000000000 ) ) ;
#102800 = CIRCLE ( 'NONE', #82137, 1.999999999999999556 ) ;
#102801 = CARTESIAN_POINT ( 'NONE',  ( -5.858824175751784047, -81.21420939127644090, -1.318356988357131998 ) ) ;
#102802 = CARTESIAN_POINT ( 'NONE',  ( 80.98407313594076129, -30.00000000000000355, -11.93458638676729144 ) ) ;
#102803 =( BOUNDED_CURVE ( )  B_SPLINE_CURVE ( 2, ( #104901, #46647, #20847, #95219, #6177, #79547, #5659, #87131, #46134 ),
 .UNSPECIFIED., .F., .F. ) 
 B_SPLINE_CURVE_WITH_KNOTS ( ( 3, 2, 2, 2, 3 ),
 ( 0.5147058823529412352, 0.5220588235294119084, 0.5294117647058824705, 0.5367647058823529216, 0.5441176470588234837 ),
 .UNSPECIFIED. ) 
 CURVE ( )  GEOMETRIC_REPRESENTATION_ITEM ( )  RATIONAL_B_SPLINE_CURVE ( ( 0.9999999999999988898, 0.9238795325112878487, 1.000000000000000000, 0.9238795325112867385, 1.000000000000000000, 0.9238795325112867385, 1.000000000000000000, 0.9238795325112867385, 1.000000000000000000 ) ) 
 REPRESENTATION_ITEM ( '' )  );
#102804 = DIRECTION ( 'NONE',  ( 0.000000000000000000, -1.000000000000000000, 0.000000000000000000 ) ) ;
#102805 = ORIENTED_EDGE ( 'NONE', *, *, #47328, .F. ) ;
#102806 = EDGE_CURVE ( 'NONE', #11951, #64333, #20822, .T. ) ;
#102807 = EDGE_CURVE ( 'NONE', #72268, #43607, #15389, .T. ) ;
#102808 = VERTEX_POINT ( 'NONE', #56610 ) ;
#102809 = ORIENTED_EDGE ( 'NONE', *, *, #89175, .F. ) ;
#102810 = CARTESIAN_POINT ( 'NONE',  ( 4.592425496802573972E-16, 0.000000000000000000, 3.500000000000000000 ) ) ;
#102811 = CARTESIAN_POINT ( 'NONE',  ( 19.53694868228239301, 43.95068891796171329, -83.64113614449196632 ) ) ;
#102812 = FACE_OUTER_BOUND ( 'NONE', #66585, .T. ) ;
#102813 = CARTESIAN_POINT ( 'NONE',  ( 48.02835407290544367, -1.200000000000000030E-05, 14.35535821593427386 ) ) ;
#102814 = CARTESIAN_POINT ( 'NONE',  ( -7.743982712349851916, -88.46213014760735405, 2.020119794285909709 ) ) ;
#102815 = EDGE_CURVE ( 'NONE', #78081, #58076, #44663, .T. ) ;
#102816 = DIRECTION ( 'NONE',  ( 0.000000000000000000, -1.000000000000000000, 0.000000000000000000 ) ) ;
#102817 = ORIENTED_EDGE ( 'NONE', *, *, #58862, .T. ) ;
#102819 = EDGE_CURVE ( 'NONE', #44784, #25785, #18893, .T. ) ;
#102818 = CARTESIAN_POINT ( 'NONE',  ( 5.036189802309444907, 49.99999999999999289, -76.26213611588271135 ) ) ;
#102820 = ORIENTED_EDGE ( 'NONE', *, *, #89043, .T. ) ;
#102821 = CARTESIAN_POINT ( 'NONE',  ( -4.660674839411964143, -63.68217514695592740, -3.778981567323764335 ) ) ;
#102822 = CARTESIAN_POINT ( 'NONE',  ( 60.44875679912436084, -38.34244523237531155, 97.82314019685307471 ) ) ;
#102823 = CARTESIAN_POINT ( 'NONE',  ( 24.62001147270324353, 295.5497811818883065, 2.086785639818852456 ) ) ;
#102824 = CONICAL_SURFACE ( 'NONE', #104494, 4.172000000000001485, 0.9599310885968750373 ) ;
#102825 = DIRECTION ( 'NONE',  ( -1.000000000000000000, -0.000000000000000000, -0.000000000000000000 ) ) ;
#102826 = CARTESIAN_POINT ( 'NONE',  ( 62.38096262930346114, -60.33914173519230673, 89.28673981057380615 ) ) ;
#102827 = ORIENTED_EDGE ( 'NONE', *, *, #7938, .F. ) ;
#102828 = ADVANCED_FACE ( 'NONE', ( #81942 ), #86243, .T. ) ;
#102829 = CARTESIAN_POINT ( 'NONE',  ( 16.64348903516523848, -1.200000000000000030E-05, 4.157797401561420081 ) ) ;
#102830 = COLOUR_RGB ( '', 0.08235294, 0.09019608, 0.10196078) ;
#102831 = CARTESIAN_POINT ( 'NONE',  ( 73.59428447264397732, 6.856755485862130937E-15, 0.000000000000000000 ) ) ;
#102832 = CARTESIAN_POINT ( 'NONE',  ( -41.58031631500816871, 436.8046394031031809, 6.058257849348906987 ) ) ;
#102833 = LINE ( 'NONE', #46706, #78974 ) ;
#102834 = EDGE_LOOP ( 'NONE', ( #15565, #15109, #67530, #67268 ) ) ;
#102835 = SURFACE_STYLE_FILL_AREA ( #20909 ) ;
#102836 = DIRECTION ( 'NONE',  ( -0.000000000000000000, -1.000000000000000000, -0.000000000000000000 ) ) ;
#102837 = DIRECTION ( 'NONE',  ( 0.000000000000000000, -1.000000000000000000, -0.000000000000000000 ) ) ;
#102838 = CARTESIAN_POINT ( 'NONE',  ( 2.494577234427376227E-15, -18.92596047533412573, 20.36976895023282097 ) ) ;
#102839 = DIRECTION ( 'NONE',  ( 0.5735764363510442720, -0.8191520442889930198, 1.003171929053526349E-16 ) ) ;
#102840 = CARTESIAN_POINT ( 'NONE',  ( 86.43023946451208417, -24.51488847468812793, 183.3687221833509966 ) ) ;
#102841 = PRESENTATION_LAYER_ASSIGNMENT (  '', '', ( #30561 ) ) ;
#102842 = CARTESIAN_POINT ( 'NONE',  ( -5.213184022122961281, 6.017063975410835930, -26.57603910408765202 ) ) ;
#102843 =( GEOMETRIC_REPRESENTATION_CONTEXT ( 3 ) GLOBAL_UNCERTAINTY_ASSIGNED_CONTEXT ( ( #40794 ) ) GLOBAL_UNIT_ASSIGNED_CONTEXT ( ( #29367, #95141, #13123 ) ) REPRESENTATION_CONTEXT ( 'NONE', 'WORKASPACE' ) );
#102844 = CARTESIAN_POINT ( 'NONE',  ( -9.426441968764315504, 10.21013571251764418, 4.999999999999999112 ) ) ;
#102845 = VERTEX_POINT ( 'NONE', #103723 ) ;
#102846 = DIRECTION ( 'NONE',  ( 0.000000000000000000, 0.000000000000000000, -1.000000000000000000 ) ) ;
#102847 = CARTESIAN_POINT ( 'NONE',  ( 36.58860353225821882, -23.84130847726161662, -30.99593518099760558 ) ) ;
#102848 = DIRECTION ( 'NONE',  ( 0.000000000000000000, 0.5000000000000008882, -0.8660254037844381525 ) ) ;
#102849 = FILL_AREA_STYLE_COLOUR ( '', #757 ) ;
#102850 = CARTESIAN_POINT ( 'NONE',  ( 35.22753116013103636, 435.7360350475310042, 6.213956812072554570 ) ) ;
#102851 = CARTESIAN_POINT ( 'NONE',  ( -100.3439110779055312, -29.99999999999999645, 157.3914886282430246 ) ) ;
#102852 = EDGE_CURVE ( 'NONE', #14808, #40836, #60473, .T. ) ;
#102853 = CARTESIAN_POINT ( 'NONE',  ( -2.500000000000001332, 1.089935651241144160E-15, -8.900000000000000355 ) ) ;
#102854 = CIRCLE ( 'NONE', #56313, 4.000000000000001776 ) ;
#102855 = CARTESIAN_POINT ( 'NONE',  ( 19.65360057920942438, -57.67192277060839700, 42.16630265707282632 ) ) ;
#102857 = CYLINDRICAL_SURFACE ( 'NONE', #91265, 5.000000000000002665 ) ;
#102856 = DIRECTION ( 'NONE',  ( -1.000000000000000000, -1.224606353822377258E-16, -0.000000000000000000 ) ) ;
#102858 = EDGE_CURVE ( 'NONE', #103547, #29512, #99988, .T. ) ;
#102859 = EDGE_CURVE ( 'NONE', #31486, #17102, #24263, .T. ) ;
#102860 = CARTESIAN_POINT ( 'NONE',  ( -18.45708139111118484, 49.99999999999999289, 61.31329639225923955 ) ) ;
#102861 = AXIS2_PLACEMENT_3D ( 'NONE', #6104, #71911, #23387 ) ;
#102862 = COLOUR_RGB ( '', 0.08235294, 0.09019608, 0.10196078) ;
#102863 = VECTOR ( 'NONE', #105666, 1000.000000000000000 ) ;
#102864 = DIRECTION ( 'NONE',  ( 0.000000000000000000, -1.000000000000000000, 0.000000000000000000 ) ) ;
#102865 =( NAMED_UNIT ( * ) PLANE_ANGLE_UNIT ( ) SI_UNIT ( $, .RADIAN. ) );
#102866 = VERTEX_POINT ( 'NONE', #66850 ) ;
#102867 = FACE_OUTER_BOUND ( 'NONE', #39267, .T. ) ;
#102868 =( NAMED_UNIT ( * ) PLANE_ANGLE_UNIT ( ) SI_UNIT ( $, .RADIAN. ) );
#102869 = AXIS2_PLACEMENT_3D ( 'NONE', #54025, #13037, #88019 ) ;
#102870 = CARTESIAN_POINT ( 'NONE',  ( -18.02399320543497296, -46.43928582069488442, 31.96005001963083458 ) ) ;
#102872 = CARTESIAN_POINT ( 'NONE',  ( 1.219658573673010116, 36.86119053457258588, -28.18247609706499546 ) ) ;
#102871 = CARTESIAN_POINT ( 'NONE',  ( -86.66579604520306646, -60.00000000000000711, -0.1178683406456105670 ) ) ;
#102873 = ORIENTED_EDGE ( 'NONE', *, *, #69001, .T. ) ;
#102874 = B_SPLINE_CURVE_WITH_KNOTS ( 'NONE', 3,
 ( #69865, #34867, #102759, #20838, #10020, #18683, #100621, #84453, #69344, #44533, #42927, #35400, #92528, #51539, #28372, #68813, #43464, #26783, #43989, #59652, #101696, #76340, #2453, #68268, #27323, #93072, #19238, #76876, #85524, #11602, #14255, #79534, #80056, #30482, #13193, #54710 ),
 .UNSPECIFIED., .F., .F.,
 ( 4, 2, 2, 2, 2, 2, 2, 2, 2, 2, 2, 2, 2, 2, 2, 2, 2, 4 ),
 ( 2.830577590387642528E-17, 0.0008074604767267502771, 0.001614920953453472799, 0.002422381430180194778, 0.003229841906906917408, 0.004037302383633640038, 0.004844762860360361800, 0.005652223337087083563, 0.006459683813813806193, 0.007267144290540527955, 0.008074604767267248850, 0.008882065243993970613, 0.009689525720720692376, 0.01049698619744741414, 0.01130444667417413764, 0.01211190715090085940, 0.01251563738926421941, 0.01291936762762757943 ),
 .UNSPECIFIED. ) ;
#102875 = CARTESIAN_POINT ( 'NONE',  ( 30.00000000000000000, 1.836970198721029589E-15, -15.00000000000000000 ) ) ;
#102876 = ORIENTED_EDGE ( 'NONE', *, *, #105684, .T. ) ;
#102877 = DIRECTION ( 'NONE',  ( -0.000000000000000000, -1.000000000000000000, -0.000000000000000000 ) ) ;
#102878 = CARTESIAN_POINT ( 'NONE',  ( 16.01541666090335880, 3.834101040393494753, -1.299565945645027920 ) ) ;
#102879 = AXIS2_PLACEMENT_3D ( 'NONE', #18325, #68458, #26439 ) ;
#102880 = CARTESIAN_POINT ( 'NONE',  ( -5.422877198588844649, -59.99999999999999289, -42.58549929937262135 ) ) ;
#102881 = EDGE_LOOP ( 'NONE', ( #51941, #95740 ) ) ;
#102882 = FACE_BOUND ( 'NONE', #91377, .T. ) ;
#102883 = CARTESIAN_POINT ( 'NONE',  ( 8.866506694866188809, 4.898587196589413815E-16, -4.000000000000000888 ) ) ;
#102884 = CARTESIAN_POINT ( 'NONE',  ( 102.0397306347427104, -52.72302187501731652, 192.0072258283632323 ) ) ;
#102886 = DIRECTION ( 'NONE',  ( 1.000000000000000000, -0.000000000000000000, -0.000000000000000000 ) ) ;
#102885 = CARTESIAN_POINT ( 'NONE',  ( 99.75754961941544252, 1.030564683017419500E-14, 0.000000000000000000 ) ) ;
#102887 = ADVANCED_FACE ( 'NONE', ( #1554 ), #23287, .T. ) ;
#102888 = VECTOR ( 'NONE', #40540, 1000.000000000000000 ) ;
#102889 = ORIENTED_EDGE ( 'NONE', *, *, #62048, .T. ) ;
#102890 = VERTEX_POINT ( 'NONE', #17777 ) ;
#102891 = CIRCLE ( 'NONE', #32230, 3.400000000000000355 ) ;
#102892 = ORIENTED_EDGE ( 'NONE', *, *, #94830, .T. ) ;
#102893 = CARTESIAN_POINT ( 'NONE',  ( 27.18528066925738429, 312.1751590076182765, 10.69940225286546642 ) ) ;
#102894 = CARTESIAN_POINT ( 'NONE',  ( 7.036764705882354143, 40.00000000373363207, -71.06385277390853616 ) ) ;
#102895 = CARTESIAN_POINT ( 'NONE',  ( 5.799999999999999822, 8.000000000000000000, 0.000000000000000000 ) ) ;
#102896 = ORIENTED_EDGE ( 'NONE', *, *, #98566, .F. ) ;
#102897 = SURFACE_SIDE_STYLE ('',( #61930 ) ) ;
#102898 = CARTESIAN_POINT ( 'NONE',  ( -6.503415501679381983, 41.93912328290132052, -68.91429205811094505 ) ) ;
#102899 = CARTESIAN_POINT ( 'NONE',  ( -94.80066220543719169, -60.00000000000000000, -0.2464906575786718901 ) ) ;
#102900 = FACE_BOUND ( 'NONE', #328, .T. ) ;
#102901 = CARTESIAN_POINT ( 'NONE',  ( 21.98983231224196544, -60.00000000000000000, 40.51305684052432809 ) ) ;
#102902 = CARTESIAN_POINT ( 'NONE',  ( -16.24780601832367566, -5.000000000000000000, 2.396121698210679885 ) ) ;
#102903 = CARTESIAN_POINT ( 'NONE',  ( -6.390966761371486449, 41.59892092783731954, -58.65495520917361461 ) ) ;
#102905 = CARTESIAN_POINT ( 'NONE',  ( 13.57004255533479942, -46.43472687649081365, 31.71508379387893228 ) ) ;
#102904 = CARTESIAN_POINT ( 'NONE',  ( -104.9451182028910239, -14.21045842199441367, 145.4712626202903323 ) ) ;
#102906 = CARTESIAN_POINT ( 'NONE',  ( -7.337702322492915208, 52.18298084268283787, 2.467673208560980491 ) ) ;
#102907 = CARTESIAN_POINT ( 'NONE',  ( -49.06124572357285984, -36.05852591224155645, 48.12833458416420029 ) ) ;
#102908 = VERTEX_POINT ( 'NONE', #75461 ) ;
#102909 = CARTESIAN_POINT ( 'NONE',  ( 4.942316422488831407, -67.89573842932429670, 13.89850810157859229 ) ) ;
#102910 = ORIENTED_EDGE ( 'NONE', *, *, #52011, .F. ) ;
#102911 = CARTESIAN_POINT ( 'NONE',  ( 39.16821133293519352, 459.8632445465572118, 1.901232704179921518 ) ) ;
#102912 = AXIS2_PLACEMENT_3D ( 'NONE', #33229, #17574, #57460 ) ;
#102913 = CARTESIAN_POINT ( 'NONE',  ( 6.000469943554649355, -5.999295083295012709, 0.2622423038614494772 ) ) ;
#102914 = ORIENTED_EDGE ( 'NONE', *, *, #66910, .T. ) ;
#102915 = CARTESIAN_POINT ( 'NONE',  ( -12.56633547050704003, -10.06780447540685408, 11.12955203454668585 ) ) ;
#102916 = AXIS2_PLACEMENT_3D ( 'NONE', #100422, #26588, #66464 ) ;
#102917 = EDGE_LOOP ( 'NONE', ( #95090, #67881, #55186, #56703, #65963 ) ) ;
#102918 = CARTESIAN_POINT ( 'NONE',  ( 89.86244880932272849, -29.99999999998984990, -1.486525042624827986 ) ) ;
#102919 = CARTESIAN_POINT ( 'NONE',  ( 6.641837668257387861, 41.74662779905570176, -59.04567176600482981 ) ) ;
#102920 = CARTESIAN_POINT ( 'NONE',  ( -1.905220702120325443E-14, 42.00000000000000711, -59.23741894013591036 ) ) ;
#102921 = CARTESIAN_POINT ( 'NONE',  ( 100.8396476006763578, -29.99999999999999645, 163.9396555014752437 ) ) ;
#102922 = CARTESIAN_POINT ( 'NONE',  ( 16.36650669486618881, -3.851859888774471706E-31, 4.000000000000000888 ) ) ;
#102923 = VERTEX_POINT ( 'NONE', #100270 ) ;
#102924 = EDGE_CURVE ( 'NONE', #47940, #6569, #93248, .T. ) ;
#102925 = ORIENTED_EDGE ( 'NONE', *, *, #28994, .F. ) ;
#102926 = EDGE_LOOP ( 'NONE', ( #105413, #55761, #59533, #37169 ) ) ;
#102927 = CARTESIAN_POINT ( 'NONE',  ( 55.41416639835406954, -25.62021389884816358, 55.60954475568744471 ) ) ;
#102928 = STYLED_ITEM ( 'NONE', ( #64546 ), #26328 ) ;
#102929 = CARTESIAN_POINT ( 'NONE',  ( 43.02621584241283870, 434.6128289108256695, 16.97888786058994270 ) ) ;
#102930 = CIRCLE ( 'NONE', #87463, 4.000000000000000888 ) ;
#102931 = CARTESIAN_POINT ( 'NONE',  ( -46.00000000000000000, 459.9277931459707247, 6.461582622321701663 ) ) ;
#102932 = ADVANCED_FACE ( 'NONE', ( #28025 ), #12841, .T. ) ;
#102933 = ORIENTED_EDGE ( 'NONE', *, *, #82254, .T. ) ;
#102935 = EDGE_CURVE ( 'NONE', #84625, #42218, #45235, .T. ) ;
#102934 = CARTESIAN_POINT ( 'NONE',  ( 9.176803346051512378, 105.5294715579744178, 3.973598758023531019 ) ) ;
#102936 = VERTEX_POINT ( 'NONE', #29103 ) ;
#102937 = CARTESIAN_POINT ( 'NONE',  ( 2.452879891156805936, 7.244083172395182402, -0.1007566405101772145 ) ) ;
#102938 = CARTESIAN_POINT ( 'NONE',  ( 101.5779485941844626, -38.45071526406401574, 199.8867405208796981 ) ) ;
#102939 = CARTESIAN_POINT ( 'NONE',  ( 11.66348175382439578, 15.91712690338637692, 9.569217749563181385 ) ) ;
#102941 = CARTESIAN_POINT ( 'NONE',  ( 83.72785699625647737, -45.28390520765234584, 8.237543405220815629 ) ) ;
#102940 = CONICAL_SURFACE ( 'NONE', #9911, 3.309500000000001663, 0.9599310885968770357 ) ;
#102942 = CARTESIAN_POINT ( 'NONE',  ( 9.999999999999996447, 15.00000000000000000, -10.00000000000000000 ) ) ;
#102943 = AXIS2_PLACEMENT_3D ( 'NONE', #20808, #78978, #69834 ) ;
#102944 = CARTESIAN_POINT ( 'NONE',  ( 33.08830340003491699, 433.8978689942874212, 24.52079292137695177 ) ) ;
#102945 = AXIS2_PLACEMENT_3D ( 'NONE', #44957, #60087, #44412 ) ;
#102946 = CARTESIAN_POINT ( 'NONE',  ( -42.61140200160144786, 465.9030374194823594, 13.21253569360413849 ) ) ;
#102947 = DIRECTION ( 'NONE',  ( 0.000000000000000000, 1.000000000000000000, 0.000000000000000000 ) ) ;
#102948 = EDGE_CURVE ( 'NONE', #7097, #63004, #13368, .T. ) ;
#102949 = CARTESIAN_POINT ( 'NONE',  ( -38.83326880618827204, 459.9245326792292303, 1.954253696922295447 ) ) ;
#102950 = AXIS2_PLACEMENT_3D ( 'NONE', #67241, #101193, #3020 ) ;
#102951 = ORIENTED_EDGE ( 'NONE', *, *, #95698, .T. ) ;
#102952 = CARTESIAN_POINT ( 'NONE',  ( 15.90864490579649626, 37.20836975595025820, -22.13037531087910992 ) ) ;
#102953 = CARTESIAN_POINT ( 'NONE',  ( -4.250171846664082764, 140.3062447900153700, 4.999999999999999112 ) ) ;
#102954 = VERTEX_POINT ( 'NONE', #29612 ) ;
#102955 = AXIS2_PLACEMENT_3D ( 'NONE', #38403, #88000, #54010 ) ;
#102956 = CARTESIAN_POINT ( 'NONE',  ( -20.21880305278369150, 304.8280059657581660, -9.005058168222323189 ) ) ;
#102957 = CARTESIAN_POINT ( 'NONE',  ( -28.92282554148816587, 311.6946508351041984, 12.06290651036217909 ) ) ;
#102958 = CARTESIAN_POINT ( 'NONE',  ( -12.01455574841702933, -4.758509052971797715, -76.85604808874542471 ) ) ;
#102959 = SURFACE_STYLE_FILL_AREA ( #95930 ) ;
#102960 = CARTESIAN_POINT ( 'NONE',  ( 4.898587196589412829E-16, -19.62499999999999289, -8.000000000000000000 ) ) ;
#102961 = CARTESIAN_POINT ( 'NONE',  ( -2.229368152238511147, -14.88154708191588504, 34.47882516350917825 ) ) ;
#102962 = CARTESIAN_POINT ( 'NONE',  ( 0.000000000000000000, -15.00000000000000000, 0.000000000000000000 ) ) ;
#102963 = ORIENTED_EDGE ( 'NONE', *, *, #60099, .F. ) ;
#102964 = CARTESIAN_POINT ( 'NONE',  ( 85.34274748661711385, -32.19989682491620897, 180.0761885193842886 ) ) ;
#102966 = VECTOR ( 'NONE', #58480, 1000.000000000000000 ) ;
#102965 = CARTESIAN_POINT ( 'NONE',  ( -49.07747248321140887, 8.835459238882952704, 14.91203737403126794 ) ) ;
#102967 = CARTESIAN_POINT ( 'NONE',  ( -15.64519568958363749, 46.18931709473498159, 4.637408661950026101 ) ) ;
#102968 = ORIENTED_EDGE ( 'NONE', *, *, #39854, .T. ) ;
#102969 = CARTESIAN_POINT ( 'NONE',  ( -96.73191789133785790, -60.15505594016180169, 95.88985520306968624 ) ) ;
#102970 = CARTESIAN_POINT ( 'NONE',  ( 0.000000000000000000, 6.928203230275505220, -4.000000000000007994 ) ) ;
#102971 = CARTESIAN_POINT ( 'NONE',  ( 10.50942704840527142, -5.000000000000002665, -93.01494055616910828 ) ) ;
#102972 = CARTESIAN_POINT ( 'NONE',  ( -30.10549840784188902, 7.858493733726967356, 42.03383688247123473 ) ) ;
#102973 = CIRCLE ( 'NONE', #59873, 10.39117206796836257 ) ;
#102974 = CARTESIAN_POINT ( 'NONE',  ( 6.162888688655346670, -3.752776749732575468, -6.499999999999999112 ) ) ;
#102975 = PRESENTATION_STYLE_ASSIGNMENT (( #70075 ) ) ;
#102976 = CIRCLE ( 'NONE', #40993, 4.000000000000007105 ) ;
#102977 = CARTESIAN_POINT ( 'NONE',  ( 7.804325080931074687, -19.38637389769215957, 35.22465547960180743 ) ) ;
#102978 = CARTESIAN_POINT ( 'NONE',  ( 3.301573598373376939, -0.7118794392489854461, 103.9445864789742728 ) ) ;
#102979 = CARTESIAN_POINT ( 'NONE',  ( 50.24570806728828387, -29.73392352015472540, 47.01200513134826764 ) ) ;
#102980 = CONICAL_SURFACE ( 'NONE', #75401, 5.000000000000001776, 0.9599310885968803664 ) ;
#102982 = CARTESIAN_POINT ( 'NONE',  ( -11.79617940926573993, 16.41796236967441303, 9.402036560305605306 ) ) ;
#102981 = CARTESIAN_POINT ( 'NONE',  ( 0.000000000000000000, -3.331654917651224235, 0.000000000000000000 ) ) ;
#102983 = ADVANCED_FACE ( 'NONE', ( #61971 ), #37172, .T. ) ;
#102984 = CARTESIAN_POINT ( 'NONE',  ( 7.653149673922322371, 294.7103690673997107, -6.445128602839910847 ) ) ;
#102985 = CARTESIAN_POINT ( 'NONE',  ( 40.00882285048881926, 314.7542622495009823, 2.793119429658786235 ) ) ;
#102986 = DIRECTION ( 'NONE',  ( 0.000000000000000000, 1.000000000000000000, 0.000000000000000000 ) ) ;
#102987 = FACE_OUTER_BOUND ( 'NONE', #47935, .T. ) ;
#102988 = AXIS2_PLACEMENT_3D ( 'NONE', #95459, #94418, #21605 ) ;
#102989 = ORIENTED_EDGE ( 'NONE', *, *, #57168, .F. ) ;
#102990 = CARTESIAN_POINT ( 'NONE',  ( -82.45001613080906111, -38.00000000000001421, 10.13691710915257183 ) ) ;
#102991 = ORIENTED_EDGE ( 'NONE', *, *, #94948, .F. ) ;
#102992 = CARTESIAN_POINT ( 'NONE',  ( -11.91718080433585314, -2.063830786854366384, 20.64942540265304416 ) ) ;
#102993 = FACE_BOUND ( 'NONE', #28250, .T. ) ;
#102994 = DIRECTION ( 'NONE',  ( 0.000000000000000000, 1.000000000000000000, 0.000000000000000000 ) ) ;
#102995 = ADVANCED_FACE ( 'NONE', ( #36121 ), #46295, .T. ) ;
#102997 = CARTESIAN_POINT ( 'NONE',  ( -7.964568475979583617, -47.40891111626400800, -34.64478426194994398 ) ) ;
#102996 = CARTESIAN_POINT ( 'NONE',  ( 9.918010731619586906, 253.7915168484321384, -1.300854425901589950 ) ) ;
#102998 = ORIENTED_EDGE ( 'NONE', *, *, #70339, .F. ) ;
#102999 = CARTESIAN_POINT ( 'NONE',  ( 33.58349330513380693, 1.593028355512270962E-15, 0.000000000000000000 ) ) ;
#103000 = FACE_OUTER_BOUND ( 'NONE', #59851, .T. ) ;
#103001 = VECTOR ( 'NONE', #40930, 1000.000000000000114 ) ;
#103002 = AXIS2_PLACEMENT_3D ( 'NONE', #73022, #1245, #83780 ) ;
#103003 = ORIENTED_EDGE ( 'NONE', *, *, #76985, .F. ) ;
#103004 = AXIS2_PLACEMENT_3D ( 'NONE', #59115, #32730, #50987 ) ;
#103005 = CARTESIAN_POINT ( 'NONE',  ( 8.082668874372532400E-15, 49.00000000000000000, -66.00000000000000000 ) ) ;
#103006 = LINE ( 'NONE', #29164, #27129 ) ;
#103007 = CARTESIAN_POINT ( 'NONE',  ( -93.39459019562438868, -60.00000000000000000, 36.07653886588029479 ) ) ;
#103008 = CONICAL_SURFACE ( 'NONE', #90926, 7.000000000000000000, 0.9599310885968753704 ) ;
#103009 = ORIENTED_EDGE ( 'NONE', *, *, #23260, .T. ) ;
#103010 = CARTESIAN_POINT ( 'NONE',  ( 66.26095113931063452, 4.000000000000015099, 4.898587196589422689E-16 ) ) ;
#103011 = FACE_BOUND ( 'NONE', #98917, .T. ) ;
#103012 = VECTOR ( 'NONE', #3060, 1000.000000000000000 ) ;
#103013 = CARTESIAN_POINT ( 'NONE',  ( 7.413001015142842931, 41.14546113202533206, -59.83891282166461423 ) ) ;
#103014 = CARTESIAN_POINT ( 'NONE',  ( -9.842984802582137149, 26.40930409524348477, 1.781981959250508618 ) ) ;
#103015 = ADVANCED_FACE ( 'NONE', ( #44172 ), #101692, .T. ) ;
#103017 = LINE ( 'NONE', #62047, #90852 ) ;
#103016 = DIRECTION ( 'NONE',  ( 0.000000000000000000, 0.000000000000000000, 1.000000000000000000 ) ) ;
#103018 = EDGE_CURVE ( 'NONE', #57174, #100925, #84535, .T. ) ;
#103019 = CARTESIAN_POINT ( 'NONE',  ( -80.20997988972960968, -60.39356314814814652, 177.0984289422948734 ) ) ;
#103020 = ORIENTED_EDGE ( 'NONE', *, *, #27648, .F. ) ;
#103021 = CARTESIAN_POINT ( 'NONE',  ( -38.41498555331915554, 491.4234641122523612, 12.30872953874726328 ) ) ;
#103022 = ORIENTED_EDGE ( 'NONE', *, *, #71220, .T. ) ;
#103023 = VERTEX_POINT ( 'NONE', #28549 ) ;
#103024 = CARTESIAN_POINT ( 'NONE',  ( 8.812315315240748959, -4.999999999999999112, -14.88097931264037399 ) ) ;
#103025 = CARTESIAN_POINT ( 'NONE',  ( -3.544943868593964709, -69.77176130519234221, 13.45484724895946904 ) ) ;
#103026 = SURFACE_STYLE_USAGE ( .BOTH. , #93341 ) ;
#103027 = ORIENTED_EDGE ( 'NONE', *, *, #87585, .T. ) ;
#103028 = CARTESIAN_POINT ( 'NONE',  ( 10.59999999999999609, 1.533819458162526451E-15, 0.000000000000000000 ) ) ;
#103029 = CARTESIAN_POINT ( 'NONE',  ( 8.999999999999996447, -4.000000000000003553, 42.58845726811989607 ) ) ;
#103030 = CARTESIAN_POINT ( 'NONE',  ( -92.76317396897962908, -57.65703681568646743, -17.81073576277876569 ) ) ;
#103031 = CARTESIAN_POINT ( 'NONE',  ( 7.551892080562057963, -13.00987702539385005, 2.647003822403974471 ) ) ;
#103032 = DIRECTION ( 'NONE',  ( -1.000000000000000000, -0.000000000000000000, -0.000000000000000000 ) ) ;
#103033 = CARTESIAN_POINT ( 'NONE',  ( 24.20499783611734657, 27.76345924012371924, 31.17339665328782772 ) ) ;
#103034 = CARTESIAN_POINT ( 'NONE',  ( -13.95403936970824965, -50.13007754844869623, 28.16216733762122004 ) ) ;
#103035 = CARTESIAN_POINT ( 'NONE',  ( 3.316968746324254536, 15.92795519102023860, -9.435590127032961405 ) ) ;
#103036 = CARTESIAN_POINT ( 'NONE',  ( 63.50796903478703115, -60.00000000000007816, -37.13796669901890368 ) ) ;
#103037 = CARTESIAN_POINT ( 'NONE',  ( -62.54317499552948334, -60.00000000000000711, 118.0918133646953976 ) ) ;
#103038 = CARTESIAN_POINT ( 'NONE',  ( -54.35042906398516038, -39.50198214953601195, 58.92073034776293383 ) ) ;
#103039 = AXIS2_PLACEMENT_3D ( 'NONE', #48503, #32896, #98651 ) ;
#103040 = EDGE_LOOP ( 'NONE', ( #60594, #30018, #89366 ) ) ;
#103041 = CARTESIAN_POINT ( 'NONE',  ( 42.45811724857436076, 486.4202366696182480, 8.302074271983164166 ) ) ;
#103042 = ORIENTED_EDGE ( 'NONE', *, *, #75605, .F. ) ;
#103043 = CARTESIAN_POINT ( 'NONE',  ( -100.6300002315544901, -45.26144706321691302, 191.8785347955782754 ) ) ;
#103044 = DIRECTION ( 'NONE',  ( -1.000000000000000000, -1.224606353822377258E-16, -0.000000000000000000 ) ) ;
#103045 = CARTESIAN_POINT ( 'NONE',  ( -30.80294602723943598, 13.24188206181652383, -41.41355684762699951 ) ) ;
#103046 = AXIS2_PLACEMENT_3D ( 'NONE', #52913, #2753, #51299 ) ;
#103047 = EDGE_LOOP ( 'NONE', ( #19704, #6272, #65267, #37022 ) ) ;
#103048 = CARTESIAN_POINT ( 'NONE',  ( 19.28427347342524101, 49.84851643466424065, 61.37487176993018778 ) ) ;
#103049 =( NAMED_UNIT ( * ) PLANE_ANGLE_UNIT ( ) SI_UNIT ( $, .RADIAN. ) );
#103050 = FACE_OUTER_BOUND ( 'NONE', #50289, .T. ) ;
#103051 = CARTESIAN_POINT ( 'NONE',  ( -7.188101187500000044, -17.28125000204838813, -8.802885111219163269E-16 ) ) ;
#103052 = CARTESIAN_POINT ( 'NONE',  ( 29.50756122520733271, 297.9063904818165724, 10.61050061783298126 ) ) ;
#103053 = CARTESIAN_POINT ( 'NONE',  ( 41.82792046605465686, 1.340359594676612611E-15, 0.000000000000000000 ) ) ;
#103054 = CARTESIAN_POINT ( 'NONE',  ( 6.928203230275508773, -85.00000000000000000, 4.000000000000001776 ) ) ;
#103055 = CARTESIAN_POINT ( 'NONE',  ( 62.21186031149353113, -30.00000000000000355, 72.58540792779400874 ) ) ;
#103056 = CARTESIAN_POINT ( 'NONE',  ( -8.955352252652177825, 136.0524461000850920, -2.602085213965210247E-15 ) ) ;
#103057 = CARTESIAN_POINT ( 'NONE',  ( -3.313708498984760276, -15.21875000409677270, -8.000000000000000000 ) ) ;
#103058 = CARTESIAN_POINT ( 'NONE',  ( -32.93320410569342016, 485.0465637715133198, 1.208268278909949478 ) ) ;
#103059 = UNCERTAINTY_MEASURE_WITH_UNIT (LENGTH_MEASURE( 1.000000000000000082E-05 ), #88173, 'distance_accuracy_value', 'NONE');
#103060 = CARTESIAN_POINT ( 'NONE',  ( -28.71080020290498780, -42.96128409593538322, 33.31360371976838053 ) ) ;
#103061 = AXIS2_PLACEMENT_3D ( 'NONE', #74193, #46354, #54411 ) ;
#103062 = ORIENTED_EDGE ( 'NONE', *, *, #57003, .T. ) ;
#103063 = CARTESIAN_POINT ( 'NONE',  ( 46.99059970337066261, -56.81049650515272020, 51.30630512147487821 ) ) ;
#103064 = CARTESIAN_POINT ( 'NONE',  ( -0.6187860399584415028, 13.31391022449570194, 49.41005378291666261 ) ) ;
#103065 = CARTESIAN_POINT ( 'NONE',  ( -5.763702088647366217, 13.53577993954648662, -3.972887565972252233 ) ) ;
#103066 = CARTESIAN_POINT ( 'NONE',  ( -87.32597803086463273, -38.58248733736562031, 199.6835492166326560 ) ) ;
#103067 = ORIENTED_EDGE ( 'NONE', *, *, #82819, .T. ) ;
#103068 = CARTESIAN_POINT ( 'NONE',  ( 89.40823501132422280, -38.38738139504339841, -17.29573669771441047 ) ) ;
#103069 = CARTESIAN_POINT ( 'NONE',  ( 13.38477778458014988, 7.844114667846795896, -8.572480637398566472 ) ) ;
#103070 = CARTESIAN_POINT ( 'NONE',  ( 16.84999999999999787, 1.533819458162526451E-15, 0.000000000000000000 ) ) ;
#103071 = PLANE ( 'NONE',  #105660 ) ;
#103072 = CARTESIAN_POINT ( 'NONE',  ( 6.541889319079672305, 41.04792457379606674, -71.02384104322176483 ) ) ;
#103073 = DIRECTION ( 'NONE',  ( 0.000000000000000000, -1.000000000000000000, 0.000000000000000000 ) ) ;
#103074 = CARTESIAN_POINT ( 'NONE',  ( -32.82875765654047484, 434.9824960647666217, 12.61072594640184441 ) ) ;
#103075 = CARTESIAN_POINT ( 'NONE',  ( -30.00000000000000355, 488.8442721620237421, 4.433647275927526721 ) ) ;
#103076 = VECTOR ( 'NONE', #87256, 999.9999999999998863 ) ;
#103077 = CARTESIAN_POINT ( 'NONE',  ( 111.0086579293828493, -60.00000000000002842, 152.2211401378526148 ) ) ;
#103078 = STYLED_ITEM ( 'NONE', ( #102444 ), #68281 ) ;
#103079 = EDGE_CURVE ( 'NONE', #96318, #90212, #86, .T. ) ;
#103080 = CARTESIAN_POINT ( 'NONE',  ( -7.896165657598945842, -68.78911131371971521, -1.307894402814547830 ) ) ;
#103081 = ORIENTED_EDGE ( 'NONE', *, *, #14366, .T. ) ;
#103082 = EDGE_CURVE ( 'NONE', #70272, #72766, #5307, .T. ) ;
#103083 = CARTESIAN_POINT ( 'NONE',  ( 0.000000000000000000, 3.000000000000002665, -13.00000000000003730 ) ) ;
#103084 = SURFACE_STYLE_USAGE ( .BOTH. , #39937 ) ;
#103085 = EDGE_LOOP ( 'NONE', ( #17417, #97141, #65633, #58140 ) ) ;
#103087 = CARTESIAN_POINT ( 'NONE',  ( 5.293319439299095208, 18.44834697312474958, -37.82265432997213850 ) ) ;
#103086 = CARTESIAN_POINT ( 'NONE',  ( -90.92816914291333319, -38.34532242824909787, 3.098464593803623046 ) ) ;
#103088 = CARTESIAN_POINT ( 'NONE',  ( 46.00000000000000711, 437.9187945550052063, 12.32659313045543747 ) ) ;
#103089 = CARTESIAN_POINT ( 'NONE',  ( 9.235395886531431551E-16, -3.000000000000000000, -8.000000000000000000 ) ) ;
#103090 = DIRECTION ( 'NONE',  ( 0.000000000000000000, -1.000000000000000000, 0.000000000000000000 ) ) ;
#103091 = CARTESIAN_POINT ( 'NONE',  ( -2.977408999572650039, -16.06250000204838457, -7.188101187500001821 ) ) ;
#103092 = VECTOR ( 'NONE', #75422, 1000.000000000000000 ) ;
#103093 = CARTESIAN_POINT ( 'NONE',  ( -9.739726766100238464, -5.000000000005447198, -87.61747884500121586 ) ) ;
#103094 = CIRCLE ( 'NONE', #37681, 5.000000000000011546 ) ;
#103095 = AXIS2_PLACEMENT_3D ( 'NONE', #89033, #98174, #24328 ) ;
#103096 = CARTESIAN_POINT ( 'NONE',  ( 30.92872287337538850, 13.87446774603010979, -40.98770496732647217 ) ) ;
#103098 = ORIENTED_EDGE ( 'NONE', *, *, #9585, .F. ) ;
#103097 = DIRECTION ( 'NONE',  ( -0.5735764363510497121, 0.8191520442889892450, 1.003171929053521665E-16 ) ) ;
#103099 = CARTESIAN_POINT ( 'NONE',  ( 83.25611969625570907, -39.47771237622612261, 172.2730610428070008 ) ) ;
#103100 = CARTESIAN_POINT ( 'NONE',  ( 8.427926236130485194, 28.44948122801527646, 3.851859888774447621E-31 ) ) ;
#103101 = CARTESIAN_POINT ( 'NONE',  ( 0.5620262070071395666, -7.564407249984330228, -6.443844059477459751 ) ) ;
#103102 = ORIENTED_EDGE ( 'NONE', *, *, #29002, .F. ) ;
#103103 = CARTESIAN_POINT ( 'NONE',  ( -35.42077910799415008, 325.1303593571471424, -4.549127494966866969 ) ) ;
#103104 = DIRECTION ( 'NONE',  ( -0.8191520442889884679, 1.003171929053520679E-16, 0.5735764363510508224 ) ) ;
#103105 = CARTESIAN_POINT ( 'NONE',  ( 1.860380241283026592, 6.431462466365327479, -0.1499059597315286207 ) ) ;
#103106 = CARTESIAN_POINT ( 'NONE',  ( 17.89629221201704823, 43.18024824084014313, 5.552246930289013171 ) ) ;
#103107 = ORIENTED_EDGE ( 'NONE', *, *, #45550, .F. ) ;
#103108 = COLOUR_RGB ( '', 0.08235294, 0.09019608, 0.10196078) ;
#103109 = CARTESIAN_POINT ( 'NONE',  ( -4.392764327028860549, -48.86087519462214601, 104.3925874334283179 ) ) ;
#103110 = DIRECTION ( 'NONE',  ( -1.000000000000000000, -1.224606353822377258E-16, -0.000000000000000000 ) ) ;
#103111 = CARTESIAN_POINT ( 'NONE',  ( 7.347880794884112834E-16, 69.00000000000000000, 5.999999999999994671 ) ) ;
#103112 = CYLINDRICAL_SURFACE ( 'NONE', #84418, 4.000000000000000000 ) ;
#103113 = EDGE_CURVE ( 'NONE', #104941, #11338, #46816, .T. ) ;
#103114 = CIRCLE ( 'NONE', #4951, 4.000000000000001776 ) ;
#103115 = CARTESIAN_POINT ( 'NONE',  ( -1.320432766682874540E-15, -18.03125000204838457, 7.188101187500000044 ) ) ;
#103116 = UNCERTAINTY_MEASURE_WITH_UNIT (LENGTH_MEASURE( 1.000000000000000082E-05 ), #36334, 'distance_accuracy_value', 'NONE');
#103117 = CARTESIAN_POINT ( 'NONE',  ( 61.11682663846713837, 4.898587196589294500E-16, -4.000000000000007105 ) ) ;
#103118 = CARTESIAN_POINT ( 'NONE',  ( 7.409113134841487507E-15, 50.00000000000000000, -60.50000000000000000 ) ) ;
#103119 = AXIS2_PLACEMENT_3D ( 'NONE', #10802, #68000, #99275 ) ;
#103120 = ORIENTED_EDGE ( 'NONE', *, *, #25695, .T. ) ;
#103121 = CARTESIAN_POINT ( 'NONE',  ( -36.63177234734323662, 490.9974527155399642, 12.47316876380962292 ) ) ;
#103122 = CARTESIAN_POINT ( 'NONE',  ( 7.500000000000000888, -4.651016565836964212, -7.928861822685564498 ) ) ;
#103123 = CARTESIAN_POINT ( 'NONE',  ( -8.755878939558428442, 19.75811540482035866, -4.999999999999364952 ) ) ;
#103124 =( BOUNDED_SURFACE ( )  B_SPLINE_SURFACE ( 3, 2, ( 
 ( #87165, #4116, #38622 ),
 ( #86120, #69912, #4651 ),
 ( #62891, #45642, #28421 ),
 ( #94738, #103343, #13776 ),
 ( #46688, #5695, #61297 ),
 ( #94191, #12191, #29490 ),
 ( #62367, #95257, #21389 ),
 ( #81682, #82772, #65532 ),
 ( #40183, #57950, #105456 ),
 ( #25093, #57414, #6756 ),
 ( #48789, #15911, #33185 ),
 ( #39676, #105969, #72550 ),
 ( #220, #90874, #23504 ),
 ( #7804, #7275, #31596 ),
 ( #40712, #96845, #32113 ),
 ( #56348, #89810, #81164 ),
 ( #74136, #14838, #16988 ),
 ( #73600, #106504, #64481 ),
 ( #24571, #80633, #66056 ),
 ( #72030, #73061, #97350 ),
 ( #98933, #47734, #49866 ),
 ( #8343, #31079, #104937 ),
 ( #63958, #32660, #64995 ),
 ( #82230, #89283, #8875 ),
 ( #90332, #98419, #22973 ),
 ( #55809, #88745, #48264 ),
 ( #97888, #24043, #15377 ),
 ( #56884, #16440, #49323 ),
 ( #41247, #2375, #50917 ),
 ( #43385, #42307, #26706 ),
 ( #58507, #2903, #92445 ),
 ( #35862, #83829, #74662 ),
 ( #18601, #51989, #59579 ),
 ( #41780, #10467, #747 ),
 ( #68185, #75740, #9938 ),
 ( #100542, #50388, #84907 ),
 ( #66589, #83300, #18059 ),
 ( #51461, #100013, #19684 ),
 ( #1291, #42845, #84376 ),
 ( #92990, #101082, #60127 ),
 ( #91412, #99470, #10992 ),
 ( #43909, #76797, #76269 ),
 ( #35321, #52523, #27240 ),
 ( #1836, #27778, #75195 ),
 ( #101622, #19153, #9389 ),
 ( #68738, #60651, #93539 ),
 ( #34257, #34793, #67128 ),
 ( #85439, #33713, #26182 ),
 ( #25644, #67662, #59042 ),
 ( #17525, #91928, #46946 ),
 ( #104120, #30808, #22179 ),
 ( #38363, #4915, #29751 ),
 ( #46432, #6484, #37846 ),
 ( #55554, #63693, #71747 ),
 ( #72806, #105195, #54489 ),
 ( #96582, #22715, #80905 ),
 ( #13512, #63154, #88490 ),
 ( #47474, #104656, #39933 ),
 ( #78782, #14566, #80370 ),
 ( #5953, #56624, #71227 ),
 ( #30265, #39414, #55029 ),
 ( #96051, #70709, #62624 ),
 ( #79321, #72289, #103600 ),
 ( #31342, #64223, #97095 ),
 ( #11522, #14041, #5441 ),
 ( #15111, #95511, #105713 ),
 ( #87961, #23236, #89016 ),
 ( #56073, #79847, #38878 ),
 ( #7016, #47999, #31855 ),
 ( #64735, #97612, #23777 ),
 ( #45905, #21652, #87434 ),
 ( #40987, #40453, #74928 ),
 ( #66322, #1012, #480 ),
 ( #49061, #99753, #81423 ),
 ( #81956, #91675, #82510 ),
 ( #74400, #33449, #49603 ),
 ( #106232, #9134, #99205 ),
 ( #65264, #90604, #8083 ),
 ( #73877, #98153, #42046 ),
 ( #33996, #8612, #41515 ),
 ( #25371, #66866, #58227 ),
 ( #57680, #73334, #7537 ),
 ( #91156, #98673, #17262 ),
 ( #32392, #16714, #106772 ),
 ( #24309, #15639, #50134 ),
 ( #83042, #32921, #57155 ) ),
 .UNSPECIFIED., .F., .F., .F. ) 
 B_SPLINE_SURFACE_WITH_KNOTS ( ( 4, 2, 2, 2, 2, 2, 2, 2, 2, 2, 2, 2, 2, 2, 2, 2, 2, 2, 2, 2, 2, 2, 2, 2, 2, 2, 2, 2, 2, 2, 2, 2, 2, 2, 2, 2, 2, 2, 2, 2, 2, 2, 4 ),
 ( 3, 3 ),
 ( 0.06724859676077497850, 0.08531197731406328644, 0.1033753578673516083, 0.1214387384206399162, 0.1304704286972840632, 0.1349862738356061298, 0.1395021189739282241, 0.1575654995272165459, 0.1665971898038606791, 0.1711130349421827734, 0.1733709575113437928, 0.1756288800805048400, 0.1846605703571490009, 0.1869184929263100203, 0.1891764154954710675, 0.1936922606337931341, 0.1942567412760833889, 0.1945389815972285164, 0.1948212219183736438, 0.1959501832029541812, 0.1982081057721152284, 0.2004660283412762478, 0.2006071485018487977, 0.2007482686624213752, 0.2010305089835665027, 0.2015949896258567575, 0.2027239509104372950, 0.2032884315527275776, 0.2034295517133001274, 0.2035706718738727050, 0.2038529121950178324, 0.2044173928373080873, 0.2049818734795983421, 0.2055463541218885970, 0.2058285944430337244, 0.2061108347641788519, 0.2072397960487593616, 0.2083687573333398713, 0.2086509976544849987, 0.2087921178150575763, 0.2089332379756301261, 0.2094977186179204087, 0.2117556411870814559 ),
 ( 0.000000000000000000, 1.000000000000000000 ),
 .UNSPECIFIED. ) 
 GEOMETRIC_REPRESENTATION_ITEM ( )  RATIONAL_B_SPLINE_SURFACE ( (
 ( 1.000000000000000000, 0.7071068666375163181, 1.000000000000000000),
 ( 1.000000000000000000, 0.7071069333971968796, 1.000000000000000000),
 ( 1.000000000000000000, 0.7071067806372003384, 1.000000000000000000),
 ( 1.000000000000000000, 0.7071067806372003384, 1.000000000000000000),
 ( 1.000000000000000000, 0.7071067802067261265, 1.000000000000000000),
 ( 1.000000000000000000, 0.7071067802067261265, 1.000000000000000000),
 ( 1.000000000000000000, 0.7071051933422836111, 1.000000000000000000),
 ( 1.000000000000000000, 0.7071044938463821872, 1.000000000000000000),
 ( 1.000000000000000000, 0.7071050750596493684, 1.000000000000000000),
 ( 1.000000000000000000, 0.7071061969560579197, 1.000000000000000000),
 ( 1.000000000000000000, 0.7071065824458093729, 1.000000000000000000),
 ( 1.000000000000000000, 0.7071068690440487359, 1.000000000000000000),
 ( 1.000000000000000000, 0.7071066644500461074, 1.000000000000000000),
 ( 1.000000000000000000, 0.7071047487608218551, 1.000000000000000000),
 ( 1.000000000000000000, 0.7071039044805524920, 1.000000000000000000),
 ( 1.000000000000000000, 0.7071067951707197263, 1.000000000000000000),
 ( 1.000000000000000000, 0.7071060022142037216, 1.000000000000000000),
 ( 1.000000000000000000, 0.7071045490108263110, 1.000000000000000000),
 ( 1.000000000000000000, 0.7071047837343714670, 1.000000000000000000),
 ( 1.000000000000000000, 0.7071057220880505589, 1.000000000000000000),
 ( 1.000000000000000000, 0.7071061026645381054, 1.000000000000000000),
 ( 1.000000000000000000, 0.7071066713307564422, 1.000000000000000000),
 ( 1.000000000000000000, 0.7071075855488917483, 1.000000000000000000),
 ( 1.000000000000000000, 0.7071018469519960714, 1.000000000000000000),
 ( 1.000000000000000000, 0.7070769257863378510, 1.000000000000000000),
 ( 1.000000000000000000, 0.7070959128786372672, 1.000000000000000000),
 ( 1.000000000000000000, 0.7071006937020449801, 1.000000000000000000),
 ( 1.000000000000000000, 0.7071069821649591525, 1.000000000000000000),
 ( 1.000000000000000000, 0.7071070273698751851, 1.000000000000000000),
 ( 1.000000000000000000, 0.7071019450278684948, 1.000000000000000000),
 ( 1.000000000000000000, 0.7071033604888681268, 1.000000000000000000),
 ( 1.000000000000000000, 0.7071062872278021105, 1.000000000000000000),
 ( 1.000000000000000000, 0.7071065490437030698, 1.000000000000000000),
 ( 1.000000000000000000, 0.7071067506450113838, 1.000000000000000000),
 ( 1.000000000000000000, 0.7071068759948633264, 1.000000000000000000),
 ( 1.000000000000000000, 0.7071066670383303610, 1.000000000000000000),
 ( 1.000000000000000000, 0.7071057208227836677, 1.000000000000000000),
 ( 1.000000000000000000, 0.7070977502787308966, 1.000000000000000000),
 ( 1.000000000000000000, 0.7070812549423161064, 1.000000000000000000),
 ( 1.000000000000000000, 0.7070331502134156176, 1.000000000000000000),
 ( 1.000000000000000000, 0.7070087972399150544, 1.000000000000000000),
 ( 1.000000000000000000, 0.7070383350363120822, 1.000000000000000000),
 ( 1.000000000000000000, 0.7070972093601404218, 1.000000000000000000),
 ( 1.000000000000000000, 0.7071064900542932685, 1.000000000000000000),
 ( 1.000000000000000000, 0.7071067816304712483, 1.000000000000000000),
 ( 1.000000000000000000, 0.7071067807484303636, 1.000000000000000000),
 ( 1.000000000000000000, 0.7071067188699946549, 1.000000000000000000),
 ( 1.000000000000000000, 0.7071063936914395720, 1.000000000000000000),
 ( 1.000000000000000000, 0.7071059926591559686, 1.000000000000000000),
 ( 1.000000000000000000, 0.7071045708296856969, 1.000000000000000000),
 ( 1.000000000000000000, 0.7071033560782118421, 1.000000000000000000),
 ( 1.000000000000000000, 0.7071008937454664744, 1.000000000000000000),
 ( 1.000000000000000000, 0.7071014222377458580, 1.000000000000000000),
 ( 1.000000000000000000, 0.7071047036589576118, 1.000000000000000000),
 ( 1.000000000000000000, 0.7071060773287295431, 1.000000000000000000),
 ( 1.000000000000000000, 0.7071067222128313290, 1.000000000000000000),
 ( 1.000000000000000000, 0.7071067639124569704, 1.000000000000000000),
 ( 1.000000000000000000, 0.7071068043621556720, 1.000000000000000000),
 ( 1.000000000000000000, 0.7071069265355697242, 1.000000000000000000),
 ( 1.000000000000000000, 0.7071075016079259035, 1.000000000000000000),
 ( 1.000000000000000000, 0.7071081591294727797, 1.000000000000000000),
 ( 1.000000000000000000, 0.7071103244092352691, 1.000000000000000000),
 ( 1.000000000000000000, 0.7071119687239084683, 1.000000000000000000),
 ( 1.000000000000000000, 0.7071137400171658705, 1.000000000000000000),
 ( 1.000000000000000000, 0.7071138641451193418, 1.000000000000000000),
 ( 1.000000000000000000, 0.7071124901834935361, 1.000000000000000000),
 ( 1.000000000000000000, 0.7071110053402942519, 1.000000000000000000),
 ( 1.000000000000000000, 0.7071088051577407718, 1.000000000000000000),
 ( 1.000000000000000000, 0.7071080886590817016, 1.000000000000000000),
 ( 1.000000000000000000, 0.7071070405652588597, 1.000000000000000000),
 ( 1.000000000000000000, 0.7071069706112402820, 1.000000000000000000),
 ( 1.000000000000000000, 0.7071058445581541729, 1.000000000000000000),
 ( 1.000000000000000000, 0.7070928369275982783, 1.000000000000000000),
 ( 1.000000000000000000, 0.7070888553714566038, 1.000000000000000000),
 ( 1.000000000000000000, 0.7070962487307334010, 1.000000000000000000),
 ( 1.000000000000000000, 0.7071039365152042011, 1.000000000000000000),
 ( 1.000000000000000000, 0.7071052774665896878, 1.000000000000000000),
 ( 1.000000000000000000, 0.7071064534178541638, 1.000000000000000000),
 ( 1.000000000000000000, 0.7071067052480206616, 1.000000000000000000),
 ( 1.000000000000000000, 0.7071068279545691393, 1.000000000000000000),
 ( 1.000000000000000000, 0.7071066124722539259, 1.000000000000000000),
 ( 1.000000000000000000, 0.7071040194681652569, 1.000000000000000000),
 ( 1.000000000000000000, 0.7070980359047702724, 1.000000000000000000),
 ( 1.000000000000000000, 0.7070730461235169573, 1.000000000000000000),
 ( 1.000000000000000000, 0.7070935438803431783, 1.000000000000000000),
 ( 1.000000000000000000, 0.7071067811865452413, 1.000000000000000000) ) ) 
 REPRESENTATION_ITEM ( '' )  SURFACE ( )  );
#103125 = ADVANCED_FACE ( 'NONE', ( #48920 ), #96539, .T. ) ;
#103126 = DIRECTION ( 'NONE',  ( 0.000000000000000000, -1.000000000000000000, 0.000000000000000000 ) ) ;
#103127 = ORIENTED_EDGE ( 'NONE', *, *, #97786, .F. ) ;
#103128 = AXIS2_PLACEMENT_3D ( 'NONE', #87451, #63171, #13532 ) ;
#103129 = CARTESIAN_POINT ( 'NONE',  ( 20.00100000000000122, 12.99999999999999289, 0.000000000000000000 ) ) ;
#103130 = CARTESIAN_POINT ( 'NONE',  ( -34.16642289233715246, 463.8422268500497125, 18.98106911353877280 ) ) ;
#103131 = VERTEX_POINT ( 'NONE', #40318 ) ;
#103132 = CARTESIAN_POINT ( 'NONE',  ( -28.34962641295014052, 34.17951769392475825, 8.951028473884061754 ) ) ;
#103133 = CARTESIAN_POINT ( 'NONE',  ( 43.88846153846154152, 4.172000000000003261, 0.000000000000000000 ) ) ;
#103134 = DIRECTION ( 'NONE',  ( 0.000000000000000000, -1.000000000000000000, 0.000000000000000000 ) ) ;
#103135 = DIRECTION ( 'NONE',  ( 0.000000000000000000, 0.000000000000000000, 1.000000000000000000 ) ) ;
#103136 = UNCERTAINTY_MEASURE_WITH_UNIT (LENGTH_MEASURE( 1.000000000000000082E-05 ), #25715, 'distance_accuracy_value', 'NONE');
#103137 = CARTESIAN_POINT ( 'NONE',  ( -94.55424737603695462, -60.00000000000000711, 202.5650574291949511 ) ) ;
#103138 = CARTESIAN_POINT ( 'NONE',  ( 16.75187969033515145, 37.11970326878314808, -21.80698433968624528 ) ) ;
#103139 = DIRECTION ( 'NONE',  ( 0.000000000000000000, 0.000000000000000000, -1.000000000000000000 ) ) ;
#103140 = CARTESIAN_POINT ( 'NONE',  ( -46.00000000000000000, 450.0000000000002274, 13.20242257375370976 ) ) ;
#103141 = CARTESIAN_POINT ( 'NONE',  ( 17.51296689355397262, 34.75029386635176820, -22.05286986923737302 ) ) ;
#103142 = ADVANCED_FACE ( 'NONE', ( #104514 ), #98, .T. ) ;
#103143 = CARTESIAN_POINT ( 'NONE',  ( -83.51272355743553533, -46.53462533077923524, 182.5745365089843801 ) ) ;
#103144 = CARTESIAN_POINT ( 'NONE',  ( 22.68881653401906817, 43.82530270060863131, -79.30803424116763267 ) ) ;
#103145 = ORIENTED_EDGE ( 'NONE', *, *, #91542, .F. ) ;
#103146 = DIRECTION ( 'NONE',  ( -0.000000000000000000, -0.000000000000000000, -1.000000000000000000 ) ) ;
#103147 = EDGE_CURVE ( 'NONE', #42028, #20871, #34584, .T. ) ;
#103148 = CARTESIAN_POINT ( 'NONE',  ( 5.981118819178460555, -68.97183456180059125, 0.5452870891823740074 ) ) ;
#103149 = CARTESIAN_POINT ( 'NONE',  ( -82.43943121196362256, -37.82767094664968255, 14.49479528845560417 ) ) ;
#103150 = DIRECTION ( 'NONE',  ( 0.000000000000000000, -1.000000000000000000, -0.000000000000000000 ) ) ;
#103151 = CARTESIAN_POINT ( 'NONE',  ( -2.880884120806427084, 62.46550056523758343, -5.000000000000000888 ) ) ;
#103152 = CARTESIAN_POINT ( 'NONE',  ( 9.439237903448747247, 141.9224268365072419, -3.070077524146086535E-13 ) ) ;
#103153 = DIRECTION ( 'NONE',  ( 1.871721906610600077E-16, 0.000000000000000000, -1.000000000000000000 ) ) ;
#103154 = CARTESIAN_POINT ( 'NONE',  ( -19.32152200348980742, 18.64316884709133504, -33.52312678235660570 ) ) ;
#103155 = CIRCLE ( 'NONE', #85930, 5.000000000000010658 ) ;
#103156 = CARTESIAN_POINT ( 'NONE',  ( 78.42622819757743002, -14.21045842199428932, 178.5071270543957951 ) ) ;
#103157 = LINE ( 'NONE', #29302, #103092 ) ;
#103158 = CARTESIAN_POINT ( 'NONE',  ( -95.73631051900581213, -30.00000000000000000, 71.50198832723137343 ) ) ;
#103159 = CARTESIAN_POINT ( 'NONE',  ( -66.70770666932376969, -29.05727726843131720, 85.70037747262490768 ) ) ;
#103160 = EDGE_LOOP ( 'NONE', ( #27447, #11641, #83420, #52272 ) ) ;
#103161 = CARTESIAN_POINT ( 'NONE',  ( 112.2652136917531465, -60.00000000000000000, 191.8488956690686962 ) ) ;
#103162 = CARTESIAN_POINT ( 'NONE',  ( -64.56209935475503414, 39.42554120405374363, -8.095817184380026177 ) ) ;
#103163 = CARTESIAN_POINT ( 'NONE',  ( 52.35809470648487007, -60.00000000002930278, 84.81990995266937716 ) ) ;
#103164 = ADVANCED_FACE ( 'NONE', ( #96447 ), #31720, .F. ) ;
#103165 = AXIS2_PLACEMENT_3D ( 'NONE', #95417, #71136, #20533 ) ;
#103166 = ORIENTED_EDGE ( 'NONE', *, *, #94481, .F. ) ;
#103167 = DIRECTION ( 'NONE',  ( 0.000000000000000000, -1.000000000000000000, 0.000000000000000000 ) ) ;
#103168 = CARTESIAN_POINT ( 'NONE',  ( 5.082755093536324154, -19.71875000204838457, 5.082755093536326818 ) ) ;
#103169 = VERTEX_POINT ( 'NONE', #14965 ) ;
#103170 = CARTESIAN_POINT ( 'NONE',  ( -11.53815258514799602, 45.46891437459017027, 14.20004885619764146 ) ) ;
#103171 = ORIENTED_EDGE ( 'NONE', *, *, #86113, .T. ) ;
#103172 = CARTESIAN_POINT ( 'NONE',  ( 6.499999999999999112, 3.752776749732559036, -8.000000000000000000 ) ) ;
#103173 = CARTESIAN_POINT ( 'NONE',  ( 7.500000000000007105, -3.000000000000000000, -68.91429205785459544 ) ) ;
#103174 = CARTESIAN_POINT ( 'NONE',  ( -90.16357200789421711, -59.99999999999997868, -18.56049759532515253 ) ) ;
#103175 = CARTESIAN_POINT ( 'NONE',  ( 33.58349330513380693, 1.593028355512270962E-15, 0.000000000000000000 ) ) ;
#103176 = CARTESIAN_POINT ( 'NONE',  ( -5.082755093536325042, -32.46875000204838813, -5.082755093536325930 ) ) ;
#103177 = CARTESIAN_POINT ( 'NONE',  ( 31.14131030317610538, 1.482358050883964840E-15, 0.000000000000000000 ) ) ;
#103178 = CARTESIAN_POINT ( 'NONE',  ( 0.000000000000000000, 0.000000000000000000, -2.868028571428571372 ) ) ;
#103179 = CARTESIAN_POINT ( 'NONE',  ( 1.000000000000000000, -48.52751354259076777, 2.643394033303763546 ) ) ;
#103180 = CARTESIAN_POINT ( 'NONE',  ( 42.98746414932995208, 5.000000000000002665, 0.000000000000000000 ) ) ;
#103181 = CARTESIAN_POINT ( 'NONE',  ( -46.00000000000000711, 437.8930939855516158, 12.65921861419373151 ) ) ;
#103182 = PRESENTATION_STYLE_ASSIGNMENT (( #94577 ) ) ;
#103183 = CARTESIAN_POINT ( 'NONE',  ( 37.71162862628988677, 389.8339943296927004, 6.083486274822005768 ) ) ;
#103184 = AXIS2_PLACEMENT_3D ( 'NONE', #943, #25854, #59779 ) ;
#103185 = ORIENTED_EDGE ( 'NONE', *, *, #87288, .F. ) ;
#103186 = DIRECTION ( 'NONE',  ( -1.000000000000000000, -0.000000000000000000, -0.000000000000000000 ) ) ;
#103187 = CARTESIAN_POINT ( 'NONE',  ( 4.551587301587300516, -1.200583151104944069, 104.4018401814738013 ) ) ;
#103188 = CARTESIAN_POINT ( 'NONE',  ( 33.54291075367279973, -46.42946800168273569, 35.89603996142585629 ) ) ;
#103189 = CARTESIAN_POINT ( 'NONE',  ( -22.03900363279597840, -4.285714285713229543, -12.70248734010661451 ) ) ;
#103190 = ORIENTED_EDGE ( 'NONE', *, *, #9058, .F. ) ;
#103191 = CARTESIAN_POINT ( 'NONE',  ( -7.996668423981794227, 47.99999999999998579, -91.14546719974913458 ) ) ;
#103192 = VECTOR ( 'NONE', #1061, 1000.000000000000000 ) ;
#103194 = FACE_OUTER_BOUND ( 'NONE', #4712, .T. ) ;
#103193 = CARTESIAN_POINT ( 'NONE',  ( 6.315295643000387038, -5.000000000000000000, -15.34937609225130117 ) ) ;
#103195 = DIRECTION ( 'NONE',  ( -1.000000000000000000, -0.000000000000000000, -0.000000000000000000 ) ) ;
#103196 = DIRECTION ( 'NONE',  ( 1.000000000000000000, 0.000000000000000000, 0.000000000000000000 ) ) ;
#103197 = DIRECTION ( 'NONE',  ( 0.000000000000000000, -1.000000000000000000, 0.000000000000000000 ) ) ;
#103198 = CARTESIAN_POINT ( 'NONE',  ( -40.95645226494054469, 436.0015890305718358, 6.362679593778101328 ) ) ;
#103199 = CARTESIAN_POINT ( 'NONE',  ( -49.07537269082070708, 14.00518788141075710, -14.91829442325389721 ) ) ;
#103201 = VERTEX_POINT ( 'NONE', #48399 ) ;
#103200 =( GEOMETRIC_REPRESENTATION_CONTEXT ( 3 ) GLOBAL_UNCERTAINTY_ASSIGNED_CONTEXT ( ( #100117 ) ) GLOBAL_UNIT_ASSIGNED_CONTEXT ( ( #49829, #56306, #89245 ) ) REPRESENTATION_CONTEXT ( 'NONE', 'WORKASPACE' ) );
#103202 = CARTESIAN_POINT ( 'NONE',  ( 92.01104092861777417, -60.00000000000000000, 18.65600228545548589 ) ) ;
#103203 = DIRECTION ( 'NONE',  ( -1.000000000000000000, -0.000000000000000000, -0.000000000000000000 ) ) ;
#103204 = CARTESIAN_POINT ( 'NONE',  ( -6.208652854214004257, 40.93126280863162236, -71.11611043310642799 ) ) ;
#103205 = DIRECTION ( 'NONE',  ( 1.000000000000000000, 0.000000000000000000, 0.000000000000000000 ) ) ;
#103206 = VERTEX_POINT ( 'NONE', #22583 ) ;
#103207 = ADVANCED_FACE ( 'NONE', ( #47861 ), #73193, .T. ) ;
#103208 = CARTESIAN_POINT ( 'NONE',  ( -104.4911618787428438, -30.00000000000223466, 196.0249069884481514 ) ) ;
#103209 = ORIENTED_EDGE ( 'NONE', *, *, #87990, .T. ) ;
#103210 = AXIS2_PLACEMENT_3D ( 'NONE', #51485, #83855, #91951 ) ;
#103211 = DIRECTION ( 'NONE',  ( 0.5735764363510442720, -0.8191520442889930198, 1.003171929053526349E-16 ) ) ;
#103212 = DIRECTION ( 'NONE',  ( -1.000000000000000000, -1.224606353822377258E-16, -0.000000000000000000 ) ) ;
#103213 = CARTESIAN_POINT ( 'NONE',  ( 14.45712292643875863, 21.77297462401915951, 4.836555868072715647 ) ) ;
#103214 = CARTESIAN_POINT ( 'NONE',  ( 82.06366534565165693, -37.81903932946467961, -13.65071145180755430 ) ) ;
#103215 = CARTESIAN_POINT ( 'NONE',  ( -7.188101187500001821, -33.87500000204838813, -2.977408999572651371 ) ) ;
#103217 = EDGE_CURVE ( 'NONE', #40330, #3694, #64605, .T. ) ;
#103216 = CARTESIAN_POINT ( 'NONE',  ( -14.29190075645216851, 7.765108448534488339, -6.049455384114764911 ) ) ;
#103218 = SURFACE_SIDE_STYLE ('',( #70322 ) ) ;
#103219 = CLOSED_SHELL ( 'NONE', ( #55172, #23880, #67258, #56944, #60242, #64397, #86861, #66714, #70552, #3575, #54542 ) ) ;
#103220 = CARTESIAN_POINT ( 'NONE',  ( 0.000000000000000000, 0.000000000000000000, -7.131971428571428184 ) ) ;
#103221 = VERTEX_POINT ( 'NONE', #106096 ) ;
#103222 = CONICAL_SURFACE ( 'NONE', #39471, 16.09658290236430389, 0.7509290623979402168 ) ;
#103224 = ORIENTED_EDGE ( 'NONE', *, *, #46459, .F. ) ;
#103223 = PRESENTATION_STYLE_ASSIGNMENT (( #103744 ) ) ;
#103225 = CARTESIAN_POINT ( 'NONE',  ( 77.23229261623454533, -53.37152101417233041, 143.0171963300477103 ) ) ;
#103226 = STYLED_ITEM ( 'NONE', ( #71272 ), #69099 ) ;
#103227 = FILL_AREA_STYLE_COLOUR ( '', #67726 ) ;
#103228 = ORIENTED_EDGE ( 'NONE', *, *, #75635, .T. ) ;
#103229 = CARTESIAN_POINT ( 'NONE',  ( -12.50000000000000533, 34.74998583579827738, -53.99885635920711024 ) ) ;
#103230 = CARTESIAN_POINT ( 'NONE',  ( 7.188101187500000044, -16.15625000204838457, 0.000000000000000000 ) ) ;
#103231 = CARTESIAN_POINT ( 'NONE',  ( -100.8911947370258844, -57.62911827813870502, 203.6698938757279223 ) ) ;
#103232 = EDGE_CURVE ( 'NONE', #78825, #56180, #60445, .T. ) ;
#103233 = EDGE_LOOP ( 'NONE', ( #66584, #40735, #52222, #57797 ) ) ;
#103234 = SURFACE_STYLE_USAGE ( .BOTH. , #77363 ) ;
#103235 = CARTESIAN_POINT ( 'NONE',  ( 4.258869285391245540, 11.59559883260999413, 5.000000000000000000 ) ) ;
#103236 = CIRCLE ( 'NONE', #77366, 0.9999999999999947820 ) ;
#103237 = CARTESIAN_POINT ( 'NONE',  ( 7.268969833840798422, 41.22981915269870967, -58.87267939806292816 ) ) ;
#103238 = DIRECTION ( 'NONE',  ( -1.000000000000000000, -1.224606353822377258E-16, -0.000000000000000000 ) ) ;
#103239 = EDGE_CURVE ( 'NONE', #57394, #45889, #87823, .T. ) ;
#103240 = CARTESIAN_POINT ( 'NONE',  ( -3.313708498984760720, -15.21875000409677270, -8.000000000000000000 ) ) ;
#103241 = CARTESIAN_POINT ( 'NONE',  ( -51.87932953685692894, -29.94853046243735406, 49.87283498340130450 ) ) ;
#103242 = VECTOR ( 'NONE', #97876, 1000.000000000000000 ) ;
#103243 = DIRECTION ( 'NONE',  ( 0.000000000000000000, 1.000000000000000000, 0.000000000000000000 ) ) ;
#103244 = CARTESIAN_POINT ( 'NONE',  ( 7.500000000000001776, 1.559114133231479071, -21.99325844590496004 ) ) ;
#103245 = CARTESIAN_POINT ( 'NONE',  ( 4.958618710454560485, 52.14943927389753497, 6.064328585294240348 ) ) ;
#103246 = SHAPE_DEFINITION_REPRESENTATION ( #47325, #103287 ) ;
#103247 = CARTESIAN_POINT ( 'NONE',  ( -11.20109389684249734, -9.957101141484953288, 18.59593266893761765 ) ) ;
#103248 = ORIENTED_EDGE ( 'NONE', *, *, #65048, .T. ) ;
#103249 = CARTESIAN_POINT ( 'NONE',  ( -1.533598151288847911, -49.97300464335175718, 44.88852685968546297 ) ) ;
#103250 = DIRECTION ( 'NONE',  ( -0.5735764363510461594, 0.8191520442889916875, 1.003171929053524870E-16 ) ) ;
#103251 = CARTESIAN_POINT ( 'NONE',  ( -2.024833989188797645, 14.39326063602704942, -6.704610268883726576 ) ) ;
#103252 = CARTESIAN_POINT ( 'NONE',  ( -13.71949818509876629, -19.30456015386723223, -37.82957963845891669 ) ) ;
#103253 = CARTESIAN_POINT ( 'NONE',  ( -82.83350497009941193, -30.00000000000000355, 151.6907841967885417 ) ) ;
#103254 = EDGE_CURVE ( 'NONE', #86482, #31074, #56487, .T. ) ;
#103255 = CARTESIAN_POINT ( 'NONE',  ( 7.500000000000008882, 42.00000000000000711, -71.41947339647146009 ) ) ;
#103256 = VERTEX_POINT ( 'NONE', #105064 ) ;
#103257 = FACE_BOUND ( 'NONE', #57696, .T. ) ;
#103258 = CARTESIAN_POINT ( 'NONE',  ( 83.70865895686264935, -57.54354250294924356, 201.5867987658908760 ) ) ;
#103259 = CARTESIAN_POINT ( 'NONE',  ( 73.58146070047708065, -60.22809872142786958, -24.87506665778998638 ) ) ;
#103260 = CIRCLE ( 'NONE', #98082, 1.000000000000000666 ) ;
#103261 = CARTESIAN_POINT ( 'NONE',  ( 72.37206225042174879, -1.232595164407830946E-29, 4.000000000000007105 ) ) ;
#103262 = DIRECTION ( 'NONE',  ( -1.000000000000000000, -1.224606353822377258E-16, -0.000000000000000000 ) ) ;
#103263 = CARTESIAN_POINT ( 'NONE',  ( 9.999999999999996447, -3.000000000000003109, -86.30899693899574743 ) ) ;
#103264 = CARTESIAN_POINT ( 'NONE',  ( -62.19705368951759539, -60.00000000000000000, 107.9267807310001643 ) ) ;
#103265 = FILL_AREA_STYLE ('',( #54686 ) ) ;
#103266 = CARTESIAN_POINT ( 'NONE',  ( 27.10511071441177222, 36.88665068479793518, -7.556984339679249985 ) ) ;
#103267 = CIRCLE ( 'NONE', #89484, 5.000000000000002665 ) ;
#103268 = CARTESIAN_POINT ( 'NONE',  ( -58.90678327790940472, 50.00000000004006750, -28.11551192219710771 ) ) ;
#103269 = CARTESIAN_POINT ( 'NONE',  ( -86.23216682740927297, -24.68519757505537626, 181.5290854991648359 ) ) ;
#103270 = EDGE_LOOP ( 'NONE', ( #20751, #84604, #14067, #101949, #53490 ) ) ;
#103271 = CARTESIAN_POINT ( 'NONE',  ( 35.68024356520923135, 373.5070696322856065, 4.158998345878070602 ) ) ;
#103272 = CARTESIAN_POINT ( 'NONE',  ( -12.50000000000000355, 41.59226156894883530, -76.70843802411151557 ) ) ;
#103273 = CARTESIAN_POINT ( 'NONE',  ( -6.494545593174295028, 41.94144595442993761, -59.61320170350516889 ) ) ;
#103274 = CARTESIAN_POINT ( 'NONE',  ( 37.00811329507128988, 491.8246567885115610, 12.57632236122393010 ) ) ;
#103275 =( NAMED_UNIT ( * ) SI_UNIT ( $, .STERADIAN. ) SOLID_ANGLE_UNIT ( ) );
#103276 = EDGE_CURVE ( 'NONE', #6482, #4006, #13900, .T. ) ;
#103277 = CARTESIAN_POINT ( 'NONE',  ( -26.15559236925495412, 305.6589228050500537, -9.603828203464059854 ) ) ;
#103278 = CARTESIAN_POINT ( 'NONE',  ( 0.000000000000000000, 0.000000000000000000, -4.567799999999999194 ) ) ;
#103280 = B_SPLINE_CURVE_WITH_KNOTS ( 'NONE', 3,
 ( #28297, #2377, #12591, #20222, #19687, #12066, #28844, #52525, #86529, #68186, #19155, #101084, #27242, #85993, #44995, #60129, #20760, #101625, #18603, #77881, #76799, #92993, #51992, #53596, #45525, #4514, #35864, #51463, #68740, #100544, #10469, #27780, #60653, #70847, #55169, #72429, #22323 ),
 .UNSPECIFIED., .F., .F.,
 ( 4, 1, 1, 1, 1, 1, 2, 2, 1, 1, 1, 2, 2, 2, 1, 1, 1, 2, 2, 1, 1, 1, 1, 2, 2, 4 ),
 ( 0.000000000000000000, 0.1249999999995662636, 0.1874999999993494093, 0.2187499999992321420, 0.2343749999991734945, 0.2421874999991536770, 0.2460937499991533439, 0.2499999999991530664, 0.3124999999992191246, 0.3437499999992522093, 0.3593749999992681965, 0.3671874999992762456, 0.3749999999992841837, 0.4999999999994025890, 0.5624999999994684252, 0.5937499999995051736, 0.6093749999995236033, 0.6171874999995341504, 0.6249999999995448086, 0.6874999999996103117, 0.7187499999996449507, 0.7343749999996623812, 0.7421874999996695976, 0.7460937499996715960, 0.7499999999996734834, 1.000000000000000000 ),
 .UNSPECIFIED. ) ;
#103279 = TOROIDAL_SURFACE ( 'NONE', #41213, 11.00000000000000000, 2.000000000000000000 ) ;
#103281 = DIRECTION ( 'NONE',  ( -1.000000000000000000, -0.000000000000000000, -0.000000000000000000 ) ) ;
#103282 = DIRECTION ( 'NONE',  ( -1.000000000000000000, -1.224606353822377258E-16, -0.000000000000000000 ) ) ;
#103283 = ORIENTED_EDGE ( 'NONE', *, *, #11649, .F. ) ;
#103284 = ADVANCED_FACE ( 'NONE', ( #64088 ), #36301, .T. ) ;
#103285 = FILL_AREA_STYLE ('',( #39621 ) ) ;
#103286 = CARTESIAN_POINT ( 'NONE',  ( 10.07982286427262686, 15.04985694343187141, 10.37301160543360545 ) ) ;
#103287 = SHAPE_REPRESENTATION ( 'plain washer hardened small grade a_din_Washer DIN 433 - 17 - 300HV', ( #10728 ), #35180 ) ;
#103288 = ADVANCED_FACE ( 'NONE', ( #13902 ), #79713, .F. ) ;
#103289 = CARTESIAN_POINT ( 'NONE',  ( 15.50035291838412199, -4.285714285712356464, 20.16952962162429941 ) ) ;
#103290 = DIRECTION ( 'NONE',  ( -0.9915366780650392009, -0.1269898409407490270, -0.02699252395738697963 ) ) ;
#103291 = AXIS2_PLACEMENT_3D ( 'NONE', #38074, #4610, #103308 ) ;
#103292 = CARTESIAN_POINT ( 'NONE',  ( 105.2982900294548614, -30.00000000000001066, 128.8790101386541096 ) ) ;
#103293 = CARTESIAN_POINT ( 'NONE',  ( -81.81404306141678262, -25.62499348290805301, 141.9831859399797054 ) ) ;
#103294 = ORIENTED_EDGE ( 'NONE', *, *, #5611, .F. ) ;
#103295 =( LENGTH_UNIT ( ) NAMED_UNIT ( * ) SI_UNIT ( .MILLI., .METRE. ) );
#103296 = DIRECTION ( 'NONE',  ( 0.000000000000000000, 1.000000000000000000, 0.000000000000000000 ) ) ;
#103297 = CARTESIAN_POINT ( 'NONE',  ( 98.32443960344940592, -57.62441092855549840, 204.2909859055558286 ) ) ;
#103298 = FACE_OUTER_BOUND ( 'NONE', #83850, .T. ) ;
#103299 = CARTESIAN_POINT ( 'NONE',  ( 36.79086635616850742, 340.8131496176287101, -0.8880945147259954320 ) ) ;
#103300 = AXIS2_PLACEMENT_3D ( 'NONE', #12852, #95382, #63562 ) ;
#103301 = CARTESIAN_POINT ( 'NONE',  ( 44.14911905790289381, 464.3766534542007207, 9.623404994951323843 ) ) ;
#103302 = VERTEX_POINT ( 'NONE', #63554 ) ;
#103303 = CARTESIAN_POINT ( 'NONE',  ( 0.000000000000000000, 304.8518027762758038, 9.936999415352289589 ) ) ;
#103304 = ADVANCED_FACE ( 'NONE', ( #23100 ), #72433, .T. ) ;
#103305 = CARTESIAN_POINT ( 'NONE',  ( -16.18712010533815615, 37.20509496956294981, 21.93868532144427164 ) ) ;
#103306 = CARTESIAN_POINT ( 'NONE',  ( 2.977408999572651815, -25.43750000204838813, 7.188101187500000933 ) ) ;
#103307 = ORIENTED_EDGE ( 'NONE', *, *, #1969, .T. ) ;
#103308 = DIRECTION ( 'NONE',  ( 0.000000000000000000, 0.000000000000000000, -1.000000000000000000 ) ) ;
#103309 = DIRECTION ( 'NONE',  ( 8.034710196240791752E-11, 0.000000000000000000, -1.000000000000000000 ) ) ;
#103310 = DIRECTION ( 'NONE',  ( 0.000000000000000000, -1.000000000000000000, 2.311253228826402606E-16 ) ) ;
#103311 = DIRECTION ( 'NONE',  ( -1.000000000000000000, -1.224606353822377258E-16, -0.000000000000000000 ) ) ;
#103312 = CARTESIAN_POINT ( 'NONE',  ( 7.000000000000000000, -14.05766640829038039, -5.232782735144291486 ) ) ;
#103313 = CARTESIAN_POINT ( 'NONE',  ( -34.64581139903613405, 463.6418748650343105, 19.44242283797569470 ) ) ;
#103314 = VERTEX_POINT ( 'NONE', #47338 ) ;
#103315 = CARTESIAN_POINT ( 'NONE',  ( 30.52000010178268496, -60.00000000000000000, -40.85847840406977127 ) ) ;
#103317 = CARTESIAN_POINT ( 'NONE',  ( 26.43631887545773651, -32.52417025399565631, 30.87970515157304519 ) ) ;
#103316 = CARTESIAN_POINT ( 'NONE',  ( -39.49898250731507687, -29.99999999999994316, 47.07929020003657428 ) ) ;
#103318 = AXIS2_PLACEMENT_3D ( 'NONE', #29522, #86680, #77507 ) ;
#103319 = CARTESIAN_POINT ( 'NONE',  ( 119.0671996398096724, 7.666536031838888654, 59.53359981990487171 ) ) ;
#103320 = EDGE_LOOP ( 'NONE', ( #30421, #68950, #34080, #48395, #83918 ) ) ;
#103321 = UNCERTAINTY_MEASURE_WITH_UNIT (LENGTH_MEASURE( 1.000000000000000082E-05 ), #47253, 'distance_accuracy_value', 'NONE');
#103322 = ORIENTED_EDGE ( 'NONE', *, *, #38723, .F. ) ;
#103323 = CARTESIAN_POINT ( 'NONE',  ( -6.851679529983103610E-15, 22.97884757028485225, 55.94820918777160301 ) ) ;
#103324 = CARTESIAN_POINT ( 'NONE',  ( 0.000000000000000000, 1.500000000000000000, 0.000000000000000000 ) ) ;
#103325 = FACE_OUTER_BOUND ( 'NONE', #73252, .T. ) ;
#103326 =( NAMED_UNIT ( * ) PLANE_ANGLE_UNIT ( ) SI_UNIT ( $, .RADIAN. ) );
#103327 = CARTESIAN_POINT ( 'NONE',  ( -15.68120647348154151, 6.021684053266456615, 7.051923121157602559 ) ) ;
#103328 = EDGE_LOOP ( 'NONE', ( #93355, #101140, #50488, #106051 ) ) ;
#103329 = FILL_AREA_STYLE_COLOUR ( '', #60024 ) ;
#103330 = CARTESIAN_POINT ( 'NONE',  ( 97.48148763265582772, -29.99999999999981171, 190.8966502933984657 ) ) ;
#103331 = CARTESIAN_POINT ( 'NONE',  ( -13.71253760832901492, 3.086396204329165727, 6.035735341873747828 ) ) ;
#103332 = DIRECTION ( 'NONE',  ( 0.000000000000000000, 1.000000000000000000, -0.000000000000000000 ) ) ;
#103333 = CARTESIAN_POINT ( 'NONE',  ( 81.12250922778763140, -30.00000000000000355, 2.073590792126307480 ) ) ;
#103334 = DIRECTION ( 'NONE',  ( -0.8191520442889881348, 1.003171929053520186E-16, 0.5735764363510513775 ) ) ;
#103335 = ORIENTED_EDGE ( 'NONE', *, *, #31292, .F. ) ;
#103336 = EDGE_CURVE ( 'NONE', #9383, #82359, #44892, .T. ) ;
#103337 = COLOUR_RGB ( '', 0.66274510, 0.83137255, 0.94901961) ;
#103338 = ORIENTED_EDGE ( 'NONE', *, *, #40959, .T. ) ;
#103339 = ORIENTED_EDGE ( 'NONE', *, *, #1960, .T. ) ;
#103340 = LINE ( 'NONE', #104381, #100292 ) ;
#103341 = FILL_AREA_STYLE_COLOUR ( '', #18343 ) ;
#103342 = CARTESIAN_POINT ( 'NONE',  ( 10.38582326156068625, 145.0440906288519614, 0.000000000000000000 ) ) ;
#103343 = CARTESIAN_POINT ( 'NONE',  ( -45.47728949670318599, 415.0252377317643209, 8.193707597952228028 ) ) ;
#103344 = CARTESIAN_POINT ( 'NONE',  ( 89.64643850830432825, 1.030564683017419500E-14, 0.000000000000000000 ) ) ;
#103345 = CARTESIAN_POINT ( 'NONE',  ( -7.744991119775235688, -88.46438785425127094, -2.016316005557098112 ) ) ;
#103347 = EDGE_CURVE ( 'NONE', #29313, #35464, #62228, .T. ) ;
#103346 = DIRECTION ( 'NONE',  ( 0.000000000000000000, 0.000000000000000000, 1.000000000000000000 ) ) ;
#103349 = ORIENTED_EDGE ( 'NONE', *, *, #100457, .T. ) ;
#103348 = PRESENTATION_LAYER_ASSIGNMENT (  '', '', ( #24143 ) ) ;
#103350 = CARTESIAN_POINT ( 'NONE',  ( 30.04499556692307394, 7.904673525308155924, 42.05327650403261686 ) ) ;
#103351 = EDGE_LOOP ( 'NONE', ( #73584, #7131, #98618, #97175, #11134 ) ) ;
#103352 = CARTESIAN_POINT ( 'NONE',  ( -6.000208918519489565, -60.99968662210032022, -0.2646532170642326709 ) ) ;
#103353 = CARTESIAN_POINT ( 'NONE',  ( -4.582575694955839829, 15.00000000000000000, 10.00000000000000000 ) ) ;
#103354 = LINE ( 'NONE', #70457, #31980 ) ;
#103355 = CARTESIAN_POINT ( 'NONE',  ( 23.45015351654351932, 303.6741448883345242, 10.11546188763766452 ) ) ;
#103356 = AXIS2_PLACEMENT_3D ( 'NONE', #96550, #40960, #73849 ) ;
#103357 = CARTESIAN_POINT ( 'NONE',  ( -83.59931608698744299, -60.00000000000002132, 191.2519107553881383 ) ) ;
#103358 = CARTESIAN_POINT ( 'NONE',  ( 63.26434788449935809, -56.86244944842989213, 90.13329942383785465 ) ) ;
#103359 = ORIENTED_EDGE ( 'NONE', *, *, #14677, .T. ) ;
#103360 = CARTESIAN_POINT ( 'NONE',  ( 28.94979900162220687, 13.71034195483037443, -39.84012157007438049 ) ) ;
#103361 = DIRECTION ( 'NONE',  ( -1.000000000000000000, -1.224606353822377258E-16, -0.000000000000000000 ) ) ;
#103362 = DIRECTION ( 'NONE',  ( 0.000000000000000000, 0.000000000000000000, -1.000000000000000000 ) ) ;
#103363 = CIRCLE ( 'NONE', #77494, 3.309499999999999886 ) ;
#103364 = CARTESIAN_POINT ( 'NONE',  ( 28.58349330513380337, 4.898587196589411843E-16, -4.000000000000001776 ) ) ;
#103365 = EDGE_CURVE ( 'NONE', #39236, #63624, #38138, .T. ) ;
#103366 = ORIENTED_EDGE ( 'NONE', *, *, #82408, .F. ) ;
#103367 = AXIS2_PLACEMENT_3D ( 'NONE', #65955, #100446, #90770 ) ;
#103368 =( LENGTH_UNIT ( ) NAMED_UNIT ( * ) SI_UNIT ( .MILLI., .METRE. ) );
#103369 = SURFACE_STYLE_FILL_AREA ( #69416 ) ;
#103370 = DIRECTION ( 'NONE',  ( -1.000000000000000000, -0.000000000000000000, -0.000000000000000000 ) ) ;
#103371 = DIRECTION ( 'NONE',  ( -0.000000000000000000, -1.000000000000000000, -0.000000000000000000 ) ) ;
#103372 = CARTESIAN_POINT ( 'NONE',  ( 1.227754105814700766E-15, 67.05096163904791240, 10.02537308446411402 ) ) ;
#103373 = DIRECTION ( 'NONE',  ( 0.000000000000000000, -1.000000000000000000, 0.000000000000000000 ) ) ;
#103374 = CARTESIAN_POINT ( 'NONE',  ( 86.68178608655959749, -24.39358399406027900, 184.9913743671155260 ) ) ;
#103375 = DIRECTION ( 'NONE',  ( 0.000000000000000000, -1.000000000000000000, 0.000000000000000000 ) ) ;
#103376 = CARTESIAN_POINT ( 'NONE',  ( -9.993721417788709260, 7.509139500089329289, 5.000000000000019540 ) ) ;
#103377 = CARTESIAN_POINT ( 'NONE',  ( 7.618844049274133390, -6.827641010705410629, 2.450177051822844732 ) ) ;
#103378 = CARTESIAN_POINT ( 'NONE',  ( 15.11650669486618881, -3.999999999999998224, 0.000000000000000000 ) ) ;
#103379 = CARTESIAN_POINT ( 'NONE',  ( 13.99656100229485389, -50.02536491266853602, 26.59581618167199579 ) ) ;
#103380 = CARTESIAN_POINT ( 'NONE',  ( 0.000000000000000000, -80.00000000000000000, 27.00000000000000000 ) ) ;
#103381 = CARTESIAN_POINT ( 'NONE',  ( -100.7873380846828724, -30.00000000000000355, 180.4097680941990234 ) ) ;
#103382 = CARTESIAN_POINT ( 'NONE',  ( 29.83349330513380337, -4.000000000000000888, 4.898587196589416773E-16 ) ) ;
#103383 = CARTESIAN_POINT ( 'NONE',  ( 25.95016476712096321, -57.67607197499474836, 43.50018178531507829 ) ) ;
#103384 = CIRCLE ( 'NONE', #17245, 0.4000000000000001887 ) ;
#103385 = DIRECTION ( 'NONE',  ( 0.000000000000000000, -1.000000000000000000, 0.000000000000000000 ) ) ;
#103386 = CARTESIAN_POINT ( 'NONE',  ( -22.54429944894614835, 43.83586929555325895, -79.50671238563580800 ) ) ;
#103387 = CARTESIAN_POINT ( 'NONE',  ( -18.55157383485121514, 50.00000000000000000, 61.19039212642342562 ) ) ;
#103388 = FACE_OUTER_BOUND ( 'NONE', #48982, .T. ) ;
#103389 = CARTESIAN_POINT ( 'NONE',  ( -46.00000000000000000, 461.6622277975411635, 10.18145404766348783 ) ) ;
#103390 = DIRECTION ( 'NONE',  ( 0.000000000000000000, -1.000000000000000000, 0.000000000000000000 ) ) ;
#103391 = DIRECTION ( 'NONE',  ( 0.000000000000000000, -0.000000000000000000, 1.000000000000000000 ) ) ;
#103392 = CARTESIAN_POINT ( 'NONE',  ( -87.29218671470692925, -28.00333867647982800, 187.7165209339487717 ) ) ;
#103393 = ORIENTED_EDGE ( 'NONE', *, *, #41266, .F. ) ;
#103394 = CARTESIAN_POINT ( 'NONE',  ( 41.29724588151264442, 485.7091420655442562, -4.558554568103089899 ) ) ;
#103395 = CARTESIAN_POINT ( 'NONE',  ( -14.23481919006072616, -18.58702783338264908, 27.09272798716932940 ) ) ;
#103397 = CARTESIAN_POINT ( 'NONE',  ( -42.51570042820637951, 437.0229838707177237, 20.73732745754740847 ) ) ;
#103396 = CARTESIAN_POINT ( 'NONE',  ( -86.89501302346295120, -60.00000000000000711, -9.734508581877785005 ) ) ;
#103398 = EDGE_CURVE ( 'NONE', #86608, #102376, #43520, .T. ) ;
#103399 = ORIENTED_EDGE ( 'NONE', *, *, #8767, .T. ) ;
#103400 = AXIS2_PLACEMENT_3D ( 'NONE', #76361, #93094, #26279 ) ;
#103401 = CARTESIAN_POINT ( 'NONE',  ( 42.98746414932995208, 1.482358050883964840E-15, 0.000000000000000000 ) ) ;
#103402 = TOROIDAL_SURFACE ( 'NONE', #91332, 8.500000000000000000, 0.5000000000000000000 ) ;
#103403 = EDGE_CURVE ( 'NONE', #54829, #85509, #43258, .T. ) ;
#103404 = CARTESIAN_POINT ( 'NONE',  ( 15.94096206886545097, 3.082184004823646184, 0.3571785271892598534 ) ) ;
#103405 = CARTESIAN_POINT ( 'NONE',  ( 72.37206225042174879, 6.856755485862130937E-15, 0.000000000000000000 ) ) ;
#103406 = ORIENTED_EDGE ( 'NONE', *, *, #28115, .T. ) ;
#103407 = DIRECTION ( 'NONE',  ( -1.000000000000000000, -0.000000000000000000, -0.000000000000000000 ) ) ;
#103408 = CARTESIAN_POINT ( 'NONE',  ( -37.56673239365849781, -1.200000000000000030E-05, 13.45617127781066280 ) ) ;
#103409 = EDGE_CURVE ( 'NONE', #32377, #75403, #67360, .T. ) ;
#103411 = LINE ( 'NONE', #37659, #99450 ) ;
#103410 = DIRECTION ( 'NONE',  ( 0.000000000000000000, 1.000000000000000000, 0.000000000000000000 ) ) ;
#103412 = CARTESIAN_POINT ( 'NONE',  ( -4.472135954999581386, -10.00000000000000888, -4.000000000000000000 ) ) ;
#103413 = ORIENTED_EDGE ( 'NONE', *, *, #33, .F. ) ;
#103415 = EDGE_CURVE ( 'NONE', #98286, #2681, #5373, .T. ) ;
#103414 = AXIS2_PLACEMENT_3D ( 'NONE', #25091, #47206, #55808 ) ;
#103416 = VERTEX_POINT ( 'NONE', #66728 ) ;
#103417 = VERTEX_POINT ( 'NONE', #10602 ) ;
#103419 =( BOUNDED_SURFACE ( )  B_SPLINE_SURFACE ( 2, 3, ( 
 ( #35598, #101366, #25932, #36671, #27519, #60396, #59318, #26451, #92189, #51195, #69535, #59860, #58789, #34539, #18341, #91685, #50650, #77083, #93805, #19435, #93273, #52265, #42583, #60919, #52805, #85731, #85179, #11264, #11803, #75484, #3200, #77623, #84115, #92731, #36143, #10214, #44735, #43127, #76012, #3740, #2112, #100815, #35062, #67930, #26977, #84652, #12864, #37735 ),
 ( #13926, #63034, #103486, #96469, #4795, #4264, #78659, #54368, #95934, #78142, #45266, #70057, #53345, #37192, #46315, #87313, #80252, #5841, #54917, #38767, #63579, #39300, #102961, #45783, #38252, #13394, #79207, #71632, #61452, #28568, #94347, #95395, #86265, #22059, #47365, #12339, #104538, #22607, #30691, #55442, #70594, #29124, #61993, #53865, #88377, #87843, #14451, #29634 ),
 ( #30150, #21535, #94885, #104003, #21025, #5329, #6361, #71116, #86793, #102427, #20509, #46836, #62510, #79738, #56505, #40338, #88896, #8497, #89952, #16060, #89435, #7423, #14991, #64111, #90488, #32806, #73218, #66204, #81309, #80791, #48418, #24192, #65680, #47883, #6903, #39825, #23123, #72701, #48941, #57038, #50018, #82389, #24716, #41399, #33338, #9020, #105600, #15525 ) ),
 .UNSPECIFIED., .F., .F., .F. ) 
 B_SPLINE_SURFACE_WITH_KNOTS ( ( 3, 3 ),
 ( 4, 2, 2, 2, 2, 2, 2, 2, 2, 2, 2, 2, 2, 2, 2, 2, 2, 2, 2, 2, 2, 2, 2, 4 ),
 ( 0.000000000000000000, 1.000000000000000000 ),
 ( 0.000000000000000000, 0.008322629228191371839, 0.01248394384228705689, 0.01664525845638274368, 0.02496788768457411378, 0.02912920229866980057, 0.03329051691276548736, 0.04161314614095686093, 0.04993577536914822756, 0.05825840459733960114, 0.06241971921143528446, 0.06658103382553097471, 0.07074234843962665109, 0.07282300574667449622, 0.07490366305372234135, 0.08322629228191372186, 0.09154892151010508849, 0.09987155073829645513, 0.1040328653523921454, 0.1081941799664878356, 0.1123554945805835259, 0.1165168091946792023, 0.1248394384228705689, 0.1331620676510619494 ),
 .UNSPECIFIED. ) 
 GEOMETRIC_REPRESENTATION_ITEM ( )  RATIONAL_B_SPLINE_SURFACE ( (
 ( 1.000000000000000000, 1.000000000000000000, 1.000000000000000000, 1.000000000000000000, 1.000000000000000000, 1.000000000000000000, 1.000000000000000000, 1.000000000000000000, 1.000000000000000000, 1.000000000000000000, 1.000000000000000000, 1.000000000000000000, 1.000000000000000000, 1.000000000000000000, 1.000000000000000000, 1.000000000000000000, 1.000000000000000000, 1.000000000000000000, 1.000000000000000000, 1.000000000000000000, 1.000000000000000000, 1.000000000000000000, 1.000000000000000000, 1.000000000000000000, 1.000000000000000000, 1.000000000000000000, 1.000000000000000000, 1.000000000000000000, 1.000000000000000000, 1.000000000000000000, 1.000000000000000000, 1.000000000000000000, 1.000000000000000000, 1.000000000000000000, 1.000000000000000000, 1.000000000000000000, 1.000000000000000000, 1.000000000000000000, 1.000000000000000000, 1.000000000000000000, 1.000000000000000000, 1.000000000000000000, 1.000000000000000000, 1.000000000000000000, 1.000000000000000000, 1.000000000000000000, 1.000000000000000000, 1.000000000000000000),
 ( 1.857142857142858317, 1.857142857142858317, 1.857142857142858317, 1.857142857142858317, 1.857142857142858317, 1.857142857142858317, 1.857142857142858317, 1.857142857142858317, 1.857142857142858317, 1.857142857142858317, 1.857142857142858317, 1.857142857142858317, 1.857142857142858317, 1.857142857142858317, 1.857142857142858317, 1.857142857142858317, 1.857142857142858317, 1.857142857142858317, 1.857142857142858317, 1.857142857142858317, 1.857142857142858317, 1.857142857142858317, 1.857142857142858317, 1.857142857142858317, 1.857142857142858317, 1.857142857142858317, 1.857142857142858317, 1.857142857142858317, 1.857142857142858317, 1.857142857142858317, 1.857142857142858317, 1.857142857142858317, 1.857142857142858317, 1.857142857142858317, 1.857142857142858317, 1.857142857142858317, 1.857142857142859205, 1.857142857142859205, 1.857142857142858317, 1.857142857142858317, 1.857142857142857428, 1.857142857142857428, 1.857142857142858317, 1.857142857142858317, 1.857142857142858317, 1.857142857142858317, 1.857142857142858317, 1.857142857142858317),
 ( 1.000000000000000000, 1.000000000000000000, 1.000000000000000000, 1.000000000000000000, 1.000000000000000000, 1.000000000000000000, 1.000000000000000000, 1.000000000000000000, 1.000000000000000000, 1.000000000000000000, 1.000000000000000000, 1.000000000000000000, 1.000000000000000000, 1.000000000000000000, 1.000000000000000000, 1.000000000000000000, 1.000000000000000000, 1.000000000000000000, 1.000000000000000000, 1.000000000000000000, 1.000000000000000000, 1.000000000000000000, 1.000000000000000000, 1.000000000000000000, 1.000000000000000000, 1.000000000000000000, 1.000000000000000000, 1.000000000000000000, 1.000000000000000000, 1.000000000000000000, 1.000000000000000000, 1.000000000000000000, 1.000000000000000000, 1.000000000000000000, 1.000000000000000000, 1.000000000000000000, 1.000000000000000000, 1.000000000000000000, 1.000000000000000000, 1.000000000000000000, 1.000000000000000000, 1.000000000000000000, 1.000000000000000000, 1.000000000000000000, 1.000000000000000000, 1.000000000000000000, 1.000000000000000000, 1.000000000000000000) ) ) 
 REPRESENTATION_ITEM ( '' )  SURFACE ( )  );
#103418 = CARTESIAN_POINT ( 'NONE',  ( 2.500000000000000000, -8.000000000000000000, 14.79019945774903988 ) ) ;
#103420 = COLOUR_RGB ( '', 0.66274510, 0.83137255, 0.94901961) ;
#103421 = CARTESIAN_POINT ( 'NONE',  ( -5.000000000000002665, 152.0000000000000000, -5.000000000000000000 ) ) ;
#103422 = ORIENTED_EDGE ( 'NONE', *, *, #17445, .F. ) ;
#103423 =( NAMED_UNIT ( * ) SI_UNIT ( $, .STERADIAN. ) SOLID_ANGLE_UNIT ( ) );
#103424 = CARTESIAN_POINT ( 'NONE',  ( -6.645598051714149967, 41.91296950070219651, -68.91429205809731684 ) ) ;
#103425 = CARTESIAN_POINT ( 'NONE',  ( -91.55378440295650933, -59.99999999999023714, 204.7501500527700671 ) ) ;
#103426 = CIRCLE ( 'NONE', #89650, 5.000000000000002665 ) ;
#103427 = DIRECTION ( 'NONE',  ( -1.000000000000000000, -1.224606353822377258E-16, -0.000000000000000000 ) ) ;
#103428 = CARTESIAN_POINT ( 'NONE',  ( 57.09504128153807301, -59.99999999999997868, -38.79348205093937452 ) ) ;
#103429 = CARTESIAN_POINT ( 'NONE',  ( 10.73738285532599512, -5.000000000000000000, 12.43173891483628601 ) ) ;
#103430 = CARTESIAN_POINT ( 'NONE',  ( -5.921004821993908429, 41.52415853127881462, -58.52392862547825558 ) ) ;
#103432 = CARTESIAN_POINT ( 'NONE',  ( 8.054255350734946362, -25.54841287528824623, 28.14046425560073317 ) ) ;
#103431 = CARTESIAN_POINT ( 'NONE',  ( -94.42208465491292202, -30.00000000000002132, 63.29659460224121403 ) ) ;
#103433 = CARTESIAN_POINT ( 'NONE',  ( 0.000000000000000000, 44.00000000000000711, 0.000000000000000000 ) ) ;
#103434 = CARTESIAN_POINT ( 'NONE',  ( -48.12968807026369689, -60.28544049161936158, 54.32557363639672587 ) ) ;
#103435 = AXIS2_PLACEMENT_3D ( 'NONE', #89131, #40046, #33046 ) ;
#103436 = CARTESIAN_POINT ( 'NONE',  ( -6.951447413152006760, 41.73217189154441087, -59.36631701933645644 ) ) ;
#103437 = ORIENTED_EDGE ( 'NONE', *, *, #13090, .F. ) ;
#103438 = CARTESIAN_POINT ( 'NONE',  ( 0.3587072354609493474, 13.57974219347169509, -49.30106301256189028 ) ) ;
#103439 = FACE_OUTER_BOUND ( 'NONE', #22515, .T. ) ;
#103440 = DIRECTION ( 'NONE',  ( -0.000000000000000000, -1.000000000000000000, -0.000000000000000000 ) ) ;
#103441 = ORIENTED_EDGE ( 'NONE', *, *, #88526, .F. ) ;
#103442 = CARTESIAN_POINT ( 'NONE',  ( -10.86574196480413335, -11.19705879606434529, 9.983399294863108508 ) ) ;
#103443 = ORIENTED_EDGE ( 'NONE', *, *, #82406, .F. ) ;
#103444 = CARTESIAN_POINT ( 'NONE',  ( 109.3019642819107418, -29.99999999999331379, 163.0555205557570559 ) ) ;
#103445 = DIRECTION ( 'NONE',  ( 0.000000000000000000, 1.000000000000000000, 0.000000000000000000 ) ) ;
#103446 = DIRECTION ( 'NONE',  ( -1.000000000000000000, 0.000000000000000000, 0.000000000000000000 ) ) ;
#103447 = CARTESIAN_POINT ( 'NONE',  ( -57.69562748392037577, 41.99999999991776178, 15.50526908263360681 ) ) ;
#103448 = CARTESIAN_POINT ( 'NONE',  ( 95.19895599661560937, -29.99999999999999645, 191.3423363543731455 ) ) ;
#103449 = DIRECTION ( 'NONE',  ( 1.000000000000000000, 1.224606353822377258E-16, 0.000000000000000000 ) ) ;
#103450 = VERTEX_POINT ( 'NONE', #18745 ) ;
#103451 = EDGE_CURVE ( 'NONE', #36922, #67654, #75966, .T. ) ;
#103452 = ORIENTED_EDGE ( 'NONE', *, *, #3134, .T. ) ;
#103453 = ORIENTED_EDGE ( 'NONE', *, *, #19513, .F. ) ;
#103454 = CARTESIAN_POINT ( 'NONE',  ( 54.20624670247494237, -42.96740642929500353, 59.98673961352833572 ) ) ;
#103455 = CARTESIAN_POINT ( 'NONE',  ( 36.84999999999999432, 1.533819458162526451E-15, 0.000000000000000000 ) ) ;
#103456 = AXIS2_PLACEMENT_3D ( 'NONE', #17299, #83075, #18368 ) ;
#103457 = FACE_OUTER_BOUND ( 'NONE', #7683, .T. ) ;
#103458 = EDGE_CURVE ( 'NONE', #52196, #23615, #877, .T. ) ;
#103459 = EDGE_CURVE ( 'NONE', #13028, #78182, #103528, .T. ) ;
#103460 = VERTEX_POINT ( 'NONE', #42443 ) ;
#103461 = CARTESIAN_POINT ( 'NONE',  ( 30.59999999999999787, 1.533819458162526451E-15, 0.000000000000000000 ) ) ;
#103462 = ORIENTED_EDGE ( 'NONE', *, *, #82608, .F. ) ;
#103463 = CARTESIAN_POINT ( 'NONE',  ( 5.799999999999999822, 8.000000000000000000, 0.000000000000000000 ) ) ;
#103464 = CARTESIAN_POINT ( 'NONE',  ( 88.58302811347638794, -38.54321962364008414, 200.1547288739133990 ) ) ;
#103465 = CARTESIAN_POINT ( 'NONE',  ( 10.10731083982912004, 15.36174436921201192, 10.31675818847685555 ) ) ;
#103466 = CARTESIAN_POINT ( 'NONE',  ( 83.89778286979191080, -45.28641516711167014, 4.373900399497115288 ) ) ;
#103467 = FACE_OUTER_BOUND ( 'NONE', #80966, .T. ) ;
#103468 = CARTESIAN_POINT ( 'NONE',  ( 33.08796297677666587, 372.6636829999529823, 24.05784598877716363 ) ) ;
#103469 = DIRECTION ( 'NONE',  ( 0.000000000000000000, 0.000000000000000000, 1.000000000000000000 ) ) ;
#103470 = CARTESIAN_POINT ( 'NONE',  ( 25.59999999999999787, -3.309499999999999886, 0.000000000000000000 ) ) ;
#103471 = SURFACE_SIDE_STYLE ('',( #23108 ) ) ;
#103472 = ORIENTED_EDGE ( 'NONE', *, *, #29149, .F. ) ;
#103473 = CARTESIAN_POINT ( 'NONE',  ( -5.656854249492381470, -10.25000000409677092, 5.656854249492379694 ) ) ;
#103474 = ADVANCED_FACE ( 'NONE', ( #51594 ), #105177, .F. ) ;
#103475 = CARTESIAN_POINT ( 'NONE',  ( -34.14329934198877226, 464.2299144111568125, 6.063562457997684341 ) ) ;
#103476 = AXIS2_PLACEMENT_3D ( 'NONE', #48505, #65239, #988 ) ;
#103477 = CARTESIAN_POINT ( 'NONE',  ( -26.49211181453642538, 36.83374520352522552, 9.907801504249466262 ) ) ;
#103478 = ORIENTED_EDGE ( 'NONE', *, *, #42760, .F. ) ;
#103479 = CARTESIAN_POINT ( 'NONE',  ( -22.06692060364423824, 305.1441668778134044, -8.937571418765491771 ) ) ;
#103480 = B_SPLINE_CURVE_WITH_KNOTS ( 'NONE', 3,
 ( #15773, #15241, #50637, #23366, #96703, #81026, #40055, #48656, #22843, #55673 ),
 .UNSPECIFIED., .F., .F.,
 ( 4, 2, 2, 2, 4 ),
 ( 0.000000000000000000, 0.2500000000000000000, 0.5000000000000000000, 0.7500000000000000000, 1.000000000000000000 ),
 .UNSPECIFIED. ) ;
#103481 = CARTESIAN_POINT ( 'NONE',  ( -36.03738032064502050, 307.9717951417662789, 13.05167544916968403 ) ) ;
#103482 = AXIS2_PLACEMENT_3D ( 'NONE', #98400, #14819, #16421 ) ;
#103483 = CARTESIAN_POINT ( 'NONE',  ( -12.08750511397919247, -4.706244484278460760, -76.83407907353502253 ) ) ;
#103484 = DIRECTION ( 'NONE',  ( -1.000000000000000000, -0.000000000000000000, -0.000000000000000000 ) ) ;
#103485 = CARTESIAN_POINT ( 'NONE',  ( 3.313708498984762052, -21.21875000000000000, -8.000000000000000000 ) ) ;
#103486 = CARTESIAN_POINT ( 'NONE',  ( -43.59233498779423854, -29.69447325614249067, 52.52981076111234415 ) ) ;
#103487 = ADVANCED_FACE ( 'NONE', ( #25789 ), #12217, .F. ) ;
#103488 = DIRECTION ( 'NONE',  ( 0.000000000000000000, 0.000000000000000000, 1.000000000000000000 ) ) ;
#103489 = ORIENTED_EDGE ( 'NONE', *, *, #20547, .F. ) ;
#103490 = CARTESIAN_POINT ( 'NONE',  ( 86.39767885033103312, -17.86857175737891978, 174.6560174384326842 ) ) ;
#103491 = EDGE_CURVE ( 'NONE', #62254, #23008, #67791, .T. ) ;
#103492 = CARTESIAN_POINT ( 'NONE',  ( -48.02835407290516656, 9.771516447483513446, 16.85535821593516559 ) ) ;
#103493 = CARTESIAN_POINT ( 'NONE',  ( 4.051286199644070329, -1.398729870307595879, 103.8758286790405236 ) ) ;
#103494 = ORIENTED_EDGE ( 'NONE', *, *, #12691, .T. ) ;
#103495 = CARTESIAN_POINT ( 'NONE',  ( 93.84014446886344274, -57.67487048525376991, 10.77052861846502907 ) ) ;
#103496 = AXIS2_PLACEMENT_3D ( 'NONE', #63161, #81431, #46953 ) ;
#103497 = CARTESIAN_POINT ( 'NONE',  ( 0.4033376246892493855, -7.198601258566898586, 0.5316568767328675449 ) ) ;
#103498 = FACE_OUTER_BOUND ( 'NONE', #106192, .T. ) ;
#103499 = CARTESIAN_POINT ( 'NONE',  ( -29.68315524076989576, 13.12249633091057177, 39.60535821593503414 ) ) ;
#103500 = CARTESIAN_POINT ( 'NONE',  ( -8.066564334389425994, -22.17767452351848689, -38.54423803581626373 ) ) ;
#103501 = AXIS2_PLACEMENT_3D ( 'NONE', #90919, #23549, #106011 ) ;
#103502 = CARTESIAN_POINT ( 'NONE',  ( 0.9999999999999941158, -1.734723475976807094E-15, 101.0455488498966758 ) ) ;
#103503 = CARTESIAN_POINT ( 'NONE',  ( 34.50342751135733010, -23.83194123643590245, 33.31419988176715918 ) ) ;
#103505 = CARTESIAN_POINT ( 'NONE',  ( -10.64386978829505814, 14.84064791310457920, 9.848362920724447633 ) ) ;
#103504 = CARTESIAN_POINT ( 'NONE',  ( 41.61991837719464371, 463.6613259647958785, 18.05819200971493288 ) ) ;
#103506 = CONICAL_SURFACE ( 'NONE', #31175, 6.500000000000000888, 0.8987552595851637793 ) ;
#103507 = CARTESIAN_POINT ( 'NONE',  ( 43.17378635866474212, 487.6240912981842826, 8.491167829005039636 ) ) ;
#103508 = CARTESIAN_POINT ( 'NONE',  ( 15.59999999999999787, 1.533819458162526451E-15, 0.000000000000000000 ) ) ;
#103509 = CARTESIAN_POINT ( 'NONE',  ( 43.58459202512976560, 371.6927194222791968, 14.08847290620314752 ) ) ;
#103510 = DIRECTION ( 'NONE',  ( -1.000000000000000000, 0.000000000000000000, 0.000000000000000000 ) ) ;
#103511 = CARTESIAN_POINT ( 'NONE',  ( -82.46191414289508259, -38.00000000000002842, 16.70185672408629785 ) ) ;
#103512 = PRODUCT_DEFINITION_SHAPE ( 'NONE', 'NONE',  #106797 ) ;
#103513 = VERTEX_POINT ( 'NONE', #34396 ) ;
#103514 = CARTESIAN_POINT ( 'NONE',  ( -9.960308305544327112, -2.965541965107718614, 15.28860432758946075 ) ) ;
#103515 = CARTESIAN_POINT ( 'NONE',  ( 56.22793774957824553, 6.975173280561618775E-15, 0.000000000000000000 ) ) ;
#103517 = CARTESIAN_POINT ( 'NONE',  ( 7.758608792424636746, -21.77038665610601598, -30.37594175526581708 ) ) ;
#103516 = DIRECTION ( 'NONE',  ( 0.000000000000000000, 0.000000000000000000, -1.000000000000000000 ) ) ;
#103518 = EDGE_CURVE ( 'NONE', #39589, #30622, #99068, .T. ) ;
#103519 = ORIENTED_EDGE ( 'NONE', *, *, #65240, .F. ) ;
#103520 = COLOUR_RGB ( '', 0.31764706, 0.68627451, 0.89019608) ;
#103521 = CARTESIAN_POINT ( 'NONE',  ( 2.387978478800936610, 7.281554020289634721, -7.069802615102036114 ) ) ;
#103522 = CARTESIAN_POINT ( 'NONE',  ( 44.83349330513380693, 1.593028355512270567E-15, 0.000000000000000000 ) ) ;
#103523 = EDGE_LOOP ( 'NONE', ( #75734, #67579, #79055, #22892, #54362 ) ) ;
#103524 = AXIS2_PLACEMENT_3D ( 'NONE', #30490, #23466, #79019 ) ;
#103525 = ADVANCED_FACE ( 'NONE', ( #92589, #100151 ), #50518, .T. ) ;
#103526 = EDGE_CURVE ( 'NONE', #2575, #12726, #95454, .T. ) ;
#103527 = DIRECTION ( 'NONE',  ( 0.000000000000000000, 0.000000000000000000, -1.000000000000000000 ) ) ;
#103528 = CIRCLE ( 'NONE', #34669, 11.00000000000000000 ) ;
#103529 = FACE_OUTER_BOUND ( 'NONE', #58853, .T. ) ;
#103530 = CARTESIAN_POINT ( 'NONE',  ( -92.73406948728150212, -59.99999999999998579, -6.025074217602045756 ) ) ;
#103531 = EDGE_LOOP ( 'NONE', ( #5427, #88693, #50570, #101441 ) ) ;
#103532 = CARTESIAN_POINT ( 'NONE',  ( 8.245342207438705273, 41.99999999999999289, -58.66077168407692710 ) ) ;
#103533 = DIRECTION ( 'NONE',  ( 0.000000000000000000, 0.000000000000000000, -1.000000000000000000 ) ) ;
#103534 = DIRECTION ( 'NONE',  ( -1.000000000000000000, -0.000000000000000000, -0.000000000000000000 ) ) ;
#103536 = DIRECTION ( 'NONE',  ( 0.000000000000000000, -0.3420201433256725987, -0.9396926207859068736 ) ) ;
#103535 = DIRECTION ( 'NONE',  ( -1.000000000000000000, 0.000000000000000000, 0.000000000000000000 ) ) ;
#103537 = EDGE_CURVE ( 'NONE', #3603, #39461, #52845, .T. ) ;
#103538 = CARTESIAN_POINT ( 'NONE',  ( -82.60715075437619248, -42.97642582163322800, 171.7397776580246500 ) ) ;
#103539 = ORIENTED_EDGE ( 'NONE', *, *, #64576, .T. ) ;
#103540 = CARTESIAN_POINT ( 'NONE',  ( 6.539198257602121700, 3.775407874310910739, -6.286450516131048438 ) ) ;
#103541 = EDGE_CURVE ( 'NONE', #86259, #81954, #17402, .T. ) ;
#103542 = VERTEX_POINT ( 'NONE', #88231 ) ;
#103543 = EDGE_CURVE ( 'NONE', #9641, #84383, #31202, .T. ) ;
#103544 = ORIENTED_EDGE ( 'NONE', *, *, #93922, .F. ) ;
#103545 = CARTESIAN_POINT ( 'NONE',  ( -12.76371622530477090, -4.999999999999998224, 12.10534828917588435 ) ) ;
#103546 = CARTESIAN_POINT ( 'NONE',  ( -6.124999999999272582, -61.24691634665675366, 14.41094225130375683 ) ) ;
#103547 = VERTEX_POINT ( 'NONE', #104391 ) ;
#103548 = CARTESIAN_POINT ( 'NONE',  ( 19.34999999999999787, 1.533819458162526451E-15, 0.000000000000000000 ) ) ;
#103549 = CARTESIAN_POINT ( 'NONE',  ( 0.000000000000000000, 0.000000000000000000, -7.131971428571428184 ) ) ;
#103550 = CARTESIAN_POINT ( 'NONE',  ( -69.44743540119901581, -57.67117814800237596, -34.85819734733303221 ) ) ;
#103551 = CARTESIAN_POINT ( 'NONE',  ( 3.454253436624921569, -49.15858197120396511, 103.7259032015043090 ) ) ;
#103552 = CARTESIAN_POINT ( 'NONE',  ( -10.28624191511820207, 43.25714326066858462, 15.40779740156164124 ) ) ;
#103553 = CARTESIAN_POINT ( 'NONE',  ( 23.97722388339762389, 27.87827700592711722, 30.95083563548385541 ) ) ;
#103554 = FACE_OUTER_BOUND ( 'NONE', #96430, .T. ) ;
#103555 = CARTESIAN_POINT ( 'NONE',  ( 3.836411046841841532, 15.00000000000000000, -9.999999999999998224 ) ) ;
#103556 = CARTESIAN_POINT ( 'NONE',  ( 94.38107034336813683, -59.99999999999990763, 5.298252861571447703 ) ) ;
#103557 = CARTESIAN_POINT ( 'NONE',  ( -68.01705929348101165, -29.99999999999997158, 119.4519777144086703 ) ) ;
#103558 = CARTESIAN_POINT ( 'NONE',  ( -55.88782504570332321, -25.61907991660268280, 56.57138212751718953 ) ) ;
#103559 = EDGE_LOOP ( 'NONE', ( #28648, #100118, #55529, #86833 ) ) ;
#103560 = DIRECTION ( 'NONE',  ( 0.000000000000000000, -1.000000000000000000, 0.000000000000000000 ) ) ;
#103561 = ORIENTED_EDGE ( 'NONE', *, *, #62385, .F. ) ;
#103562 = CARTESIAN_POINT ( 'NONE',  ( -101.5044452224088047, -52.72315398099703998, 192.7887324484784699 ) ) ;
#103563 = CARTESIAN_POINT ( 'NONE',  ( -30.92841573401175381, 13.86971257847473460, -40.99043602818892396 ) ) ;
#103564 = ORIENTED_EDGE ( 'NONE', *, *, #9617, .T. ) ;
#103565 = CARTESIAN_POINT ( 'NONE',  ( 19.41389256533520324, 49.95052971997019142, 60.89323077825420683 ) ) ;
#103567 =( GEOMETRIC_REPRESENTATION_CONTEXT ( 3 ) GLOBAL_UNCERTAINTY_ASSIGNED_CONTEXT ( ( #101979 ) ) GLOBAL_UNIT_ASSIGNED_CONTEXT ( ( #13568, #29803, #95056 ) ) REPRESENTATION_CONTEXT ( 'NONE', 'WORKASPACE' ) );
#103566 = FILL_AREA_STYLE ('',( #52351 ) ) ;
#103568 = CARTESIAN_POINT ( 'NONE',  ( 3.400000000000000355, 0.000000000000000000, -4.987924522925830217 ) ) ;
#103569 = CARTESIAN_POINT ( 'NONE',  ( -5.082755093536326818, -12.59375000204838635, 5.082755093536325042 ) ) ;
#103570 = CYLINDRICAL_SURFACE ( 'NONE', #37881, 1.250000000000001110 ) ;
#103571 = SURFACE_STYLE_FILL_AREA ( #37820 ) ;
#103572 = CARTESIAN_POINT ( 'NONE',  ( -40.75641113481592726, 360.0948485545300741, 24.37153223514695100 ) ) ;
#103573 = VECTOR ( 'NONE', #22852, 1000.000000000000000 ) ;
#103574 = CARTESIAN_POINT ( 'NONE',  ( -9.041837334944171189, 137.4638978311212725, -1.155557966632342738E-30 ) ) ;
#103575 = CARTESIAN_POINT ( 'NONE',  ( 30.38238271166915538, 438.0643985705939372, 22.32817737082370257 ) ) ;
#103576 = CARTESIAN_POINT ( 'NONE',  ( -33.94783393359910662, 484.1261039197349305, 1.321740980884783978 ) ) ;
#103577 = CARTESIAN_POINT ( 'NONE',  ( -28.86452025935745880, -46.43714135143746091, 33.97076303928542984 ) ) ;
#103578 = VERTEX_POINT ( 'NONE', #73068 ) ;
#103579 = VERTEX_POINT ( 'NONE', #14311 ) ;
#103580 = CARTESIAN_POINT ( 'NONE',  ( 47.01442997823554748, -46.44001080992690333, 48.25839572838238922 ) ) ;
#103581 = CARTESIAN_POINT ( 'NONE',  ( -0.2951772788882962018, 7.823394093897796608, 51.71673678500803106 ) ) ;
#103582 = AXIS2_PLACEMENT_3D ( 'NONE', #37667, #11732, #29569 ) ;
#103583 = CARTESIAN_POINT ( 'NONE',  ( -6.321595794353349618, 15.64364823866884180, -3.012682989575209636 ) ) ;
#103584 = EDGE_CURVE ( 'NONE', #54844, #44950, #30012, .T. ) ;
#103585 = STYLED_ITEM ( 'NONE', ( #72183 ), #73760 ) ;
#103586 = CARTESIAN_POINT ( 'NONE',  ( -104.4730387931192581, -38.40368207287023239, 197.9910534897900902 ) ) ;
#103587 = ORIENTED_EDGE ( 'NONE', *, *, #81782, .T. ) ;
#103588 = CARTESIAN_POINT ( 'NONE',  ( 90.73652762505595604, -38.34866151637469045, 17.91778245446875317 ) ) ;
#103589 = CARTESIAN_POINT ( 'NONE',  ( 81.38975290692940234, -59.99999999999997158, 184.8793320046452777 ) ) ;
#103590 = CARTESIAN_POINT ( 'NONE',  ( -19.43447931428028141, 49.96600724177113761, 60.75670255394499009 ) ) ;
#103591 = CARTESIAN_POINT ( 'NONE',  ( 5.558539409542769150, 40.95021212697733404, -70.99752138050020278 ) ) ;
#103592 = CARTESIAN_POINT ( 'NONE',  ( -31.17407356531878193, 437.9983974556887460, 21.19255796710519846 ) ) ;
#103593 = CARTESIAN_POINT ( 'NONE',  ( -32.13417934727930714, 435.4422780298330622, 16.28732618035900614 ) ) ;
#103594 = DIRECTION ( 'NONE',  ( 0.000000000000000000, 1.000000000000000000, 0.000000000000000000 ) ) ;
#103595 = CARTESIAN_POINT ( 'NONE',  ( 77.81167547839096699, -60.00000000000001421, 192.4355787521637922 ) ) ;
#103596 = B_SPLINE_CURVE_WITH_KNOTS ( 'NONE', 3,
 ( #90157, #31940, #82598, #81503, #65881, #24399, #97701, #42131, #24915, #74494 ),
 .UNSPECIFIED., .F., .F.,
 ( 4, 2, 2, 2, 4 ),
 ( 0.000000000000000000, 0.2499999999999999722, 0.5000000000000000000, 0.7500000000000000000, 1.000000000000000000 ),
 .UNSPECIFIED. ) ;
#103597 = DIRECTION ( 'NONE',  ( 0.000000000000000000, -1.000000000000000000, 0.000000000000000000 ) ) ;
#103598 = EDGE_CURVE ( 'NONE', #47451, #89958, #96613, .T. ) ;
#103599 = ORIENTED_EDGE ( 'NONE', *, *, #70560, .T. ) ;
#103600 = CARTESIAN_POINT ( 'NONE',  ( -32.41288963471964735, 299.5866157103865248, -0.9436238929854601221 ) ) ;
#103601 = CARTESIAN_POINT ( 'NONE',  ( 6.928203230275509661, 30.00000000000000000, 4.000000000000000000 ) ) ;
#103602 = CARTESIAN_POINT ( 'NONE',  ( -7.414580834929596520, 27.35343719718517974, 3.010264818013835608 ) ) ;
#103603 = ORIENTED_EDGE ( 'NONE', *, *, #15299, .F. ) ;
#103605 = CARTESIAN_POINT ( 'NONE',  ( 5.272632769170305878, 14.19522521122798331, -33.98504043590990165 ) ) ;
#103604 = CARTESIAN_POINT ( 'NONE',  ( -104.9207578273651364, -38.39526174885175180, 197.5709644312131559 ) ) ;
#103606 = CARTESIAN_POINT ( 'NONE',  ( 5.656854249492380582, -21.31249999999999289, -5.656854249492379694 ) ) ;
#103607 = DIRECTION ( 'NONE',  ( 0.000000000000000000, 0.000000000000000000, 1.000000000000000000 ) ) ;
#103608 =( NAMED_UNIT ( * ) PLANE_ANGLE_UNIT ( ) SI_UNIT ( $, .RADIAN. ) );
#103609 = CARTESIAN_POINT ( 'NONE',  ( -5.082755093536325042, -15.96875000204838635, -5.082755093536325930 ) ) ;
#103610 = VECTOR ( 'NONE', #62592, 1000.000000000000000 ) ;
#103611 = CARTESIAN_POINT ( 'NONE',  ( 5.036189802309102070, -5.000000000000015099, -93.73786388411730286 ) ) ;
#103612 = AXIS2_PLACEMENT_3D ( 'NONE', #76041, #51221, #102455 ) ;
#103613 = CARTESIAN_POINT ( 'NONE',  ( 0.000000000000000000, 4.898587196589413815E-16, -4.000000000000000888 ) ) ;
#103615 = VERTEX_POINT ( 'NONE', #48272 ) ;
#103614 =( NAMED_UNIT ( * ) PLANE_ANGLE_UNIT ( ) SI_UNIT ( $, .RADIAN. ) );
#103616 = CARTESIAN_POINT ( 'NONE',  ( 84.78132171091615987, -25.52741569763149698, 164.4133495432128882 ) ) ;
#103617 = EDGE_CURVE ( 'NONE', #18245, #95748, #53573, .T. ) ;
#103618 = LINE ( 'NONE', #62130, #17052 ) ;
#103619 = CARTESIAN_POINT ( 'NONE',  ( 37.56673239365873940, 27.88554838446218653, 10.95617127780822564 ) ) ;
#103620 = ORIENTED_EDGE ( 'NONE', *, *, #28390, .F. ) ;
#103621 = CARTESIAN_POINT ( 'NONE',  ( -37.58421307733613048, 369.0431394919717718, 4.069084478531508786 ) ) ;
#103622 = DIRECTION ( 'NONE',  ( -1.000000000000000000, -0.000000000000000000, -0.000000000000000000 ) ) ;
#103623 = DIRECTION ( 'NONE',  ( 0.000000000000000000, 1.000000000000000000, 0.000000000000000000 ) ) ;
#103624 = DIRECTION ( 'NONE',  ( 1.000000000000000000, -0.000000000000000000, -0.000000000000000000 ) ) ;
#103625 = CARTESIAN_POINT ( 'NONE',  ( -23.01379380627861693, 43.78037731197083815, -78.86126435638672660 ) ) ;
#103626 = FACE_OUTER_BOUND ( 'NONE', #12644, .T. ) ;
#103627 = ORIENTED_EDGE ( 'NONE', *, *, #94417, .T. ) ;
#103628 =( NAMED_UNIT ( * ) SI_UNIT ( $, .STERADIAN. ) SOLID_ANGLE_UNIT ( ) );
#103629 = CARTESIAN_POINT ( 'NONE',  ( -77.71356797093831403, -30.00000000000000355, -16.14039426699441648 ) ) ;
#103630 = DIRECTION ( 'NONE',  ( -1.000000000000000000, -1.224606353822377258E-16, -0.000000000000000000 ) ) ;
#103631 = DIRECTION ( 'NONE',  ( -1.000000000000000000, -0.000000000000000000, -0.000000000000000000 ) ) ;
#103633 = CARTESIAN_POINT ( 'NONE',  ( -15.99999999999999645, 4.197692598229818550, -4.745459346021418057 ) ) ;
#103632 = CARTESIAN_POINT ( 'NONE',  ( 43.74985542820356699, 435.5770091380370559, 16.96136490515564788 ) ) ;
#103634 = PRODUCT_DEFINITION ( 'UNKNOWN', '', #98952, #2472 ) ;
#103635 = CARTESIAN_POINT ( 'NONE',  ( 4.401442555609581635E-16, -17.28125000204838813, -7.188101187500000044 ) ) ;
#103636 = CARTESIAN_POINT ( 'NONE',  ( -30.00000000000000000, 488.7105273189911259, 4.072454560254398892 ) ) ;
#103637 = CARTESIAN_POINT ( 'NONE',  ( 1.224646799147353454E-15, 70.00000000000000000, 10.00000000000000178 ) ) ;
#103638 = ITEM_DEFINED_TRANSFORMATION ( 'NONE', 'NONE', #31775,  #10728 ) ;
#103639 = ORIENTED_EDGE ( 'NONE', *, *, #21752, .F. ) ;
#103640 = CONICAL_SURFACE ( 'NONE', #105339, 13.50000000000000178, 1.047197551196596077 ) ;
#103641 = CIRCLE ( 'NONE', #93332, 4.000000000000000000 ) ;
#103642 = FACE_OUTER_BOUND ( 'NONE', #85528, .T. ) ;
#103643 = CARTESIAN_POINT ( 'NONE',  ( 33.09999999999999432, 1.533819458162526451E-15, 0.000000000000000000 ) ) ;
#103644 = CARTESIAN_POINT ( 'NONE',  ( -9.076657994649689698, 14.02231722283517534, -4.999999999999365841 ) ) ;
#103645 = LINE ( 'NONE', #22227, #67035 ) ;
#103646 = CARTESIAN_POINT ( 'NONE',  ( -2.352990130084491319E-16, 7.505553499465148271, -6.064240316920404439 ) ) ;
#103647 = ORIENTED_EDGE ( 'NONE', *, *, #5285, .F. ) ;
#103648 =( NAMED_UNIT ( * ) SI_UNIT ( $, .STERADIAN. ) SOLID_ANGLE_UNIT ( ) );
#103649 = CARTESIAN_POINT ( 'NONE',  ( 6.249999999999998224, 0.000000000000000000, 0.000000000000000000 ) ) ;
#103651 = ORIENTED_EDGE ( 'NONE', *, *, #93820, .F. ) ;
#103650 = STYLED_ITEM ( 'NONE', ( #61131 ), #19950 ) ;
#103652 = EDGE_CURVE ( 'NONE', #9392, #48472, #10518, .T. ) ;
#103653 = COLOUR_RGB ( '', 0.72549020, 0.75294118, 0.79215686) ;
#103654 = CARTESIAN_POINT ( 'NONE',  ( -1.545654944154558175, -0.02845455282771877301, 101.5781950003720624 ) ) ;
#103655 =( NAMED_UNIT ( * ) SI_UNIT ( $, .STERADIAN. ) SOLID_ANGLE_UNIT ( ) );
#103656 = CARTESIAN_POINT ( 'NONE',  ( -17.74039601254163045, 36.76373445370536075, 22.27539783717242727 ) ) ;
#103657 = CARTESIAN_POINT ( 'NONE',  ( -107.9499919529012431, -60.00000000000000000, 195.7098482030020250 ) ) ;
#103658 = CARTESIAN_POINT ( 'NONE',  ( -43.03357534758885095, 463.2291678140052227, 4.675918524150252331 ) ) ;
#103659 = CARTESIAN_POINT ( 'NONE',  ( 0.08224679563971286356, -7.710515798486365036, -2.644994884459105577 ) ) ;
#103660 = DIRECTION ( 'NONE',  ( 0.000000000000000000, 0.000000000000000000, 1.000000000000000000 ) ) ;
#103661 = CARTESIAN_POINT ( 'NONE',  ( 17.97939362404986952, 34.27531155324909662, -23.34516625433381520 ) ) ;
#103662 = CARTESIAN_POINT ( 'NONE',  ( -82.60006740705316020, -57.21883819474334842, 187.3423846480518762 ) ) ;
#103663 = B_SPLINE_CURVE_WITH_KNOTS ( 'NONE', 3,
 ( #53999, #86939, #13009, #8106, #48561, #104687, #55582, #81451, #24856, #71776, #56107, #22745, #88520, #72323, #23263, #57182, #57705, #98701, #40483, #5981, #49086, #90098 ),
 .UNSPECIFIED., .F., .F.,
 ( 4, 2, 2, 2, 2, 2, 2, 2, 2, 2, 4 ),
 ( 0.0002601258248896089241, 0.0007638464171177765079, 0.001015706713231860625, 0.001267567009345944851, 0.001519427305460029076, 0.001771287601574113302, 0.002275008193802294330, 0.002778728786030475358, 0.003282449378258655952, 0.003786169970486836980, 0.004289890562715018008 ),
 .UNSPECIFIED. ) ;
#103664 = CARTESIAN_POINT ( 'NONE',  ( 37.85403811240345107, 42.20638415471038485, -58.45930149705038303 ) ) ;
#103665 = ADVANCED_FACE ( 'NONE', ( #15385 ), #54771, .T. ) ;
#103666 = ORIENTED_EDGE ( 'NONE', *, *, #29989, .T. ) ;
#103667 = CARTESIAN_POINT ( 'NONE',  ( 5.500000000000007105, 42.00000000000000000, -65.90297134474647578 ) ) ;
#103668 = ADVANCED_FACE ( 'NONE', ( #38120 ), #168, .T. ) ;
#103669 = CARTESIAN_POINT ( 'NONE',  ( 5.909155701201247446, -68.86261680188732726, 1.073778020691679824 ) ) ;
#103670 = CARTESIAN_POINT ( 'NONE',  ( -83.71921483055798774, -37.82245684421392440, 34.46557360337037323 ) ) ;
#103671 = AXIS2_PLACEMENT_3D ( 'NONE', #81491, #64808, #7611 ) ;
#103672 = LINE ( 'NONE', #62696, #30576 ) ;
#103673 = B_SPLINE_CURVE_WITH_KNOTS ( 'NONE', 3,
 ( #18307, #36636, #2618, #26421 ),
 .UNSPECIFIED., .F., .F.,
 ( 4, 4 ),
 ( 3.766727042548887005E-15, 0.0002629889189324963639 ),
 .UNSPECIFIED. ) ;
#103674 = AXIS2_PLACEMENT_3D ( 'NONE', #38597, #104362, #99445 ) ;
#103675 = CARTESIAN_POINT ( 'NONE',  ( 9.439237903996360757, 141.9224268364482668, -4.999999999999999112 ) ) ;
#103676 = DIRECTION ( 'NONE',  ( 0.000000000000000000, -0.000000000000000000, 1.000000000000000000 ) ) ;
#103677 = CARTESIAN_POINT ( 'NONE',  ( 5.022013495303141006, 18.64316884711713840, 38.36535705883633796 ) ) ;
#103678 = CARTESIAN_POINT ( 'NONE',  ( 94.36203364593035303, -29.99999999999990763, 200.0833959884570845 ) ) ;
#103679 = CARTESIAN_POINT ( 'NONE',  ( -6.738183602098730825E-15, 17.51648154115788714, 55.02144460582525909 ) ) ;
#103680 = CARTESIAN_POINT ( 'NONE',  ( -104.6757555735165113, -59.99999999999997158, 94.38003174760403624 ) ) ;
#103681 = COLOUR_RGB ( '', 0.31764706, 0.68627451, 0.89019608) ;
#103682 = B_SPLINE_CURVE_WITH_KNOTS ( 'NONE', 3,
 ( #17691, #26878, #92627, #101268, #18785, #34438 ),
 .UNSPECIFIED., .F., .F.,
 ( 4, 2, 4 ),
 ( 0.000000000000000000, 0.002307655110370377804, 0.004615310220740755608 ),
 .UNSPECIFIED. ) ;
#103683 = CARTESIAN_POINT ( 'NONE',  ( -65.14366692970418171, -32.53254546774595468, 82.99592137394043334 ) ) ;
#103684 = ORIENTED_EDGE ( 'NONE', *, *, #64126, .F. ) ;
#103685 = CARTESIAN_POINT ( 'NONE',  ( 23.32141611262068892, 39.42442110531605692, 60.74505580753970690 ) ) ;
#103686 = CARTESIAN_POINT ( 'NONE',  ( 86.64996127643055956, -59.99999999999018740, 203.5283718990660304 ) ) ;
#103687 = ORIENTED_EDGE ( 'NONE', *, *, #37577, .T. ) ;
#103688 = DIRECTION ( 'NONE',  ( 0.000000000000000000, 0.000000000000000000, -1.000000000000000000 ) ) ;
#103689 = CARTESIAN_POINT ( 'NONE',  ( 7.188101187500000933, -22.43750000204838813, -2.977408999572650483 ) ) ;
#103690 = ORIENTED_EDGE ( 'NONE', *, *, #24932, .F. ) ;
#103691 = CARTESIAN_POINT ( 'NONE',  ( 61.37206225042174879, -1.232595164407830946E-29, 4.000000000000007105 ) ) ;
#103692 = VERTEX_POINT ( 'NONE', #7284 ) ;
#103693 = CARTESIAN_POINT ( 'NONE',  ( 10.28624191511840458, -1.200000000000000030E-05, 12.90779740156148847 ) ) ;
#103694 = SURFACE_STYLE_FILL_AREA ( #4471 ) ;
#103695 = CARTESIAN_POINT ( 'NONE',  ( -56.69921514847198551, -59.99999999999997868, -36.46084757427505707 ) ) ;
#103696 = CARTESIAN_POINT ( 'NONE',  ( 4.699999999999999289, 7.505553499465139389, 0.000000000000000000 ) ) ;
#103697 = CARTESIAN_POINT ( 'NONE',  ( -7.188101187500002709, -33.68750000204839523, 2.977408999572648707 ) ) ;
#103698 = CARTESIAN_POINT ( 'NONE',  ( 5.799999999999999822, 4.618802153517003184, -8.000000000000000000 ) ) ;
#103699 = CARTESIAN_POINT ( 'NONE',  ( 104.0908829527487711, 5.000000000000020428, 0.000000000000000000 ) ) ;
#103700 = CARTESIAN_POINT ( 'NONE',  ( 5.000000000000000000, -62.87212009006479008, 13.68440685388289602 ) ) ;
#103701 = CARTESIAN_POINT ( 'NONE',  ( 8.021436534415164826E-15, 79.50000000000000000, 65.50000000000000000 ) ) ;
#103702 = CARTESIAN_POINT ( 'NONE',  ( 33.00000000000000000, 450.0000000000002274, 13.20242257375370976 ) ) ;
#103703 = CARTESIAN_POINT ( 'NONE',  ( -43.58447375880955121, 371.6794660751320976, 14.08692068712289469 ) ) ;
#103704 = CARTESIAN_POINT ( 'NONE',  ( 24.51545473835047417, 303.7716308844144351, -9.801422722447242109 ) ) ;
#103705 = ORIENTED_EDGE ( 'NONE', *, *, #65236, .T. ) ;
#103706 = CARTESIAN_POINT ( 'NONE',  ( -9.169161018550420650, 53.73561361817692728, -1.678544271685364464 ) ) ;
#103707 =( NAMED_UNIT ( * ) SI_UNIT ( $, .STERADIAN. ) SOLID_ANGLE_UNIT ( ) );
#103708 = CARTESIAN_POINT ( 'NONE',  ( 36.21250698581494731, -25.65782209074169629, 33.24609087713096756 ) ) ;
#103709 = CARTESIAN_POINT ( 'NONE',  ( 2.227375807149031495, -1.734723475976807094E-15, 17.01589776168603407 ) ) ;
#103710 = EDGE_LOOP ( 'NONE', ( #6372, #77385, #71044, #10394 ) ) ;
#103711 = CARTESIAN_POINT ( 'NONE',  ( 6.169949891408089471, -4.949864754179694515, 4.426582755167080663 ) ) ;
#103712 = ADVANCED_FACE ( 'NONE', ( #38629 ), #40190, .T. ) ;
#103713 = VERTEX_POINT ( 'NONE', #14846 ) ;
#103715 = CYLINDRICAL_SURFACE ( 'NONE', #30276, 4.000000000000000000 ) ;
#103714 = CARTESIAN_POINT ( 'NONE',  ( 5.469880142252465660, -5.000000000000000000, -15.44784794604731637 ) ) ;
#103716 = DIRECTION ( 'NONE',  ( 0.000000000000000000, 0.000000000000000000, 1.000000000000000000 ) ) ;
#103717 = DIRECTION ( 'NONE',  ( 0.000000000000000000, 1.000000000000000000, -0.000000000000000000 ) ) ;
#103718 = DIRECTION ( 'NONE',  ( 0.000000000000000000, 0.000000000000000000, -1.000000000000000000 ) ) ;
#103719 = CARTESIAN_POINT ( 'NONE',  ( -48.99295625602604787, 13.11026251878874227, -16.41069188771936638 ) ) ;
#103720 = DIRECTION ( 'NONE',  ( -1.000000000000000000, -1.224606353822377258E-16, -0.000000000000000000 ) ) ;
#103721 = ORIENTED_EDGE ( 'NONE', *, *, #19819, .F. ) ;
#103722 = CARTESIAN_POINT ( 'NONE',  ( 92.56714293118520231, -60.00000000000000711, -2.262852274558210475 ) ) ;
#103723 = CARTESIAN_POINT ( 'NONE',  ( 9.235395886531431551E-16, -3.000000000000000000, -8.000000000000000000 ) ) ;
#103725 = DIRECTION ( 'NONE',  ( 0.000000000000000000, -0.6935263888315827963, 0.7204312236391647861 ) ) ;
#103724 = AXIS2_PLACEMENT_3D ( 'NONE', #74426, #18901, #58802 ) ;
#103726 = CIRCLE ( 'NONE', #95125, 5.000000000000001776 ) ;
#103727 = CARTESIAN_POINT ( 'NONE',  ( 0.000000000000000000, 4.898587196589412829E-16, -4.000000000000000000 ) ) ;
#103728 = CARTESIAN_POINT ( 'NONE',  ( -11.42114566974704992, 14.07739106013302788, -9.943574220663299101 ) ) ;
#103729 = ADVANCED_FACE ( 'NONE', ( #6220 ), #100062, .T. ) ;
#103730 = VERTEX_POINT ( 'NONE', #63439 ) ;
#103731 = CARTESIAN_POINT ( 'NONE',  ( -72.27031706507756326, -30.00000000000000711, 102.6033500751135108 ) ) ;
#103732 = ORIENTED_EDGE ( 'NONE', *, *, #70473, .T. ) ;
#103733 = DIRECTION ( 'NONE',  ( 0.000000000000000000, -1.000000000000000000, 0.000000000000000000 ) ) ;
#103734 = CARTESIAN_POINT ( 'NONE',  ( 59.89460441624491693, -4.000000000000000000, 4.898587196589421703E-16 ) ) ;
#103735 = CARTESIAN_POINT ( 'NONE',  ( 0.000000000000000000, 0.000000000000000000, 0.000000000000000000 ) ) ;
#103736 = CARTESIAN_POINT ( 'NONE',  ( 16.11127471224495622, 21.68306317500850611, 1.725009018242721792 ) ) ;
#103737 = CARTESIAN_POINT ( 'NONE',  ( 82.42550243480754091, -45.27952612892028839, -15.39413152779067495 ) ) ;
#103738 = AXIS2_PLACEMENT_3D ( 'NONE', #85421, #20200, #11505 ) ;
#103739 = CARTESIAN_POINT ( 'NONE',  ( -2.977408999572650039, -29.56250000204838813, -7.188101187500001821 ) ) ;
#103740 = LINE ( 'NONE', #87048, #22620 ) ;
#103741 = CARTESIAN_POINT ( 'NONE',  ( 0.000000000000000000, 49.00000000000000000, 0.000000000000000000 ) ) ;
#103742 = VECTOR ( 'NONE', #14345, 1000.000000000000000 ) ;
#103743 = EDGE_LOOP ( 'NONE', ( #105802, #62204, #9268, #19675, #19146 ) ) ;
#103745 = ORIENTED_EDGE ( 'NONE', *, *, #10619, .F. ) ;
#103744 = SURFACE_STYLE_USAGE ( .BOTH. , #3466 ) ;
#103746 = CARTESIAN_POINT ( 'NONE',  ( 79.16640897475440397, -49.90285545602715445, 152.0307613521693213 ) ) ;
#103747 = ADVANCED_FACE ( 'NONE', ( #47742 ), #27753, .F. ) ;
#103748 = SURFACE_STYLE_USAGE ( .BOTH. , #75887 ) ;
#103749 = ORIENTED_EDGE ( 'NONE', *, *, #35630, .T. ) ;
#103750 = CARTESIAN_POINT ( 'NONE',  ( -12.50000000000000711, 34.67384678108815166, -53.88384558013568437 ) ) ;
#103751 = EDGE_CURVE ( 'NONE', #63106, #5701, #8753, .T. ) ;
#103752 = CARTESIAN_POINT ( 'NONE',  ( 5.082755093536324154, -17.84375000204838457, 5.082755093536326818 ) ) ;
#103753 =( BOUNDED_SURFACE ( )  B_SPLINE_SURFACE ( 2, 3, ( 
 ( #11486, #53033, #77307, #61685, #3423, #102645, #36364, #100507, #94574, #44413, #20724, #85403, #19650, #69234, #28803, #2337, #10431, #28262, #27743, #52483, #53561, #92954, #20183, #85955, #76763, #10949, #86492, #35824, #12026, #101584, #45488, #44958, #77840, #3953 ),
 ( #19114, #26664, #51424, #69750, #68151, #78355, #59543, #34756, #67630, #92411, #18560, #43347, #76231, #35278, #27198, #101044, #51951, #87008, #97190, #80470, #6581, #79420, #95613, #96149, #104758, #63790, #13079, #22282, #21756, #5014, #56175, #46008, #5534, #55130 ),
 ( #23334, #30908, #47043, #38460, #46526, #14664, #88059, #96675, #79942, #47574, #39514, #37949, #22812, #71327, #55647, #29847, #87529, #72389, #70807, #4479, #88583, #71852, #105293, #104220, #14140, #62725, #31439, #30367, #54591, #13611, #37416, #63258, #64317, #6052 ) ),
 .UNSPECIFIED., .F., .T., .F. ) 
 B_SPLINE_SURFACE_WITH_KNOTS ( ( 3, 3 ),
 ( 4, 2, 2, 2, 2, 2, 2, 2, 2, 2, 2, 2, 2, 2, 2, 2, 4 ),
 ( 0.000000000000000000, 1.000000000000000000 ),
 ( -3.141592653589793116, -2.748893571891068976, -2.356194490192344837, -1.963495408493620697, -1.570796326794896558, -1.178097245096172418, -0.7853981633974482790, -0.3926990816987241395, 0.000000000000000000, 0.3926990816987241395, 0.7853981633974482790, 1.178097245096172418, 1.570796326794896558, 1.963495408493620697, 2.356194490192344837, 2.748893571891068976, 3.141592653589793116 ),
 .UNSPECIFIED. ) 
 GEOMETRIC_REPRESENTATION_ITEM ( )  RATIONAL_B_SPLINE_SURFACE ( (
 ( 1.000000000000000000, 1.000000000000000000, 1.000000000000000000, 1.000000000000000000, 1.000000000000000000, 1.000000000000000000, 1.000000000000000000, 1.000000000000000000, 1.000000000000000000, 1.000000000000000000, 1.000000000000000000, 1.000000000000000000, 1.000000000000000000, 1.000000000000000000, 1.000000000000000000, 1.000000000000000000, 1.000000000000000000, 1.000000000000000000, 1.000000000000000000, 1.000000000000000000, 1.000000000000000000, 1.000000000000000000, 1.000000000000000000, 1.000000000000000000, 1.000000000000000000, 1.000000000000000000, 1.000000000000000000, 1.000000000000000000, 1.000000000000000000, 1.000000000000000000, 1.000000000000000000, 1.000000000000000000, 1.000000000000000000, 1.000000000000000000),
 ( 1.857142857142858317, 1.857142857142858317, 1.857142857142858317, 1.857142857142858317, 1.857142857142858317, 1.857142857142858317, 1.857142857142858317, 1.857142857142858317, 1.857142857142858317, 1.857142857142858317, 1.857142857142858317, 1.857142857142858317, 1.857142857142858317, 1.857142857142858317, 1.857142857142858317, 1.857142857142858317, 1.857142857142858317, 1.857142857142858317, 1.857142857142858317, 1.857142857142858317, 1.857142857142858317, 1.857142857142858317, 1.857142857142858317, 1.857142857142858317, 1.857142857142858317, 1.857142857142858317, 1.857142857142858317, 1.857142857142858317, 1.857142857142858317, 1.857142857142858317, 1.857142857142858317, 1.857142857142858317, 1.857142857142858317, 1.857142857142858317),
 ( 1.000000000000000000, 1.000000000000000000, 1.000000000000000000, 1.000000000000000000, 1.000000000000000000, 1.000000000000000000, 1.000000000000000000, 1.000000000000000000, 1.000000000000000000, 1.000000000000000000, 1.000000000000000000, 1.000000000000000000, 1.000000000000000000, 1.000000000000000000, 1.000000000000000000, 1.000000000000000000, 1.000000000000000000, 1.000000000000000000, 1.000000000000000000, 1.000000000000000000, 1.000000000000000000, 1.000000000000000000, 1.000000000000000000, 1.000000000000000000, 1.000000000000000000, 1.000000000000000000, 1.000000000000000000, 1.000000000000000000, 1.000000000000000000, 1.000000000000000000, 1.000000000000000000, 1.000000000000000000, 1.000000000000000000, 1.000000000000000000) ) ) 
 REPRESENTATION_ITEM ( '' )  SURFACE ( )  );
#103754 = CARTESIAN_POINT ( 'NONE',  ( -96.25446706653225704, -57.62198180035323247, 204.5564252943773340 ) ) ;
#103755 = ADVANCED_FACE ( 'NONE', ( #39156 ), #44969, .T. ) ;
#103756 = CARTESIAN_POINT ( 'NONE',  ( 8.647875585311235014, 302.6863304874600544, 9.901865528037117059 ) ) ;
#103757 = ORIENTED_EDGE ( 'NONE', *, *, #49584, .T. ) ;
#103758 =( GEOMETRIC_REPRESENTATION_CONTEXT ( 3 ) GLOBAL_UNCERTAINTY_ASSIGNED_CONTEXT ( ( #2142 ) ) GLOBAL_UNIT_ASSIGNED_CONTEXT ( ( #89430, #55959, #32261 ) ) REPRESENTATION_CONTEXT ( 'NONE', 'WORKASPACE' ) );
#103759 = CARTESIAN_POINT ( 'NONE',  ( 3.840629472727446691E-14, -1.200000000000000030E-05, 28.50000000000000000 ) ) ;
#103760 = CARTESIAN_POINT ( 'NONE',  ( -5.725004243152315375, -13.57519148255367547, -1.812899781754681472 ) ) ;
#103761 = CARTESIAN_POINT ( 'NONE',  ( 7.040774347399620936, 41.35742771039598153, -58.68913404742972517 ) ) ;
#103762 = FACE_OUTER_BOUND ( 'NONE', #24186, .T. ) ;
#103763 = CARTESIAN_POINT ( 'NONE',  ( 3.313708498984762496, -9.968750004096770923, 7.999999999999998224 ) ) ;
#103764 = CARTESIAN_POINT ( 'NONE',  ( -3.619505474376166987, -12.72493135072700809, 32.14504651205703567 ) ) ;
#103765 = CARTESIAN_POINT ( 'NONE',  ( -45.99999999995679900, 486.6678415250283933, 5.056251502196789538 ) ) ;
#103766 = CARTESIAN_POINT ( 'NONE',  ( -36.64823341582351901, 437.5392299810053487, 4.281405873620232505 ) ) ;
#103768 = EDGE_CURVE ( 'NONE', #76086, #97178, #69056, .T. ) ;
#103767 = PRODUCT_CONTEXT ( 'NONE', #94869, 'mechanical' ) ;
#103769 = CARTESIAN_POINT ( 'NONE',  ( 16.64348903516499334, 45.60392139269944067, 6.657797401562596917 ) ) ;
#103770 = ORIENTED_EDGE ( 'NONE', *, *, #36245, .F. ) ;
#103771 = CARTESIAN_POINT ( 'NONE',  ( -0.7777777777777783452, -50.00000000000000711, 40.97837836547554957 ) ) ;
#103772 = FACE_OUTER_BOUND ( 'NONE', #19739, .T. ) ;
#103773 = CARTESIAN_POINT ( 'NONE',  ( -3.866873951915034802, 16.79560018603664417, -5.835353434046841592 ) ) ;
#103774 = CARTESIAN_POINT ( 'NONE',  ( 2.261098177828874789, -17.79480199333886148, -37.95484528153015447 ) ) ;
#103775 = CARTESIAN_POINT ( 'NONE',  ( -70.24286758344388204, -29.99999999999999645, 96.10628421054605042 ) ) ;
#103776 = DIRECTION ( 'NONE',  ( 0.000000000000000000, 1.000000000000000000, 0.000000000000000000 ) ) ;
#103777 = ORIENTED_EDGE ( 'NONE', *, *, #55416, .T. ) ;
#103778 = CARTESIAN_POINT ( 'NONE',  ( -25.86082360276708414, 37.20200679985001102, -8.660809983426863923 ) ) ;
#103779 = CARTESIAN_POINT ( 'NONE',  ( 106.6288915411791436, -57.65244875278279579, 200.4099561371844516 ) ) ;
#103780 = CARTESIAN_POINT ( 'NONE',  ( 61.30676048588166083, -21.77000062380585632, -22.67053275276132140 ) ) ;
#103781 = CARTESIAN_POINT ( 'NONE',  ( 66.74444444444444002, 3.309500000000014541, 0.000000000000000000 ) ) ;
#103782 = FACE_OUTER_BOUND ( 'NONE', #53634, .T. ) ;
#103783 = DIRECTION ( 'NONE',  ( 0.5735764363510468256, 0.8191520442889913545, 0.000000000000000000 ) ) ;
#103784 = CARTESIAN_POINT ( 'NONE',  ( -55.48269212579123888, -60.00000000000000711, 86.66456991474446170 ) ) ;
#103785 = CARTESIAN_POINT ( 'NONE',  ( -4.424031367838773932, 4.951337798340085250, -6.056431503345439005 ) ) ;
#103786 = CYLINDRICAL_SURFACE ( 'NONE', #51106, 4.000000000000000000 ) ;
#103787 = CARTESIAN_POINT ( 'NONE',  ( -65.26738680890619548, 48.00000000000000000, 0.8120011905346659065 ) ) ;
#103788 = CARTESIAN_POINT ( 'NONE',  ( -86.37828719965159507, -20.94065575718939698, 181.4663392420019363 ) ) ;
#103789 = AXIS2_PLACEMENT_3D ( 'NONE', #376, #26346, #59207 ) ;
#103790 = ORIENTED_EDGE ( 'NONE', *, *, #4122, .F. ) ;
#103791 = CARTESIAN_POINT ( 'NONE',  ( 35.72263983187427527, 379.3987609744327187, 4.779922119910973599 ) ) ;
#103792 = DIRECTION ( 'NONE',  ( -1.000000000000000000, -0.000000000000000000, -0.000000000000000000 ) ) ;
#103793 = CARTESIAN_POINT ( 'NONE',  ( -5.701072573891631912, 41.97507564787665757, -59.34341760267744803 ) ) ;
#103794 = CARTESIAN_POINT ( 'NONE',  ( 34.12349128637390550, 490.8027302422246407, 11.84948222508928062 ) ) ;
#103795 = CARTESIAN_POINT ( 'NONE',  ( 11.94619295074513410, -4.803972694421123180, -76.87644205112506768 ) ) ;
#103796 = ADVANCED_FACE ( 'NONE', ( #89819 ), #95789, .F. ) ;
#103797 = CARTESIAN_POINT ( 'NONE',  ( -82.42414396666261212, -45.26226855185817044, -15.39094701099094387 ) ) ;
#103798 = VECTOR ( 'NONE', #81947, 1000.000000000000000 ) ;
#103799 = FACE_OUTER_BOUND ( 'NONE', #7294, .T. ) ;
#103800 = LINE ( 'NONE', #30471, #46550 ) ;
#103801 = ORIENTED_EDGE ( 'NONE', *, *, #45141, .F. ) ;
#103802 = AXIS2_PLACEMENT_3D ( 'NONE', #44849, #36256, #20620 ) ;
#103803 = EDGE_CURVE ( 'NONE', #102776, #10296, #36378, .T. ) ;
#103804 = CARTESIAN_POINT ( 'NONE',  ( -3.750000000000004441, -6.495190528383288253, 1.734723475976807094E-15 ) ) ;
#103805 = CARTESIAN_POINT ( 'NONE',  ( -35.81121297974355144, 464.1169797044130974, 19.43538228465078177 ) ) ;
#103806 = CARTESIAN_POINT ( 'NONE',  ( 86.74683449613482367, -14.21045842199431242, 20.02856677177719646 ) ) ;
#103807 = CARTESIAN_POINT ( 'NONE',  ( -77.21040881692944424, -53.37756037490176908, 143.0221096505717071 ) ) ;
#103808 = ORIENTED_EDGE ( 'NONE', *, *, #102113, .T. ) ;
#103809 = DIRECTION ( 'NONE',  ( -1.000000000000000000, -1.224606353822377258E-16, -0.000000000000000000 ) ) ;
#103810 = CARTESIAN_POINT ( 'NONE',  ( -6.158268339717665185E-14, -15.58845726811991739, -11.79422863405993382 ) ) ;
#103811 = CARTESIAN_POINT ( 'NONE',  ( 81.34140718358432309, -57.51511421472552144, 200.0314531987298210 ) ) ;
#103812 =( REPRESENTATION_RELATIONSHIP ('NONE','NONE', #69581, #58557 ) REPRESENTATION_RELATIONSHIP_WITH_TRANSFORMATION ( #651 )SHAPE_REPRESENTATION_RELATIONSHIP( ) );
#103813 = CARTESIAN_POINT ( 'NONE',  ( 56.71111273679790088, 49.99999999999999289, 27.46638368304382993 ) ) ;
#103814 = UNCERTAINTY_MEASURE_WITH_UNIT (LENGTH_MEASURE( 1.000000000000000082E-05 ), #16698, 'distance_accuracy_value', 'NONE');
#103815 = CARTESIAN_POINT ( 'NONE',  ( 37.63019879891060526, 304.9912133630514859, -7.664751180836238298 ) ) ;
#103816 = DIRECTION ( 'NONE',  ( -1.000000000000000000, -1.224606353822377258E-16, -0.000000000000000000 ) ) ;
#103817 = ORIENTED_EDGE ( 'NONE', *, *, #3335, .F. ) ;
#103818 = DIRECTION ( 'NONE',  ( 0.000000000000000000, 1.000000000000000000, 0.000000000000000000 ) ) ;
#103819 = CARTESIAN_POINT ( 'NONE',  ( -14.75116209839011994, 43.55504285526384933, -90.22050492866908655 ) ) ;
#103820 = CARTESIAN_POINT ( 'NONE',  ( -7.188101187500000044, -24.40625000204838813, -8.802885111219163269E-16 ) ) ;
#103821 = ORIENTED_EDGE ( 'NONE', *, *, #46663, .F. ) ;
#103822 = CARTESIAN_POINT ( 'NONE',  ( 0.000000000000000000, 195.0000000000000000, 0.000000000000000000 ) ) ;
#103823 = MECHANICAL_DESIGN_GEOMETRIC_PRESENTATION_REPRESENTATION (  '', ( #15971 ), #95220 ) ;
#103824 = CARTESIAN_POINT ( 'NONE',  ( 11.08349330513380160, 1.593028355512270567E-15, 0.000000000000000000 ) ) ;
#103825 = CARTESIAN_POINT ( 'NONE',  ( 8.331345277524542681, 0.000000000000000000, -8.000000000000000000 ) ) ;
#103826 = EDGE_CURVE ( 'NONE', #13133, #58498, #1843, .T. ) ;
#103827 = CARTESIAN_POINT ( 'NONE',  ( 82.42421628608209971, 1.030564683017419500E-14, 0.000000000000000000 ) ) ;
#103828 = CARTESIAN_POINT ( 'NONE',  ( 6.931097425531398848, -13.59559899332509225, -6.365431243532045258 ) ) ;
#103829 = LINE ( 'NONE', #88189, #87446 ) ;
#103830 = ORIENTED_EDGE ( 'NONE', *, *, #56773, .F. ) ;
#103831 = CARTESIAN_POINT ( 'NONE',  ( -7.036764705882398552, 40.00000000007573675, -71.06385277390853616 ) ) ;
#103833 = CARTESIAN_POINT ( 'NONE',  ( 27.75406281153830435, -49.90938140761433317, 34.23113296838447894 ) ) ;
#103832 = CARTESIAN_POINT ( 'NONE',  ( -67.91869938964059372, -14.21045842199436571, 108.3284777829519214 ) ) ;
#103834 = CARTESIAN_POINT ( 'NONE',  ( 24.29723907929104598, 27.70462894893681494, -31.30642834101323047 ) ) ;
#103835 = ORIENTED_EDGE ( 'NONE', *, *, #71011, .T. ) ;
#103836 = EDGE_CURVE ( 'NONE', #36200, #52034, #51932, .T. ) ;
#103837 = VERTEX_POINT ( 'NONE', #57420 ) ;
#103838 = CARTESIAN_POINT ( 'NONE',  ( -22.67073868809948678, -4.285714285714296246, -11.17734400176827769 ) ) ;
#103839 = CARTESIAN_POINT ( 'NONE',  ( 111.8964183755431918, 22.97884757028484870, -55.94820918777157459 ) ) ;
#103840 = CARTESIAN_POINT ( 'NONE',  ( -12.13034742782427955, 48.00000000000000000, -93.82352941176471006 ) ) ;
#103841 = SURFACE_SIDE_STYLE ('',( #88730 ) ) ;
#103842 = CYLINDRICAL_SURFACE ( 'NONE', #60716, 6.999999999999992895 ) ;
#103843 = ORIENTED_EDGE ( 'NONE', *, *, #91217, .F. ) ;
#103844 = EDGE_CURVE ( 'NONE', #23955, #19635, #37803, .T. ) ;
#103845 = CARTESIAN_POINT ( 'NONE',  ( 17.50000000000002132, 47.99999999999999289, 64.09953197957062798 ) ) ;
#103846 = CARTESIAN_POINT ( 'NONE',  ( 85.46602935900409648, -29.99999999999995026, 174.5920392183242029 ) ) ;
#103847 = CARTESIAN_POINT ( 'NONE',  ( -13.58269433839552676, 24.75340072303480810, 0.6690760600839953387 ) ) ;
#103848 = CARTESIAN_POINT ( 'NONE',  ( 2.377971153322278042E-07, -60.00000000000000000, 39.63907915656436387 ) ) ;
#103849 = CARTESIAN_POINT ( 'NONE',  ( 81.59427637599597460, -29.99999999999999645, -6.810622583152962761 ) ) ;
#103850 = DIRECTION ( 'NONE',  ( -1.000000000000000000, -1.224606353822377258E-16, -0.000000000000000000 ) ) ;
#103851 = EDGE_CURVE ( 'NONE', #37257, #14360, #48461, .T. ) ;
#103852 = ORIENTED_EDGE ( 'NONE', *, *, #76182, .T. ) ;
#103853 = VERTEX_POINT ( 'NONE', #9946 ) ;
#103854 = ORIENTED_EDGE ( 'NONE', *, *, #19931, .F. ) ;
#103855 = CARTESIAN_POINT ( 'NONE',  ( -13.50000000000000000, 7.794228634059933825, -1.205771365940051520 ) ) ;
#103856 = PLANE ( 'NONE',  #38018 ) ;
#103857 = CARTESIAN_POINT ( 'NONE',  ( -7.550180524134850302, -88.00559247213188030, 2.651855549982492732 ) ) ;
#103858 = LINE ( 'NONE', #22455, #94976 ) ;
#103859 = ORIENTED_EDGE ( 'NONE', *, *, #31985, .T. ) ;
#103860 = CARTESIAN_POINT ( 'NONE',  ( 43.03185303983483578, 485.3613526602390493, 6.073233449168488285 ) ) ;
#103861 = ORIENTED_EDGE ( 'NONE', *, *, #86141, .F. ) ;
#103862 = CARTESIAN_POINT ( 'NONE',  ( 42.40769230769231513, 1.411358822780289120E-15, 0.000000000000000000 ) ) ;
#103863 = CARTESIAN_POINT ( 'NONE',  ( 60.67466929282835508, -38.34223859905504384, 98.54665191328351170 ) ) ;
#103864 = CARTESIAN_POINT ( 'NONE',  ( -40.67924138885464913, 485.8013567632088439, -4.837443355060405459 ) ) ;
#103865 = AXIS2_PLACEMENT_3D ( 'NONE', #42003, #33952, #50604 ) ;
#103866 = CARTESIAN_POINT ( 'NONE',  ( 6.289572920342629381, -5.584521518880467106, -3.985288806461540823 ) ) ;
#103867 = CARTESIAN_POINT ( 'NONE',  ( 64.12946791427296489, -32.52996445180959029, 80.08306847456309185 ) ) ;
#103868 = AXIS2_PLACEMENT_3D ( 'NONE', #92779, #67981, #50701 ) ;
#103869 = ORIENTED_EDGE ( 'NONE', *, *, #26486, .F. ) ;
#103870 = CARTESIAN_POINT ( 'NONE',  ( -48.02835407290534420, -1.200000000000000030E-05, -14.35535821593460248 ) ) ;
#103871 = CARTESIAN_POINT ( 'NONE',  ( -63.92463504160575383, -37.78188829957583295, -33.13005288218677435 ) ) ;
#103872 = VECTOR ( 'NONE', #33771, 1000.000000000000000 ) ;
#103873 = CARTESIAN_POINT ( 'NONE',  ( -6.984140731825568160, 9.027579208887587470, -0.5385323539060862252 ) ) ;
#103874 = CARTESIAN_POINT ( 'NONE',  ( 0.000000000000000000, -1.341159125180006795, 0.000000000000000000 ) ) ;
#103875 = EDGE_CURVE ( 'NONE', #90268, #37125, #11770, .T. ) ;
#103876 = EDGE_LOOP ( 'NONE', ( #31591, #102136, #36481 ) ) ;
#103877 = LINE ( 'NONE', #62387, #95358 ) ;
#103878 = B_SPLINE_CURVE_WITH_KNOTS ( 'NONE', 3,
 ( #55880, #80706, #106038, #48338 ),
 .UNSPECIFIED., .F., .F.,
 ( 4, 4 ),
 ( 0.000000000000000000, 0.001748759895725735458 ),
 .UNSPECIFIED. ) ;
#103879 = CARTESIAN_POINT ( 'NONE',  ( 30.62829732754926582, -60.00000000000002842, -35.06421439060901690 ) ) ;
#103880 = AXIS2_PLACEMENT_3D ( 'NONE', #25362, #105706, #31848 ) ;
#103881 = ADVANCED_FACE ( 'NONE', ( #59585 ), #38203, .T. ) ;
#103882 = CARTESIAN_POINT ( 'NONE',  ( 60.63333333333333286, 3.309500000000014541, 4.052968581778174646E-16 ) ) ;
#103883 = CARTESIAN_POINT ( 'NONE',  ( 5.656854249492380582, -29.00000000409677270, -5.656854249492379694 ) ) ;
#103884 = CARTESIAN_POINT ( 'NONE',  ( 6.725979247667768668, 3.622307570260303144, -6.470294263593357798 ) ) ;
#103885 = CARTESIAN_POINT ( 'NONE',  ( 86.89257692234927788, -42.78194120415572144, 189.7856798060613528 ) ) ;
#103886 = CARTESIAN_POINT ( 'NONE',  ( -5.272286809540803532, 14.23042150740707079, -34.01614571496379114 ) ) ;
#103887 = B_SPLINE_CURVE_WITH_KNOTS ( 'NONE', 3,
 ( #66930, #23841, #17322, #24888, #90664, #15703, #48591, #83099, #50707, #83619, #42639, #75536, #81480, #106293, #73392, #92238 ),
 .UNSPECIFIED., .F., .F.,
 ( 4, 2, 2, 2, 2, 2, 2, 4 ),
 ( 9.697399036122160616E-19, 0.001212534658637846657, 0.002425069317275692447, 0.004850138634551384026, 0.006062673293189230032, 0.007275207951827075172, 0.008487742610464922913, 0.009700277269102768052 ),
 .UNSPECIFIED. ) ;
#103888 = CARTESIAN_POINT ( 'NONE',  ( -8.826886570201967430, 18.27301070672071148, 4.999999999999999112 ) ) ;
#103889 = EDGE_CURVE ( 'NONE', #3192, #67680, #34800, .T. ) ;
#103892 = EDGE_CURVE ( 'NONE', #20022, #76857, #29586, .T. ) ;
#103891 = AXIS2_PLACEMENT_3D ( 'NONE', #27398, #43004, #51611 ) ;
#103890 = CARTESIAN_POINT ( 'NONE',  ( 27.88494491742561721, -20.99829245791718790, -32.55451976490055443 ) ) ;
#103893 = CARTESIAN_POINT ( 'NONE',  ( -2.019483917365790222E-25, 304.8518027762758038, 8.936999415352287812 ) ) ;
#103894 = EDGE_LOOP ( 'NONE', ( #87898, #72668, #62956, #58065, #24811, #45995, #64299, #76263, #12502, #84527, #70554 ) ) ;
#103895 = CARTESIAN_POINT ( 'NONE',  ( 13.95266368664216294, -50.20567487918883387, 25.82453759514263680 ) ) ;
#103896 = DIRECTION ( 'NONE',  ( 0.000000000000000000, 0.000000000000000000, -1.000000000000000000 ) ) ;
#103897 = VECTOR ( 'NONE', #42299, 1000.000000000000227 ) ;
#103898 = CARTESIAN_POINT ( 'NONE',  ( -99.15767263151849420, -29.99999999999998934, 188.4520339999081671 ) ) ;
#103899 = MECHANICAL_DESIGN_GEOMETRIC_PRESENTATION_REPRESENTATION (  '', ( #60811 ), #95295 ) ;
#103900 = DIRECTION ( 'NONE',  ( -0.000000000000000000, -0.000000000000000000, -1.000000000000000000 ) ) ;
#103901 = CARTESIAN_POINT ( 'NONE',  ( 32.03033611666798919, -57.68913864069202191, 46.57911711074292782 ) ) ;
#103903 = FILL_AREA_STYLE_COLOUR ( '', #82623 ) ;
#103902 = CARTESIAN_POINT ( 'NONE',  ( 10.11927453338527094, 43.29088567661159459, 15.40779740156148669 ) ) ;
#103904 = CARTESIAN_POINT ( 'NONE',  ( -38.82095410878641673, 477.1411610313862752, -1.685344478752615727 ) ) ;
#103905 = CARTESIAN_POINT ( 'NONE',  ( -18.38921465765557173, 50.00000000000000000, 61.39959187812481645 ) ) ;
#103906 = SURFACE_SIDE_STYLE ('',( #38665 ) ) ;
#103907 = DIRECTION ( 'NONE',  ( 1.000000000000000000, 1.224606353822377258E-16, 0.000000000000000000 ) ) ;
#103908 = CARTESIAN_POINT ( 'NONE',  ( 92.53532739719321398, 1.030564683017419500E-14, 0.000000000000000000 ) ) ;
#103909 = PRESENTATION_STYLE_ASSIGNMENT (( #32041 ) ) ;
#103910 = FACE_OUTER_BOUND ( 'NONE', #37406, .T. ) ;
#103911 = ORIENTED_EDGE ( 'NONE', *, *, #63635, .T. ) ;
#103912 = CARTESIAN_POINT ( 'NONE',  ( 40.86966971611426658, 485.5857298029578146, -4.179518346805715545 ) ) ;
#103913 = CARTESIAN_POINT ( 'NONE',  ( 21.08349330513380693, 4.898587196589411843E-16, -4.000000000000001776 ) ) ;
#103914 = CARTESIAN_POINT ( 'NONE',  ( -14.34294123642693997, -25.55009647558605224, 28.25866928844338588 ) ) ;
#103916 = CARTESIAN_POINT ( 'NONE',  ( 39.45725925859274952, 460.7192990590706927, 2.112476274834731882 ) ) ;
#103915 = CARTESIAN_POINT ( 'NONE',  ( -106.1474143027046324, -59.99999999999999289, 180.7708242920181476 ) ) ;
#103917 = EDGE_CURVE ( 'NONE', #86142, #28378, #82906, .T. ) ;
#103918 = EDGE_LOOP ( 'NONE', ( #18594, #32778, #32195, #23088, #31922, #54168 ) ) ;
#103919 = B_SPLINE_CURVE_WITH_KNOTS ( 'NONE', 3,
 ( #88719, #72523, #73569, #14810 ),
 .UNSPECIFIED., .F., .F.,
 ( 4, 4 ),
 ( 0.000000000000000000, 0.0008765341530664233537 ),
 .UNSPECIFIED. ) ;
#103920 = DIRECTION ( 'NONE',  ( 0.000000000000000000, -1.000000000000000000, 0.000000000000000000 ) ) ;
#103921 = CARTESIAN_POINT ( 'NONE',  ( -13.18841494988442342, 42.68946335806984393, -92.36892705870020848 ) ) ;
#103922 = EDGE_CURVE ( 'NONE', #39827, #53391, #89834, .T. ) ;
#103923 = CARTESIAN_POINT ( 'NONE',  ( 15.94091178690282362, 3.082798537041105291, -0.3736180972855698834 ) ) ;
#103924 = CARTESIAN_POINT ( 'NONE',  ( 72.06213202562246067, -59.99999999999999289, 154.7422713602608724 ) ) ;
#103925 = CARTESIAN_POINT ( 'NONE',  ( -44.66387834505498944, 341.6072687625629101, 1.189588019127773677 ) ) ;
#103926 = ORIENTED_EDGE ( 'NONE', *, *, #4137, .T. ) ;
#103927 = CARTESIAN_POINT ( 'NONE',  ( 32.17889379758945267, 439.3695696554025858, 23.63219374846805465 ) ) ;
#103928 = CARTESIAN_POINT ( 'NONE',  ( 4.898587196589412829E-16, -21.31250000409676915, -8.000000000000000000 ) ) ;
#103929 = AXIS2_PLACEMENT_3D ( 'NONE', #50487, #83399, #9497 ) ;
#103931 = CARTESIAN_POINT ( 'NONE',  ( 4.250000000000000000, 0.000000000000000000, -3.393184225085859929 ) ) ;
#103930 = CARTESIAN_POINT ( 'NONE',  ( 51.84565611112584804, -38.00000000000000711, 53.44666998630373911 ) ) ;
#103932 = CARTESIAN_POINT ( 'NONE',  ( 0.000000000000000000, -2.000000000000000000, 0.000000000000000000 ) ) ;
#103933 =( LENGTH_UNIT ( ) NAMED_UNIT ( * ) SI_UNIT ( .MILLI., .METRE. ) );
#103934 = VERTEX_POINT ( 'NONE', #74142 ) ;
#103935 = CIRCLE ( 'NONE', #103868, 3.309500000000007880 ) ;
#103936 = ORIENTED_EDGE ( 'NONE', *, *, #90136, .T. ) ;
#103937 = CARTESIAN_POINT ( 'NONE',  ( -27.53978464381656366, 314.0199944737697137, 12.16771398945173566 ) ) ;
#103938 = PRESENTATION_LAYER_ASSIGNMENT (  '', '', ( #43665 ) ) ;
#103939 = ORIENTED_EDGE ( 'NONE', *, *, #27784, .F. ) ;
#103940 = CARTESIAN_POINT ( 'NONE',  ( 48.10000000000000142, 4.475777889183788807E-16, -3.309499999999999886 ) ) ;
#103941 = ORIENTED_EDGE ( 'NONE', *, *, #41028, .F. ) ;
#103942 = EDGE_CURVE ( 'NONE', #31195, #45709, #50162, .T. ) ;
#103943 = CARTESIAN_POINT ( 'NONE',  ( -5.700736385538761830, 42.00193813219923555, -69.19507739564853921 ) ) ;
#103944 = B_SPLINE_CURVE_WITH_KNOTS ( 'NONE', 3,
 ( #44788, #3787, #39868, #82443, #65733, #81891, #32323, #80836 ),
 .UNSPECIFIED., .F., .F.,
 ( 4, 2, 2, 4 ),
 ( 0.000000000000000000, 0.0002399520006080664222, 0.0004799040012161328445, 0.0009598080024322654721 ),
 .UNSPECIFIED. ) ;
#103945 = CARTESIAN_POINT ( 'NONE',  ( -90.78562293538325889, -60.00000000002675904, 204.6252288958342263 ) ) ;
#103946 = CARTESIAN_POINT ( 'NONE',  ( 46.00000000000000711, 485.7857398469772647, -0.3390537564248662927 ) ) ;
#103947 = CARTESIAN_POINT ( 'NONE',  ( 72.43113064393337197, -59.99999999999998579, 157.5155133769252416 ) ) ;
#103948 = DIRECTION ( 'NONE',  ( 0.2776092459786534405, 0.06763270420356301549, -0.9583104527601048472 ) ) ;
#103949 = CARTESIAN_POINT ( 'NONE',  ( -6.263552781412762727, 41.61160193526471573, -58.64895252977191120 ) ) ;
#103950 = VECTOR ( 'NONE', #14971, 1000.000000000000000 ) ;
#103952 = CARTESIAN_POINT ( 'NONE',  ( 11.24629686663563888, -32.51060762582239505, 29.33386000569823793 ) ) ;
#103951 = CARTESIAN_POINT ( 'NONE',  ( -99.89444227931625164, -30.00000000000003197, 96.08249125629401988 ) ) ;
#103953 = FILL_AREA_STYLE ('',( #71578 ) ) ;
#103954 = CARTESIAN_POINT ( 'NONE',  ( -48.56021830926045624, -18.75688510409356979, 42.04449221851854901 ) ) ;
#103955 = CARTESIAN_POINT ( 'NONE',  ( -6.831363903021533623, 41.73171925724633979, -59.17722475679354233 ) ) ;
#103956 = ORIENTED_EDGE ( 'NONE', *, *, #5200, .F. ) ;
#103957 = CARTESIAN_POINT ( 'NONE',  ( 36.64823341582350480, 437.5392299810053487, 4.281405873620231617 ) ) ;
#103958 = CARTESIAN_POINT ( 'NONE',  ( 0.000000000000000000, 0.000000000000000000, -7.974599999999995248 ) ) ;
#103959 = SURFACE_STYLE_USAGE ( .BOTH. , #105557 ) ;
#103960 = VERTEX_POINT ( 'NONE', #12071 ) ;
#103961 = CARTESIAN_POINT ( 'NONE',  ( -8.239527348356862291, -12.24602314337617059, 8.669075505165368511 ) ) ;
#103962 = VERTEX_POINT ( 'NONE', #61178 ) ;
#103963 = CARTESIAN_POINT ( 'NONE',  ( 90.70307972239879746, -30.00000000003412381, 199.4269904992890758 ) ) ;
#103964 = FILL_AREA_STYLE ('',( #22020 ) ) ;
#103965 =( GEOMETRIC_REPRESENTATION_CONTEXT ( 3 ) GLOBAL_UNCERTAINTY_ASSIGNED_CONTEXT ( ( #9511 ) ) GLOBAL_UNIT_ASSIGNED_CONTEXT ( ( #65286, #9157, #31368 ) ) REPRESENTATION_CONTEXT ( 'NONE', 'WORKASPACE' ) );
#103966 = CARTESIAN_POINT ( 'NONE',  ( 5.902962692465450800, 41.87327339699978523, -59.02279353628206593 ) ) ;
#103967 = CARTESIAN_POINT ( 'NONE',  ( 10.04205104294044482, 18.64316884711816513, -37.36680950588930727 ) ) ;
#103968 = CARTESIAN_POINT ( 'NONE',  ( 99.07418092138790655, -30.00000000000000000, 188.6523126474757532 ) ) ;
#103969 = CIRCLE ( 'NONE', #76406, 4.000000000000002665 ) ;
#103970 = DIRECTION ( 'NONE',  ( 0.000000000000000000, -0.3420201433256727652, -0.9396926207859068736 ) ) ;
#103971 = EDGE_CURVE ( 'NONE', #89440, #27308, #78435, .T. ) ;
#103972 = ORIENTED_EDGE ( 'NONE', *, *, #78158, .T. ) ;
#103973 = CIRCLE ( 'NONE', #57453, 3.000000000000020872 ) ;
#103974 = ORIENTED_EDGE ( 'NONE', *, *, #75429, .F. ) ;
#103975 = ORIENTED_EDGE ( 'NONE', *, *, #106108, .T. ) ;
#103977 = CARTESIAN_POINT ( 'NONE',  ( 12.21253585067004543, 1.340359594676612611E-15, 0.000000000000000000 ) ) ;
#103976 = COLOUR_RGB ( '', 0.31764706, 0.68627451, 0.89019608) ;
#103978 = CARTESIAN_POINT ( 'NONE',  ( -46.00000000000000000, 438.3644743595980344, 10.24495404218449757 ) ) ;
#103979 = DIRECTION ( 'NONE',  ( -1.000000000000000000, -1.224606353822377258E-16, -0.000000000000000000 ) ) ;
#103980 = ORIENTED_EDGE ( 'NONE', *, *, #1973, .T. ) ;
#103981 = CARTESIAN_POINT ( 'NONE',  ( -16.01235146068397697, 3.721755040407972892, -0.3223148954708403013 ) ) ;
#103982 = ORIENTED_EDGE ( 'NONE', *, *, #29125, .F. ) ;
#103983 = CARTESIAN_POINT ( 'NONE',  ( 0.000000000000000000, 8.660254037844390851, -0.9999999999999974465 ) ) ;
#103984 = CARTESIAN_POINT ( 'NONE',  ( 105.2440405677593276, -38.38944072604935798, 197.2348950601119668 ) ) ;
#103985 = CARTESIAN_POINT ( 'NONE',  ( 11.81070278343545610, 6.722221634647634225, 9.055894994455341518 ) ) ;
#103986 = CARTESIAN_POINT ( 'NONE',  ( 85.00044501559656851, -52.70739042385801554, 7.105829972696751540 ) ) ;
#103987 = CARTESIAN_POINT ( 'NONE',  ( -4.999999999999999112, 0.000000000000000000, 35.66025403784438197 ) ) ;
#103988 = CARTESIAN_POINT ( 'NONE',  ( 33.16871688984772959, 397.1242636821970677, 25.83017931078799734 ) ) ;
#103989 = CARTESIAN_POINT ( 'NONE',  ( 7.808623696107298784, 4.508310992947659024, -7.999704684617482187 ) ) ;
#103990 = CARTESIAN_POINT ( 'NONE',  ( -39.08187240373793969, 460.7913535929719728, 2.155912156267088875 ) ) ;
#103991 = FILL_AREA_STYLE ('',( #95385 ) ) ;
#103992 = ORIENTED_EDGE ( 'NONE', *, *, #13536, .T. ) ;
#103993 = CARTESIAN_POINT ( 'NONE',  ( -12.34835181856066555, -4.332967528434497062, -12.86601580078907148 ) ) ;
#103994 = EDGE_CURVE ( 'NONE', #35302, #337, #15758, .T. ) ;
#103995 = CARTESIAN_POINT ( 'NONE',  ( 7.500000000000007105, -3.000000000000000000, -68.91429205785459544 ) ) ;
#103996 = CARTESIAN_POINT ( 'NONE',  ( -26.10555842523061898, 37.18665756854946380, 8.037934041381376460 ) ) ;
#103997 = ORIENTED_EDGE ( 'NONE', *, *, #32973, .F. ) ;
#103998 = CARTESIAN_POINT ( 'NONE',  ( 4.898587196589412829E-16, -16.81250000409677270, -8.000000000000000000 ) ) ;
#103999 = CARTESIAN_POINT ( 'NONE',  ( -31.19627331860082720, 299.4406361361442350, 10.96598005625576100 ) ) ;
#104000 = DIRECTION ( 'NONE',  ( 0.000000000000000000, -1.000000000000000000, 0.000000000000000000 ) ) ;
#104001 = FILL_AREA_STYLE_COLOUR ( '', #64501 ) ;
#104002 = CARTESIAN_POINT ( 'NONE',  ( 8.000000000000000000, -12.40624999999999289, -3.313708498984761608 ) ) ;
#104003 = CARTESIAN_POINT ( 'NONE',  ( -40.11045082424308816, -37.66163030632180408, 50.00889850192834274 ) ) ;
#104004 = ADVANCED_FACE ( 'NONE', ( #20764 ), #93299, .T. ) ;
#104005 = LINE ( 'NONE', #87316, #10570 ) ;
#104006 = PRESENTATION_LAYER_ASSIGNMENT (  '', '', ( #90237 ) ) ;
#104007 = ORIENTED_EDGE ( 'NONE', *, *, #9325, .T. ) ;
#104008 = CARTESIAN_POINT ( 'NONE',  ( 84.74745017207317233, -42.96139324155009831, 184.9190875993280656 ) ) ;
#104009 = CARTESIAN_POINT ( 'NONE',  ( -48.28084718957928345, 9.217476947337136295, 16.83779905917586817 ) ) ;
#104010 = CARTESIAN_POINT ( 'NONE',  ( 30.00000000000000000, 500.0000000000002274, 5.000000000000001776 ) ) ;
#104011 = EDGE_LOOP ( 'NONE', ( #92289, #105337, #68093, #42300 ) ) ;
#104012 = CIRCLE ( 'NONE', #45445, 5.000000000000010658 ) ;
#104013 = CARTESIAN_POINT ( 'NONE',  ( 94.19019775188388621, -57.67257497933957922, 22.53043024018837315 ) ) ;
#104014 = EDGE_CURVE ( 'NONE', #96544, #59570, #18098, .T. ) ;
#104015 = CARTESIAN_POINT ( 'NONE',  ( 35.73700087854440000, 437.1201388800395193, 4.567739269147286230 ) ) ;
#104016 = CARTESIAN_POINT ( 'NONE',  ( 6.876313068639422710, -4.333298119783811408, 16.54772121370670135 ) ) ;
#104017 = CARTESIAN_POINT ( 'NONE',  ( 29.49619080111450131, 13.37262004692844464, 39.61417171781327795 ) ) ;
#104018 = AXIS2_PLACEMENT_3D ( 'NONE', #4871, #71186, #62584 ) ;
#104019 = ORIENTED_EDGE ( 'NONE', *, *, #25665, .F. ) ;
#104020 = DIRECTION ( 'NONE',  ( 0.000000000000000000, 0.000000000000000000, 1.000000000000000000 ) ) ;
#104021 = CARTESIAN_POINT ( 'NONE',  ( 36.08349330513379982, 1.593028355512270567E-15, 0.000000000000000000 ) ) ;
#104022 = CARTESIAN_POINT ( 'NONE',  ( 3.677584134044427078, -1.015418994119225760, 104.5297932675492234 ) ) ;
#104023 = CARTESIAN_POINT ( 'NONE',  ( 36.18613319579441878, -24.61962019850594885, 33.95388689007886285 ) ) ;
#104025 = FILL_AREA_STYLE_COLOUR ( '', #77479 ) ;
#104024 = SURFACE_STYLE_FILL_AREA ( #12885 ) ;
#104026 = CARTESIAN_POINT ( 'NONE',  ( 42.19618372163381537, 487.7264399052799035, 8.629926728122860879 ) ) ;
#104027 = DIRECTION ( 'NONE',  ( -1.000000000000000000, 0.000000000000000000, 0.000000000000000000 ) ) ;
#104028 = VERTEX_POINT ( 'NONE', #28848 ) ;
#104029 = CARTESIAN_POINT ( 'NONE',  ( -33.85941220253381800, -31.37761359142308137, -29.86486766534904902 ) ) ;
#104030 = DIRECTION ( 'NONE',  ( 0.000000000000000000, 1.000000000000000000, 0.000000000000000000 ) ) ;
#104031 = CARTESIAN_POINT ( 'NONE',  ( -83.17519967775672285, -38.00000000000002132, -9.623065349217405640 ) ) ;
#104032 = CONICAL_SURFACE ( 'NONE', #45554, 4.000000000000001776, 0.9599310885968774798 ) ;
#104033 = ORIENTED_EDGE ( 'NONE', *, *, #31292, .T. ) ;
#104034 = CARTESIAN_POINT ( 'NONE',  ( -9.620303054984660207, -0.5026337155641874554, 19.91726907925657386 ) ) ;
#104035 = FACE_OUTER_BOUND ( 'NONE', #102926, .T. ) ;
#104036 = CARTESIAN_POINT ( 'NONE',  ( 16.33361799548379523, 1.482358050883964840E-15, 0.000000000000000000 ) ) ;
#104037 =( BOUNDED_SURFACE ( )  B_SPLINE_SURFACE ( 3, 2, ( 
 ( #26426, #92165, #10186 ),
 ( #100788, #26950, #18312 ),
 ( #43099, #75987, #59827 ),
 ( #92702, #18861, #51704 ),
 ( #84623, #5302, #47332 ),
 ( #79176, #30659, #55414 ),
 ( #29606, #4232, #86238 ),
 ( #6330, #63008, #61963 ),
 ( #103978, #62478, #13363 ),
 ( #30118, #78631, #39272 ) ),
 .UNSPECIFIED., .F., .F., .F. ) 
 B_SPLINE_SURFACE_WITH_KNOTS ( ( 4, 2, 2, 2, 4 ),
 ( 3, 3 ),
 ( 0.007286154432480420814, 0.008335500519278869064, 0.009384846606077319048, 0.01043419269287576730, 0.01148353877967421555 ),
 ( 0.000000000000000000, 0.8533017117288693720 ),
 .UNSPECIFIED. ) 
 GEOMETRIC_REPRESENTATION_ITEM ( )  RATIONAL_B_SPLINE_SURFACE ( (
 ( 1.000000000000000000, 0.8072324461154417596, 0.9434426596218448147),
 ( 1.000000000000000000, 0.8170226563706388667, 0.9463150737943484270),
 ( 1.000000000000000000, 0.8232679997191755250, 0.9481474361521402550),
 ( 1.000000000000000000, 0.8276101782779371474, 0.9494214164760159669),
 ( 1.000000000000000000, 0.8256847820051311793, 0.9488565118010874322),
 ( 1.000000000000000000, 0.8144349657408164189, 0.9455558542224080654),
 ( 1.000000000000000000, 0.8051540590290614530, 0.9428328679659709888),
 ( 1.000000000000000000, 0.7811619758966467097, 0.9357936729108033980),
 ( 1.000000000000000000, 0.7664691029299778302, 0.9314828342828123109),
 ( 1.000000000000000000, 0.7500737150327089209, 0.9266724836026711820) ) ) 
 REPRESENTATION_ITEM ( '' )  SURFACE ( )  );
#104039 = CARTESIAN_POINT ( 'NONE',  ( -34.26200826892031870, -21.77016632158549569, -28.20174604461301016 ) ) ;
#104038 = CARTESIAN_POINT ( 'NONE',  ( 0.000000000000000000, -19.99999999999998934, 0.000000000000000000 ) ) ;
#104040 = ADVANCED_FACE ( 'NONE', ( #51998 ), #48762, .T. ) ;
#104041 = STYLED_ITEM ( 'NONE', ( #102975 ), #64127 ) ;
#104042 = ORIENTED_EDGE ( 'NONE', *, *, #87050, .F. ) ;
#104043 = VECTOR ( 'NONE', #34132, 1000.000000000000227 ) ;
#104044 = CARTESIAN_POINT ( 'NONE',  ( 5.174575781541514097, 5.672711317429273592, -7.030005583190789942 ) ) ;
#104045 = ORIENTED_EDGE ( 'NONE', *, *, #18891, .F. ) ;
#104046 = ADVANCED_FACE ( 'NONE', ( #72980 ), #47650, .F. ) ;
#104047 = EDGE_CURVE ( 'NONE', #52425, #28015, #42613, .T. ) ;
#104048 = CARTESIAN_POINT ( 'NONE',  ( 6.222742520105473574, 7.673830019007162662, -0.2914634815676393487 ) ) ;
#104049 = DIRECTION ( 'NONE',  ( 0.000000000000000000, 0.000000000000000000, -1.000000000000000000 ) ) ;
#104050 = CARTESIAN_POINT ( 'NONE',  ( -92.65510230062061225, -60.00000000000000000, -3.796815982375457477 ) ) ;
#104051 = ORIENTED_EDGE ( 'NONE', *, *, #91945, .T. ) ;
#104052 = CARTESIAN_POINT ( 'NONE',  ( 6.459123244420549526, 42.00000000000000000, -59.79223455627352735 ) ) ;
#104053 = CARTESIAN_POINT ( 'NONE',  ( 12.49986889690059222, -3.000000000000002665, -76.70852482682694529 ) ) ;
#104054 = CARTESIAN_POINT ( 'NONE',  ( -9.165151389911681434, 30.00000000000000000, -4.000000000000000000 ) ) ;
#104056 = LINE ( 'NONE', #79783, #49563 ) ;
#104055 = CARTESIAN_POINT ( 'NONE',  ( 0.000000000000000000, 0.000000000000000000, 0.000000000000000000 ) ) ;
#104057 = CARTESIAN_POINT ( 'NONE',  ( -81.73723767783293681, -49.95509653891984669, 174.6705688511061396 ) ) ;
#104058 = VERTEX_POINT ( 'NONE', #64912 ) ;
#104059 = CARTESIAN_POINT ( 'NONE',  ( -16.90652009647373077, -0.000000000000000000, -2.220657265743024134 ) ) ;
#104060 = ORIENTED_EDGE ( 'NONE', *, *, #43111, .T. ) ;
#104061 = ORIENTED_EDGE ( 'NONE', *, *, #69541, .T. ) ;
#104062 = CARTESIAN_POINT ( 'NONE',  ( 42.18756898894580587, 484.4522853017719513, -2.425645685620450909 ) ) ;
#104063 = CARTESIAN_POINT ( 'NONE',  ( -5.000000000000000000, -14.11573700085287442, 9.475244962101804447 ) ) ;
#104064 = VERTEX_POINT ( 'NONE', #55210 ) ;
#104065 = ADVANCED_FACE ( 'NONE', ( #105373 ), #83117, .T. ) ;
#104066 = MECHANICAL_DESIGN_GEOMETRIC_PRESENTATION_REPRESENTATION (  '', ( #30043 ), #24871 ) ;
#104067 = CARTESIAN_POINT ( 'NONE',  ( 15.56772955930212099, 46.04746595587301528, -6.065209611211576757 ) ) ;
#104068 = CARTESIAN_POINT ( 'NONE',  ( -9.999999999999960920, 15.00000000000001066, -3.836411046841922801 ) ) ;
#104069 = CARTESIAN_POINT ( 'NONE',  ( -82.32950074003311158, -57.52534511946047502, 200.7509962287250573 ) ) ;
#104070 = CARTESIAN_POINT ( 'NONE',  ( -43.97709758272682734, 485.9234630640621617, 4.765357662999615052 ) ) ;
#104071 = CARTESIAN_POINT ( 'NONE',  ( -18.91781669292785395, 48.00000000000000000, 62.18610382930904734 ) ) ;
#104072 = CARTESIAN_POINT ( 'NONE',  ( 3.750000000000004885, -6.495190528383287365, 1.734723475976807094E-15 ) ) ;
#104073 = CARTESIAN_POINT ( 'NONE',  ( -17.51117938516228634, 36.87948859581990035, -22.05134542098268113 ) ) ;
#104074 = CARTESIAN_POINT ( 'NONE',  ( 86.55961277372783513, -14.21045842199431597, 7.754469001180375187 ) ) ;
#104075 = EDGE_CURVE ( 'NONE', #56514, #35363, #36079, .T. ) ;
#104076 = CARTESIAN_POINT ( 'NONE',  ( -55.44100834966593538, -14.21045842199449361, 70.81055559928208254 ) ) ;
#104077 = CARTESIAN_POINT ( 'NONE',  ( -53.90679042101523777, -60.32124336610769433, 66.32078629646572665 ) ) ;
#104078 = VERTEX_POINT ( 'NONE', #2139 ) ;
#104079 = CARTESIAN_POINT ( 'NONE',  ( 6.984567718307133077, 16.97316992422711124, -0.5333114754527591428 ) ) ;
#104080 = CIRCLE ( 'NONE', #71363, 0.4000000000000001887 ) ;
#104081 = ORIENTED_EDGE ( 'NONE', *, *, #54906, .F. ) ;
#104082 = CARTESIAN_POINT ( 'NONE',  ( -99.83212472546227900, -45.25428798288277221, 192.7520070752582626 ) ) ;
#104083 = VECTOR ( 'NONE', #56412, 1000.000000000000000 ) ;
#104084 = CARTESIAN_POINT ( 'NONE',  ( -29.85995211472205213, 18.03913124950666003, -39.60535821593472861 ) ) ;
#104085 = ORIENTED_EDGE ( 'NONE', *, *, #79841, .T. ) ;
#104086 = CARTESIAN_POINT ( 'NONE',  ( 19.39022949357585546, 49.93247698687046210, 61.01543061342935914 ) ) ;
#104087 = PRESENTATION_LAYER_ASSIGNMENT (  '', '', ( #35220 ) ) ;
#104088 = CARTESIAN_POINT ( 'NONE',  ( 108.5726971398995886, -38.35682900653360150, 191.4692688943128474 ) ) ;
#104089 = SURFACE_STYLE_USAGE ( .BOTH. , #37816 ) ;
#104090 = CARTESIAN_POINT ( 'NONE',  ( -3.594029361870008099, -9.531975552773351623, 6.225090491531445558 ) ) ;
#104091 = DIRECTION ( 'NONE',  ( 0.000000000000000000, -1.000000000000000000, 0.000000000000000000 ) ) ;
#104092 = LINE ( 'NONE', #30232, #44690 ) ;
#104093 = CARTESIAN_POINT ( 'NONE',  ( -25.93947128054312756, 296.0094280503604978, 10.18659011856751384 ) ) ;
#104094 = CARTESIAN_POINT ( 'NONE',  ( -7.963455549596985428, 52.64303760444155955, -0.000000000000000000 ) ) ;
#104095 = CARTESIAN_POINT ( 'NONE',  ( 4.324717655747504885, -48.88831368632219210, 104.4045892612655990 ) ) ;
#104096 = FACE_OUTER_BOUND ( 'NONE', #3110, .T. ) ;
#104097 = UNCERTAINTY_MEASURE_WITH_UNIT (LENGTH_MEASURE( 1.000000000000000082E-05 ), #60796, 'distance_accuracy_value', 'NONE');
#104098 = CARTESIAN_POINT ( 'NONE',  ( -27.46968486408479393, -42.96035443980599666, 32.94799843992185373 ) ) ;
#104099 = VERTEX_POINT ( 'NONE', #35092 ) ;
#104100 = ORIENTED_EDGE ( 'NONE', *, *, #10839, .T. ) ;
#104101 = CARTESIAN_POINT ( 'NONE',  ( 47.91978359059700665, -53.35808289020361883, 51.77896845157469841 ) ) ;
#104102 = CARTESIAN_POINT ( 'NONE',  ( -0.3586650412126671794, 13.57975806887350245, 49.30105652963410989 ) ) ;
#104103 = CARTESIAN_POINT ( 'NONE',  ( 28.17977184163764193, 3.851859888774471706E-31, 5.000000000000001776 ) ) ;
#104104 = CARTESIAN_POINT ( 'NONE',  ( -110.8309764612567818, -38.35617722019826203, 166.2611764703423489 ) ) ;
#104105 = ORIENTED_EDGE ( 'NONE', *, *, #60303, .F. ) ;
#104106 = CARTESIAN_POINT ( 'NONE',  ( 91.36700694265483946, -38.39761548113196454, -9.638155343660422147 ) ) ;
#104107 = DIRECTION ( 'NONE',  ( 0.000000000000000000, -1.000000000000000000, 0.000000000000000000 ) ) ;
#104108 = CARTESIAN_POINT ( 'NONE',  ( 32.18412820475327862, 464.7176420235827550, 10.95006602420748010 ) ) ;
#104109 = FILL_AREA_STYLE_COLOUR ( '', #85055 ) ;
#104110 = CARTESIAN_POINT ( 'NONE',  ( -31.43278154310612393, 439.6985105754050664, 23.49139273982680010 ) ) ;
#104111 = CARTESIAN_POINT ( 'NONE',  ( 44.35000000000000142, 1.533819458162526451E-15, 0.000000000000000000 ) ) ;
#104112 = CARTESIAN_POINT ( 'NONE',  ( -33.50185725303997231, 488.2566613463952194, 10.59321780392846613 ) ) ;
#104113 = CARTESIAN_POINT ( 'NONE',  ( -30.00000000000000355, 488.7105343895983083, 4.072475191987426690 ) ) ;
#104114 = CARTESIAN_POINT ( 'NONE',  ( 86.89686805065835529, -59.99999999999999289, 200.9617660479750896 ) ) ;
#104115 = CIRCLE ( 'NONE', #5948, 3.309500000000001663 ) ;
#104116 = CIRCLE ( 'NONE', #50666, 4.000000000000000000 ) ;
#104117 = PRESENTATION_STYLE_ASSIGNMENT (( #23233 ) ) ;
#104118 = ORIENTED_EDGE ( 'NONE', *, *, #103851, .T. ) ;
#104119 = CARTESIAN_POINT ( 'NONE',  ( 55.54612012703360335, -42.96652821328475369, 62.92581338446308337 ) ) ;
#104120 = CARTESIAN_POINT ( 'NONE',  ( -30.46600437442538123, 308.5397930899359267, -8.697262802616858579 ) ) ;
#104121 = CARTESIAN_POINT ( 'NONE',  ( 3.363648053944603422, -48.78517836376548189, 104.5995868353016505 ) ) ;
#104122 = ADVANCED_FACE ( 'NONE', ( #4291 ), #19744, .F. ) ;
#104123 = AXIS2_PLACEMENT_3D ( 'NONE', #83329, #66620, #84936 ) ;
#104124 =( GEOMETRIC_REPRESENTATION_CONTEXT ( 3 ) GLOBAL_UNCERTAINTY_ASSIGNED_CONTEXT ( ( #35156 ) ) GLOBAL_UNIT_ASSIGNED_CONTEXT ( ( #70053, #94883, #21023 ) ) REPRESENTATION_CONTEXT ( 'NONE', 'WORKASPACE' ) );
#104125 = CARTESIAN_POINT ( 'NONE',  ( -6.944371705245973025, 29.46100308575449134, -3.972324460300561633 ) ) ;
#104126 = ORIENTED_EDGE ( 'NONE', *, *, #77519, .T. ) ;
#104128 = CARTESIAN_POINT ( 'NONE',  ( -14.47558186359348298, 21.82849871097600314, -4.801378726369249783 ) ) ;
#104127 = CARTESIAN_POINT ( 'NONE',  ( -101.2596523789430734, -38.35544838490221053, 95.56470404527684082 ) ) ;
#104129 = FACE_OUTER_BOUND ( 'NONE', #74171, .T. ) ;
#104130 = DIRECTION ( 'NONE',  ( 0.000000000000000000, 0.000000000000000000, -1.000000000000000000 ) ) ;
#104131 = CARTESIAN_POINT ( 'NONE',  ( 7.188101187499999156, -12.12500000204838990, 2.977408999572654924 ) ) ;
#104132 = CARTESIAN_POINT ( 'NONE',  ( -1.308996937480704004, -4.999999999999988454, -95.00000000000001421 ) ) ;
#104133 = EDGE_CURVE ( 'NONE', #53057, #101395, #100849, .T. ) ;
#104134 = EDGE_CURVE ( 'NONE', #92392, #38377, #35632, .T. ) ;
#104135 = CARTESIAN_POINT ( 'NONE',  ( 30.48723010194639471, 12.91713162683277538, -41.81530375792760879 ) ) ;
#104137 = EDGE_LOOP ( 'NONE', ( #27187, #70441, #72210, #41796, #64824 ) ) ;
#104136 = FILL_AREA_STYLE ('',( #45918 ) ) ;
#104138 = CARTESIAN_POINT ( 'NONE',  ( 85.21594557227290068, -22.03823677191263997, 162.9487912823339002 ) ) ;
#104139 = EDGE_CURVE ( 'NONE', #64475, #30636, #19991, .T. ) ;
#104140 = CARTESIAN_POINT ( 'NONE',  ( -46.00000000000000000, 461.6622277975413340, 10.18145404766431206 ) ) ;
#104141 = CARTESIAN_POINT ( 'NONE',  ( -35.53357291648787708, 439.5860488598422080, 24.00787122424867093 ) ) ;
#104142 = ORIENTED_EDGE ( 'NONE', *, *, #64563, .F. ) ;
#104143 = CARTESIAN_POINT ( 'NONE',  ( -37.71426560610335343, 395.7663590576279944, 6.364238202227666896 ) ) ;
#104144 = ADVANCED_FACE ( 'NONE', ( #68504 ), #50170, .F. ) ;
#104145 = CARTESIAN_POINT ( 'NONE',  ( 17.95960601129987211, 34.46549755681294158, 22.69733944828496774 ) ) ;
#104146 = DIRECTION ( 'NONE',  ( 0.000000000000000000, 0.000000000000000000, -1.000000000000000000 ) ) ;
#104147 = DIRECTION ( 'NONE',  ( 0.000000000000000000, -0.7633528697427554022, 0.6459817305895730888 ) ) ;
#104148 = B_SPLINE_SURFACE_WITH_KNOTS ( 'NONE', 3, 3, ( 
 ( #23919, #73475, #7674, #14711, #97752, #105334, #106372, #105850, #63829, #16310 ),
 ( #96718, #39555, #74014, #49743, #33065, #40067, #55691, #65405, #90746, #98298 ),
 ( #82651, #89153, #8223, #80507, #56760, #88620, #64869, #6628, #24455, #31478 ),
 ( #8752, #71899, #89688, #64361, #15785, #97231, #90211, #23378, #82102, #104800 ),
 ( #30952, #56215, #96, #15255, #65935, #98814, #24969, #16864, #48141, #22854 ),
 ( #81039, #7155, #72945, #31996, #91291, #11256, #43643, #44187, #77075, #78134 ),
 ( #52257, #3190, #36661, #101878, #86786, #28038, #68466, #69527, #94337, #36135 ),
 ( #76532, #60910, #86256, #69003, #28560, #33584, #35589, #101357, #77614, #93798 ) ),
 .UNSPECIFIED., .F., .F., .F.,
 ( 4, 2, 2, 4 ),
 ( 4, 2, 2, 2, 4 ),
 ( 0.000000000000000000, 0.2500000000000000000, 0.5000000000000000000, 1.000000000000000000 ),
 ( 0.000000000000000000, 0.1250000000000000000, 0.2500000000000000000, 0.5000000000000000000, 1.000000000000000000 ),
 .UNSPECIFIED. ) ;
#104149 = ORIENTED_EDGE ( 'NONE', *, *, #51284, .T. ) ;
#104150 =( LENGTH_UNIT ( ) NAMED_UNIT ( * ) SI_UNIT ( .MILLI., .METRE. ) );
#104151 = CARTESIAN_POINT ( 'NONE',  ( 43.00000000000000000, 450.0000000000002274, 13.20242257375370976 ) ) ;
#104152 = CARTESIAN_POINT ( 'NONE',  ( -5.000000000000000000, -14.29242795212260297, -6.555798487938274910 ) ) ;
#104153 = DIRECTION ( 'NONE',  ( 1.000000000000000000, -0.000000000000000000, -0.000000000000000000 ) ) ;
#104155 = CARTESIAN_POINT ( 'NONE',  ( -10.61644205368614280, 13.93655468994954560, -9.960933018827816454 ) ) ;
#104154 = CARTESIAN_POINT ( 'NONE',  ( -0.3592832422766795153, -18.03253741398754428, 35.00534045900273128 ) ) ;
#104156 = AXIS2_PLACEMENT_3D ( 'NONE', #60052, #11988, #75119 ) ;
#104157 = CARTESIAN_POINT ( 'NONE',  ( 7.188101187500001821, -17.56250000204838457, -2.977408999572650483 ) ) ;
#104158 = CARTESIAN_POINT ( 'NONE',  ( 16.36917923056512691, 294.5678716157545978, -2.060237494721419260 ) ) ;
#104159 = AXIS2_PLACEMENT_3D ( 'NONE', #66420, #1127, #99305 ) ;
#104160 =( NAMED_UNIT ( * ) SI_UNIT ( $, .STERADIAN. ) SOLID_ANGLE_UNIT ( ) );
#104161 = AXIS2_PLACEMENT_3D ( 'NONE', #3008, #20322, #94705 ) ;
#104162 = CIRCLE ( 'NONE', #57646, 6.499999999999999112 ) ;
#104163 = EDGE_LOOP ( 'NONE', ( #43877, #63713, #102185, #70637, #102415, #51997 ) ) ;
#104164 = SURFACE_STYLE_USAGE ( .BOTH. , #89054 ) ;
#104165 = CARTESIAN_POINT ( 'NONE',  ( 7.908230272949222872, -3.123266379892265299, -7.776722524729861696 ) ) ;
#104166 = COLOUR_RGB ( '', 0.72549020, 0.75294118, 0.79215686) ;
#104167 = CARTESIAN_POINT ( 'NONE',  ( -9.545014793598884495, 9.306529264753056196, -5.000000000000000888 ) ) ;
#104168 = CARTESIAN_POINT ( 'NONE',  ( 8.349999999999999645, 1.411358822780289120E-15, 0.000000000000000000 ) ) ;
#104169 = ORIENTED_EDGE ( 'NONE', *, *, #45581, .T. ) ;
#104170 = DIRECTION ( 'NONE',  ( 0.000000000000000000, -1.000000000000000000, 0.000000000000000000 ) ) ;
#104171 = CARTESIAN_POINT ( 'NONE',  ( 3.313708498984722972, -21.40625000409676915, -8.000000000000040856 ) ) ;
#104172 = EDGE_LOOP ( 'NONE', ( #34677, #69052, #8849 ) ) ;
#104173 = EDGE_CURVE ( 'NONE', #77164, #8054, #43680, .T. ) ;
#104174 = DIRECTION ( 'NONE',  ( -1.000000000000000000, -1.224606353822377258E-16, -0.000000000000000000 ) ) ;
#104175 = CARTESIAN_POINT ( 'NONE',  ( -1.238932115551811597, -1.825546356131314218E-15, 101.3452916561003434 ) ) ;
#104176 =( NAMED_UNIT ( * ) PLANE_ANGLE_UNIT ( ) SI_UNIT ( $, .RADIAN. ) );
#104177 = UNCERTAINTY_MEASURE_WITH_UNIT (LENGTH_MEASURE( 1.000000000000000082E-05 ), #102638, 'distance_accuracy_value', 'NONE');
#104178 = CARTESIAN_POINT ( 'NONE',  ( -106.7033407227921771, -60.00000000000000711, 120.7809815305387815 ) ) ;
#104179 =( NAMED_UNIT ( * ) SI_UNIT ( $, .STERADIAN. ) SOLID_ANGLE_UNIT ( ) );
#104180 = SURFACE_SIDE_STYLE ('',( #71285 ) ) ;
#104181 = CARTESIAN_POINT ( 'NONE',  ( 30.00000000000000000, 450.0000000000002274, 13.20242257375370976 ) ) ;
#104182 = CARTESIAN_POINT ( 'NONE',  ( -84.74376759734492737, -35.85438675842900835, 179.5104609505815745 ) ) ;
#104183 = ORIENTED_EDGE ( 'NONE', *, *, #37711, .F. ) ;
#104184 = DIRECTION ( 'NONE',  ( 0.000000000000000000, 0.000000000000000000, 1.000000000000000000 ) ) ;
#104185 = AXIS2_PLACEMENT_3D ( 'NONE', #12349, #3213, #52275 ) ;
#104186 = ORIENTED_EDGE ( 'NONE', *, *, #94287, .F. ) ;
#104187 = DIRECTION ( 'NONE',  ( 0.000000000000000000, -1.000000000000000000, 0.000000000000000000 ) ) ;
#104188 = CARTESIAN_POINT ( 'NONE',  ( 4.813668318631093790, -66.79513229826685006, 3.583991016754781267 ) ) ;
#104189 = ORIENTED_EDGE ( 'NONE', *, *, #59720, .T. ) ;
#104190 = CARTESIAN_POINT ( 'NONE',  ( -84.91794694852686121, -52.70031527363017432, 9.720178435334927869 ) ) ;
#104191 = FACE_BOUND ( 'NONE', #78222, .T. ) ;
#104192 =( NAMED_UNIT ( * ) SI_UNIT ( $, .STERADIAN. ) SOLID_ANGLE_UNIT ( ) );
#104193 = CARTESIAN_POINT ( 'NONE',  ( 4.678819457397414894, 143.9212778189090614, -5.000000000000000888 ) ) ;
#104194 = SURFACE_STYLE_FILL_AREA ( #38950 ) ;
#104195 = CARTESIAN_POINT ( 'NONE',  ( -15.50526908267491066, 41.99999999999999289, 57.69562748408483088 ) ) ;
#104196 = CARTESIAN_POINT ( 'NONE',  ( 78.64960161195060095, -14.21045842199435860, 174.1843170503133251 ) ) ;
#104197 = ADVANCED_FACE ( 'NONE', ( #52835 ), #77754, .T. ) ;
#104198 = CARTESIAN_POINT ( 'NONE',  ( -112.5893510171550105, -59.99999999999995026, 145.0943965991558002 ) ) ;
#104199 = CARTESIAN_POINT ( 'NONE',  ( -64.58854662160332794, -36.00888594457155989, 83.18360510322872869 ) ) ;
#104200 = EDGE_LOOP ( 'NONE', ( #23341, #66703, #89805, #41651, #89278, #72707 ) ) ;
#104201 = CARTESIAN_POINT ( 'NONE',  ( -56.56213115054879381, 39.42553718104704785, 32.16477550070589331 ) ) ;
#104202 = CARTESIAN_POINT ( 'NONE',  ( 72.64833377984137996, -60.00000000001470113, 181.7429652714145334 ) ) ;
#104203 = VERTEX_POINT ( 'NONE', #77654 ) ;
#104204 = CARTESIAN_POINT ( 'NONE',  ( 13.72589306172073442, -57.01108507920052659, 29.76321791924474525 ) ) ;
#104205 = B_SPLINE_CURVE_WITH_KNOTS ( 'NONE', 3,
 ( #58078, #31713, #868, #72672 ),
 .UNSPECIFIED., .F., .F.,
 ( 4, 4 ),
 ( 0.000000000000000000, 0.0007664883490339958897 ),
 .UNSPECIFIED. ) ;
#104206 = CARTESIAN_POINT ( 'NONE',  ( -1.320432766682874540E-15, -19.90625000204838457, 7.188101187500000044 ) ) ;
#104207 = ADVANCED_FACE ( 'NONE', ( #101396 ), #43326, .T. ) ;
#104208 = CARTESIAN_POINT ( 'NONE',  ( -30.00000000000000000, 500.0000000000002274, -5.000000000000001776 ) ) ;
#104209 = VERTEX_POINT ( 'NONE', #28603 ) ;
#104210 = FACE_OUTER_BOUND ( 'NONE', #84147, .T. ) ;
#104211 = VERTEX_POINT ( 'NONE', #84148 ) ;
#104212 = CARTESIAN_POINT ( 'NONE',  ( 10.92969676275519042, 45.30189166192086958, -15.24269870591670184 ) ) ;
#104213 = CARTESIAN_POINT ( 'NONE',  ( 47.29141116144560186, 18.29911311166214105, -14.59113362281996551 ) ) ;
#104214 = CARTESIAN_POINT ( 'NONE',  ( -38.87179246869587246, -59.99999999999997868, -39.79893131892280422 ) ) ;
#104215 = CARTESIAN_POINT ( 'NONE',  ( 2.212097561415789837, -14.31130214556282354, -0.5355294694856076454 ) ) ;
#104216 = CARTESIAN_POINT ( 'NONE',  ( -5.082755093536325042, -24.96875000204838813, -5.082755093536325930 ) ) ;
#104217 = FACE_OUTER_BOUND ( 'NONE', #81271, .T. ) ;
#104218 = CARTESIAN_POINT ( 'NONE',  ( -32.09911992168218831, 438.9232547152092252, 23.66653216045979491 ) ) ;
#104219 = CARTESIAN_POINT ( 'NONE',  ( 5.000000000000000000, -38.85173860975186955, 2.939083565186168201 ) ) ;
#104220 = CARTESIAN_POINT ( 'NONE',  ( 9.739726766100236688, 48.00000000000000000, -87.61747884500007899 ) ) ;
#104221 = DIRECTION ( 'NONE',  ( 0.000000000000000000, -1.000000000000000000, 0.000000000000000000 ) ) ;
#104222 = CARTESIAN_POINT ( 'NONE',  ( -38.55369376853367669, 309.5668124549920321, 1.485156153254792999 ) ) ;
#104223 = CARTESIAN_POINT ( 'NONE',  ( 103.5194293720434047, -60.00000000000000000, 191.8575224287939136 ) ) ;
#104224 = VERTEX_POINT ( 'NONE', #53377 ) ;
#104225 = DIRECTION ( 'NONE',  ( 0.000000000000000000, 0.000000000000000000, -1.000000000000000000 ) ) ;
#104226 = CARTESIAN_POINT ( 'NONE',  ( -16.06635273549532883, 42.44526696066479587, -88.41241673432038795 ) ) ;
#104227 = CARTESIAN_POINT ( 'NONE',  ( 37.15806814115364176, -42.96900667323284040, 37.34969296406126915 ) ) ;
#104228 = CIRCLE ( 'NONE', #43956, 1.000000000000002442 ) ;
#104229 = CARTESIAN_POINT ( 'NONE',  ( 2.910977163135976653, -8.673617379884035472E-16, -22.23822744035697241 ) ) ;
#104230 = ORIENTED_EDGE ( 'NONE', *, *, #3920, .T. ) ;
#104231 = CARTESIAN_POINT ( 'NONE',  ( 8.099999999999999645, -3.752776749732575468, -6.499999999999999112 ) ) ;
#104232 = STYLED_ITEM ( 'NONE', ( #61507 ), #87940 ) ;
#104233 = VERTEX_POINT ( 'NONE', #10248 ) ;
#104235 = CARTESIAN_POINT ( 'NONE',  ( 20.97754405179121662, 294.8763868968453608, 9.942224931492262385 ) ) ;
#104234 = DIRECTION ( 'NONE',  ( 0.000000000000000000, 0.000000000000000000, 1.000000000000000000 ) ) ;
#104236 = CARTESIAN_POINT ( 'NONE',  ( -32.96114378239634846, 439.7497662205610709, 24.15381041467389167 ) ) ;
#104237 = CARTESIAN_POINT ( 'NONE',  ( 68.45015997180047407, 4.000000000000014211, 0.000000000000000000 ) ) ;
#104238 = VECTOR ( 'NONE', #27353, 999.9999999999998863 ) ;
#104239 = CIRCLE ( 'NONE', #66356, 5.000000000000001776 ) ;
#104240 = CARTESIAN_POINT ( 'NONE',  ( 0.000000000000000000, 45.89575828009193259, 11.27631144943088337 ) ) ;
#104241 = CARTESIAN_POINT ( 'NONE',  ( -42.68684796707171358, 436.2654864220197055, 7.155924890008083850 ) ) ;
#104242 = AXIS2_PLACEMENT_3D ( 'NONE', #90807, #32593, #98865 ) ;
#104243 = CARTESIAN_POINT ( 'NONE',  ( 4.656390720430120034, -86.31646185960545381, 3.786082374785836535 ) ) ;
#104244 = FILL_AREA_STYLE ('',( #71345 ) ) ;
#104245 = CARTESIAN_POINT ( 'NONE',  ( 93.27314801925561483, -59.99999999999999289, 34.94592296014532451 ) ) ;
#104246 = CARTESIAN_POINT ( 'NONE',  ( 0.2565376335216122961, -2.516992571280024737, 6.500000000000000888 ) ) ;
#104247 = PRESENTATION_LAYER_ASSIGNMENT (  '', '', ( #52579 ) ) ;
#104248 = CARTESIAN_POINT ( 'NONE',  ( 0.000000000000000000, 0.000000000000000000, 0.000000000000000000 ) ) ;
#104249 = CARTESIAN_POINT ( 'NONE',  ( -16.75187969033532553, -1.200000000000000030E-05, 24.30698433968612449 ) ) ;
#104250 = ORIENTED_EDGE ( 'NONE', *, *, #80456, .F. ) ;
#104251 = CARTESIAN_POINT ( 'NONE',  ( -90.09582030224672167, -29.99999999995693400, -6.009880044648006958 ) ) ;
#104252 = ORIENTED_EDGE ( 'NONE', *, *, #16074, .F. ) ;
#104253 = EDGE_CURVE ( 'NONE', #20962, #13350, #57083, .T. ) ;
#104254 = DIRECTION ( 'NONE',  ( -1.000000000000000000, -1.224606353822377258E-16, -0.000000000000000000 ) ) ;
#104255 = CARTESIAN_POINT ( 'NONE',  ( -16.02369196221458125, 4.084267053699538685, 2.245701149452017376 ) ) ;
#104256 = CARTESIAN_POINT ( 'NONE',  ( 8.441095186811990558, 28.00979909688833658, 2.456708350805680174E-12 ) ) ;
#104257 = CARTESIAN_POINT ( 'NONE',  ( 14.66255430294002515, 22.40929092344816809, -3.546301636246186550 ) ) ;
#104258 = CARTESIAN_POINT ( 'NONE',  ( 84.35043940098535131, -60.17546792520573007, -17.01487635743571758 ) ) ;
#104259 = CARTESIAN_POINT ( 'NONE',  ( 7.188101187500000044, -33.03125000204838813, 0.000000000000000000 ) ) ;
#104260 = DIRECTION ( 'NONE',  ( 1.000000000000000000, -0.000000000000000000, -0.000000000000000000 ) ) ;
#104261 = CARTESIAN_POINT ( 'NONE',  ( 0.000000000000000000, 4.898587196589412829E-16, -4.000000000000000000 ) ) ;
#104262 = CARTESIAN_POINT ( 'NONE',  ( 34.92245183780732276, 464.4742769089222065, 18.75702545252121922 ) ) ;
#104263 = ADVANCED_FACE ( 'NONE', ( #39328 ), #46864, .T. ) ;
#104264 = ORIENTED_EDGE ( 'NONE', *, *, #67018, .T. ) ;
#104265 = EDGE_CURVE ( 'NONE', #54829, #55601, #80819, .T. ) ;
#104267 = ORIENTED_EDGE ( 'NONE', *, *, #59396, .F. ) ;
#104266 = CARTESIAN_POINT ( 'NONE',  ( 24.34999999999999787, -3.309499999999999886, 0.000000000000000000 ) ) ;
#104268 = CARTESIAN_POINT ( 'NONE',  ( 78.86428744248468092, -49.90252285640023899, 149.9481409427032474 ) ) ;
#104269 = B_SPLINE_CURVE_WITH_KNOTS ( 'NONE', 3,
 ( #54240, #78018, #71501, #46185, #87711, #13793, #5196, #5712, #4134, #103871, #62382, #86667, #30550, #12736, #45658, #30020, #69931, #78539, #61858, #79077, #63447, #94754, #20903, #53738, #4668, #37602, #70464, #87184, #29508, #38127, #62906, #21932, #2124, #35077, #34552, #91700, #42599, #52279, #17813, #85191, #51747, #67946, #44211, #91180, #51209, #36154, #18356, #58804, #75495, #76552, #77097, #11276, #59874, #25396, #68491, #58252, #27532, #100827, #50160, #1591, #26996, #2664, #3216, #67426, #26464, #92747, #10750, #69026, #60410, #18903, #50664, #83580, #100303, #59331, #84129, #17285, #93289, #10228, #9689, #34017, #76026, #92202, #84665, #43144, #83065, #9158, #42066, #43664, #25945, #35615, #101379, #19448, #74953, #1044, #66889, #99776, #13937, #70606, #69549, #78156, #4808, #87856, #29137, #101899, #93819, #103500, #22072, #19974, #37746, #52821, #79748, #28059, #3754, #85747, #54930, #13407, #11817, #70073 ),
 .UNSPECIFIED., .F., .F.,
 ( 4, 2, 2, 2, 1, 2, 2, 2, 2, 1, 1, 2, 2, 2, 2, 2, 1, 1, 1, 1, 2, 2, 2, 2, 1, 1, 1, 2, 2, 1, 2, 2, 1, 1, 1, 1, 2, 2, 2, 1, 2, 2, 1, 1, 1, 2, 2, 1, 1, 2, 2, 1, 1, 1, 2, 2, 2, 2, 1, 1, 1, 1, 1, 2, 2, 2, 1, 2, 2, 2, 2, 2, 1, 1, 4 ),
 ( 0.000000000000000000, 0.03109947195041606882, 0.06219894390083216540, 0.06608637789463417400, 0.06997381188843615485, 0.07774867987604017205, 0.09329841585124813708, 0.1243978878016639561, 0.1263416047985648771, 0.1282853217954657843, 0.1321727557892676541, 0.1399476237768715048, 0.1554973597520793449, 0.1865968317024948031, 0.1870827609517200507, 0.1875686902009452983, 0.1885405486993957380, 0.1904842656962965064, 0.1943716996900981542, 0.2021465676777013665, 0.2176963036529078188, 0.2487957756033205292, 0.2497676341017708856, 0.2507394926002212143, 0.2526832095971218162, 0.2565706435909231309, 0.2643455115785259824, 0.2798952475537313522, 0.3109947195041422030, 0.3119665780025925317, 0.3124525072518176683, 0.3125132484079708450, 0.3125739895641240218, 0.3126954718764308749, 0.3129384365010439151, 0.3148821534979506787, 0.3187695874917642058, 0.3265444554793912602, 0.3420941914546455909, 0.3430660499530990282, 0.3435519792023257746, 0.3437949438269390368, 0.3440379084515524100, 0.3459816254484592846, 0.3498690594422732003, 0.3576439274299010873, 0.3731936634051568613, 0.3741655219036103541, 0.3746514511528371005, 0.3748944157774504737, 0.3750158980897572714, 0.3751373804020640135, 0.3770810973989722759, 0.3809685313927887451, 0.3887433993804217947, 0.4042931353556878937, 0.4062368523525962116, 0.4064798169772098069, 0.4067227816018233466, 0.4072087108510503706, 0.4081805693495044740, 0.4120680033433208878, 0.4198428713309536042, 0.4353926073062189817, 0.4373363243031271330, 0.4383081828015812365, 0.4392800413000353399, 0.4431674752938518091, 0.4509423432814846366, 0.4664920792567503471, 0.4684357962536586095, 0.4703795132505668164, 0.4742669472443832301, 0.4820418152320161131, 0.4975915512072818236 ),
 .UNSPECIFIED. ) ;
#104270 = CARTESIAN_POINT ( 'NONE',  ( -38.80476300150524338, 27.34311131113723903, -12.01468182136296470 ) ) ;
#104271 = ORIENTED_EDGE ( 'NONE', *, *, #101481, .F. ) ;
#104272 = CARTESIAN_POINT ( 'NONE',  ( -12.50000000000000533, 26.69172216273781117, -44.20484773317921423 ) ) ;
#104273 = EDGE_CURVE ( 'NONE', #60854, #46619, #11566, .T. ) ;
#104274 = FILL_AREA_STYLE_COLOUR ( '', #85708 ) ;
#104275 = CARTESIAN_POINT ( 'NONE',  ( 7.188101187499999156, -17.75000000204838457, 2.977408999572654924 ) ) ;
#104276 = VECTOR ( 'NONE', #15813, 1000.000000000000114 ) ;
#104277 = CARTESIAN_POINT ( 'NONE',  ( 4.154708322984369194E-08, -57.67120202538961138, 41.61186700422869933 ) ) ;
#104278 = CARTESIAN_POINT ( 'NONE',  ( 15.88575968060462706, 294.5610636378226559, 1.875232630976614967 ) ) ;
#104279 = ORIENTED_EDGE ( 'NONE', *, *, #100585, .T. ) ;
#104280 = CARTESIAN_POINT ( 'NONE',  ( 4.560915367935576725, 8.779328275237030965, 4.999999999999999112 ) ) ;
#104281 = CARTESIAN_POINT ( 'NONE',  ( 6.951447288752834019, 41.73217225470716585, -59.36631759480938086 ) ) ;
#104282 = CARTESIAN_POINT ( 'NONE',  ( -5.656854249492379694, -13.62500000409676915, -5.656854249492380582 ) ) ;
#104283 = CARTESIAN_POINT ( 'NONE',  ( -19.58630244784536956, -16.93174034405112494, 31.48444303673279165 ) ) ;
#104284 = CARTESIAN_POINT ( 'NONE',  ( -2.499999999981197707, -21.99834632368703069, -30.53960193249073640 ) ) ;
#104285 = CARTESIAN_POINT ( 'NONE',  ( -0.8333333325078958742, -30.00000000000000355, -31.89470688134987597 ) ) ;
#104286 = CARTESIAN_POINT ( 'NONE',  ( 7.500000000000001776, -4.015205788346293048, -20.09376801818934766 ) ) ;
#104287 = DIRECTION ( 'NONE',  ( 0.2472079847635963445, 0.000000000000000000, 0.9689624411034318818 ) ) ;
#104288 = VECTOR ( 'NONE', #95557, 1000.000000000000000 ) ;
#104289 = CARTESIAN_POINT ( 'NONE',  ( 141.8829176528313951, 104.1183258647170362, 378.2207925529395993 ) ) ;
#104290 = CARTESIAN_POINT ( 'NONE',  ( -9.165151389911684987, 30.26735155607116923, -4.000000000000001776 ) ) ;
#104291 = ORIENTED_EDGE ( 'NONE', *, *, #60644, .F. ) ;
#104292 = CARTESIAN_POINT ( 'NONE',  ( 11.06447879995736194, 43.17496316643826759, 15.13962491005383271 ) ) ;
#104293 = CARTESIAN_POINT ( 'NONE',  ( -2.455962139888340889, 15.75268258782372754, 9.700350089084293970 ) ) ;
#104294 = DIRECTION ( 'NONE',  ( -0.000000000000000000, -0.000000000000000000, 1.000000000000000000 ) ) ;
#104295 = CARTESIAN_POINT ( 'NONE',  ( -73.92168396121962815, -30.09624395831016841, -28.12708220521432878 ) ) ;
#104296 = CARTESIAN_POINT ( 'NONE',  ( -70.11123173094190975, -29.99999999999999645, 95.68224316551422248 ) ) ;
#104297 = CARTESIAN_POINT ( 'NONE',  ( 101.4868948250290259, 1.016364837396684119E-14, 0.000000000000000000 ) ) ;
#104298 = CIRCLE ( 'NONE', #45799, 8.750000000000033751 ) ;
#104299 = EDGE_LOOP ( 'NONE', ( #41497, #80887, #51048 ) ) ;
#104300 = LINE ( 'NONE', #80023, #13408 ) ;
#104301 = CARTESIAN_POINT ( 'NONE',  ( 107.1778406945288822, -57.65541713316640937, 199.8906253976937251 ) ) ;
#104302 = CARTESIAN_POINT ( 'NONE',  ( 72.01055813165709196, -21.77032294813915314, -18.48580111295489914 ) ) ;
#104303 = EDGE_CURVE ( 'NONE', #44258, #13998, #84673, .T. ) ;
#104304 = CARTESIAN_POINT ( 'NONE',  ( 5.000000000000000000, 6.123233995736766282E-16, -1.446714285714285841 ) ) ;
#104305 = CARTESIAN_POINT ( 'NONE',  ( -14.87170168469266329, 23.06219547136248949, 1.058210525625679299 ) ) ;
#104306 = B_SPLINE_CURVE_WITH_KNOTS ( 'NONE', 3,
 ( #27934, #77504, #13272, #37613, #95285, #102303, #44075, #11682, #53749, #12219 ),
 .UNSPECIFIED., .F., .F.,
 ( 4, 2, 2, 2, 4 ),
 ( 0.000000000000000000, 0.001118707926289531874, 0.002237415852579063748, 0.003356123778868598875, 0.004474831705158133568 ),
 .UNSPECIFIED. ) ;
#104307 = CARTESIAN_POINT ( 'NONE',  ( 34.84618260875170392, 489.9833681528626812, 11.97975507378813731 ) ) ;
#104308 = CARTESIAN_POINT ( 'NONE',  ( -75.40897020374366377, -60.00000000000000711, 183.9572039174722988 ) ) ;
#104309 = AXIS2_PLACEMENT_3D ( 'NONE', #5031, #94591, #37963 ) ;
#104310 = CIRCLE ( 'NONE', #64667, 2.000000000000000000 ) ;
#104311 = DIRECTION ( 'NONE',  ( 0.000000000000000000, 0.000000000000000000, 1.000000000000000000 ) ) ;
#104312 = CARTESIAN_POINT ( 'NONE',  ( 31.36650669486618881, 1.474610560812782335E-15, 0.000000000000000000 ) ) ;
#104313 = CARTESIAN_POINT ( 'NONE',  ( 56.06936961874005476, 50.00000000006009770, -33.41736086627872027 ) ) ;
#104314 = CARTESIAN_POINT ( 'NONE',  ( -84.47662886974657681, -57.45685610910329899, 191.4181384606809218 ) ) ;
#104315 = VERTEX_POINT ( 'NONE', #23150 ) ;
#104316 = CARTESIAN_POINT ( 'NONE',  ( 36.65380293431815062, 373.4724601506463841, 4.384826873228177213 ) ) ;
#104317 = VECTOR ( 'NONE', #56295, 1000.000000000000000 ) ;
#104318 = CIRCLE ( 'NONE', #28608, 5.000000000000001776 ) ;
#104320 = EDGE_CURVE ( 'NONE', #74273, #34458, #72143, .T. ) ;
#104319 = CARTESIAN_POINT ( 'NONE',  ( -7.414346147791996522, -12.64589157662264363, -3.010818766110527456 ) ) ;
#104321 =( NAMED_UNIT ( * ) SI_UNIT ( $, .STERADIAN. ) SOLID_ANGLE_UNIT ( ) );
#104322 = CARTESIAN_POINT ( 'NONE',  ( -82.37491455164230558, -37.78085970200692145, -12.96758841603934798 ) ) ;
#104323 = CARTESIAN_POINT ( 'NONE',  ( 8.866506694866188809, 1.474610560812782335E-15, 0.000000000000000000 ) ) ;
#104324 = CARTESIAN_POINT ( 'NONE',  ( 13.69330508143927538, 0.000000000000000000, 5.000000000000002665 ) ) ;
#104325 = ORIENTED_EDGE ( 'NONE', *, *, #88444, .F. ) ;
#104326 = CARTESIAN_POINT ( 'NONE',  ( 17.98163244489454726, 50.00000000000000000, 61.91178591759881300 ) ) ;
#104327 = CARTESIAN_POINT ( 'NONE',  ( 7.000000000000000000, 0.000000000000000000, -4.874849604647447876 ) ) ;
#104328 = DIRECTION ( 'NONE',  ( 0.000000000000000000, -1.000000000000000000, 0.000000000000000000 ) ) ;
#104329 = CARTESIAN_POINT ( 'NONE',  ( 89.66801957890137942, -59.99999999999992895, -23.31517609469964469 ) ) ;
#104330 = CARTESIAN_POINT ( 'NONE',  ( -78.49245547457638850, -53.37694864719454557, 151.3764068736151955 ) ) ;
#104331 = VERTEX_POINT ( 'NONE', #9049 ) ;
#104332 = CARTESIAN_POINT ( 'NONE',  ( 12.27067942234224418, -14.21045842199423959, 34.40196113412964962 ) ) ;
#104333 = CARTESIAN_POINT ( 'NONE',  ( 57.45015997180046696, 6.975173280561618775E-15, 0.000000000000000000 ) ) ;
#104334 = CARTESIAN_POINT ( 'NONE',  ( 73.26562775815939688, -57.64134225645462806, 183.1174502722914781 ) ) ;
#104335 = PLANE ( 'NONE',  #66675 ) ;
#104336 = CARTESIAN_POINT ( 'NONE',  ( 36.73469237171850921, 305.2482013543003632, 0.4103627608394692095 ) ) ;
#104337 = ADVANCED_FACE ( 'NONE', ( #16625 ), #72091, .F. ) ;
#104338 = CARTESIAN_POINT ( 'NONE',  ( -14.29190075645648683, 6.456385560661901835, 7.561819230138081771 ) ) ;
#104339 = ORIENTED_EDGE ( 'NONE', *, *, #64505, .T. ) ;
#104340 =( LENGTH_UNIT ( ) NAMED_UNIT ( * ) SI_UNIT ( .MILLI., .METRE. ) );
#104342 = CARTESIAN_POINT ( 'NONE',  ( -101.1105981715984683, -52.71026112637824923, 130.0485633398400864 ) ) ;
#104341 = FACE_OUTER_BOUND ( 'NONE', #71842, .T. ) ;
#104343 = CARTESIAN_POINT ( 'NONE',  ( 2.977408999572651815, -26.93750000204838457, 7.188101187500000933 ) ) ;
#104345 = DIRECTION ( 'NONE',  ( 0.000000000000000000, -2.311253228826401127E-16, -1.000000000000000000 ) ) ;
#104344 =( BOUNDED_CURVE ( )  B_SPLINE_CURVE ( 2, ( #8720, #106337, #1132 ),
 .UNSPECIFIED., .F., .F. ) 
 B_SPLINE_CURVE_WITH_KNOTS ( ( 3, 3 ),
 ( 0.000000000000000000, 1.000000000000000000 ),
 .UNSPECIFIED. ) 
 CURVE ( )  GEOMETRIC_REPRESENTATION_ITEM ( )  RATIONAL_B_SPLINE_CURVE ( ( 1.000000000000000000, 1.857142857142858317, 1.000000000000000000 ) ) 
 REPRESENTATION_ITEM ( '' )  );
#104346 = AXIS2_PLACEMENT_3D ( 'NONE', #97845, #64438, #55253 ) ;
#104348 = ADVANCED_FACE ( 'NONE', ( #82423 ), #105306, .T. ) ;
#104347 = CYLINDRICAL_SURFACE ( 'NONE', #22307, 4.000000000000000000 ) ;
#104349 = CARTESIAN_POINT ( 'NONE',  ( -44.33510700167990137, 435.2103804628540047, 13.54837514018881706 ) ) ;
#104350 = CARTESIAN_POINT ( 'NONE',  ( 25.85216931545142316, 37.20485424854442158, 8.663044351978108182 ) ) ;
#104351 = FACE_OUTER_BOUND ( 'NONE', #48852, .T. ) ;
#104352 = B_SPLINE_CURVE_WITH_KNOTS ( 'NONE', 3,
 ( #45017, #22344, #21285, #5069, #21812, #12084, #95671, #4007, #5593, #94633, #63320, #46065, #103760, #3481, #36420, #20777, #96215, #54120, #102701, #78948, #78415, #55190, #38516, #86548, #69804, #54652, #69291, #45542, #28864, #61191, #38003, #70338, #29897, #102164, #79481, #88117 ),
 .UNSPECIFIED., .F., .F.,
 ( 4, 2, 2, 2, 2, 2, 2, 2, 2, 2, 2, 2, 2, 2, 2, 2, 2, 4 ),
 ( 0.000000000000000000, 0.0008074604767267238225, 0.001614920953453447645, 0.002422381430180171359, 0.003229841906906895290, 0.004037302383633619221, 0.004844762860360342718, 0.005652223337087066216, 0.006459683813813790580, 0.007267144290540514077, 0.008074604767267238442, 0.008882065243993961939, 0.009689525720720685437, 0.01049698619744740893, 0.01130444667417413243, 0.01211190715090085593, 0.01251563738926422115, 0.01291936762762758636 ),
 .UNSPECIFIED. ) ;
#104353 = CARTESIAN_POINT ( 'NONE',  ( -36.71005241817288578, 463.3006260613076961, 20.13736821485169415 ) ) ;
#104354 = VERTEX_POINT ( 'NONE', #73786 ) ;
#104355 = DIRECTION ( 'NONE',  ( -0.000000000000000000, -1.000000000000000000, -0.000000000000000000 ) ) ;
#104357 = CARTESIAN_POINT ( 'NONE',  ( 27.61218054589077298, -46.43287580142983728, 33.58888037689876427 ) ) ;
#104356 = CARTESIAN_POINT ( 'NONE',  ( 0.01688885742776671806, 7.321065037175427115, 3.319543390096037605 ) ) ;
#104358 = CARTESIAN_POINT ( 'NONE',  ( -24.31874290140378747, 25.21043322494278627, 32.55344527691972445 ) ) ;
#104359 = ORIENTED_EDGE ( 'NONE', *, *, #642, .F. ) ;
#104360 = UNCERTAINTY_MEASURE_WITH_UNIT (LENGTH_MEASURE( 1.000000000000000082E-05 ), #103933, 'distance_accuracy_value', 'NONE');
#104361 = ORIENTED_EDGE ( 'NONE', *, *, #24425, .F. ) ;
#104362 = DIRECTION ( 'NONE',  ( -1.000000000000000000, -0.000000000000000000, -0.000000000000000000 ) ) ;
#104363 = DIRECTION ( 'NONE',  ( -1.000000000000000000, -1.224606353822377258E-16, -0.000000000000000000 ) ) ;
#104364 = CARTESIAN_POINT ( 'NONE',  ( -43.55333112596418488, 465.2342844084849958, 9.238213423004522085 ) ) ;
#104365 = CARTESIAN_POINT ( 'NONE',  ( -0.1687456348417130103, 51.27204578583049255, -10.24141503192701919 ) ) ;
#104366 = CARTESIAN_POINT ( 'NONE',  ( 7.114815031913489740, 3.125246181595257688, 14.67111259585466954 ) ) ;
#104367 = CARTESIAN_POINT ( 'NONE',  ( -7.500000000000000888, 3.988838049906422434, -0.8529248949437571170 ) ) ;
#104368 = VERTEX_POINT ( 'NONE', #74319 ) ;
#104369 = CARTESIAN_POINT ( 'NONE',  ( 28.51326288413663690, -59.99999999999999289, -41.06723538131018358 ) ) ;
#104370 = CIRCLE ( 'NONE', #9657, 5.000000000000002665 ) ;
#104371 = CARTESIAN_POINT ( 'NONE',  ( 84.25108322389057491, -29.99999999999987566, 163.2339291413038609 ) ) ;
#104372 = CARTESIAN_POINT ( 'NONE',  ( -10.54854822160233674, 17.80311496882384503, 9.603326997340017712 ) ) ;
#104373 = CARTESIAN_POINT ( 'NONE',  ( 0.000000000000000000, 57.18445727710329862, -19.59103268995865221 ) ) ;
#104374 = DIRECTION ( 'NONE',  ( -0.000000000000000000, 1.000000000000000000, -0.000000000000000000 ) ) ;
#104375 =( BOUNDED_SURFACE ( )  B_SPLINE_SURFACE ( 3, 2, ( 
 ( #106110, #40331, #47877 ),
 ( #14446, #63572, #31735 ),
 ( #80784, #32260, #13390 ),
 ( #65139, #6897, #80247 ) ),
 .UNSPECIFIED., .F., .F., .F. ) 
 B_SPLINE_SURFACE_WITH_KNOTS ( ( 4, 4 ),
 ( 3, 3 ),
 ( 6.505213034913026604E-18, 0.002066227528073411295 ),
 ( 0.000000000000000000, 1.000000000000000000 ),
 .UNSPECIFIED. ) 
 GEOMETRIC_REPRESENTATION_ITEM ( )  RATIONAL_B_SPLINE_SURFACE ( (
 ( 1.000000000000000000, 0.7788880963805245861, 1.000000000000000000),
 ( 1.000000000000000000, 0.7743040464398175393, 1.000000000000000000),
 ( 1.000000000000000000, 0.7669333544817443782, 1.000000000000000000),
 ( 1.000000000000000000, 0.7583909709669810484, 1.000000000000000000) ) ) 
 REPRESENTATION_ITEM ( '' )  SURFACE ( )  );
#104376 = LINE ( 'NONE', #37037, #38149 ) ;
#104377 = ORIENTED_EDGE ( 'NONE', *, *, #10751, .F. ) ;
#104378 = MECHANICAL_DESIGN_GEOMETRIC_PRESENTATION_REPRESENTATION (  '', ( #90606 ), #7895 ) ;
#104379 = ORIENTED_EDGE ( 'NONE', *, *, #1063, .T. ) ;
#104380 = VERTEX_POINT ( 'NONE', #99115 ) ;
#104381 = CARTESIAN_POINT ( 'NONE',  ( 8.349999999999999645, 4.172000000000003261, 5.109226446042759579E-16 ) ) ;
#104382 = LINE ( 'NONE', #28419, #11442 ) ;
#104383 = CARTESIAN_POINT ( 'NONE',  ( 38.09999999999998721, 0.000000000000000000, 0.000000000000000000 ) ) ;
#104384 = CARTESIAN_POINT ( 'NONE',  ( -7.149999999999890221, 41.65000000000012648, -59.82695526680724640 ) ) ;
#104385 = DIRECTION ( 'NONE',  ( 0.000000000000000000, -1.000000000000000000, 0.000000000000000000 ) ) ;
#104386 = CARTESIAN_POINT ( 'NONE',  ( -46.00000000000000711, 485.6346359681443232, -1.078553770025317826 ) ) ;
#104387 = CARTESIAN_POINT ( 'NONE',  ( 6.326445470157511686, -6.578717624163894939, 2.268395195563513767 ) ) ;
#104388 = ORIENTED_EDGE ( 'NONE', *, *, #83427, .F. ) ;
#104389 = CARTESIAN_POINT ( 'NONE',  ( -2.617478844988693432, 48.00000000000000000, -94.73972676610495114 ) ) ;
#104390 = ORIENTED_EDGE ( 'NONE', *, *, #4968, .F. ) ;
#104391 = CARTESIAN_POINT ( 'NONE',  ( 39.83349330513380693, -4.000000000000000888, 4.898587196589416773E-16 ) ) ;
#104392 = SURFACE_SIDE_STYLE ('',( #38630 ) ) ;
#104393 = AXIS2_PLACEMENT_3D ( 'NONE', #47461, #72279, #104107 ) ;
#104394 = VECTOR ( 'NONE', #81505, 1000.000000000000000 ) ;
#104395 = CIRCLE ( 'NONE', #6223, 10.00000000000000178 ) ;
#104396 = CARTESIAN_POINT ( 'NONE',  ( -81.39518705382832309, -59.99999999999992184, 184.9064298456866879 ) ) ;
#104397 = CARTESIAN_POINT ( 'NONE',  ( 62.26579310671900203, -56.86312895564053349, 87.13878417979945823 ) ) ;
#104398 = ORIENTED_EDGE ( 'NONE', *, *, #85294, .T. ) ;
#104399 = CARTESIAN_POINT ( 'NONE',  ( 42.74607419124097163, 464.8137795011914477, 15.62215520944410052 ) ) ;
#104400 = CIRCLE ( 'NONE', #6231, 5.000000000000001776 ) ;
#104401 = EDGE_CURVE ( 'NONE', #27178, #57410, #24428, .T. ) ;
#104402 = DIRECTION ( 'NONE',  ( 0.000000000000000000, -1.000000000000000000, 0.000000000000000000 ) ) ;
#104403 = DIRECTION ( 'NONE',  ( 0.000000000000000000, -1.000000000000000000, 0.000000000000000000 ) ) ;
#104404 = EDGE_CURVE ( 'NONE', #90141, #30305, #79508, .T. ) ;
#104405 = FILL_AREA_STYLE ('',( #57429 ) ) ;
#104406 = ORIENTED_EDGE ( 'NONE', *, *, #67, .T. ) ;
#104407 =( NAMED_UNIT ( * ) PLANE_ANGLE_UNIT ( ) SI_UNIT ( $, .RADIAN. ) );
#104408 = PRESENTATION_STYLE_ASSIGNMENT (( #40205 ) ) ;
#104409 = CARTESIAN_POINT ( 'NONE',  ( -31.68901581506993637, -60.00000000000002132, -34.94011393958808753 ) ) ;
#104410 = AXIS2_PLACEMENT_3D ( 'NONE', #65801, #99756, #17795 ) ;
#104411 = EDGE_CURVE ( 'NONE', #26612, #105449, #56652, .T. ) ;
#104412 = LINE ( 'NONE', #103882, #59891 ) ;
#104413 = CARTESIAN_POINT ( 'NONE',  ( -8.000000000000000000, -30.03125000409677625, -3.313708498984762496 ) ) ;
#104414 = CARTESIAN_POINT ( 'NONE',  ( 5.219866590719942856, -5.000000000000000000, -8.922269033013279227 ) ) ;
#104415 = CARTESIAN_POINT ( 'NONE',  ( 86.81478249919962309, -39.10848448064970029, 188.7318862069557781 ) ) ;
#104416 = CARTESIAN_POINT ( 'NONE',  ( -5.290983596874198724, 17.95105532768313594, -37.37422055138609522 ) ) ;
#104417 = CIRCLE ( 'NONE', #44149, 5.000000000000001776 ) ;
#104418 = CARTESIAN_POINT ( 'NONE',  ( -8.826886570334650628, 18.27301070672817573, 6.352460523676195047E-13 ) ) ;
#104419 = CARTESIAN_POINT ( 'NONE',  ( -3.983107665916332252, 5.570601890521282407, -6.171481112545252223 ) ) ;
#104420 = CARTESIAN_POINT ( 'NONE',  ( -2.019483917365790222E-25, 303.8518027762758038, 9.936999415352289589 ) ) ;
#104421 = ORIENTED_EDGE ( 'NONE', *, *, #54806, .T. ) ;
#104422 = CARTESIAN_POINT ( 'NONE',  ( 13.49952125780149714, -52.22498368979241690, 30.71129996282902397 ) ) ;
#104423 = CARTESIAN_POINT ( 'NONE',  ( 0.000000000000000000, 0.000000000000000000, 27.00000000000000000 ) ) ;
#104424 = CIRCLE ( 'NONE', #45844, 4.000000000000001776 ) ;
#104425 = CARTESIAN_POINT ( 'NONE',  ( 39.14272297605699436, -60.00000000000003553, 50.93124313437822082 ) ) ;
#104426 = CARTESIAN_POINT ( 'NONE',  ( -100.7945030569529479, -30.00000000000000355, 162.5532351115364236 ) ) ;
#104427 = CARTESIAN_POINT ( 'NONE',  ( -40.75255125189226391, 485.0466573014779215, -4.066699219997739867 ) ) ;
#104428 = CARTESIAN_POINT ( 'NONE',  ( 35.32811641198794206, -57.69550348741336876, 49.48441236252082831 ) ) ;
#104430 = FACE_OUTER_BOUND ( 'NONE', #21158, .T. ) ;
#104429 = CARTESIAN_POINT ( 'NONE',  ( -9.221249107921773103, 248.9517862850150891, 3.869340886054255968 ) ) ;
#104431 = EDGE_CURVE ( 'NONE', #46114, #79431, #30587, .T. ) ;
#104432 = CARTESIAN_POINT ( 'NONE',  ( -18.66418957901244724, 50.00000000000000711, 61.03986302535336250 ) ) ;
#104433 = CARTESIAN_POINT ( 'NONE',  ( -10.00000000000004086, 14.99999999999998934, 4.210530276627957313 ) ) ;
#104434 = DIRECTION ( 'NONE',  ( 0.000000000000000000, 1.000000000000000000, 0.000000000000000000 ) ) ;
#104435 = CARTESIAN_POINT ( 'NONE',  ( -1.413758147757360861, -60.00000000000000711, 39.63760611331755257 ) ) ;
#104436 = CARTESIAN_POINT ( 'NONE',  ( 11.47105347311152634, -16.49375446481005270, -34.68891165858038761 ) ) ;
#104437 =( NAMED_UNIT ( * ) SI_UNIT ( $, .STERADIAN. ) SOLID_ANGLE_UNIT ( ) );
#104438 = MECHANICAL_DESIGN_GEOMETRIC_PRESENTATION_REPRESENTATION (  '', ( #73395 ), #88977 ) ;
#104439 = FILL_AREA_STYLE ('',( #12772 ) ) ;
#104440 = ORIENTED_EDGE ( 'NONE', *, *, #6989, .F. ) ;
#104441 = CARTESIAN_POINT ( 'NONE',  ( 17.50000000000001066, 51.39211690089886986, 62.71362001260527563 ) ) ;
#104442 = CARTESIAN_POINT ( 'NONE',  ( 40.91184305475058380, 436.7571283257985328, 21.64376470813695263 ) ) ;
#104443 = CARTESIAN_POINT ( 'NONE',  ( -10.48329054730247556, -60.36588335206413092, 33.96539373894616176 ) ) ;
#104446 = ADVANCED_FACE ( 'NONE', ( #45172, #63478, #21965, #22507 ), #87215, .F. ) ;
#104445 = CARTESIAN_POINT ( 'NONE',  ( 39.83997765698279636, 460.7086825730507371, 2.106271324414728419 ) ) ;
#104444 = CARTESIAN_POINT ( 'NONE',  ( -87.60448404220831264, -59.99999999999997158, 36.07240305281307258 ) ) ;
#104447 = ADVANCED_FACE ( 'NONE', ( #5748 ), #69144, .F. ) ;
#104448 = CIRCLE ( 'NONE', #7974, 8.000000000000000000 ) ;
#104449 = ORIENTED_EDGE ( 'NONE', *, *, #81453, .T. ) ;
#104450 = CARTESIAN_POINT ( 'NONE',  ( 26.11182265785232559, 35.05542332294329810, 8.043516664989388332 ) ) ;
#104451 = CARTESIAN_POINT ( 'NONE',  ( 16.07816244836988417, 5.101897851387931837, -4.232350007286695970 ) ) ;
#104452 = DIRECTION ( 'NONE',  ( -1.000000000000000000, -1.224606353822377258E-16, -0.000000000000000000 ) ) ;
#104453 = PRESENTATION_LAYER_ASSIGNMENT (  '', '', ( #63205 ) ) ;
#104454 = CARTESIAN_POINT ( 'NONE',  ( 15.93933706297306507, 3.102176837441567248, 0.7193050692217635156 ) ) ;
#104455 = CARTESIAN_POINT ( 'NONE',  ( 72.21310543845304153, -60.00000000000000000, 155.8912871955335788 ) ) ;
#104456 = CARTESIAN_POINT ( 'NONE',  ( -0.7751162123649483204, 54.19727782468113730, -8.015928695369900936 ) ) ;
#104457 = ORIENTED_EDGE ( 'NONE', *, *, #100752, .T. ) ;
#104458 = CARTESIAN_POINT ( 'NONE',  ( 0.000000000000000000, 0.000000000000000000, 0.000000000000000000 ) ) ;
#104459 = CIRCLE ( 'NONE', #83743, 4.000000000000000888 ) ;
#104460 = CARTESIAN_POINT ( 'NONE',  ( -34.10831268713208431, 434.1698048432537576, 11.21913565533539447 ) ) ;
#104461 = CIRCLE ( 'NONE', #11443, 4.000000000000000888 ) ;
#104462 = AXIS2_PLACEMENT_3D ( 'NONE', #105583, #15512, #81292 ) ;
#104463 = STYLED_ITEM ( 'NONE', ( #45981 ), #36850 ) ;
#104464 = CARTESIAN_POINT ( 'NONE',  ( 3.168307535684225851, 112.8159850782372047, -5.000000000000000000 ) ) ;
#104465 = EDGE_CURVE ( 'NONE', #13469, #92048, #33039, .T. ) ;
#104466 = CARTESIAN_POINT ( 'NONE',  ( -4.526657684027568074, -2.093347780961939186, 103.5746540667394555 ) ) ;
#104467 = ORIENTED_EDGE ( 'NONE', *, *, #15197, .F. ) ;
#104468 = EDGE_LOOP ( 'NONE', ( #18812, #66885, #3997, #35873 ) ) ;
#104470 = PRESENTATION_LAYER_ASSIGNMENT (  '', '', ( #52820 ) ) ;
#104469 = CARTESIAN_POINT ( 'NONE',  ( -24.52418941431424315, 305.4846864080880664, 10.29874865197013101 ) ) ;
#104471 = ORIENTED_EDGE ( 'NONE', *, *, #35706, .F. ) ;
#104472 = ADVANCED_FACE ( 'NONE', ( #29540 ), #10657, .T. ) ;
#104473 = DIRECTION ( 'NONE',  ( -1.000000000000000000, 0.000000000000000000, -0.000000000000000000 ) ) ;
#104474 = CYLINDRICAL_SURFACE ( 'NONE', #86369, 6.999999999999992895 ) ;
#104475 = EDGE_LOOP ( 'NONE', ( #68707, #102487, #22329, #41715, #75570, #6328 ) ) ;
#104476 = SURFACE_STYLE_USAGE ( .BOTH. , #102897 ) ;
#104477 = SURFACE_STYLE_USAGE ( .BOTH. , #47818 ) ;
#104478 = CARTESIAN_POINT ( 'NONE',  ( -114.4908978873841647, -60.00000000000980549, 166.8152118193485194 ) ) ;
#104479 = CARTESIAN_POINT ( 'NONE',  ( 6.338255145480260921, 2.729868969643340471, -6.500000000000002665 ) ) ;
#104480 = CARTESIAN_POINT ( 'NONE',  ( 40.78730011461682636, -60.00000000000002132, 53.21614385487430354 ) ) ;
#104481 = CARTESIAN_POINT ( 'NONE',  ( 85.18902050349326771, -60.00000000000000000, -15.68190703514374107 ) ) ;
#104483 = CARTESIAN_POINT ( 'NONE',  ( 12.35463245259948906, -35.99170037105584896, 29.94182087016703875 ) ) ;
#104482 = CARTESIAN_POINT ( 'NONE',  ( -91.50803816462422446, -30.00000000000001776, 42.72771024551138908 ) ) ;
#104484 = CARTESIAN_POINT ( 'NONE',  ( -45.62210685601630900, -49.89848660444781814, 47.30625596735477956 ) ) ;
#104485 = ADVANCED_FACE ( 'NONE', ( #4169 ), #94160, .F. ) ;
#104486 = CARTESIAN_POINT ( 'NONE',  ( 28.58349330513380337, 1.593028355512270962E-15, 0.000000000000000000 ) ) ;
#104487 = PRODUCT ( 'hex flange bolt_din_DIN 6921 - M8 x 30 x 30-S', 'hex flange bolt_din_DIN 6921 - M8 x 30 x 30-S', '', ( #15287 ) ) ;
#104488 = ORIENTED_EDGE ( 'NONE', *, *, #33854, .F. ) ;
#104489 = EDGE_CURVE ( 'NONE', #77149, #54299, #89854, .T. ) ;
#104490 = CARTESIAN_POINT ( 'NONE',  ( 1.106418893442917994, 12.12096734116461150, -49.90218892958102259 ) ) ;
#104491 = FILL_AREA_STYLE_COLOUR ( '', #18609 ) ;
#104492 = CARTESIAN_POINT ( 'NONE',  ( -1.262177448353618889E-25, 304.8518027762758038, -9.000000000000005329 ) ) ;
#104493 = LINE ( 'NONE', #88331, #93429 ) ;
#104495 = ORIENTED_EDGE ( 'NONE', *, *, #38825, .T. ) ;
#104494 = AXIS2_PLACEMENT_3D ( 'NONE', #48221, #103816, #81124 ) ;
#104496 = CARTESIAN_POINT ( 'NONE',  ( -9.235252277563404277, -13.40511626313917048, 16.47531707632386500 ) ) ;
#104497 = ORIENTED_EDGE ( 'NONE', *, *, #101021, .T. ) ;
#104498 = CARTESIAN_POINT ( 'NONE',  ( 103.5655738155463581, -30.00000000000023093, 196.9807721782169097 ) ) ;
#104499 =( LENGTH_UNIT ( ) NAMED_UNIT ( * ) SI_UNIT ( .MILLI., .METRE. ) );
#104500 = CARTESIAN_POINT ( 'NONE',  ( 6.294742690869562729, 41.94828263799632850, -59.44631289860604539 ) ) ;
#104501 =( GEOMETRIC_REPRESENTATION_CONTEXT ( 3 ) GLOBAL_UNCERTAINTY_ASSIGNED_CONTEXT ( ( #11363 ) ) GLOBAL_UNIT_ASSIGNED_CONTEXT ( ( #41082, #36756, #27067 ) ) REPRESENTATION_CONTEXT ( 'NONE', 'WORKASPACE' ) );
#104502 = SURFACE_STYLE_FILL_AREA ( #31704 ) ;
#104503 = CARTESIAN_POINT ( 'NONE',  ( 97.34229447618668019, -30.00000000000000000, 190.9596792136885597 ) ) ;
#104504 = CARTESIAN_POINT ( 'NONE',  ( 0.4988340113715863944, 3.871605243926953488, 8.000000000000000000 ) ) ;
#104505 = EDGE_LOOP ( 'NONE', ( #41910, #67230, #76457, #52045, #35949, #49717 ) ) ;
#104506 = ORIENTED_EDGE ( 'NONE', *, *, #12881, .T. ) ;
#104507 = ORIENTED_EDGE ( 'NONE', *, *, #105893, .F. ) ;
#104508 = CARTESIAN_POINT ( 'NONE',  ( -27.72867908628325040, 36.41173040130990302, 9.902678004857877525 ) ) ;
#104509 = CARTESIAN_POINT ( 'NONE',  ( 20.59999999999999787, -3.309499999999999886, 0.000000000000000000 ) ) ;
#104510 = CARTESIAN_POINT ( 'NONE',  ( 20.97754405179127346, 294.8763868968453608, 9.942224931492237516 ) ) ;
#104511 = ORIENTED_EDGE ( 'NONE', *, *, #17445, .T. ) ;
#104512 = CARTESIAN_POINT ( 'NONE',  ( -79.35676939654273099, -38.35606429531669903, -26.89919366358169128 ) ) ;
#104513 = ORIENTED_EDGE ( 'NONE', *, *, #79892, .F. ) ;
#104514 = FACE_OUTER_BOUND ( 'NONE', #102687, .T. ) ;
#104515 = CARTESIAN_POINT ( 'NONE',  ( 91.60420904625036087, -38.50451920916797377, 200.9222943262674050 ) ) ;
#104516 = CARTESIAN_POINT ( 'NONE',  ( 14.78767551106102474, 5.758539365854975500, 6.917020875423936843 ) ) ;
#104517 = CARTESIAN_POINT ( 'NONE',  ( 82.73356237690738624, -37.85693543688039142, 2.979072353819682828 ) ) ;
#104518 = CARTESIAN_POINT ( 'NONE',  ( 84.34874083255445498, -38.00000000000004974, 179.1776475100507184 ) ) ;
#104519 = CARTESIAN_POINT ( 'NONE',  ( 36.03903953312295272, 307.9766817680012991, 13.05290268685154231 ) ) ;
#104520 = CARTESIAN_POINT ( 'NONE',  ( 5.656854249492380582, -24.50000000409677270, -5.656854249492379694 ) ) ;
#104521 = CARTESIAN_POINT ( 'NONE',  ( 9.797174393178825657E-16, -30.00000000000000000, -8.000000000000000000 ) ) ;
#104522 = TOROIDAL_SURFACE ( 'NONE', #11508, 12.00000000000000000, 2.000000000000000000 ) ;
#104523 = CARTESIAN_POINT ( 'NONE',  ( 0.000000000000000000, -2.000000000000000000, 0.000000000000000000 ) ) ;
#104524 = CARTESIAN_POINT ( 'NONE',  ( 1.450845733305902385, -0.02389980327605355920, 101.4859859777359077 ) ) ;
#104525 = VERTEX_POINT ( 'NONE', #90387 ) ;
#104526 = EDGE_CURVE ( 'NONE', #54991, #38679, #101087, .T. ) ;
#104527 = DIRECTION ( 'NONE',  ( -1.000000000000000000, -1.224606353822377258E-16, -0.000000000000000000 ) ) ;
#104528 = CARTESIAN_POINT ( 'NONE',  ( -33.89250494191506391, 463.6575930728432127, 6.993601543838152246 ) ) ;
#104529 = CARTESIAN_POINT ( 'NONE',  ( -31.83945028356544782, 465.6738295161418364, 10.98138951113073780 ) ) ;
#104530 = VERTEX_POINT ( 'NONE', #64530 ) ;
#104531 = CARTESIAN_POINT ( 'NONE',  ( 32.12958771267400948, 464.7275665249413237, 11.12424126545837133 ) ) ;
#104532 = CARTESIAN_POINT ( 'NONE',  ( -25.70845616436730197, 305.2466841868522351, 10.47404382804886147 ) ) ;
#104533 = CARTESIAN_POINT ( 'NONE',  ( -12.50000000000000355, -3.000000000000001776, -76.70872284621019332 ) ) ;
#104534 = UNCERTAINTY_MEASURE_WITH_UNIT (LENGTH_MEASURE( 1.000000000000000082E-05 ), #26585, 'distance_accuracy_value', 'NONE');
#104535 = CARTESIAN_POINT ( 'NONE',  ( -8.000000000000000000, -17.74999999999999645, -9.797174393178825657E-16 ) ) ;
#104536 = CIRCLE ( 'NONE', #92518, 4.000000000000000888 ) ;
#104538 = CARTESIAN_POINT ( 'NONE',  ( 32.10152049993604351, -25.19009005012509306, 40.01174804926688466 ) ) ;
#104537 = MECHANICAL_DESIGN_GEOMETRIC_PRESENTATION_REPRESENTATION (  '', ( #68368 ), #30503 ) ;
#104539 = EDGE_CURVE ( 'NONE', #82046, #10704, #15963, .T. ) ;
#104540 =( BOUNDED_CURVE ( )  B_SPLINE_CURVE ( 2, ( #103995, #47874, #5833 ),
 .UNSPECIFIED., .F., .F. ) 
 B_SPLINE_CURVE_WITH_KNOTS ( ( 3, 3 ),
 ( 0.000000000000000000, 1.000000000000000000 ),
 .UNSPECIFIED. ) 
 CURVE ( )  GEOMETRIC_REPRESENTATION_ITEM ( )  RATIONAL_B_SPLINE_CURVE ( ( 1.000000000000000000, 1.857142857142858317, 1.000000000000000000 ) ) 
 REPRESENTATION_ITEM ( '' )  );
#104541 = STYLED_ITEM ( 'NONE', ( #19680 ), #23944 ) ;
#104542 = CIRCLE ( 'NONE', #71808, 4.000000000000001776 ) ;
#104543 = AXIS2_PLACEMENT_3D ( 'NONE', #66550, #64051, #25607 ) ;
#104544 = VERTEX_POINT ( 'NONE', #65045 ) ;
#104545 = CARTESIAN_POINT ( 'NONE',  ( 85.96484678228922860, -28.40575032613359951, 181.6661039577698773 ) ) ;
#104546 = CARTESIAN_POINT ( 'NONE',  ( -49.09793955338193427, 7.820164633611648597, 16.25544133048934725 ) ) ;
#104547 = DIRECTION ( 'NONE',  ( 0.000000000000000000, 1.000000000000000000, 0.000000000000000000 ) ) ;
#104548 = EDGE_LOOP ( 'NONE', ( #94485, #53513, #73337, #39578 ) ) ;
#104549 = CARTESIAN_POINT ( 'NONE',  ( 94.28774462368049569, -57.67244037246990729, 24.05690785289403522 ) ) ;
#104550 = FACE_OUTER_BOUND ( 'NONE', #51607, .T. ) ;
#104551 = CARTESIAN_POINT ( 'NONE',  ( -30.00229752355677704, 12.60065794652347471, 39.63915577993667938 ) ) ;
#104552 =( LENGTH_UNIT ( ) NAMED_UNIT ( * ) SI_UNIT ( .MILLI., .METRE. ) );
#104553 = EDGE_CURVE ( 'NONE', #53038, #93080, #95279, .T. ) ;
#104554 = DIRECTION ( 'NONE',  ( 1.000000000000000000, 0.000000000000000000, 0.000000000000000000 ) ) ;
#104555 = CARTESIAN_POINT ( 'NONE',  ( -2.094395098902536390, -4.999999999999998224, -8.000000000000000000 ) ) ;
#104556 = CARTESIAN_POINT ( 'NONE',  ( -1.249327701954737080, 8.410337540188283612, -7.776713651267457728 ) ) ;
#104558 = CARTESIAN_POINT ( 'NONE',  ( -12.11780882157808037, 7.885269496745385354, 8.622659793487008173 ) ) ;
#104557 = CARTESIAN_POINT ( 'NONE',  ( 0.000000000000000000, 6.123233995736770227E-16, -5.000000000000002665 ) ) ;
#104559 = EDGE_CURVE ( 'NONE', #27202, #78767, #48314, .T. ) ;
#104560 = FACE_BOUND ( 'NONE', #63950, .T. ) ;
#104561 = CARTESIAN_POINT ( 'NONE',  ( -16.64348903516526335, 43.75610143575153899, -4.157797401561264650 ) ) ;
#104562 = CARTESIAN_POINT ( 'NONE',  ( 11.69514296591814961, -5.000000000000000000, -88.12259424195812585 ) ) ;
#104563 = CARTESIAN_POINT ( 'NONE',  ( 10.00000000000003730, 14.99999999999998934, -4.210530276627963531 ) ) ;
#104564 = DIRECTION ( 'NONE',  ( 0.5735764363510442720, -0.8191520442889930198, 1.003171929053526349E-16 ) ) ;
#104565 = CARTESIAN_POINT ( 'NONE',  ( -102.0812981579065735, -37.99999999999997868, 157.7097999441383251 ) ) ;
#104566 = AXIS2_PLACEMENT_3D ( 'NONE', #78874, #5002, #21743 ) ;
#104567 = ADVANCED_FACE ( 'NONE', ( #74715 ), #60673, .F. ) ;
#104568 = ORIENTED_EDGE ( 'NONE', *, *, #17234, .F. ) ;
#104569 = CARTESIAN_POINT ( 'NONE',  ( 6.692588830498428010, -3.932766476276041256, -6.892929031562517572 ) ) ;
#104570 = LINE ( 'NONE', #71145, #12473 ) ;
#104571 = CARTESIAN_POINT ( 'NONE',  ( -10.35119932786764174, -16.29280028192038898, -34.78455815056601352 ) ) ;
#104574 = EDGE_CURVE ( 'NONE', #93003, #81288, #53970, .T. ) ;
#104573 = CARTESIAN_POINT ( 'NONE',  ( -37.82507325719418390, -34.58951407227882413, -29.84568773776970474 ) ) ;
#104572 = FACE_OUTER_BOUND ( 'NONE', #33175, .T. ) ;
#104575 = ORIENTED_EDGE ( 'NONE', *, *, #98165, .T. ) ;
#104576 = DIRECTION ( 'NONE',  ( -1.000000000000000000, 0.000000000000000000, 0.000000000000000000 ) ) ;
#104577 = VERTEX_POINT ( 'NONE', #796 ) ;
#104578 = CIRCLE ( 'NONE', #77106, 5.000000000000001776 ) ;
#104579 = CARTESIAN_POINT ( 'NONE',  ( 6.222742520105470021, 3.584500230190543313, 6.791463481567635796 ) ) ;
#104580 = LINE ( 'NONE', #12905, #33889 ) ;
#104581 = CARTESIAN_POINT ( 'NONE',  ( -92.68008335882309723, -60.00000000000002132, -4.308470193755781885 ) ) ;
#104582 = ORIENTED_EDGE ( 'NONE', *, *, #57883, .T. ) ;
#104583 = CARTESIAN_POINT ( 'NONE',  ( 26.69900261086841198, 1.482358050883964840E-15, 0.000000000000000000 ) ) ;
#104584 = CARTESIAN_POINT ( 'NONE',  ( -8.239452746273963513, 54.07618835787194200, -1.562132243825230082 ) ) ;
#104585 = CARTESIAN_POINT ( 'NONE',  ( 99.94675357384078040, -52.77032261955505277, 194.2389869445230772 ) ) ;
#104586 = CARTESIAN_POINT ( 'NONE',  ( 9.165151389911699198, 249.9999999999999432, -4.000000000000002665 ) ) ;
#104587 = EDGE_CURVE ( 'NONE', #38642, #77985, #45128, .T. ) ;
#104588 = CARTESIAN_POINT ( 'NONE',  ( -80.02865028407020986, -53.38608073763546713, 163.9029365645991163 ) ) ;
#104589 = CONICAL_SURFACE ( 'NONE', #66734, 3.309500000000001663, 0.9599310885968770357 ) ;
#104590 = VERTEX_POINT ( 'NONE', #101670 ) ;
#104591 = ORIENTED_EDGE ( 'NONE', *, *, #2572, .F. ) ;
#104592 = ORIENTED_EDGE ( 'NONE', *, *, #93469, .T. ) ;
#104593 = CARTESIAN_POINT ( 'NONE',  ( 31.13164466794002649, 436.9146031748717860, 23.68605626514782969 ) ) ;
#104594 = EDGE_CURVE ( 'NONE', #65105, #42645, #105381, .T. ) ;
#104595 = CARTESIAN_POINT ( 'NONE',  ( -6.018857979291350802, -63.35165937125906765, 14.35967520096848027 ) ) ;
#104596 = DIRECTION ( 'NONE',  ( -1.000000000000000000, -0.000000000000000000, -0.000000000000000000 ) ) ;
#104597 = ORIENTED_EDGE ( 'NONE', *, *, #59004, .F. ) ;
#104598 = CYLINDRICAL_SURFACE ( 'NONE', #58257, 9.999999999999994671 ) ;
#104599 = CARTESIAN_POINT ( 'NONE',  ( -9.216463528758735535, 15.13241195026071928, -3.884543032213800373 ) ) ;
#104600 = CARTESIAN_POINT ( 'NONE',  ( -93.14832842661381562, -57.61817439972283239, 204.4570750068989469 ) ) ;
#104601 = CARTESIAN_POINT ( 'NONE',  ( -43.75401118688380819, 486.3173572309548263, 5.908089951475163915 ) ) ;
#104602 = B_SPLINE_CURVE_WITH_KNOTS ( 'NONE', 3,
 ( #4749, #43606, #3697, #60352, #93227, #77038, #76498, #45223, #35555, #85132, #69489, #44148, #20462, #102375, #28526, #61406, #53304, #102913, #86223, #78099, #4217, #37150, #79688, #89393, #39783, #64583, #71587, #7381, #97454, #96426, #30640, #106073, #72658, #23610, #56462, #54325 ),
 .UNSPECIFIED., .F., .F.,
 ( 4, 2, 2, 2, 2, 2, 2, 2, 2, 2, 2, 2, 2, 2, 2, 2, 2, 4 ),
 ( 0.000000000000000000, 0.0008074604767267249067, 0.001614920953453449813, 0.002422381430180174829, 0.003229841906906899627, 0.004037302383633624425, 0.004844762860360349657, 0.005652223337087074889, 0.006459683813813799254, 0.007267144290540524486, 0.008074604767267248850, 0.008882065243993974082, 0.009689525720720699314, 0.01049698619744742455, 0.01130444667417414978, 0.01211190715090087501, 0.01251563738926423329, 0.01291936762762759330 ),
 .UNSPECIFIED. ) ;
#104603 = CYLINDRICAL_SURFACE ( 'NONE', #41077, 8.000000000000000000 ) ;
#104604 = CIRCLE ( 'NONE', #1256, 1.000000000000000888 ) ;
#104605 = CARTESIAN_POINT ( 'NONE',  ( -15.90614609307868399, -4.000000000000002665, 18.57417562100670949 ) ) ;
#104606 = CONICAL_SURFACE ( 'NONE', #21956, 3.309500000000001663, 0.9599310885968770357 ) ;
#104607 = CARTESIAN_POINT ( 'NONE',  ( 1.005716520562355942, 27.47520070304291551, -40.24667390188346161 ) ) ;
#104608 = CARTESIAN_POINT ( 'NONE',  ( 87.24803233485737053, -14.21045842199430709, -0.3983294879921217557 ) ) ;
#104609 = EDGE_CURVE ( 'NONE', #48268, #58994, #67187, .T. ) ;
#104610 = CARTESIAN_POINT ( 'NONE',  ( -40.90223414571102012, -60.00000000000005684, 57.82070650035302606 ) ) ;
#104611 = CARTESIAN_POINT ( 'NONE',  ( -51.55243906946975585, -49.90950515671671184, 57.17738528615195293 ) ) ;
#104612 = ORIENTED_EDGE ( 'NONE', *, *, #39428, .F. ) ;
#104613 = CARTESIAN_POINT ( 'NONE',  ( 0.000000000000000000, 0.000000000000000000, 4.000000000000000000 ) ) ;
#104614 = CONICAL_SURFACE ( 'NONE', #87395, 4.000000000000000000, 0.9599310885968912466 ) ;
#104615 = VERTEX_POINT ( 'NONE', #83881 ) ;
#104616 = VECTOR ( 'NONE', #90539, 1000.000000000000000 ) ;
#104617 = CARTESIAN_POINT ( 'NONE',  ( -102.1345869732698191, -60.20522555469838011, 194.0426171803833029 ) ) ;
#104618 = AXIS2_PLACEMENT_3D ( 'NONE', #96833, #71474, #47198 ) ;
#104619 = CARTESIAN_POINT ( 'NONE',  ( -30.82452621380396351, 13.29951192218421063, -41.36733700123911461 ) ) ;
#104620 = ORIENTED_EDGE ( 'NONE', *, *, #10161, .F. ) ;
#104621 = DIRECTION ( 'NONE',  ( 0.000000000000000000, 0.000000000000000000, -1.000000000000000000 ) ) ;
#104622 = CARTESIAN_POINT ( 'NONE',  ( 88.43115089625497660, -38.37427755674787022, -18.98099822564858385 ) ) ;
#104623 = DIRECTION ( 'NONE',  ( -0.8191520442889974607, 0.000000000000000000, -0.5735764363510379438 ) ) ;
#104624 = EDGE_CURVE ( 'NONE', #105779, #31486, #19357, .T. ) ;
#104625 = CARTESIAN_POINT ( 'NONE',  ( -2.503177626522498755, 294.8391969429503092, 9.934319910064267845 ) ) ;
#104626 = CARTESIAN_POINT ( 'NONE',  ( 0.000000000000000000, 49.00000000000000000, 66.00000000000000000 ) ) ;
#104627 = CARTESIAN_POINT ( 'NONE',  ( -40.93292669599463096, 378.0706848361106722, 26.55786848468904537 ) ) ;
#104628 =( GEOMETRIC_REPRESENTATION_CONTEXT ( 3 ) GLOBAL_UNCERTAINTY_ASSIGNED_CONTEXT ( ( #53443 ) ) GLOBAL_UNIT_ASSIGNED_CONTEXT ( ( #89906, #40290, #56991 ) ) REPRESENTATION_CONTEXT ( 'NONE', 'WORKASPACE' ) );
#104629 = CARTESIAN_POINT ( 'NONE',  ( -9.994988777600744001E-16, -0.6346842323187741330, 6.499999999999998224 ) ) ;
#104630 = CARTESIAN_POINT ( 'NONE',  ( 4.092977972706264289, 52.07635395608964757, -6.911964971445145878 ) ) ;
#104631 = CARTESIAN_POINT ( 'NONE',  ( -0.08412175410183092561, 34.17188553058034728, 29.75000000000000000 ) ) ;
#104632 = CARTESIAN_POINT ( 'NONE',  ( 8.000000000000000000, -24.49999999999999289, 0.000000000000000000 ) ) ;
#104633 = ORIENTED_EDGE ( 'NONE', *, *, #89448, .T. ) ;
#104634 = ORIENTED_EDGE ( 'NONE', *, *, #66865, .T. ) ;
#104635 = CARTESIAN_POINT ( 'NONE',  ( 49.49069524382411345, -46.43876033542694159, 52.19611476058279464 ) ) ;
#104636 = CARTESIAN_POINT ( 'NONE',  ( 29.83349330513380693, -3.851859888774471706E-31, 4.000000000000001776 ) ) ;
#104637 = CARTESIAN_POINT ( 'NONE',  ( -6.560397950766611253, 16.17087793925111328, 2.451970031105680015 ) ) ;
#104638 = CARTESIAN_POINT ( 'NONE',  ( -110.9980754224539368, -38.35624728847308518, 173.2928619168303896 ) ) ;
#104639 = CIRCLE ( 'NONE', #34079, 3.309500000000001663 ) ;
#104640 = ORIENTED_EDGE ( 'NONE', *, *, #64914, .T. ) ;
#104641 = CARTESIAN_POINT ( 'NONE',  ( 91.20265291891645631, -38.35752600691088077, -0.7216000038766476887 ) ) ;
#104642 = CARTESIAN_POINT ( 'NONE',  ( 10.76947298832407363, 15.76878063321550982, -9.614905453851129380 ) ) ;
#104643 = CARTESIAN_POINT ( 'NONE',  ( -19.35755210044912289, 49.90709869893811401, 61.15086111258641210 ) ) ;
#104644 = CARTESIAN_POINT ( 'NONE',  ( 96.73119497196310590, -60.15121125156788651, 95.89194316550425867 ) ) ;
#104645 = CARTESIAN_POINT ( 'NONE',  ( -31.50544488634473339, 439.3527810931634576, 23.21716044688400515 ) ) ;
#104646 = CYLINDRICAL_SURFACE ( 'NONE', #17121, 4.999999999999999112 ) ;
#104647 = CARTESIAN_POINT ( 'NONE',  ( -35.75515486453239333, 408.9583410871374554, 6.060592194821802892 ) ) ;
#104648 = CARTESIAN_POINT ( 'NONE',  ( 9.797174393178825657E-16, 35.00000000000000000, 8.000000000000000000 ) ) ;
#104649 = CARTESIAN_POINT ( 'NONE',  ( -32.16914446836677399, 486.0693400665468289, 5.247150504720089259 ) ) ;
#104650 = VECTOR ( 'NONE', #20064, 1000.000000000000000 ) ;
#104651 = CARTESIAN_POINT ( 'NONE',  ( 95.26165383619279226, -60.00000000000000711, 202.5694694144836205 ) ) ;
#104652 = AXIS2_PLACEMENT_3D ( 'NONE', #83109, #59931, #75000 ) ;
#104653 = SURFACE_STYLE_FILL_AREA ( #80367 ) ;
#104654 = ORIENTED_EDGE ( 'NONE', *, *, #54265, .F. ) ;
#104655 = CARTESIAN_POINT ( 'NONE',  ( 56.58617729883268765, -39.49445358650807947, 63.80126640809557870 ) ) ;
#104656 = CARTESIAN_POINT ( 'NONE',  ( -34.68392891983880588, 301.0938521591136805, -8.596509045476626198 ) ) ;
#104657 = EDGE_CURVE ( 'NONE', #36986, #39480, #20625, .T. ) ;
#104658 = DIRECTION ( 'NONE',  ( 0.000000000000000000, 0.000000000000000000, -1.000000000000000000 ) ) ;
#104659 = CARTESIAN_POINT ( 'NONE',  ( -6.944031699373470090, 29.46539345443872193, 3.972913591453822502 ) ) ;
#104660 = ORIENTED_EDGE ( 'NONE', *, *, #52977, .F. ) ;
#104662 = CARTESIAN_POINT ( 'NONE',  ( -9.933618426942553370, -50.20576216351469867, 25.82409549033520690 ) ) ;
#104661 = CARTESIAN_POINT ( 'NONE',  ( -109.1755639416890773, -38.35617105290818074, 189.5517844986839293 ) ) ;
#104663 = CARTESIAN_POINT ( 'NONE',  ( 4.028951842967195773, -3.000000000000000444, 6.990291106834064294 ) ) ;
#104664 = CARTESIAN_POINT ( 'NONE',  ( 19.73463816634110657, 304.7971333121958537, 8.925379062039144884 ) ) ;
#104665 = CARTESIAN_POINT ( 'NONE',  ( 37.62251730745840916, 437.3427388312647395, 4.535622330043188377 ) ) ;
#104666 = CARTESIAN_POINT ( 'NONE',  ( 3.313708498984762496, -32.28125000000000000, 7.999999999999998224 ) ) ;
#104667 = CARTESIAN_POINT ( 'NONE',  ( -9.999999999999992895, -3.000000000000002665, -83.69100306252320820 ) ) ;
#104668 = EDGE_CURVE ( 'NONE', #34171, #6924, #59093, .T. ) ;
#104669 = AXIS2_PLACEMENT_3D ( 'NONE', #21888, #14275, #78488 ) ;
#104670 = CARTESIAN_POINT ( 'NONE',  ( 4.472135954999578722, 249.9999999999999432, 4.000000000000002665 ) ) ;
#104671 =( GEOMETRIC_REPRESENTATION_CONTEXT ( 3 ) GLOBAL_UNCERTAINTY_ASSIGNED_CONTEXT ( ( #95485 ) ) GLOBAL_UNIT_ASSIGNED_CONTEXT ( ( #56930, #83878, #42897 ) ) REPRESENTATION_CONTEXT ( 'NONE', 'WORKASPACE' ) );
#104672 = ORIENTED_EDGE ( 'NONE', *, *, #53359, .T. ) ;
#104673 = CARTESIAN_POINT ( 'NONE',  ( 81.50921258790607737, -57.01699942316916747, 182.3434811776381252 ) ) ;
#104674 = CARTESIAN_POINT ( 'NONE',  ( -45.99999999996713740, 463.5261361515072167, 9.383844849049905790 ) ) ;
#104675 = AXIS2_PLACEMENT_3D ( 'NONE', #3617, #85063, #75896 ) ;
#104676 = CARTESIAN_POINT ( 'NONE',  ( -34.11324467909268776, 439.1267449652036134, 24.05939132677088921 ) ) ;
#104677 = ORIENTED_EDGE ( 'NONE', *, *, #32330, .F. ) ;
#104678 = DIRECTION ( 'NONE',  ( -1.000000000000000000, -0.000000000000000000, 0.000000000000000000 ) ) ;
#104679 = CARTESIAN_POINT ( 'NONE',  ( 5.689604056830701140, -4.325321803359224226, -16.92223617908316413 ) ) ;
#104680 = CARTESIAN_POINT ( 'NONE',  ( 13.58349330513380160, -4.000000000000000888, 4.898587196589416773E-16 ) ) ;
#104681 = DIRECTION ( 'NONE',  ( 1.734723475976807094E-16, 0.000000000000000000, 1.000000000000000000 ) ) ;
#104682 = CARTESIAN_POINT ( 'NONE',  ( -34.55272070743144042, 42.66495351264344293, -62.99786256745820623 ) ) ;
#104683 = PRESENTATION_STYLE_ASSIGNMENT (( #38908 ) ) ;
#104684 =( BOUNDED_SURFACE ( )  B_SPLINE_SURFACE ( 3, 2, ( 
 ( #92381, #42775, #75667 ),
 ( #92915, #34725, #93990 ),
 ( #58976, #51919, #51387 ),
 ( #52451, #67598, #100476 ),
 ( #36330, #50849, #20150 ),
 ( #27706, #26636, #59507 ),
 ( #43836, #35245, #2298 ),
 ( #18527, #27167, #84302 ),
 ( #28230, #11455, #44381 ),
 ( #11993, #2840, #10397 ),
 ( #43313, #10918, #85922 ),
 ( #76196, #91863, #60580 ) ),
 .UNSPECIFIED., .F., .F., .F. ) 
 B_SPLINE_SURFACE_WITH_KNOTS ( ( 4, 2, 2, 2, 2, 4 ),
 ( 3, 3 ),
 ( 7.589415207398531038E-19, 0.0007735885786023073089, 0.001547177157204613750, 0.001933971446505767080, 0.002320765735806920409, 0.003094354314409226633 ),
 ( 0.000000000000000000, 1.000000000000000000 ),
 .UNSPECIFIED. ) 
 GEOMETRIC_REPRESENTATION_ITEM ( )  RATIONAL_B_SPLINE_SURFACE ( (
 ( 1.000000000000000000, 0.9603284238771496728, 1.000000000000000000),
 ( 1.000000000000000000, 0.9628724889917197327, 1.000000000000000000),
 ( 1.000000000000000000, 0.9663306537743611146, 1.000000000000000000),
 ( 1.000000000000000000, 0.9744563874115511615, 1.000000000000000000),
 ( 1.000000000000000000, 0.9789903143386995410, 1.000000000000000000),
 ( 1.000000000000000000, 0.9855527733005633451, 1.000000000000000000),
 ( 1.000000000000000000, 0.9877025284829050733, 1.000000000000000000),
 ( 1.000000000000000000, 0.9916277982505179445, 1.000000000000000000),
 ( 1.000000000000000000, 0.9934221110298004920, 1.000000000000000000),
 ( 1.000000000000000000, 0.9980179737616273750, 1.000000000000000000),
 ( 1.000000000000000000, 1.000016370385754527, 1.000000000000000000),
 ( 1.000000000000000000, 1.000000000000000000, 1.000000000000000000) ) ) 
 REPRESENTATION_ITEM ( '' )  SURFACE ( )  );
#104685 = EDGE_CURVE ( 'NONE', #7953, #85648, #18112, .T. ) ;
#104686 = EDGE_LOOP ( 'NONE', ( #39372, #100682, #46944, #67039, #73370 ) ) ;
#104687 = CARTESIAN_POINT ( 'NONE',  ( 38.32383406387373981, 25.24657036848469360, 13.20420819894402698 ) ) ;
#104688 = CARTESIAN_POINT ( 'NONE',  ( -4.628159615119684211, -47.68919827030617142, 102.5435725457686118 ) ) ;
#104690 = CARTESIAN_POINT ( 'NONE',  ( -11.77640042769365536, 19.16702799015035197, -7.901857338882000370 ) ) ;
#104689 = CARTESIAN_POINT ( 'NONE',  ( 0.000000000000000000, 195.0000000000000000, 0.000000000000000000 ) ) ;
#104691 = CARTESIAN_POINT ( 'NONE',  ( 2.977408999572650927, -18.87500000204838457, -7.188101187500001821 ) ) ;
#104692 = AXIS2_PLACEMENT_3D ( 'NONE', #44367, #10904, #103135 ) ;
#104693 = CARTESIAN_POINT ( 'NONE',  ( -52.56483885390523625, 40.83906611473335602, -38.23529411764706509 ) ) ;
#104694 =( GEOMETRIC_REPRESENTATION_CONTEXT ( 3 ) GLOBAL_UNCERTAINTY_ASSIGNED_CONTEXT ( ( #96557 ) ) GLOBAL_UNIT_ASSIGNED_CONTEXT ( ( #29563, #39225, #62434 ) ) REPRESENTATION_CONTEXT ( 'NONE', 'WORKASPACE' ) );
#104695 = TOROIDAL_SURFACE ( 'NONE', #40949, 57.21727615095610275, 0.5000000000000000000 ) ;
#104696 = CARTESIAN_POINT ( 'NONE',  ( 13.86650669486618881, 4.000000000000003553, 4.898587196589414801E-16 ) ) ;
#104697 = ITEM_DEFINED_TRANSFORMATION ( 'NONE', 'NONE', #102356,  #10728 ) ;
#104698 = ORIENTED_EDGE ( 'NONE', *, *, #14487, .T. ) ;
#104699 = CARTESIAN_POINT ( 'NONE',  ( -4.472135954999580498, -10.00000000000000888, 4.000000000000000000 ) ) ;
#104700 = DIRECTION ( 'NONE',  ( -1.000000000000000000, -0.000000000000000000, -0.000000000000000000 ) ) ;
#104701 = CARTESIAN_POINT ( 'NONE',  ( -8.340816975846024661, 120.4114851255831837, -4.999999999997459810 ) ) ;
#104702 = LINE ( 'NONE', #79887, #37812 ) ;
#104703 = CARTESIAN_POINT ( 'NONE',  ( 0.000000000000000000, 0.000000000000000000, 0.000000000000000000 ) ) ;
#104704 = ORIENTED_EDGE ( 'NONE', *, *, #38929, .T. ) ;
#104705 = AXIS2_PLACEMENT_3D ( 'NONE', #27012, #1609, #100321 ) ;
#104706 = LINE ( 'NONE', #14088, #3307 ) ;
#104707 = FACE_OUTER_BOUND ( 'NONE', #42641, .T. ) ;
#104708 = ORIENTED_EDGE ( 'NONE', *, *, #19691, .T. ) ;
#104709 = B_SPLINE_CURVE_WITH_KNOTS ( 'NONE', 3,
 ( #99364, #58402, #1740, #91314, #83722, #17423, #42209, #75091 ),
 .UNSPECIFIED., .F., .F.,
 ( 4, 2, 2, 4 ),
 ( 6.938893903907228378E-18, 0.005764214328876836498, 0.008646321493315253445, 0.01152842865775367126 ),
 .UNSPECIFIED. ) ;
#104710 = CARTESIAN_POINT ( 'NONE',  ( -2.321165800182275252, -0.2152620590929751054, 102.3911379722518262 ) ) ;
#104711 = CARTESIAN_POINT ( 'NONE',  ( 6.815830331203684977, 1.210606185736183200E-13, -6.171384342982610072 ) ) ;
#104712 = CARTESIAN_POINT ( 'NONE',  ( -112.1936433325827522, -60.00000000000000000, 169.7638481750816197 ) ) ;
#104713 = PLANE ( 'NONE',  #104870 ) ;
#104714 = DIRECTION ( 'NONE',  ( -1.000000000000000000, -0.000000000000000000, -0.000000000000000000 ) ) ;
#104715 = CARTESIAN_POINT ( 'NONE',  ( -4.651132217449170270, -5.000000000000000000, -15.66661053588738106 ) ) ;
#104716 = LINE ( 'NONE', #54556, #26844 ) ;
#104717 = AXIS2_PLACEMENT_3D ( 'NONE', #8059, #83025, #25904 ) ;
#104718 = B_SPLINE_CURVE_WITH_KNOTS ( 'NONE', 3,
 ( #6212, #86650, #30004, #70968 ),
 .UNSPECIFIED., .F., .F.,
 ( 4, 4 ),
 ( 1.022751534364685075E-16, 0.001950293525757256386 ),
 .UNSPECIFIED. ) ;
#104719 = CARTESIAN_POINT ( 'NONE',  ( -83.65218577006966427, -39.46595630469712290, 175.6988558114236980 ) ) ;
#104720 = VERTEX_POINT ( 'NONE', #17576 ) ;
#104721 = CARTESIAN_POINT ( 'NONE',  ( 34.56161316558368668, 42.66376877430343484, -62.98563745867910768 ) ) ;
#104722 = ORIENTED_EDGE ( 'NONE', *, *, #11957, .T. ) ;
#104723 = DIRECTION ( 'NONE',  ( -1.000000000000000000, 0.000000000000000000, 0.000000000000000000 ) ) ;
#104724 = EDGE_CURVE ( 'NONE', #79974, #24620, #72652, .T. ) ;
#104725 = CARTESIAN_POINT ( 'NONE',  ( 6.000208918519489565, -69.00031337789968688, -0.2646532170642288406 ) ) ;
#104726 = CARTESIAN_POINT ( 'NONE',  ( -86.28082192411680751, -60.14685432405564569, 19.04948843146160442 ) ) ;
#104727 = DIRECTION ( 'NONE',  ( 0.000000000000000000, -1.000000000000000000, 0.000000000000000000 ) ) ;
#104728 = ADVANCED_FACE ( 'NONE', ( #42360 ), #34310, .F. ) ;
#104729 = CIRCLE ( 'NONE', #39314, 4.172000000000001485 ) ;
#104730 = FILL_AREA_STYLE ('',( #106303 ) ) ;
#104731 = CARTESIAN_POINT ( 'NONE',  ( 3.225607053692172599, 36.35104404975468384, -4.999999999999997335 ) ) ;
#104732 = CARTESIAN_POINT ( 'NONE',  ( 7.500000000000000888, 9.184850993605149917E-16, 0.000000000000000000 ) ) ;
#104733 = AXIS2_PLACEMENT_3D ( 'NONE', #90570, #16681, #49572 ) ;
#104734 = CARTESIAN_POINT ( 'NONE',  ( 96.06638400950703272, -14.21045842199450426, 198.0643409056117434 ) ) ;
#104735 = EDGE_CURVE ( 'NONE', #56878, #30328, #36530, .T. ) ;
#104736 = CARTESIAN_POINT ( 'NONE',  ( -91.97835729869039767, -14.21045842199439591, 64.70454208516892436 ) ) ;
#104737 = CARTESIAN_POINT ( 'NONE',  ( -67.15909898532748912, -22.10498377052748964, 83.34062656716834283 ) ) ;
#104738 = ORIENTED_EDGE ( 'NONE', *, *, #21556, .F. ) ;
#104739 = CARTESIAN_POINT ( 'NONE',  ( 5.938258408366269947, 39.42529018484425052, 64.79746803155040880 ) ) ;
#104740 = CARTESIAN_POINT ( 'NONE',  ( 57.63154298134735853, -59.99999999998056666, 100.7219984684233367 ) ) ;
#104741 = VERTEX_POINT ( 'NONE', #86041 ) ;
#104742 = CARTESIAN_POINT ( 'NONE',  ( 1.980960943318600176, -22.06722745478349168, 27.56539235055124948 ) ) ;
#104743 = CARTESIAN_POINT ( 'NONE',  ( 7.188101187499999156, -16.62500000204838813, 2.977408999572654924 ) ) ;
#104744 = DIRECTION ( 'NONE',  ( -1.000000000000000000, -1.224606353822377258E-16, -0.000000000000000000 ) ) ;
#104745 = ORIENTED_EDGE ( 'NONE', *, *, #59348, .F. ) ;
#104747 = DIRECTION ( 'NONE',  ( 0.000000000000000000, -1.000000000000000000, 0.000000000000000000 ) ) ;
#104746 = VECTOR ( 'NONE', #99232, 1000.000000000000000 ) ;
#104748 = VERTEX_POINT ( 'NONE', #62293 ) ;
#104749 = FACE_BOUND ( 'NONE', #62552, .T. ) ;
#104750 = CARTESIAN_POINT ( 'NONE',  ( -15.00099999999999767, 12.99999999999999289, 0.000000000000000000 ) ) ;
#104751 = CARTESIAN_POINT ( 'NONE',  ( -104.6983220124084397, -60.00000000000001421, 108.3235972286209261 ) ) ;
#104752 = LINE ( 'NONE', #38455, #27907 ) ;
#104753 = CARTESIAN_POINT ( 'NONE',  ( 2.977408999572650927, -28.25000000204838813, -7.188101187500001821 ) ) ;
#104754 = EDGE_CURVE ( 'NONE', #47192, #19669, #81262, .T. ) ;
#104755 = DIRECTION ( 'NONE',  ( 1.000000000000000000, 1.224606353822377258E-16, 0.000000000000000000 ) ) ;
#104756 = CARTESIAN_POINT ( 'NONE',  ( -5.290067270632268226, 54.20842449845686417, -6.031152949374520844 ) ) ;
#104757 = CARTESIAN_POINT ( 'NONE',  ( 5.000000000000000888, -59.33342285675411176, 7.478329308075513104 ) ) ;
#104758 = CARTESIAN_POINT ( 'NONE',  ( 9.999999999999989342, 49.99999999999999289, -86.30899693748767731 ) ) ;
#104759 =( LENGTH_UNIT ( ) NAMED_UNIT ( * ) SI_UNIT ( .MILLI., .METRE. ) );
#104760 = CARTESIAN_POINT ( 'NONE',  ( 0.000000000000000000, 7.505553499465140277, 3.755786496842903002E-16 ) ) ;
#104761 = CARTESIAN_POINT ( 'NONE',  ( 27.16282903641085866, 305.1222582335363995, -9.499934379274456830 ) ) ;
#104762 = CARTESIAN_POINT ( 'NONE',  ( -37.36874049225535543, -25.67000572301214945, 33.86699708943749698 ) ) ;
#104763 = ORIENTED_EDGE ( 'NONE', *, *, #33671, .F. ) ;
#104764 = CARTESIAN_POINT ( 'NONE',  ( 17.81438722625302518, 1.482358050883964840E-15, 0.000000000000000000 ) ) ;
#104765 = CIRCLE ( 'NONE', #87537, 7.500000000000006217 ) ;
#104766 = CONICAL_SURFACE ( 'NONE', #6590, 3.309500000000001663, 0.9599310885968770357 ) ;
#104767 = CARTESIAN_POINT ( 'NONE',  ( 41.58657417432790737, -49.88673011520329936, 42.49169459770972423 ) ) ;
#104769 = STYLED_ITEM ( 'NONE', ( #4593 ), #41066 ) ;
#104768 = CARTESIAN_POINT ( 'NONE',  ( -10.45706415777455689, -1.734723475976807094E-15, -13.60704923275582701 ) ) ;
#104770 = ORIENTED_EDGE ( 'NONE', *, *, #86740, .T. ) ;
#104771 = AXIS2_PLACEMENT_3D ( 'NONE', #92722, #34530, #52256 ) ;
#104772 = CARTESIAN_POINT ( 'NONE',  ( 6.222742520105474462, -7.673830019007166214, -0.2914634815676421797 ) ) ;
#104773 = CARTESIAN_POINT ( 'NONE',  ( -73.67975493303866585, -38.32615326775285780, 157.6922298713693067 ) ) ;
#104774 = ORIENTED_EDGE ( 'NONE', *, *, #45010, .T. ) ;
#104776 = CARTESIAN_POINT ( 'NONE',  ( -21.25502769577498796, 305.0480251235313176, 9.978840188629131802 ) ) ;
#104775 = CARTESIAN_POINT ( 'NONE',  ( 6.286008769881732405, -5.000000000000000000, -15.35021772302718190 ) ) ;
#104777 = CARTESIAN_POINT ( 'NONE',  ( -32.92225573320412479, 439.7404251386054739, 24.14402493977262765 ) ) ;
#104778 = DIRECTION ( 'NONE',  ( 0.000000000000000000, -1.000000000000000000, 0.000000000000000000 ) ) ;
#104779 = AXIS2_PLACEMENT_3D ( 'NONE', #75623, #11946, #2249 ) ;
#104780 = CARTESIAN_POINT ( 'NONE',  ( 1.249493494485172995, 43.73042964061625071, -17.18013998211830540 ) ) ;
#104781 =( LENGTH_UNIT ( ) NAMED_UNIT ( * ) SI_UNIT ( .MILLI., .METRE. ) );
#104782 = CARTESIAN_POINT ( 'NONE',  ( -49.27079747525463915, 12.96457032161196210, -15.75812555157997075 ) ) ;
#104783 = CARTESIAN_POINT ( 'NONE',  ( -3.995243879123565378, -48.66248409693900356, 43.59136604025376016 ) ) ;
#104784 = CARTESIAN_POINT ( 'NONE',  ( 95.45921739354632507, -60.00000000000001421, 52.31160816427112792 ) ) ;
#104785 = CARTESIAN_POINT ( 'NONE',  ( 6.162888688655344005, -3.752776749732561257, 6.500000000000000000 ) ) ;
#104786 = CARTESIAN_POINT ( 'NONE',  ( 0.2565376335216109638, -2.516992571280020741, 6.499999999999999112 ) ) ;
#104787 = DIRECTION ( 'NONE',  ( -1.000000000000000000, 0.000000000000000000, 0.000000000000000000 ) ) ;
#104788 = ORIENTED_EDGE ( 'NONE', *, *, #14168, .T. ) ;
#104789 = ADVANCED_FACE ( 'NONE', ( #61223 ), #94107, .T. ) ;
#104790 = STYLED_ITEM ( 'NONE', ( #77118 ), #44186 ) ;
#104791 = CARTESIAN_POINT ( 'NONE',  ( -88.03351418313572196, -29.99999999999498002, -16.96970854458511724 ) ) ;
#104792 = ORIENTED_EDGE ( 'NONE', *, *, #69262, .F. ) ;
#104793 = DIRECTION ( 'NONE',  ( 0.000000000000000000, 0.000000000000000000, 1.000000000000000000 ) ) ;
#104794 = CARTESIAN_POINT ( 'NONE',  ( -16.01537386455369116, 3.832633078741163768, -1.292357405291790773 ) ) ;
#104795 = CARTESIAN_POINT ( 'NONE',  ( 4.474494503600904061, 9.481805777968613569, 5.000000000000002665 ) ) ;
#104796 = DIRECTION ( 'NONE',  ( 0.000000000000000000, 0.000000000000000000, -1.000000000000000000 ) ) ;
#104797 =( LENGTH_UNIT ( ) NAMED_UNIT ( * ) SI_UNIT ( .MILLI., .METRE. ) );
#104798 = CARTESIAN_POINT ( 'NONE',  ( -2.977408999572654480, -23.00000000204839523, 7.188101187499999156 ) ) ;
#104799 = CARTESIAN_POINT ( 'NONE',  ( 0.000000000000000000, 0.000000000000000000, 0.000000000000000000 ) ) ;
#104801 = ADVANCED_FACE ( 'NONE', ( #20810 ), #88229, .T. ) ;
#104800 = CARTESIAN_POINT ( 'NONE',  ( 7.412969500702210723, 41.14559805159964156, -68.91429205978418793 ) ) ;
#104802 = ADVANCED_FACE ( 'NONE', ( #88149 ), #20510, .F. ) ;
#104803 = VERTEX_POINT ( 'NONE', #53644 ) ;
#104804 = AXIS2_PLACEMENT_3D ( 'NONE', #47970, #6988, #39907 ) ;
#104805 =( GEOMETRIC_REPRESENTATION_CONTEXT ( 3 ) GLOBAL_UNCERTAINTY_ASSIGNED_CONTEXT ( ( #4093 ) ) GLOBAL_UNIT_ASSIGNED_CONTEXT ( ( #55373, #23583, #87750 ) ) REPRESENTATION_CONTEXT ( 'NONE', 'WORKASPACE' ) );
#104807 = ORIENTED_EDGE ( 'NONE', *, *, #99487, .T. ) ;
#104806 = CARTESIAN_POINT ( 'NONE',  ( -37.56673239365849781, 25.47613764497371136, 13.45617127781066280 ) ) ;
#104808 = CARTESIAN_POINT ( 'NONE',  ( 80.62625263358452798, -46.43735505546275988, 158.8973765016157813 ) ) ;
#104809 = LINE ( 'NONE', #22859, #93688 ) ;
#104810 = ORIENTED_EDGE ( 'NONE', *, *, #16465, .T. ) ;
#104811 = CARTESIAN_POINT ( 'NONE',  ( -12.50000000000000888, 33.93135344289294864, -52.79621944607910677 ) ) ;
#104812 = CARTESIAN_POINT ( 'NONE',  ( -14.83962450835064928, 1.409789280633743314, -2.191244623882634635 ) ) ;
#104813 = CARTESIAN_POINT ( 'NONE',  ( 7.188101187500000933, -11.56250000204838635, -2.977408999572650483 ) ) ;
#104814 = CARTESIAN_POINT ( 'NONE',  ( -8.012931681025682785E-15, -7.321656987762868773, 3.318518101603009196 ) ) ;
#104815 = CARTESIAN_POINT ( 'NONE',  ( -57.91314980999670325, -57.67646044164155228, 100.3416927154360536 ) ) ;
#104816 = B_SPLINE_SURFACE_WITH_KNOTS ( 'NONE', 3, 3, ( 
 ( #70364, #88144, #87087, #104302 ),
 ( #103259, #47657, #63346, #55733 ),
 ( #73916, #14224, #32966, #78973 ),
 ( #38540, #106785, #24870, #79506 ),
 ( #12633, #21839, #6138, #96243 ),
 ( #62287, #22373, #95178, #8123 ),
 ( #21309, #13162, #62808, #65837 ),
 ( #70888, #98717, #41035, #46090 ),
 ( #54678, #39066, #86570, #103780 ),
 ( #29922, #55217, #71947, #95697 ),
 ( #87615, #104851, #30994, #63876 ),
 ( #45567, #96765, #78439, #49646 ),
 ( #92767, #91200, #51227, #82554 ),
 ( #100324, #75519, #9710, #43165 ),
 ( #524, #35100, #34039, #90649 ),
 ( #84153, #33487, #68511, #42620 ),
 ( #16755, #2148, #9173, #83086 ),
 ( #66365, #99247, #1613, #27016 ),
 ( #84684, #74975, #18376, #10252 ),
 ( #34575, #50686, #8655, #76046 ),
 ( #67448, #17839, #58273, #59360 ),
 ( #2690, #50180, #42086, #83604 ),
 ( #101403, #26485, #74445, #41562 ),
 ( #92222, #58826, #25415, #59895 ),
 ( #91718, #17307, #67966, #1065 ),
 ( #66912, #99796, #18928, #100857 ),
 ( #51770, #10769, #25967, #43687 ),
 ( #76575, #35641, #57727, #12896 ),
 ( #45300, #12374, #53385, #103517 ),
 ( #78180, #45825, #29156, #38285 ),
 ( #78697, #102464, #13429, #60955 ),
 ( #93312, #77662, #4829, #3775 ),
 ( #86302, #4297, #21566, #101921 ),
 ( #69047, #5367, #62541, #93840 ),
 ( #71149, #36710, #28611, #62028 ),
 ( #60436, #46350, #70093, #70627 ),
 ( #94384, #37232, #79240, #53897 ),
 ( #27557, #21058, #37764, #61494 ),
 ( #20003, #102997, #87352, #29671 ),
 ( #94921, #86827, #95428, #54407 ),
 ( #28081, #69574, #19468, #20546 ),
 ( #52304, #85213, #11303, #44232 ),
 ( #52844, #77122, #3235, #36179 ),
 ( #85768, #11842, #44773, #6400 ),
 ( #106153, #46869, #57075, #81873 ),
 ( #105633, #38796, #32309, #56538 ),
 ( #98075, #31774, #72216, #47916 ),
 ( #7999, #40908, #63070, #104039 ),
 ( #105118, #30178, #104573, #23158 ),
 ( #95970, #31260, #64146, #22094 ),
 ( #23693, #40371, #80287, #54949 ),
 ( #97016, #87877, #64654, #30727 ),
 ( #47394, #13959, #65182, #80824 ),
 ( #6937, #89990, #97529, #48978 ),
 ( #88410, #55994, #16097, #79767 ),
 ( #5872, #71666, #39335, #89469 ),
 ( #88935, #63614, #15026, #96503 ),
 ( #15563, #22638, #55473, #39858 ),
 ( #72731, #14481, #48452, #81345 ),
 ( #7457, #73250, #24227, #73795 ),
 ( #51648, #32842, #84572, #41965 ),
 ( #25842, #34454, #106692, #18251 ),
 ( #99124, #65719, #49521, #8529 ),
 ( #43044, #57598, #100733, #91075 ),
 ( #24751, #75395, #74326, #58700 ),
 ( #90521, #34979, #17709, #75932 ),
 ( #59769, #1492, #18804, #66241 ) ),
 .UNSPECIFIED., .F., .F., .F.,
 ( 4, 3, 3, 3, 3, 3, 3, 3, 3, 3, 3, 3, 3, 3, 3, 3, 3, 3, 3, 3, 3, 3, 4 ),
 ( 4, 4 ),
 ( 0.4267139204576358424, 0.4312935645218702874, 0.4358732085861046768, 0.4404528526503390662, 0.4450324967145734556, 0.4541917848430422344, 0.4633510729715110132, 0.4725103610999797921, 0.4816696492284485709, 0.4908289373569173497, 0.4954085814211517391, 0.4999882254853861285, 0.5045678695496205179, 0.5091475136138550184, 0.5183068017423237972, 0.5274660898707925760, 0.5366253779992613548, 0.5457846661277301337, 0.5549439542561989125, 0.5595235983204333019, 0.5641032423846676913, 0.5686828864489020807, 0.5732625305131364701 ),
 ( 0.03623606276729821052, 1.318162535682649183 ),
 .UNSPECIFIED. ) ;
#104817 = CARTESIAN_POINT ( 'NONE',  ( 16.55832830662598454, 294.5717066613688075, 1.877661829258160164 ) ) ;
#104818 = EDGE_CURVE ( 'NONE', #76724, #50280, #12116, .T. ) ;
#104819 = ORIENTED_EDGE ( 'NONE', *, *, #74065, .T. ) ;
#104820 = AXIS2_PLACEMENT_3D ( 'NONE', #102468, #84687, #28615 ) ;
#104821 = CARTESIAN_POINT ( 'NONE',  ( 0.000000000000000000, -80.00000000000000000, 27.00000000000000000 ) ) ;
#104822 = DIRECTION ( 'NONE',  ( 1.000000000000000000, 1.224606353822377258E-16, 0.000000000000000000 ) ) ;
#104823 = AXIS2_PLACEMENT_3D ( 'NONE', #20205, #85425, #59565 ) ;
#104824 = CARTESIAN_POINT ( 'NONE',  ( -9.999952458099484076, 81.00011885476135376, 0.2653554233229110659 ) ) ;
#104825 = ADVANCED_FACE ( 'NONE', ( #95706, #96253 ), #86575, .T. ) ;
#104826 = DIRECTION ( 'NONE',  ( 0.000000000000000000, 0.000000000000000000, 1.000000000000000000 ) ) ;
#104827 = ORIENTED_EDGE ( 'NONE', *, *, #30835, .F. ) ;
#104828 = CARTESIAN_POINT ( 'NONE',  ( -5.656854249492381470, -14.75000000409677092, 5.656854249492379694 ) ) ;
#104829 = CARTESIAN_POINT ( 'NONE',  ( -11.21238143379541619, -14.07322973648245856, 31.83197821777864078 ) ) ;
#104830 = CARTESIAN_POINT ( 'NONE',  ( -40.61984019992077322, 488.7256223871871725, 10.90533736068143433 ) ) ;
#104831 = AXIS2_PLACEMENT_3D ( 'NONE', #20445, #52743, #37133 ) ;
#104832 = CARTESIAN_POINT ( 'NONE',  ( 1.637502573363885733E-19, 51.26930509877138320, -10.24999999999999822 ) ) ;
#104834 = ADVANCED_FACE ( 'NONE', ( #32584 ), #61955, .F. ) ;
#104833 = B_SPLINE_CURVE_WITH_KNOTS ( 'NONE', 3,
 ( #43277, #69164, #102034, #76162, #50294, #92881, #83197, #9294, #42204, #75088, #67030, #94503, #53494, #95033, #55062, #37877, #87992, #78816 ),
 .UNSPECIFIED., .F., .F.,
 ( 4, 2, 2, 2, 2, 2, 2, 2, 4 ),
 ( 8.673617379884035472E-19, 0.003013683243355653411, 0.004520524865033480333, 0.005273945675872394011, 0.006027366486711306821, 0.007534208108389134177, 0.009041049730066960666, 0.01054789135174478976, 0.01205473297342261538 ),
 .UNSPECIFIED. ) ;
#104835 = CIRCLE ( 'NONE', #23951, 3.000000000000000000 ) ;
#104836 = CARTESIAN_POINT ( 'NONE',  ( -9.220915120640585272, 86.04454886432084493, -3.870126578504838655 ) ) ;
#104837 = CARTESIAN_POINT ( 'NONE',  ( 4.331367822450267191, 52.16488944962013363, 6.474629951035481668 ) ) ;
#104838 = APPLICATION_PROTOCOL_DEFINITION ( 'draft international standard', 'automotive_design', 1998, #71366 ) ;
#104839 = CARTESIAN_POINT ( 'NONE',  ( -9.843039827103243766, 33.59083502508334362, -1.781495459429555339 ) ) ;
#104840 = ORIENTED_EDGE ( 'NONE', *, *, #64647, .T. ) ;
#104841 = CARTESIAN_POINT ( 'NONE',  ( 10.45210760954369711, 43.22598471715434698, 15.39953001771810648 ) ) ;
#104842 =( NAMED_UNIT ( * ) SI_UNIT ( $, .STERADIAN. ) SOLID_ANGLE_UNIT ( ) );
#104843 = CARTESIAN_POINT ( 'NONE',  ( 38.58349330513380693, 1.593028355512270567E-15, 0.000000000000000000 ) ) ;
#104844 = CARTESIAN_POINT ( 'NONE',  ( -46.00000000000000000, 461.8824355611604915, 11.41562375508724081 ) ) ;
#104845 = CARTESIAN_POINT ( 'NONE',  ( -62.66006049324404614, -30.00000000000001066, 73.77690815432163163 ) ) ;
#104846 = CARTESIAN_POINT ( 'NONE',  ( 7.500000000000007105, 42.00000000000000711, -62.89165061482971453 ) ) ;
#104847 = EDGE_LOOP ( 'NONE', ( #31745, #5154, #92401, #95867 ) ) ;
#104848 = DIRECTION ( 'NONE',  ( -1.000000000000000000, -0.000000000000000000, -0.000000000000000000 ) ) ;
#104849 = CARTESIAN_POINT ( 'NONE',  ( 92.90827380281179160, -57.61735079984537578, 204.4405232865525477 ) ) ;
#104850 = TOROIDAL_SURFACE ( 'NONE', #96242, 7.500000000000006217, 5.000000000000000000 ) ;
#104851 = CARTESIAN_POINT ( 'NONE',  ( 59.93292360988266410, -47.40898519424397506, -27.52549038968009043 ) ) ;
#104852 = VECTOR ( 'NONE', #80781, 1000.000000000000000 ) ;
#104853 = CARTESIAN_POINT ( 'NONE',  ( 33.77559172535807619, 464.7834715296606305, 7.192701217093271815 ) ) ;
#104854 = CARTESIAN_POINT ( 'NONE',  ( -14.87468076902975334, 23.07153947553970497, -1.073492826241112086 ) ) ;
#104855 = CARTESIAN_POINT ( 'NONE',  ( -6.276528120735480165, 53.84035791979297159, 6.497148600190744361 ) ) ;
#104856 = CARTESIAN_POINT ( 'NONE',  ( -72.92009701100754171, -59.99999999999999289, 161.7471689223172007 ) ) ;
#104857 = COLOUR_RGB ( '', 0.08235294, 0.09019608, 0.10196078) ;
#104858 = CARTESIAN_POINT ( 'NONE',  ( -35.96492786661492858, 302.4488314805894902, -8.278427239160079054 ) ) ;
#104859 = DIRECTION ( 'NONE',  ( -1.000000000000000000, -1.224606353822377258E-16, -0.000000000000000000 ) ) ;
#104860 = CARTESIAN_POINT ( 'NONE',  ( -23.38163988261890225, 49.99999999999999289, 60.94087333798560735 ) ) ;
#104861 = CARTESIAN_POINT ( 'NONE',  ( -85.22359929980800075, -42.93809111955054192, 186.3718570108496237 ) ) ;
#104862 = EDGE_LOOP ( 'NONE', ( #64117, #81465, #84154, #31325, #44542 ) ) ;
#104863 = CARTESIAN_POINT ( 'NONE',  ( 36.71071896821285208, 382.3218912538050063, 5.272091887305267122 ) ) ;
#104864 = ORIENTED_EDGE ( 'NONE', *, *, #101860, .F. ) ;
#104865 = CARTESIAN_POINT ( 'NONE',  ( -7.002619243997879828, -11.05007318013818995, -3.868708944012998252 ) ) ;
#104866 = B_SPLINE_CURVE_WITH_KNOTS ( 'NONE', 3,
 ( #79611, #87197, #5211, #69422, #87729, #12221, #13807, #94223, #102842, #5726, #38142, #46720, #38650, #13274, #95287, #12751, #45151, #70996, #102305, #78032, #103886, #78554, #71516, #96354, #104416, #4150, #30562, #63461, #22485, #85610, #94769, #11684, #4683, #37079, #69945, #29010, #20918 ),
 .UNSPECIFIED., .F., .F.,
 ( 4, 2, 2, 2, 1, 1, 1, 1, 1, 1, 2, 2, 2, 2, 1, 1, 1, 1, 1, 1, 1, 2, 2, 2, 4 ),
 ( 0.000000000000000000, 0.1250000000000049405, 0.1875000000000073552, 0.2187500000000086042, 0.2343750000000092704, 0.2421875000000095757, 0.2460937500000097145, 0.2480468750000097422, 0.2490234375000097422, 0.2495117187500097422, 0.2497558593750097700, 0.2500000000000097700, 0.3750000000000363598, 0.4375000000000498490, 0.4687500000000565659, 0.4843750000000598965, 0.4921875000000616174, 0.4960937500000625056, 0.4980468750000630052, 0.4990234375000631162, 0.4995117187500632827, 0.4997558593750633382, 0.5000000000000633937, 0.7500000000000316414, 1.000000000000000000 ),
 .UNSPECIFIED. ) ;
#104867 = EDGE_CURVE ( 'NONE', #21082, #80415, #61862, .T. ) ;
#104868 = CARTESIAN_POINT ( 'NONE',  ( -13.99999999999998401, 59.99999999999999289, 6.999999999999989342 ) ) ;
#104869 = CARTESIAN_POINT ( 'NONE',  ( 42.19618372163381537, 487.7264399052799604, 8.629926728122889301 ) ) ;
#104870 = AXIS2_PLACEMENT_3D ( 'NONE', #21711, #13035, #96634 ) ;
#104871 = CARTESIAN_POINT ( 'NONE',  ( 0.5805565836007581249, -3.752776749732553263, 6.499999999999999112 ) ) ;
#104872 = EDGE_CURVE ( 'NONE', #95845, #13222, #45035, .T. ) ;
#104873 = DIRECTION ( 'NONE',  ( -1.000000000000000000, -0.000000000000000000, -0.000000000000000000 ) ) ;
#104874 = CONICAL_SURFACE ( 'NONE', #6692, 5.000000000000001776, 0.9599310885968803664 ) ;
#104875 = ORIENTED_EDGE ( 'NONE', *, *, #29791, .T. ) ;
#104876 = SURFACE_STYLE_USAGE ( .BOTH. , #6157 ) ;
#104877 = CARTESIAN_POINT ( 'NONE',  ( -0.5984201754795734907, -8.314755988442767531, -0.7022220667781350345 ) ) ;
#104878 = EDGE_CURVE ( 'NONE', #93427, #35284, #75117, .T. ) ;
#104879 = CARTESIAN_POINT ( 'NONE',  ( -13.50000000000000000, 7.794228634059933825, -1.205771365940051520 ) ) ;
#104880 = AXIS2_PLACEMENT_3D ( 'NONE', #51848, #42702, #99872 ) ;
#104881 = CARTESIAN_POINT ( 'NONE',  ( -33.20892452561020036, 484.6201576160080435, 4.300277591919697606 ) ) ;
#104882 = ADVANCED_FACE ( 'NONE', ( #34179 ), #43304, .T. ) ;
#104883 = CIRCLE ( 'NONE', #25697, 10.00000000000000000 ) ;
#104884 = CARTESIAN_POINT ( 'NONE',  ( 92.19440588371723777, -59.99999999999994316, -19.86251273113072102 ) ) ;
#104885 = CARTESIAN_POINT ( 'NONE',  ( -77.88326922906453831, -53.37685894332580716, 147.1956358302255410 ) ) ;
#104886 = ORIENTED_EDGE ( 'NONE', *, *, #5200, .T. ) ;
#104887 = CARTESIAN_POINT ( 'NONE',  ( 35.98705420554111356, -30.00000000000000355, 43.73599804831894033 ) ) ;
#104888 = CARTESIAN_POINT ( 'NONE',  ( 73.06332208692298025, -57.64923196330578037, 181.6867478007702630 ) ) ;
#104889 = DIRECTION ( 'NONE',  ( -1.000000000000000000, -1.224606353822377258E-16, -0.000000000000000000 ) ) ;
#104891 = CIRCLE ( 'NONE', #30848, 3.400000000000000355 ) ;
#104890 = CARTESIAN_POINT ( 'NONE',  ( 40.82495241567565358, 312.4806794415787294, -5.803827984348647107 ) ) ;
#104892 = CARTESIAN_POINT ( 'NONE',  ( -12.04654684923174912, 10.50803151810102598, 9.704396884749211694 ) ) ;
#104893 = ORIENTED_EDGE ( 'NONE', *, *, #54811, .T. ) ;
#104894 = CONICAL_SURFACE ( 'NONE', #15337, 4.172000000000001485, 0.9599310885968750373 ) ;
#104895 = CARTESIAN_POINT ( 'NONE',  ( -23.21751746555247919, 25.98869614573810694, 30.70617127781050471 ) ) ;
#104896 = LINE ( 'NONE', #6714, #92677 ) ;
#104898 = CARTESIAN_POINT ( 'NONE',  ( -103.0586439431804564, -60.15481352663451986, 134.7074848548440400 ) ) ;
#104897 = PLANE ( 'NONE',  #57014 ) ;
#104899 = CARTESIAN_POINT ( 'NONE',  ( -7.188101187500001821, -18.50000000204838457, -2.977408999572651371 ) ) ;
#104900 = ADVANCED_FACE ( 'NONE', ( #67058 ), #70812, .F. ) ;
#104901 = CARTESIAN_POINT ( 'NONE',  ( -1.469576158976823947E-15, -20.56250000409676915, 8.000000000000000000 ) ) ;
#104902 = CARTESIAN_POINT ( 'NONE',  ( -8.000000000000000000, -23.74999999999999289, -9.797174393178825657E-16 ) ) ;
#104903 = CARTESIAN_POINT ( 'NONE',  ( 0.3379698803298797349, 34.18408244316042044, 29.71496935741117085 ) ) ;
#104904 = DIRECTION ( 'NONE',  ( 1.000000000000000000, 1.224606353822377258E-16, 0.000000000000000000 ) ) ;
#104905 = SURFACE_SIDE_STYLE ('',( #39114 ) ) ;
#104906 = B_SPLINE_CURVE_WITH_KNOTS ( 'NONE', 3,
 ( #85745, #35613, #60409, #11275, #77095, #3215, #11816, #34016, #44748, #1042, #99774, #18354, #75494, #25944, #91699, #2123, #92201, #1590, #17812, #42597, #50663, #83579, #67425, #9687, #67945, #100302, #59330, #84128, #51207, #100826, #59872, #92746, #38264, #63045 ),
 .UNSPECIFIED., .F., .F.,
 ( 4, 2, 2, 2, 2, 2, 2, 2, 2, 2, 2, 2, 2, 2, 2, 2, 4 ),
 ( 0.000000000000000000, 0.06250000000000000000, 0.1250000000000000000, 0.1875000000000000000, 0.2500000000000000000, 0.3125000000000000000, 0.3750000000000000000, 0.4375000000000000000, 0.5000000000000000000, 0.5625000000000000000, 0.6250000000000000000, 0.6875000000000000000, 0.7500000000000000000, 0.8125000000000000000, 0.8750000000000000000, 0.9375000000000000000, 1.000000000000000000 ),
 .UNSPECIFIED. ) ;
#104907 = VECTOR ( 'NONE', #40468, 1000.000000000000000 ) ;
#104908 = EDGE_LOOP ( 'NONE', ( #90693, #33482, #76678, #34992, #63090 ) ) ;
#104909 = CARTESIAN_POINT ( 'NONE',  ( -7.040972322291190189, 41.74416393942964731, -59.82830748482982841 ) ) ;
#104911 = CARTESIAN_POINT ( 'NONE',  ( 27.49024895849569106, -29.05222164557826758, 30.53773838945769725 ) ) ;
#104910 = CARTESIAN_POINT ( 'NONE',  ( -21.36131896786188378, -60.00000000000002132, 42.72829597934922674 ) ) ;
#104912 = CARTESIAN_POINT ( 'NONE',  ( -23.84475511469840470, 25.80478802837803443, 30.86282763156348707 ) ) ;
#104913 = CLOSED_SHELL ( 'NONE', ( #61100, #51253, #56334, #79916, #61999, #45788, #37095, #23856, #16370, #14978, #31419, #48112, #26978, #71449, #99582, #62823, #80126, #38379, #18314, #99150, #23488, #97817, #34878, #46374, #85335, #28886, #58390, #5751, #10229, #84424, #66333, #83465, #45798, #92323, #94044, #19861, #19338, #105615, #84896, #103729, #97248, #60927, #9691, #91316, #101063, #22867, #105611, #96420, #33801, #19829, #93886, #33865, #89651, #52670, #4059, #67686, #66172, #63035, #27666, #59712, #22435, #71749, #67849, #64499, #30246, #21155, #100783, #95907, #103881, #29414, #77217, #91539, #75265, #29194, #100316, #1619, #12353, #6226, #80383, #25721, #82700, #61318, #62960, #63667, #104046, #59489, #11423, #71062, #22117, #74618, #30236, #44252, #72595, #1027, #8383, #92230, #8810, #40377, #31835, #12777, #93596, #58551, #95644, #72855, #76431, #105441, #87340, #5743, #42817, #86974, #95935, #70819, #104207, #80803, #35957, #67778, #103712, #62035, #8606, #15517, #23558, #103284, #41947, #106013, #60561, #86726, #31467, #6214, #50651, #74850, #102730, #14248, #45937, #76160, #20906, #22396, #47248, #46462, #84952, #25238, #76069, #35801, #75939, #36765, #40294, #66384, #101731, #89647, #101228, #54413, #30995, #20002, #4062, #94850, #104348, #63253, #105777, #96247, #2086, #37763, #10760, #16542, #18096, #56589, #75285, #10901, #77558 ) ) ;
#104914 = ORIENTED_EDGE ( 'NONE', *, *, #21720, .F. ) ;
#104915 = ORIENTED_EDGE ( 'NONE', *, *, #73533, .F. ) ;
#104917 = CARTESIAN_POINT ( 'NONE',  ( -0.6468308027566224139, 43.23255578745401095, -18.58280467064760799 ) ) ;
#104916 = CARTESIAN_POINT ( 'NONE',  ( 0.000000000000000000, -3.035766082959412415E-15, -13.99700487351915612 ) ) ;
#104918 = SURFACE_STYLE_FILL_AREA ( #98398 ) ;
#104919 = CARTESIAN_POINT ( 'NONE',  ( 7.195949543451931163, 41.08281217721444278, -58.60025093677088392 ) ) ;
#104920 = CIRCLE ( 'NONE', #1559, 7.000000000000000000 ) ;
#104921 = CARTESIAN_POINT ( 'NONE',  ( -8.000000000000000000, -19.43750000409677270, -9.797174393178825657E-16 ) ) ;
#104922 = CARTESIAN_POINT ( 'NONE',  ( 30.59999999999999787, -3.309499999999999886, 4.475777889183790779E-16 ) ) ;
#104923 = CARTESIAN_POINT ( 'NONE',  ( 10.51296777078104050, 50.00000000000000000, -92.64705882352942012 ) ) ;
#104924 = VERTEX_POINT ( 'NONE', #43826 ) ;
#104925 = CIRCLE ( 'NONE', #42931, 3.309500000000007880 ) ;
#104926 = CARTESIAN_POINT ( 'NONE',  ( 32.09297087671797755, -60.00000000000002132, -40.66494470579936404 ) ) ;
#104927 = CARTESIAN_POINT ( 'NONE',  ( 88.81459683227794244, -29.99999999999995737, 188.4117534872304418 ) ) ;
#104928 = CARTESIAN_POINT ( 'NONE',  ( 0.000000000000000000, 61.34242035161803841, -9.357204421225127078 ) ) ;
#104929 = CARTESIAN_POINT ( 'NONE',  ( 0.000000000000000000, -5.000000000000000888, -73.00000000000001421 ) ) ;
#104930 = CARTESIAN_POINT ( 'NONE',  ( 47.90347347824236834, 10.05236241843094014, -16.85535821593550665 ) ) ;
#104931 = ORIENTED_EDGE ( 'NONE', *, *, #44547, .F. ) ;
#104932 = ORIENTED_EDGE ( 'NONE', *, *, #86010, .T. ) ;
#104933 = ORIENTED_EDGE ( 'NONE', *, *, #24389, .T. ) ;
#104934 = CARTESIAN_POINT ( 'NONE',  ( 44.26831907014823742, 485.5169161718123974, 3.139294003717259418 ) ) ;
#104935 = CARTESIAN_POINT ( 'NONE',  ( 41.36650669486618881, 1.474610560812782335E-15, 0.000000000000000000 ) ) ;
#104936 = CARTESIAN_POINT ( 'NONE',  ( 29.22860602677112851, 312.6791165392893390, 12.31020644618178572 ) ) ;
#104937 = CARTESIAN_POINT ( 'NONE',  ( -42.33059488474484766, 332.4056956521847610, 7.101971215149171179 ) ) ;
#104938 = CARTESIAN_POINT ( 'NONE',  ( -31.90195216159215263, 465.6468698803304846, 10.69263942007498969 ) ) ;
#104939 = FACE_OUTER_BOUND ( 'NONE', #70468, .T. ) ;
#104940 = DIRECTION ( 'NONE',  ( -0.000000000000000000, -1.000000000000000000, -0.000000000000000000 ) ) ;
#104941 = VERTEX_POINT ( 'NONE', #76717 ) ;
#104943 = EDGE_CURVE ( 'NONE', #29420, #4192, #31194, .T. ) ;
#104942 = CARTESIAN_POINT ( 'NONE',  ( 0.000000000000000000, 200.0000000000000000, 0.000000000000000000 ) ) ;
#104944 = ORIENTED_EDGE ( 'NONE', *, *, #86469, .F. ) ;
#104945 = DIRECTION ( 'NONE',  ( 0.000000000000000000, -1.000000000000000000, 0.000000000000000000 ) ) ;
#104946 = FILL_AREA_STYLE_COLOUR ( '', #69434 ) ;
#104947 = CARTESIAN_POINT ( 'NONE',  ( -38.81358894280032956, 485.1131561813190274, -4.191378885295818257 ) ) ;
#104948 = CIRCLE ( 'NONE', #17094, 5.000000000000001776 ) ;
#104949 = AXIS2_PLACEMENT_3D ( 'NONE', #78913, #95122, #31839 ) ;
#104950 = CARTESIAN_POINT ( 'NONE',  ( 0.5047266530460114975, 295.8573157252483270, -10.00013740465520762 ) ) ;
#104951 = CARTESIAN_POINT ( 'NONE',  ( 64.69054239873878487, -29.05368727968382458, 79.89853205579872508 ) ) ;
#104952 = VERTEX_POINT ( 'NONE', #83746 ) ;
#104953 = CARTESIAN_POINT ( 'NONE',  ( 41.92560882005241041, 464.5504518700566905, 16.85555372449807265 ) ) ;
#104954 = CARTESIAN_POINT ( 'NONE',  ( 0.000000000000000000, 0.000000000000000000, 66.50000000000000000 ) ) ;
#104955 = ADVANCED_FACE ( 'NONE', ( #17452 ), #91337, .T. ) ;
#104956 = ORIENTED_EDGE ( 'NONE', *, *, #81711, .T. ) ;
#104957 = AXIS2_PLACEMENT_3D ( 'NONE', #64034, #97964, #56424 ) ;
#104958 = CARTESIAN_POINT ( 'NONE',  ( 46.79790428518975176, 18.85533329945889847, 15.37169442865920033 ) ) ;
#104959 = AXIS2_PLACEMENT_3D ( 'NONE', #50634, #18872, #66314 ) ;
#104960 = DIRECTION ( 'NONE',  ( -1.000000000000000000, -1.224606353822377258E-16, -0.000000000000000000 ) ) ;
#104961 = CARTESIAN_POINT ( 'NONE',  ( -8.000000000000001776, -32.84375000409677625, 3.313708498984758943 ) ) ;
#104962 = CARTESIAN_POINT ( 'NONE',  ( 86.68877158589015153, -20.67351136403616962, 184.9441422176963385 ) ) ;
#104963 = EDGE_CURVE ( 'NONE', #13998, #47451, #29513, .T. ) ;
#104964 = CIRCLE ( 'NONE', #34400, 4.000000000000001776 ) ;
#104965 = SURFACE_STYLE_USAGE ( .BOTH. , #6240 ) ;
#104966 = ADVANCED_FACE ( 'NONE', ( #667 ), #67351, .T. ) ;
#104967 = CARTESIAN_POINT ( 'NONE',  ( -3.997663733872217406, 15.09624604205074938, 4.999999999999999112 ) ) ;
#104968 = FACE_OUTER_BOUND ( 'NONE', #6189, .T. ) ;
#104969 = CARTESIAN_POINT ( 'NONE',  ( 19.83463548332442983, 303.8035096162418540, 9.926734387303303819 ) ) ;
#104970 = ORIENTED_EDGE ( 'NONE', *, *, #26652, .F. ) ;
#104971 = LINE ( 'NONE', #81196, #71388 ) ;
#104972 = CARTESIAN_POINT ( 'NONE',  ( 99.17777777777777715, 1.023464760207051730E-14, 0.000000000000000000 ) ) ;
#104973 = CARTESIAN_POINT ( 'NONE',  ( 17.37359531700059634, -60.00000000000000711, 39.95162597743414068 ) ) ;
#104974 = CARTESIAN_POINT ( 'NONE',  ( -100.7567655553329757, -29.99999999999999645, 180.7204987279467048 ) ) ;
#104975 = CIRCLE ( 'NONE', #42915, 4.000000000000001776 ) ;
#104976 = DIRECTION ( 'NONE',  ( 0.000000000000000000, 0.000000000000000000, 1.000000000000000000 ) ) ;
#104977 = CARTESIAN_POINT ( 'NONE',  ( 36.41245709655431284, -57.69609435492582605, 50.68243955302485659 ) ) ;
#104979 = DIRECTION ( 'NONE',  ( -1.000000000000000000, -1.224606353822377258E-16, -0.000000000000000000 ) ) ;
#104978 = CARTESIAN_POINT ( 'NONE',  ( 71.14984002819953446, 6.856755485862130937E-15, 0.000000000000000000 ) ) ;
#104981 = CARTESIAN_POINT ( 'NONE',  ( 23.21751746555303342, 28.11705169068991594, 30.70617127781016720 ) ) ;
#104980 = AXIS2_PLACEMENT_3D ( 'NONE', #103177, #104755, #55644 ) ;
#104982 = CARTESIAN_POINT ( 'NONE',  ( -32.09335762069173370, 464.8098810386746322, 11.80769741171398302 ) ) ;
#104983 = DIRECTION ( 'NONE',  ( 0.000000000000000000, 0.000000000000000000, 1.000000000000000000 ) ) ;
#104984 = CARTESIAN_POINT ( 'NONE',  ( -20.99456667357952000, -60.00000000000000000, 40.35920817678867678 ) ) ;
#104985 = CARTESIAN_POINT ( 'NONE',  ( 0.4783642039767228016, -15.39516892388123637, -35.22788256086853664 ) ) ;
#104986 = CIRCLE ( 'NONE', #24092, 4.000000000000007105 ) ;
#104987 = B_SPLINE_CURVE_WITH_KNOTS ( 'NONE', 3,
 ( #3880, #93954, #3346, #78810, #36810, #69673, #69156, #4940, #68076, #76689, #53489, #86414, #35749, #28718, #60538, #61600, #60015, #94495, #19040, #51877, #93424, #19578, #85326, #28189, #52406, #11412, #77230, #99093, #57043, #106122 ),
 .UNSPECIFIED., .F., .F.,
 ( 4, 2, 2, 2, 2, 2, 2, 2, 2, 2, 2, 2, 2, 2, 4 ),
 ( 0.0007661829082509325969, 0.0009991316538646626087, 0.001232080399478392404, 0.001697977890705861101, 0.002163875381933329581, 0.002629772873160798278, 0.003561567855615739575, 0.004493362838070681306, 0.005425157820525623037, 0.006356952802980563033, 0.006822850294208039103, 0.007288747785435514305, 0.007754645276662990375, 0.007987594022276733180, 0.008220542767890477720 ),
 .UNSPECIFIED. ) ;
#104988 = VERTEX_POINT ( 'NONE', #77267 ) ;
#104989 = CARTESIAN_POINT ( 'NONE',  ( -3.040531029381596806, -49.16841272187355116, 104.0108099329909095 ) ) ;
#104990 = CARTESIAN_POINT ( 'NONE',  ( -12.53346734362791359, -49.92094994888364567, 32.26888292110559320 ) ) ;
#104992 = CARTESIAN_POINT ( 'NONE',  ( 39.08699041849416034, 460.7998460666120764, 2.161775044689363767 ) ) ;
#104991 = CARTESIAN_POINT ( 'NONE',  ( -86.83940835675045378, -60.00000000000007105, -10.29891589400428309 ) ) ;
#104993 = ORIENTED_EDGE ( 'NONE', *, *, #67531, .T. ) ;
#104994 = CARTESIAN_POINT ( 'NONE',  ( 25.88305778034912308, 35.08525496124520515, 8.493710876074011651 ) ) ;
#104995 = CARTESIAN_POINT ( 'NONE',  ( -7.334017076212031583, -3.381213663715922468, -18.44266608209038338 ) ) ;
#104996 = CARTESIAN_POINT ( 'NONE',  ( 43.52560348121181732, 486.7876442849059231, 7.034435017225325382 ) ) ;
#104997 = CIRCLE ( 'NONE', #46416, 1.000000000000000444 ) ;
#104998 = FACE_OUTER_BOUND ( 'NONE', #86052, .T. ) ;
#104999 = ADVANCED_FACE ( 'NONE', ( #93982 ), #58961, .F. ) ;
#105000 = CARTESIAN_POINT ( 'NONE',  ( -3.400000000000000355, 4.163799117101001052E-16, -3.012075477074183105 ) ) ;
#105001 = CARTESIAN_POINT ( 'NONE',  ( 72.06473877601102629, -59.99999999999999289, 154.7618788949081932 ) ) ;
#105002 = CARTESIAN_POINT ( 'NONE',  ( -1.097258412180344811, 54.05209286624712206, -8.380528997215506593 ) ) ;
#105003 = ORIENTED_EDGE ( 'NONE', *, *, #18780, .F. ) ;
#105004 = CARTESIAN_POINT ( 'NONE',  ( 44.08840282922849241, 485.7747746244180007, 4.178803824087734320 ) ) ;
#105005 = LINE ( 'NONE', #55881, #47113 ) ;
#105007 = DIRECTION ( 'NONE',  ( 0.000000000000000000, 0.000000000000000000, 1.000000000000000000 ) ) ;
#105006 = CARTESIAN_POINT ( 'NONE',  ( 1.363418823244991529, -14.21045842199435150, 34.36840973699906954 ) ) ;
#105008 = SURFACE_STYLE_FILL_AREA ( #14914 ) ;
#105009 = CARTESIAN_POINT ( 'NONE',  ( -4.642888266381866913, -2.342832151813632802, 102.5319024079573751 ) ) ;
#105010 = ORIENTED_EDGE ( 'NONE', *, *, #90940, .F. ) ;
#105011 = CARTESIAN_POINT ( 'NONE',  ( -25.27112035471596130, 306.2417877789772547, 10.47586605097270329 ) ) ;
#105012 = EDGE_CURVE ( 'NONE', #18921, #11593, #64322, .T. ) ;
#105013 = ORIENTED_EDGE ( 'NONE', *, *, #19065, .F. ) ;
#105014 = DIRECTION ( 'NONE',  ( -1.000000000000000000, -0.000000000000000000, -0.000000000000000000 ) ) ;
#105015 =( BOUNDED_SURFACE ( )  B_SPLINE_SURFACE ( 3, 2, ( 
 ( #94525, #79897, #61633 ),
 ( #80424, #88012, #104175 ),
 ( #103654, #71801, #79373 ),
 ( #72347, #53516, #46998 ),
 ( #104710, #95570, #30863 ),
 ( #14619, #47529, #6533 ),
 ( #39466, #105249, #20677 ),
 ( #54544, #62680, #78311 ),
 ( #38416, #86964, #86443 ),
 ( #63209, #37368, #96100 ) ),
 .UNSPECIFIED., .F., .F., .F. ) 
 B_SPLINE_SURFACE_WITH_KNOTS ( ( 4, 2, 2, 2, 4 ),
 ( 3, 3 ),
 ( -1.185673698477775140E-05, 0.001057471059733317183, 0.002126798856451412017, 0.003196126653169506851, 0.004265454449887602119 ),
 ( 0.000000000000000000, 1.000000000000000000 ),
 .UNSPECIFIED. ) 
 GEOMETRIC_REPRESENTATION_ITEM ( )  RATIONAL_B_SPLINE_SURFACE ( (
 ( 1.000000000000000000, 1.000000000000000000, 1.000000000000000000),
 ( 1.000000000000000000, 0.9999925199709330803, 1.000000000000000000),
 ( 1.000000000000000000, 0.9961033022472992604, 1.000000000000000000),
 ( 1.000000000000000000, 0.9800616282250097511, 1.000000000000000000),
 ( 1.000000000000000000, 0.9678427155945901195, 1.000000000000000000),
 ( 1.000000000000000000, 0.9345111840693876015, 1.000000000000000000),
 ( 1.000000000000000000, 0.9135791977929141883, 1.000000000000000000),
 ( 1.000000000000000000, 0.8625981283153052459, 1.000000000000000000),
 ( 1.000000000000000000, 0.8325406200923007871, 1.000000000000000000),
 ( 1.000000000000000000, 0.7974033994356889421, 1.000000000000000000) ) ) 
 REPRESENTATION_ITEM ( '' )  SURFACE ( )  );
#105016 = EDGE_CURVE ( 'NONE', #104028, #65683, #91686, .T. ) ;
#105017 = DIRECTION ( 'NONE',  ( 0.000000000000000000, 0.000000000000000000, 1.000000000000000000 ) ) ;
#105018 = CARTESIAN_POINT ( 'NONE',  ( 61.37206225042174879, -4.000000000000000000, 0.000000000000000000 ) ) ;
#105019 = ORIENTED_EDGE ( 'NONE', *, *, #48711, .F. ) ;
#105020 = CARTESIAN_POINT ( 'NONE',  ( 4.205882352941182845, -5.000000000000002665, -72.69916451482998809 ) ) ;
#105021 = CARTESIAN_POINT ( 'NONE',  ( 6.249254171376327882, -12.00724809823987549, 11.39149369528576017 ) ) ;
#105022 = CARTESIAN_POINT ( 'NONE',  ( -108.4957846533182675, -60.00000000000615330, 199.0410807392527772 ) ) ;
#105023 = CARTESIAN_POINT ( 'NONE',  ( 6.172076129340783091, 1.395179846520576694, -6.500000000000001776 ) ) ;
#105024 = PRESENTATION_LAYER_ASSIGNMENT (  '', '', ( #98015 ) ) ;
#105025 = CARTESIAN_POINT ( 'NONE',  ( 84.31499252833064872, -60.00000000000002132, 199.6929933629102152 ) ) ;
#105026 =( LENGTH_UNIT ( ) NAMED_UNIT ( * ) SI_UNIT ( .MILLI., .METRE. ) );
#105027 = DIRECTION ( 'NONE',  ( 0.000000000000000000, -1.000000000000000000, 0.000000000000000000 ) ) ;
#105029 = CARTESIAN_POINT ( 'NONE',  ( 13.76622771894575514, -60.35868451098616561, 34.04349415497945586 ) ) ;
#105028 = CARTESIAN_POINT ( 'NONE',  ( -109.4306967521916221, -29.99999999999999645, 166.0290040158848797 ) ) ;
#105030 = CARTESIAN_POINT ( 'NONE',  ( 82.55399726781115533, -38.00000000000001421, 6.763662827364390395 ) ) ;
#105031 = CARTESIAN_POINT ( 'NONE',  ( 0.000000000000000000, 0.9999999999999943379, 0.000000000000000000 ) ) ;
#105032 = VECTOR ( 'NONE', #80272, 1000.000000000000000 ) ;
#105033 = CARTESIAN_POINT ( 'NONE',  ( -44.20937707563757613, -53.34858502187538676, 46.33038334879231712 ) ) ;
#105034 = DIRECTION ( 'NONE',  ( 0.5000000000000014433, 0.8660254037844379305, -0.000000000000000000 ) ) ;
#105035 = ORIENTED_EDGE ( 'NONE', *, *, #92073, .T. ) ;
#105036 = CARTESIAN_POINT ( 'NONE',  ( 16.10099529212903846, 21.87266829489345454, 0.2127561331699810987 ) ) ;
#105037 = FACE_OUTER_BOUND ( 'NONE', #33573, .T. ) ;
#105038 =( NAMED_UNIT ( * ) SI_UNIT ( $, .STERADIAN. ) SOLID_ANGLE_UNIT ( ) );
#105039 = PRESENTATION_LAYER_ASSIGNMENT (  '', '', ( #24151 ) ) ;
#105040 = CARTESIAN_POINT ( 'NONE',  ( 6.818946241788777840, 304.7371849810256208, -9.024366745380079990 ) ) ;
#105041 = CARTESIAN_POINT ( 'NONE',  ( 31.14694070047868735, 432.3293837220155069, 24.29762062537629319 ) ) ;
#105042 = EDGE_LOOP ( 'NONE', ( #12186, #12584, #106044, #10897, #13184, #58026 ) ) ;
#105043 = CARTESIAN_POINT ( 'NONE',  ( -9.773816476656509877, -12.75255233517122022, 16.96466978235007161 ) ) ;
#105044 = ORIENTED_EDGE ( 'NONE', *, *, #89010, .T. ) ;
#105045 = CARTESIAN_POINT ( 'NONE',  ( 106.6412839208548036, -30.00000000000165912, 192.5192194241506627 ) ) ;
#105046 = CARTESIAN_POINT ( 'NONE',  ( 45.99999999999999289, 460.6999119684549555, 7.611097089574335506 ) ) ;
#105047 = CARTESIAN_POINT ( 'NONE',  ( 6.494545870870014781, 41.94144576370731414, -59.61320117837396282 ) ) ;
#105048 = CARTESIAN_POINT ( 'NONE',  ( 1.829579891623863529E-15, 10.71892156097790583, 14.93965356295127478 ) ) ;
#105049 = CARTESIAN_POINT ( 'NONE',  ( 87.55810224661499319, -30.00000000000000711, 73.94386861778465914 ) ) ;
#105050 = CIRCLE ( 'NONE', #41284, 4.000000000000000888 ) ;
#105051 = DIRECTION ( 'NONE',  ( -1.000000000000000000, -0.000000000000000000, -0.000000000000000000 ) ) ;
#105052 = EDGE_LOOP ( 'NONE', ( #75178, #10026 ) ) ;
#105053 = AXIS2_PLACEMENT_3D ( 'NONE', #62785, #13676, #97778 ) ;
#105054 = ORIENTED_EDGE ( 'NONE', *, *, #49072, .F. ) ;
#105055 = ORIENTED_EDGE ( 'NONE', *, *, #84286, .T. ) ;
#105056 = CARTESIAN_POINT ( 'NONE',  ( 0.000000000000000000, 4.898587196589413815E-16, -4.000000000000000888 ) ) ;
#105057 = CARTESIAN_POINT ( 'NONE',  ( 25.11650669486618881, 1.474610560812782335E-15, 0.000000000000000000 ) ) ;
#105058 = CARTESIAN_POINT ( 'NONE',  ( 33.58349330513379982, 1.593028355512270567E-15, 0.000000000000000000 ) ) ;
#105059 = ORIENTED_EDGE ( 'NONE', *, *, #81241, .F. ) ;
#105061 = EDGE_CURVE ( 'NONE', #10331, #43, #48609, .T. ) ;
#105060 = CARTESIAN_POINT ( 'NONE',  ( 103.5111111111111057, 4.172000000000019249, 5.109226446042768454E-16 ) ) ;
#105062 = AXIS2_PLACEMENT_3D ( 'NONE', #76910, #84483, #43492 ) ;
#105063 = ORIENTED_EDGE ( 'NONE', *, *, #4678, .T. ) ;
#105064 = CARTESIAN_POINT ( 'NONE',  ( 13.86650669486618881, -3.851859888774471706E-31, 4.000000000000000888 ) ) ;
#105065 = CARTESIAN_POINT ( 'NONE',  ( 78.47953390179775113, -38.63294422717142851, 189.6624935433154349 ) ) ;
#105066 = CARTESIAN_POINT ( 'NONE',  ( 13.12502261391177250, 8.285386694269465835, 8.822864485936415591 ) ) ;
#105067 = CARTESIAN_POINT ( 'NONE',  ( 84.14018061964620188, -45.28747372694517281, 0.6296579836999579571 ) ) ;
#105068 = CARTESIAN_POINT ( 'NONE',  ( 84.14737378976931836, -37.99999999999996447, 177.7231074054740532 ) ) ;
#105069 = CARTESIAN_POINT ( 'NONE',  ( 31.25856554251603470, 324.7076297242331293, 15.31063495038612565 ) ) ;
#105070 = CARTESIAN_POINT ( 'NONE',  ( -43.75010090113919148, 464.8337800386752292, 11.75004750935041109 ) ) ;
#105071 = CIRCLE ( 'NONE', #12048, 6.500000000000000888 ) ;
#105072 = FACE_OUTER_BOUND ( 'NONE', #18729, .T. ) ;
#105073 = CARTESIAN_POINT ( 'NONE',  ( -39.32386068306119142, 460.7288320239698578, 2.118193558184112923 ) ) ;
#105074 = CARTESIAN_POINT ( 'NONE',  ( 33.58349330513380693, 1.593028355512270962E-15, 0.000000000000000000 ) ) ;
#105075 = ORIENTED_EDGE ( 'NONE', *, *, #81408, .T. ) ;
#105076 = EDGE_CURVE ( 'NONE', #102006, #64162, #70764, .T. ) ;
#105077 = CARTESIAN_POINT ( 'NONE',  ( 17.23461538461538467, 1.411358822780289120E-15, 0.000000000000000000 ) ) ;
#105078 = CARTESIAN_POINT ( 'NONE',  ( -34.89951189943284504, 462.5771273340574226, 5.012025534192016352 ) ) ;
#105079 = DIRECTION ( 'NONE',  ( 0.000000000000000000, 1.000000000000000000, 0.000000000000000000 ) ) ;
#105080 = EDGE_LOOP ( 'NONE', ( #52774, #59727, #39818, #16109, #65642, #56005 ) ) ;
#105081 = LINE ( 'NONE', #97488, #85488 ) ;
#105082 = CARTESIAN_POINT ( 'NONE',  ( -32.84478897102435724, 300.3640702886290796, 3.177245060986884972 ) ) ;
#105083 = CARTESIAN_POINT ( 'NONE',  ( 9.833493305133801599, 1.593028355512270567E-15, 0.000000000000000000 ) ) ;
#105084 = PRESENTATION_STYLE_ASSIGNMENT (( #41397 ) ) ;
#105085 = CARTESIAN_POINT ( 'NONE',  ( -3.313708498984760720, -16.53124999999999289, -8.000000000000000000 ) ) ;
#105086 = DIRECTION ( 'NONE',  ( 0.9722532735310974727, 0.000000000000000000, -0.2339306993707007676 ) ) ;
#105087 = AXIS2_PLACEMENT_3D ( 'NONE', #56790, #73503, #14207 ) ;
#105088 = CARTESIAN_POINT ( 'NONE',  ( 0.000000000000000000, 9.797174393178825657E-16, -8.000000000000000000 ) ) ;
#105089 = EDGE_LOOP ( 'NONE', ( #70324, #71604, #69000, #99265, #2425, #68469, #75163 ) ) ;
#105090 = CARTESIAN_POINT ( 'NONE',  ( 86.24358644654743955, -21.22751543189874468, 178.4789263468928766 ) ) ;
#105091 = EDGE_CURVE ( 'NONE', #11535, #63343, #95154, .T. ) ;
#105092 = EDGE_CURVE ( 'NONE', #88621, #98079, #86304, .T. ) ;
#105093 = LINE ( 'NONE', #38260, #12495 ) ;
#105094 = ORIENTED_EDGE ( 'NONE', *, *, #44380, .T. ) ;
#105095 = CARTESIAN_POINT ( 'NONE',  ( 93.83744002707871346, -57.67473800415772445, 11.12884359937129730 ) ) ;
#105096 = DIRECTION ( 'NONE',  ( 0.000000000000000000, 0.000000000000000000, -1.000000000000000000 ) ) ;
#105097 = CYLINDRICAL_SURFACE ( 'NONE', #52381, 10.00000000000000178 ) ;
#105098 = CARTESIAN_POINT ( 'NONE',  ( 28.43946827300317892, 12.73388556380912817, 40.70676336658340944 ) ) ;
#105099 = EDGE_CURVE ( 'NONE', #12476, #52196, #30705, .T. ) ;
#105100 = AXIS2_PLACEMENT_3D ( 'NONE', #75431, #19907, #68421 ) ;
#105101 = CARTESIAN_POINT ( 'NONE',  ( 29.68315524077034340, 18.29184282782460969, 39.60535821593451544 ) ) ;
#105102 = CARTESIAN_POINT ( 'NONE',  ( 7.137815226408910974, -4.999999999999998224, 4.175893272575850190 ) ) ;
#105103 = LINE ( 'NONE', #57058, #67006 ) ;
#105105 = CARTESIAN_POINT ( 'NONE',  ( -11.77137377981709498, 11.34323235146788988, 9.877945527872393328 ) ) ;
#105104 = CARTESIAN_POINT ( 'NONE',  ( 37.46539396549699319, 482.0424347141847647, 15.05118261291089254 ) ) ;
#105106 = CARTESIAN_POINT ( 'NONE',  ( -15.39658166598003319, 44.03750247749371738, -5.597717089993270889 ) ) ;
#105107 = CARTESIAN_POINT ( 'NONE',  ( -28.35330149161957536, 36.33377328164552011, -8.699764177244842855 ) ) ;
#105108 = CARTESIAN_POINT ( 'NONE',  ( -25.43785777808176718, -28.36737569912000367, -30.30737543915739707 ) ) ;
#105109 = CARTESIAN_POINT ( 'NONE',  ( 19.29515645702225868, 1.482358050883964840E-15, 0.000000000000000000 ) ) ;
#105110 = CARTESIAN_POINT ( 'NONE',  ( -101.4594870179214894, -37.99999999999997868, 151.1679595334590260 ) ) ;
#105111 = EDGE_CURVE ( 'NONE', #62320, #74466, #12713, .T. ) ;
#105112 = ORIENTED_EDGE ( 'NONE', *, *, #93572, .F. ) ;
#105113 = DIRECTION ( 'NONE',  ( -1.000000000000000000, -1.224606353822377258E-16, -0.000000000000000000 ) ) ;
#105114 = SURFACE_STYLE_USAGE ( .BOTH. , #72212 ) ;
#105115 = CARTESIAN_POINT ( 'NONE',  ( -19.58115073825180374, -18.43134085946331169, -33.78044860928109472 ) ) ;
#105116 = CIRCLE ( 'NONE', #75863, 4.000000000000000888 ) ;
#105118 = CARTESIAN_POINT ( 'NONE',  ( -38.79060871343663308, -60.22819976177238743, -34.02320779555699914 ) ) ;
#105117 = DIRECTION ( 'NONE',  ( 0.000000000000000000, -1.000000000000000000, 0.000000000000000000 ) ) ;
#105119 = EDGE_LOOP ( 'NONE', ( #3712, #21718, #7967, #2317, #23435 ) ) ;
#105120 = AXIS2_PLACEMENT_3D ( 'NONE', #3887, #11418, #20113 ) ;
#105121 = CARTESIAN_POINT ( 'NONE',  ( -0.2791032213812740803, 8.821394357840562250, -7.929128246061908136 ) ) ;
#105122 = ORIENTED_EDGE ( 'NONE', *, *, #104963, .T. ) ;
#105123 = CARTESIAN_POINT ( 'NONE',  ( 1.469576158976823356E-15, 50.00000000000000000, -73.00000000000001421 ) ) ;
#105124 = CIRCLE ( 'NONE', #62124, 7.000000000000000000 ) ;
#105125 = CARTESIAN_POINT ( 'NONE',  ( 0.000000000000000000, 0.000000000000000000, 62.00000000000000000 ) ) ;
#105126 = CARTESIAN_POINT ( 'NONE',  ( -92.63321420215758906, -60.00000000000000711, -3.375781646321903029 ) ) ;
#105127 = EDGE_LOOP ( 'NONE', ( #55228, #84200, #38081, #14045, #18880 ) ) ;
#105128 = CARTESIAN_POINT ( 'NONE',  ( 59.83737978852683881, -37.40166281318659003, -25.85311039118933962 ) ) ;
#105129 = CARTESIAN_POINT ( 'NONE',  ( 101.3985084166410218, -60.23849521171775478, 194.8049258406955175 ) ) ;
#105131 = CARTESIAN_POINT ( 'NONE',  ( 0.000000000000000000, 0.000000000000000000, 0.000000000000000000 ) ) ;
#105130 = CARTESIAN_POINT ( 'NONE',  ( -5.290067270632216712, 51.34639538792298907, 8.531152949374556371 ) ) ;
#105132 = MECHANICAL_DESIGN_GEOMETRIC_PRESENTATION_REPRESENTATION (  '', ( #41388 ), #50008 ) ;
#105133 = CARTESIAN_POINT ( 'NONE',  ( -84.79477645726274204, -22.09607886015096767, 158.8527075901939156 ) ) ;
#105134 = ORIENTED_EDGE ( 'NONE', *, *, #30378, .F. ) ;
#105135 = VERTEX_POINT ( 'NONE', #45441 ) ;
#105136 = ORIENTED_EDGE ( 'NONE', *, *, #10839, .F. ) ;
#105137 = CARTESIAN_POINT ( 'NONE',  ( 32.13232479388067730, 428.0674789085878729, 24.77008313062577827 ) ) ;
#105138 = EDGE_CURVE ( 'NONE', #62320, #37220, #89750, .T. ) ;
#105139 = CARTESIAN_POINT ( 'NONE',  ( -4.999999999999959144, -13.68989806552422728, 13.02619096221388517 ) ) ;
#105140 = VERTEX_POINT ( 'NONE', #5499 ) ;
#105141 = CARTESIAN_POINT ( 'NONE',  ( -9.151133496029672187, 15.07443463110270088, -4.034557488804598968 ) ) ;
#105142 = CARTESIAN_POINT ( 'NONE',  ( -73.72791963761318357, -57.62431822613736898, 185.7849209195708227 ) ) ;
#105143 = CARTESIAN_POINT ( 'NONE',  ( -16.51294481928371383, 294.5655612426596690, -2.060814981937608259 ) ) ;
#105144 = LINE ( 'NONE', #40403, #14995 ) ;
#105145 = CARTESIAN_POINT ( 'NONE',  ( 0.7408669144212451929, 15.11700796861005003, -9.999999999997889688 ) ) ;
#105146 = AXIS2_PLACEMENT_3D ( 'NONE', #39453, #38400, #48036 ) ;
#105147 = ADVANCED_FACE ( 'NONE', ( #94531 ), #36321, .F. ) ;
#105148 = CARTESIAN_POINT ( 'NONE',  ( -16.35184830034500791, -14.21045842199432663, -36.83529024868766300 ) ) ;
#105149 = CARTESIAN_POINT ( 'NONE',  ( -51.40736910322219444, -29.99999999999990052, 68.09419600167673536 ) ) ;
#105150 = CARTESIAN_POINT ( 'NONE',  ( -52.51426326109795895, -36.04149165182834480, 53.95691964957212861 ) ) ;
#105151 = AXIS2_PLACEMENT_3D ( 'NONE', #75992, #67907, #10714 ) ;
#105152 = ORIENTED_EDGE ( 'NONE', *, *, #7935, .T. ) ;
#105153 = CARTESIAN_POINT ( 'NONE',  ( 3.177522834362841664, 20.29592454198039775, -6.239376119109595997 ) ) ;
#105154 = ORIENTED_EDGE ( 'NONE', *, *, #68759, .F. ) ;
#105155 = CARTESIAN_POINT ( 'NONE',  ( -98.11506906225089608, -60.34699860078747236, 196.5395051151577093 ) ) ;
#105156 = CARTESIAN_POINT ( 'NONE',  ( 0.7145311798163270778, 9.237604307034018802, 3.185620757954082679E-16 ) ) ;
#105157 = ORIENTED_EDGE ( 'NONE', *, *, #88763, .T. ) ;
#105158 = CARTESIAN_POINT ( 'NONE',  ( 19.09459860920181029, 49.66572022866124314, 61.74879405875589100 ) ) ;
#105159 = CARTESIAN_POINT ( 'NONE',  ( 107.2300937431054990, -38.36237930411618180, 194.4693520903244348 ) ) ;
#105160 = CARTESIAN_POINT ( 'NONE',  ( 5.744562646538029504, 12.99999999999999112, -4.000000000000000000 ) ) ;
#105161 = CARTESIAN_POINT ( 'NONE',  ( 0.000000000000000000, 0.000000000000000000, 0.000000000000000000 ) ) ;
#105162 =( NAMED_UNIT ( * ) SI_UNIT ( $, .STERADIAN. ) SOLID_ANGLE_UNIT ( ) );
#105163 = CARTESIAN_POINT ( 'NONE',  ( 43.53995238963187120, 465.2530981678414719, 9.299505628815621705 ) ) ;
#105164 = CARTESIAN_POINT ( 'NONE',  ( 84.60172713863487104, -30.00000000000000355, 166.5370262984466763 ) ) ;
#105165 = CARTESIAN_POINT ( 'NONE',  ( 95.42421628608209971, 1.030564683017419500E-14, 0.000000000000000000 ) ) ;
#105166 = CARTESIAN_POINT ( 'NONE',  ( 43.00000000000000000, 436.5989882784185738, 19.94133085611158407 ) ) ;
#105167 = DIRECTION ( 'NONE',  ( 0.000000000000000000, 1.000000000000000000, 0.000000000000000000 ) ) ;
#105168 = EDGE_CURVE ( 'NONE', #10653, #67063, #7046, .T. ) ;
#105169 = LINE ( 'NONE', #70155, #75833 ) ;
#105170 = CIRCLE ( 'NONE', #82762, 6.000000000000012434 ) ;
#105171 = AXIS2_PLACEMENT_3D ( 'NONE', #201, #66037, #33165 ) ;
#105172 = ORIENTED_EDGE ( 'NONE', *, *, #45255, .F. ) ;
#105173 = ORIENTED_EDGE ( 'NONE', *, *, #3409, .T. ) ;
#105174 = CARTESIAN_POINT ( 'NONE',  ( 50.22232791766091253, -39.51160255249801878, 51.10789571635989859 ) ) ;
#105175 = DIRECTION ( 'NONE',  ( -1.000000000000000000, 0.000000000000000000, 0.000000000000000000 ) ) ;
#105176 = CARTESIAN_POINT ( 'NONE',  ( -6.075240630612073645, 15.03060843655180001, 3.485377474036336576 ) ) ;
#105177 =( BOUNDED_SURFACE ( )  B_SPLINE_SURFACE ( 3, 2, ( 
 ( #24695, #59178, #66188 ),
 ( #348, #83433, #98544 ),
 ( #57545, #92057, #16578 ),
 ( #83968, #42988, #26841 ) ),
 .UNSPECIFIED., .F., .F., .F. ) 
 B_SPLINE_SURFACE_WITH_KNOTS ( ( 4, 4 ),
 ( 3, 3 ),
 ( 2.726768463801043652E-17, 0.0001614739849793452150 ),
 ( 0.000000000000000000, 1.000000000000000000 ),
 .UNSPECIFIED. ) 
 GEOMETRIC_REPRESENTATION_ITEM ( )  RATIONAL_B_SPLINE_SURFACE ( (
 ( 1.000000000000000000, 0.9028401456532979541, 1.000000000000000000),
 ( 1.000000000000000000, 0.9031964952773774424, 1.000000000000000000),
 ( 1.000000000000000000, 0.9035643897147043191, 1.000000000000000000),
 ( 1.000000000000000000, 0.9039444415359939589, 1.000000000000000000) ) ) 
 REPRESENTATION_ITEM ( '' )  SURFACE ( )  );
#105179 = EDGE_CURVE ( 'NONE', #65683, #65608, #67584, .T. ) ;
#105178 = CARTESIAN_POINT ( 'NONE',  ( -104.7053668603516599, -38.39921602607821427, 197.7787533616209430 ) ) ;
#105180 = VERTEX_POINT ( 'NONE', #90128 ) ;
#105181 = CARTESIAN_POINT ( 'NONE',  ( 90.74466543776695460, -38.34261519167259991, 6.545665434262897264 ) ) ;
#105182 = CARTESIAN_POINT ( 'NONE',  ( 11.44060156327110001, 7.577557493472524719, -9.471991900697743105 ) ) ;
#105183 = CYLINDRICAL_SURFACE ( 'NONE', #73345, 7.000000000000000000 ) ;
#105184 = CARTESIAN_POINT ( 'NONE',  ( 95.60192313703464606, -37.84851270224621800, 111.4288484754221713 ) ) ;
#105185 = B_SPLINE_CURVE_WITH_KNOTS ( 'NONE', 3,
 ( #67070, #38693, #37879, #52416 ),
 .UNSPECIFIED., .F., .F.,
 ( 4, 4 ),
 ( 3.198672041575564518E-17, 0.0001993833013610890766 ),
 .UNSPECIFIED. ) ;
#105186 =( NAMED_UNIT ( * ) SI_UNIT ( $, .STERADIAN. ) SOLID_ANGLE_UNIT ( ) );
#105187 = CARTESIAN_POINT ( 'NONE',  ( 30.00000000000000000, 0.000000000000000000, 0.000000000000000000 ) ) ;
#105188 = CARTESIAN_POINT ( 'NONE',  ( 33.46689243939714231, 485.1693579416230477, 2.982310567427692405 ) ) ;
#105189 = CARTESIAN_POINT ( 'NONE',  ( 86.93613143775358765, -59.99999999999999289, 200.9776908624942280 ) ) ;
#105190 = AXIS2_PLACEMENT_3D ( 'NONE', #22451, #55296, #32659 ) ;
#105191 = CARTESIAN_POINT ( 'NONE',  ( 18.35799360122013724, 45.00000000000000000, 62.38167341223874018 ) ) ;
#105192 = STYLED_ITEM ( 'NONE', ( #42984 ), #50038 ) ;
#105193 = ORIENTED_EDGE ( 'NONE', *, *, #89988, .T. ) ;
#105194 = CARTESIAN_POINT ( 'NONE',  ( 57.77568988088241753, -32.54838333112581239, 63.57324009296404199 ) ) ;
#105195 = CARTESIAN_POINT ( 'NONE',  ( -35.16787835860036893, 301.6138128548261648, -8.474289318537694626 ) ) ;
#105196 = EDGE_CURVE ( 'NONE', #7253, #88567, #40512, .T. ) ;
#105197 = EDGE_CURVE ( 'NONE', #73295, #104315, #97673, .T. ) ;
#105198 = CARTESIAN_POINT ( 'NONE',  ( 9.933368185767806224, -50.20648247506351680, 25.82212275612567964 ) ) ;
#105199 = CARTESIAN_POINT ( 'NONE',  ( -7.551892080562055298, 26.99012297460616239, 2.647003822403974471 ) ) ;
#105200 = ORIENTED_EDGE ( 'NONE', *, *, #104574, .T. ) ;
#105202 = DIRECTION ( 'NONE',  ( 0.000000000000000000, 1.000000000000000000, 0.000000000000000000 ) ) ;
#105201 = CARTESIAN_POINT ( 'NONE',  ( -110.5502611048591177, -38.35605075777012019, 160.8838554956551832 ) ) ;
#105203 = CARTESIAN_POINT ( 'NONE',  ( 9.833493305133801599, 1.593028355512270567E-15, 0.000000000000000000 ) ) ;
#105204 = CARTESIAN_POINT ( 'NONE',  ( 31.39110793407987643, 426.5490676794047999, 23.68232819820003598 ) ) ;
#105205 = DIRECTION ( 'NONE',  ( 0.000000000000000000, -1.000000000000000000, 0.000000000000000000 ) ) ;
#105206 = CARTESIAN_POINT ( 'NONE',  ( -5.656854249492379694, -32.93749999999999289, -5.656854249492380582 ) ) ;
#105207 = CARTESIAN_POINT ( 'NONE',  ( 9.999999999999994671, -3.000000000000002665, -83.69100306252322241 ) ) ;
#105208 = CIRCLE ( 'NONE', #84577, 22.55262289886175964 ) ;
#105209 = AXIS2_PLACEMENT_3D ( 'NONE', #13395, #20512, #30151 ) ;
#105210 = DIRECTION ( 'NONE',  ( 2.312964634635754888E-15, -0.9612814585413570478, -0.2755684261024861081 ) ) ;
#105211 = ORIENTED_EDGE ( 'NONE', *, *, #71778, .T. ) ;
#105212 = CARTESIAN_POINT ( 'NONE',  ( 84.00887293287516400, -35.95423091463445076, 173.7886553935154268 ) ) ;
#105213 = CARTESIAN_POINT ( 'NONE',  ( 8.017323899013264921, 48.02671738540060176, -1.301042606982606307E-15 ) ) ;
#105214 = B_SPLINE_CURVE_WITH_KNOTS ( 'NONE', 3,
 ( #53733, #4663, #37596, #54236, #53212, #22463, #87179, #20899, #69927, #5191, #72041, #13259, #54777, #95796, #94750, #46700, #13787, #104950, #12731, #80119 ),
 .UNSPECIFIED., .F., .F.,
 ( 4, 2, 2, 2, 2, 2, 2, 2, 2, 4 ),
 ( 0.000000000000000000, 0.001681824184508711427, 0.003363648369017425456, 0.005045472553526139485, 0.005886384645780496500, 0.006727296738034854381, 0.008409120922543570145, 0.01009094510705228591, 0.01177276929156100167, 0.01345459347606971744 ),
 .UNSPECIFIED. ) ;
#105215 = CARTESIAN_POINT ( 'NONE',  ( 36.94626557873471029, 28.08634120636191511, 11.10896912859703711 ) ) ;
#105216 = ORIENTED_EDGE ( 'NONE', *, *, #32315, .F. ) ;
#105217 = DIRECTION ( 'NONE',  ( 0.000000000000000000, 1.000000000000000000, 0.000000000000000000 ) ) ;
#105218 = CARTESIAN_POINT ( 'NONE',  ( 7.499999907820169120, -3.000141485254359086, -20.99866594743181736 ) ) ;
#105219 = CARTESIAN_POINT ( 'NONE',  ( 8.929771841637641927, 1.482358050883964840E-15, 0.000000000000000000 ) ) ;
#105220 = CARTESIAN_POINT ( 'NONE',  ( 30.11650669486618881, 4.898587196589411843E-16, -4.000000000000000888 ) ) ;
#105221 = CARTESIAN_POINT ( 'NONE',  ( -20.41470034681368872, 43.90732458266749205, -82.43442711126550648 ) ) ;
#105222 = CARTESIAN_POINT ( 'NONE',  ( -28.58355031029979187, 11.06033896639473468, -41.46143022647145671 ) ) ;
#105223 = ADVANCED_FACE ( 'NONE', ( #65850 ), #8140, .T. ) ;
#105224 = ORIENTED_EDGE ( 'NONE', *, *, #103617, .F. ) ;
#105225 = AXIS2_PLACEMENT_3D ( 'NONE', #56683, #38936, #47535 ) ;
#105226 = CARTESIAN_POINT ( 'NONE',  ( 6.832273232158016185, 3.329759989367381490, -6.449140625371640567 ) ) ;
#105227 = CARTESIAN_POINT ( 'NONE',  ( 1.218775023799697266, 25.73288003004027757, 39.17967733385442131 ) ) ;
#105228 = ADVANCED_FACE ( 'NONE', ( #89605 ), #31418, .T. ) ;
#105230 = CARTESIAN_POINT ( 'NONE',  ( -10.88958497527556268, 9.025501054700395542, -10.01831549336726290 ) ) ;
#105229 = DIRECTION ( 'NONE',  ( -1.000000000000000000, -1.224606353822377258E-16, -0.000000000000000000 ) ) ;
#105231 = AXIS2_PLACEMENT_3D ( 'NONE', #72038, #72560, #31604 ) ;
#105232 = CARTESIAN_POINT ( 'NONE',  ( 5.082755093536324154, -19.34375000204838457, 5.082755093536326818 ) ) ;
#105233 = CYLINDRICAL_SURFACE ( 'NONE', #25082, 10.00000000000000178 ) ;
#105234 = CARTESIAN_POINT ( 'NONE',  ( -7.040774328009894667, 41.35742559143615438, -58.68913211047703982 ) ) ;
#105235 = ITEM_DEFINED_TRANSFORMATION ( 'NONE', 'NONE', #83421,  #10728 ) ;
#105236 = ORIENTED_EDGE ( 'NONE', *, *, #46330, .F. ) ;
#105237 = EDGE_CURVE ( 'NONE', #30745, #61384, #48588, .T. ) ;
#105238 = CARTESIAN_POINT ( 'NONE',  ( 38.54515645702225868, 1.482358050883964840E-15, 0.000000000000000000 ) ) ;
#105239 = CARTESIAN_POINT ( 'NONE',  ( 24.23541427165741169, 25.18558254665225959, 32.70087860212819919 ) ) ;
#105240 = CARTESIAN_POINT ( 'NONE',  ( -2.939951578610683125, 97.11948718078730280, -5.000000000000002665 ) ) ;
#105241 = CARTESIAN_POINT ( 'NONE',  ( -9.500000000000003553, -4.999999999999998224, -68.91429205785459544 ) ) ;
#105242 = DIRECTION ( 'NONE',  ( -1.000000000000000000, -0.000000000000000000, -0.000000000000000000 ) ) ;
#105243 = AXIS2_PLACEMENT_3D ( 'NONE', #4759, #47326, #79699 ) ;
#105244 = EDGE_LOOP ( 'NONE', ( #1408, #73815 ) ) ;
#105245 = CARTESIAN_POINT ( 'NONE',  ( 9.349999999999997868, 1.533819458162526451E-15, 0.000000000000000000 ) ) ;
#105246 = DIRECTION ( 'NONE',  ( 0.000000000000000000, 0.000000000000000000, -1.000000000000000000 ) ) ;
#105247 = ORIENTED_EDGE ( 'NONE', *, *, #47450, .T. ) ;
#105248 =( NAMED_UNIT ( * ) SI_UNIT ( $, .STERADIAN. ) SOLID_ANGLE_UNIT ( ) );
#105249 = CARTESIAN_POINT ( 'NONE',  ( -2.894864961505325240, -0.4655938164488910291, 103.3614437639293584 ) ) ;
#105250 = DIRECTION ( 'NONE',  ( 1.000000000000000000, 0.000000000000000000, 0.000000000000000000 ) ) ;
#105251 = UNCERTAINTY_MEASURE_WITH_UNIT (LENGTH_MEASURE( 1.000000000000000082E-05 ), #679, 'distance_accuracy_value', 'NONE');
#105252 = CARTESIAN_POINT ( 'NONE',  ( -112.1932564010748763, -60.00000000000000711, 169.7459552627697121 ) ) ;
#105253 = LINE ( 'NONE', #45965, #17029 ) ;
#105254 = CARTESIAN_POINT ( 'NONE',  ( 23.96375140441108442, 306.3052962357393199, 10.25885168886986243 ) ) ;
#105255 = CARTESIAN_POINT ( 'NONE',  ( 38.85446894546219454, 460.8903912184133560, 2.218456751110199132 ) ) ;
#105256 = CARTESIAN_POINT ( 'NONE',  ( 3.140974613990258568, -5.000000000000002665, -73.31232788067565309 ) ) ;
#105257 = CARTESIAN_POINT ( 'NONE',  ( -81.50822721619086053, -57.02328051233624961, 182.3449969974295755 ) ) ;
#105258 = ORIENTED_EDGE ( 'NONE', *, *, #29291, .T. ) ;
#105259 =( NAMED_UNIT ( * ) SI_UNIT ( $, .STERADIAN. ) SOLID_ANGLE_UNIT ( ) );
#105260 = AXIS2_PLACEMENT_3D ( 'NONE', #83565, #43124, #67927 ) ;
#105261 = CIRCLE ( 'NONE', #88110, 5.000000000000002665 ) ;
#105262 = EDGE_LOOP ( 'NONE', ( #78594, #99055, #32462, #10476 ) ) ;
#105263 = PLANE ( 'NONE',  #7834 ) ;
#105264 = ADVANCED_FACE ( 'NONE', ( #81476 ), #34892, .F. ) ;
#105265 = CARTESIAN_POINT ( 'NONE',  ( -15.73175472929735541, 303.5560492990851458, 9.874135533399703846 ) ) ;
#105266 = CARTESIAN_POINT ( 'NONE',  ( 8.020869781911409646, 47.74450561243745739, -2.456496610752231936E-12 ) ) ;
#105267 = CARTESIAN_POINT ( 'NONE',  ( -33.00000000000000000, 450.0000000000002274, 13.20242257375370976 ) ) ;
#105268 = CARTESIAN_POINT ( 'NONE',  ( 81.26467260280679739, 6.123233995736582872E-16, -5.000000000000011546 ) ) ;
#105269 = AXIS2_PLACEMENT_3D ( 'NONE', #16001, #7361, #55893 ) ;
#105270 = EDGE_CURVE ( 'NONE', #59177, #31781, #83054, .T. ) ;
#105271 = CARTESIAN_POINT ( 'NONE',  ( 83.90815637317848541, -29.99999999999993605, 196.6622986253035208 ) ) ;
#105272 = CIRCLE ( 'NONE', #12259, 7.025805963803935406 ) ;
#105273 = CARTESIAN_POINT ( 'NONE',  ( -108.9224886339666085, -60.00000000000004263, 119.6925845435806650 ) ) ;
#105274 = CARTESIAN_POINT ( 'NONE',  ( -62.87621289667217894, -36.01054220196925115, 78.31231431900522466 ) ) ;
#105275 = ORIENTED_EDGE ( 'NONE', *, *, #62580, .T. ) ;
#105276 = CARTESIAN_POINT ( 'NONE',  ( -63.01300532932567222, 38.95394457514182562, 9.559250005201390010 ) ) ;
#105277 = CARTESIAN_POINT ( 'NONE',  ( 77.05631773205139723, -60.00000000000989075, 196.3100209729188919 ) ) ;
#105278 = VERTEX_POINT ( 'NONE', #39472 ) ;
#105279 = CARTESIAN_POINT ( 'NONE',  ( 3.020116147952439434, -35.99142716605504688, 29.88345697530386502 ) ) ;
#105280 = CARTESIAN_POINT ( 'NONE',  ( 5.082755093536325930, -20.84375000204838813, -5.082755093536325042 ) ) ;
#105281 = DIRECTION ( 'NONE',  ( 0.000000000000000000, -1.000000000000000000, 0.000000000000000000 ) ) ;
#105282 = ORIENTED_EDGE ( 'NONE', *, *, #87004, .F. ) ;
#105283 = DIRECTION ( 'NONE',  ( 0.000000000000000000, 0.000000000000000000, -1.000000000000000000 ) ) ;
#105284 = ORIENTED_EDGE ( 'NONE', *, *, #34477, .F. ) ;
#105285 = DIRECTION ( 'NONE',  ( 1.000000000000000000, 0.000000000000000000, 0.000000000000000000 ) ) ;
#105286 = CYLINDRICAL_SURFACE ( 'NONE', #10984, 4.000000000000000000 ) ;
#105287 = CARTESIAN_POINT ( 'NONE',  ( -85.23168696672351530, -60.00000000000006395, 200.2110442732997910 ) ) ;
#105288 = CARTESIAN_POINT ( 'NONE',  ( 41.36650669486618881, 1.474610560812782335E-15, 0.000000000000000000 ) ) ;
#105289 = CARTESIAN_POINT ( 'NONE',  ( 7.188101187499999156, -28.62500000204838457, 2.977408999572654924 ) ) ;
#105290 = CARTESIAN_POINT ( 'NONE',  ( 36.14207491791087534, 485.3942915881601152, -3.424055767584778920 ) ) ;
#105291 = CARTESIAN_POINT ( 'NONE',  ( -6.496475337783281567, 53.67452587285551857, -6.917066593337933611 ) ) ;
#105292 = CARTESIAN_POINT ( 'NONE',  ( 5.000000000000000000, -68.02076148470871431, 16.47608826392310277 ) ) ;
#105293 = CARTESIAN_POINT ( 'NONE',  ( 8.737863884125493641, 48.00000000000000000, -90.03618980230170621 ) ) ;
#105294 = CARTESIAN_POINT ( 'NONE',  ( 10.66896053074161088, -11.24066709036755007, 17.92507180936227940 ) ) ;
#105295 = CARTESIAN_POINT ( 'NONE',  ( -43.51678756415928007, 365.4275696025253524, 13.28716395725119348 ) ) ;
#105296 = ADVANCED_FACE ( 'NONE', ( #88018 ), #100605, .F. ) ;
#105297 = CARTESIAN_POINT ( 'NONE',  ( 20.68638090159294762, 302.8702952610971693, -9.996063631021495866 ) ) ;
#105298 = CARTESIAN_POINT ( 'NONE',  ( -33.47199527190278445, -56.84231303533334057, 37.78255240090093992 ) ) ;
#105299 = COLOUR_RGB ( '', 0.72549020, 0.75294118, 0.79215686) ;
#105300 = ORIENTED_EDGE ( 'NONE', *, *, #12003, .F. ) ;
#105301 = DIRECTION ( 'NONE',  ( 0.8191520442889913545, 1.003171929053524254E-16, -0.5735764363510468256 ) ) ;
#105302 = CARTESIAN_POINT ( 'NONE',  ( 40.33337910916750957, -42.97531841030273370, 39.77847369127800192 ) ) ;
#105303 = VECTOR ( 'NONE', #48496, 1000.000000000000000 ) ;
#105304 = CARTESIAN_POINT ( 'NONE',  ( -13.66642973270730010, -3.469446951953614189E-15, -17.78317311658304689 ) ) ;
#105305 = ORIENTED_EDGE ( 'NONE', *, *, #81848, .F. ) ;
#105306 = CONICAL_SURFACE ( 'NONE', #100149, 3.309500000000001663, 0.9599310885968770357 ) ;
#105307 = CARTESIAN_POINT ( 'NONE',  ( -74.85312537499551411, -38.33503454998542992, 168.0912832715343086 ) ) ;
#105308 = B_SPLINE_CURVE_WITH_KNOTS ( 'NONE', 3,
 ( #71200, #78756, #104095, #22690, #62599, #21628, #14014, #30235 ),
 .UNSPECIFIED., .F., .F.,
 ( 4, 2, 2, 4 ),
 ( 0.000000000000000000, 7.350793746623692176E-05, 0.0001470158749324738435, 0.0002940317498649437297 ),
 .UNSPECIFIED. ) ;
#105309 = ORIENTED_EDGE ( 'NONE', *, *, #47774, .T. ) ;
#105311 = CARTESIAN_POINT ( 'NONE',  ( 22.91651842568168362, 295.0901107613288445, -9.949346074078583513 ) ) ;
#105310 = CARTESIAN_POINT ( 'NONE',  ( 9.352623941358347182, -4.999999999999999112, -18.60510039294834783 ) ) ;
#105312 = CARTESIAN_POINT ( 'NONE',  ( 54.03872891708841308, 4.000000000000015099, 4.898587196589422689E-16 ) ) ;
#105313 = CARTESIAN_POINT ( 'NONE',  ( -34.88900972249400212, 464.6206820655984870, 18.69027339340994232 ) ) ;
#105314 = FACE_OUTER_BOUND ( 'NONE', #29041, .T. ) ;
#105315 = DIRECTION ( 'NONE',  ( 0.000000000000000000, -1.000000000000000000, 0.000000000000000000 ) ) ;
#105316 = CARTESIAN_POINT ( 'NONE',  ( 79.82022815836235452, -2.002967142162725287E-29, 5.000000000000011546 ) ) ;
#105317 = CARTESIAN_POINT ( 'NONE',  ( -4.438869422347556437, -48.05855701245207001, 43.18766101621736908 ) ) ;
#105318 = CARTESIAN_POINT ( 'NONE',  ( 93.06500352313815938, -60.00000000000000000, 32.93591750832660381 ) ) ;
#105319 = PLANE ( 'NONE',  #11804 ) ;
#105320 =( BOUNDED_SURFACE ( )  B_SPLINE_SURFACE ( 3, 2, ( 
 ( #55339, #7317, #21959 ),
 ( #13286, #6798, #39718 ),
 ( #80154, #79625, #62406 ),
 ( #23550, #30048, #55851 ) ),
 .UNSPECIFIED., .F., .F., .F. ) 
 B_SPLINE_SURFACE_WITH_KNOTS ( ( 4, 4 ),
 ( 3, 3 ),
 ( 2.769486029396972526E-15, 0.002106423517722433563 ),
 ( 0.000000000000000000, 1.000000000000000000 ),
 .UNSPECIFIED. ) 
 GEOMETRIC_REPRESENTATION_ITEM ( )  RATIONAL_B_SPLINE_SURFACE ( (
 ( 1.000000000000000000, 0.7977970988452620649, 1.000000000000000000),
 ( 1.000000000000000000, 0.8078744440618430556, 1.000000000000000000),
 ( 1.000000000000000000, 0.8177468419059694682, 1.000000000000000000),
 ( 1.000000000000000000, 0.8274831119535078772, 1.000000000000000000) ) ) 
 REPRESENTATION_ITEM ( '' )  SURFACE ( )  );
#105321 = CARTESIAN_POINT ( 'NONE',  ( 0.05458999538772688065, -1.264741368073328376, 6.499999999999999112 ) ) ;
#105322 = CARTESIAN_POINT ( 'NONE',  ( 41.46910480218704009, 484.7338956289814860, -3.418960549715446717 ) ) ;
#105323 = ORIENTED_EDGE ( 'NONE', *, *, #90686, .T. ) ;
#105324 = VECTOR ( 'NONE', #48910, 1000.000000000000000 ) ;
#105325 = CARTESIAN_POINT ( 'NONE',  ( -67.63917399235995731, -30.00000000000001066, 87.92849407231595649 ) ) ;
#105326 = ORIENTED_EDGE ( 'NONE', *, *, #77990, .F. ) ;
#105327 = CARTESIAN_POINT ( 'NONE',  ( -9.667921046838758414, -57.17403655832323039, 29.56517872135010094 ) ) ;
#105328 = CARTESIAN_POINT ( 'NONE',  ( -15.93933706297316988, 3.102176837440797641, -0.7193050692103517552 ) ) ;
#105329 = CARTESIAN_POINT ( 'NONE',  ( 9.239881048102057903, 12.03209342865604548, 5.000000000000307310 ) ) ;
#105330 = CYLINDRICAL_SURFACE ( 'NONE', #100095, 4.000000000000000000 ) ;
#105331 = CARTESIAN_POINT ( 'NONE',  ( -23.05203244996622658, 28.15092755562140425, -30.71439907890194831 ) ) ;
#105332 = CARTESIAN_POINT ( 'NONE',  ( 2.977408999572651815, -22.81250000204838813, 7.188101187500000933 ) ) ;
#105333 = CYLINDRICAL_SURFACE ( 'NONE', #63948, 4.000000000000000000 ) ;
#105334 = CARTESIAN_POINT ( 'NONE',  ( 6.921856739985490670, 41.59435684990518922, -70.13580383465757961 ) ) ;
#105335 = EDGE_LOOP ( 'NONE', ( #38857, #96874, #53552, #34314 ) ) ;
#105337 = ORIENTED_EDGE ( 'NONE', *, *, #25478, .T. ) ;
#105336 = FACE_OUTER_BOUND ( 'NONE', #104862, .T. ) ;
#105338 = CARTESIAN_POINT ( 'NONE',  ( 82.67279699970272588, -29.08879217702658337, 151.5812038771563550 ) ) ;
#105339 = AXIS2_PLACEMENT_3D ( 'NONE', #41041, #98724, #40507 ) ;
#105340 = CARTESIAN_POINT ( 'NONE',  ( 14.11595029532510281, 2.410436752314619735, -5.024000119269086184 ) ) ;
#105341 = ORIENTED_EDGE ( 'NONE', *, *, #35063, .F. ) ;
#105342 = CIRCLE ( 'NONE', #95042, 5.000000000000000000 ) ;
#105343 = LINE ( 'NONE', #31488, #37687 ) ;
#105344 = CARTESIAN_POINT ( 'NONE',  ( -1.159778043035263995, 17.01122172421377599, -50.01806045519258959 ) ) ;
#105345 = CARTESIAN_POINT ( 'NONE',  ( -5.082755093536325042, -12.59375000204838280, -5.082755093536325930 ) ) ;
#105346 = CARTESIAN_POINT ( 'NONE',  ( 17.61650669486618881, 1.474610560812782335E-15, 0.000000000000000000 ) ) ;
#105347 = VECTOR ( 'NONE', #91166, 1000.000000000000000 ) ;
#105348 = CARTESIAN_POINT ( 'NONE',  ( -52.60809588292248407, -57.67627119646954981, 84.38067992663381744 ) ) ;
#105349 = CARTESIAN_POINT ( 'NONE',  ( 6.683837171061806082, -3.955946848495971668, -6.851900933636991375 ) ) ;
#105350 = EDGE_CURVE ( 'NONE', #62254, #4153, #41574, .T. ) ;
#105351 = ORIENTED_EDGE ( 'NONE', *, *, #105959, .F. ) ;
#105352 = EDGE_CURVE ( 'NONE', #3260, #91113, #26053, .T. ) ;
#105353 = SURFACE_STYLE_USAGE ( .BOTH. , #22870 ) ;
#105355 = CARTESIAN_POINT ( 'NONE',  ( 3.996126808948607056, 136.8744835974398768, 5.000000000000001776 ) ) ;
#105354 = AXIS2_PLACEMENT_3D ( 'NONE', #82065, #57251, #24412 ) ;
#105356 = CARTESIAN_POINT ( 'NONE',  ( 7.320805580757752118, 41.41776788117373798, -59.82972163162600054 ) ) ;
#105357 = EDGE_CURVE ( 'NONE', #54223, #69803, #42636, .T. ) ;
#105358 = CIRCLE ( 'NONE', #15808, 4.000000000000003553 ) ;
#105359 = DIRECTION ( 'NONE',  ( -0.8191520442889974607, 0.000000000000000000, -0.5735764363510380548 ) ) ;
#105360 = ORIENTED_EDGE ( 'NONE', *, *, #31857, .T. ) ;
#105361 = CARTESIAN_POINT ( 'NONE',  ( -8.000000000000000000, -13.53125000409676915, -3.313708498984762496 ) ) ;
#105362 = CARTESIAN_POINT ( 'NONE',  ( -20.36232553423073810, -17.25202226850461784, 31.47323143012087954 ) ) ;
#105363 = CARTESIAN_POINT ( 'NONE',  ( -1.000000000000000222, -59.21823443912413865, 7.425173686806289197 ) ) ;
#105364 = CARTESIAN_POINT ( 'NONE',  ( -9.644834624769973885, 88.00890500205777300, 2.648308524638419925 ) ) ;
#105365 = CARTESIAN_POINT ( 'NONE',  ( 40.62117264245587478, 438.3092160654453551, 22.60618477163586348 ) ) ;
#105366 = APPLICATION_PROTOCOL_DEFINITION ( 'draft international standard', 'automotive_design', 1998, #49301 ) ;
#105367 = CARTESIAN_POINT ( 'NONE',  ( -9.220915120640583496, 31.04454886432083782, -3.870126578504839987 ) ) ;
#105368 = ORIENTED_EDGE ( 'NONE', *, *, #76977, .T. ) ;
#105369 = CARTESIAN_POINT ( 'NONE',  ( 11.10166199660593911, 43.72034362052824008, 13.20706475317513373 ) ) ;
#105370 = EDGE_CURVE ( 'NONE', #47279, #104577, #77099, .T. ) ;
#105371 = CARTESIAN_POINT ( 'NONE',  ( -3.648665620917406649, 14.99999999999996625, 10.00000000000006750 ) ) ;
#105372 = DIRECTION ( 'NONE',  ( 0.000000000000000000, -1.000000000000000000, 0.000000000000000000 ) ) ;
#105373 = FACE_OUTER_BOUND ( 'NONE', #59633, .T. ) ;
#105374 = DIRECTION ( 'NONE',  ( 1.000000000000000000, 0.000000000000000000, 0.000000000000000000 ) ) ;
#105375 = DIRECTION ( 'NONE',  ( 1.000000000000000000, 0.000000000000000000, 0.000000000000000000 ) ) ;
#105376 = AXIS2_PLACEMENT_3D ( 'NONE', #55623, #106306, #16792 ) ;
#105377 = EDGE_LOOP ( 'NONE', ( #90981, #102162, #33372, #77557, #62705, #6402, #94323 ) ) ;
#105378 = CARTESIAN_POINT ( 'NONE',  ( 0.3194001229792609586, 3.115132258397516729, -7.999999999999998224 ) ) ;
#105379 = CARTESIAN_POINT ( 'NONE',  ( 101.9849436419454491, -57.63211355776580547, 203.2755632733008042 ) ) ;
#105380 = CARTESIAN_POINT ( 'NONE',  ( 36.98821436528865547, 463.5274861635172101, 19.70078135305745803 ) ) ;
#105381 = CIRCLE ( 'NONE', #34819, 4.000000000000007105 ) ;
#105382 = CARTESIAN_POINT ( 'NONE',  ( -14.45712292644103769, 21.77297462402690087, 4.836555868059321917 ) ) ;
#105383 = CARTESIAN_POINT ( 'NONE',  ( 51.78317192880091113, 40.83906611472102810, 39.73656039206255741 ) ) ;
#105384 = CARTESIAN_POINT ( 'NONE',  ( -74.81262360460598870, -59.99999999999999289, 179.8084771762270293 ) ) ;
#105385 = CARTESIAN_POINT ( 'NONE',  ( -37.51854390953261742, 313.5286481325095451, 14.45587837336505999 ) ) ;
#105386 = CARTESIAN_POINT ( 'NONE',  ( -1.000000000000000888, -46.00000000000000000, 40.07669683062201926 ) ) ;
#105387 = CARTESIAN_POINT ( 'NONE',  ( -44.66387834505498944, 341.6072687625629101, 1.189588019127773677 ) ) ;
#105388 = CARTESIAN_POINT ( 'NONE',  ( -85.87270434792566220, -32.01548043290308243, 183.1783680013945741 ) ) ;
#105389 = ORIENTED_EDGE ( 'NONE', *, *, #68925, .F. ) ;
#105390 = CARTESIAN_POINT ( 'NONE',  ( 28.61526283629831724, 309.3341729851595119, -8.977869265197252702 ) ) ;
#105391 = ORIENTED_EDGE ( 'NONE', *, *, #12881, .F. ) ;
#105392 = CARTESIAN_POINT ( 'NONE',  ( 11.60474022311935016, -4.919048487758927557, -76.97896355670452806 ) ) ;
#105393 = EDGE_CURVE ( 'NONE', #103837, #12868, #90661, .T. ) ;
#105394 = CARTESIAN_POINT ( 'NONE',  ( -32.86055893256200733, 316.8313229355889575, -6.875028717072126483 ) ) ;
#105395 = CARTESIAN_POINT ( 'NONE',  ( -84.13922450232199424, -52.73021857188881967, -15.00297300780911947 ) ) ;
#105396 = CYLINDRICAL_SURFACE ( 'NONE', #46198, 4.000000000000000000 ) ;
#105397 = CARTESIAN_POINT ( 'NONE',  ( 33.00000000000000000, 500.0000000000002274, 0.000000000000000000 ) ) ;
#105398 = ORIENTED_EDGE ( 'NONE', *, *, #58298, .T. ) ;
#105399 = CARTESIAN_POINT ( 'NONE',  ( 18.61247279103750074, 50.00000000000000000, 61.10966258427338715 ) ) ;
#105400 = EDGE_CURVE ( 'NONE', #84383, #9641, #45190, .T. ) ;
#105401 = EDGE_CURVE ( 'NONE', #71944, #67484, #65446, .T. ) ;
#105402 = CARTESIAN_POINT ( 'NONE',  ( 5.193195059372482212E-16, -7.895640089090903757, -6.564402953523731377 ) ) ;
#105403 = CARTESIAN_POINT ( 'NONE',  ( 0.5805565836007658964, 7.505553499465141165, -3.996997974842411264E-16 ) ) ;
#105404 = CARTESIAN_POINT ( 'NONE',  ( 94.69963775048552179, -60.00000000000009948, 1.032162584924374293 ) ) ;
#105405 = CARTESIAN_POINT ( 'NONE',  ( -73.66749217889153556, -56.85450343998585510, 127.7611477684293391 ) ) ;
#105406 = ORIENTED_EDGE ( 'NONE', *, *, #87345, .T. ) ;
#105407 = CARTESIAN_POINT ( 'NONE',  ( 48.02079947780210745, -30.00000000000000711, 60.50169175835635826 ) ) ;
#105408 = CARTESIAN_POINT ( 'NONE',  ( 5.000000000000000888, 0.000000000000000000, -10.00000000000000000 ) ) ;
#105409 = CARTESIAN_POINT ( 'NONE',  ( 77.56974481787175080, -57.51673336786241464, 195.9651212718508475 ) ) ;
#105410 = CARTESIAN_POINT ( 'NONE',  ( 68.45015997180047407, 6.975173280561618775E-15, 0.000000000000000000 ) ) ;
#105411 = CARTESIAN_POINT ( 'NONE',  ( 39.03119707554853335, 311.0870578039430825, 1.866927532141321677 ) ) ;
#105412 = CARTESIAN_POINT ( 'NONE',  ( 89.93133926947346879, -5.000000000000000000, 0.000000000000000000 ) ) ;
#105413 = ORIENTED_EDGE ( 'NONE', *, *, #92919, .F. ) ;
#105414 = DIRECTION ( 'NONE',  ( -0.000000000000000000, 1.000000000000000000, -0.000000000000000000 ) ) ;
#105415 = VECTOR ( 'NONE', #75079, 1000.000000000000000 ) ;
#105416 = CYLINDRICAL_SURFACE ( 'NONE', #99601, 5.000000000000000888 ) ;
#105418 = CARTESIAN_POINT ( 'NONE',  ( -99.35947654427663167, -37.82049538106502951, 135.1392028905823111 ) ) ;
#105417 = CARTESIAN_POINT ( 'NONE',  ( 0.000000000000000000, 0.000000000000000000, -1.446714285714285841 ) ) ;
#105419 = CARTESIAN_POINT ( 'NONE',  ( 4.401442555609581635E-16, -17.28125000204838813, -7.188101187500000044 ) ) ;
#105420 = CARTESIAN_POINT ( 'NONE',  ( 43.67509741642236065, 485.0313177283746882, 1.734658347999106676 ) ) ;
#105421 = AXIS2_PLACEMENT_3D ( 'NONE', #92607, #19838, #76417 ) ;
#105422 = CARTESIAN_POINT ( 'NONE',  ( 6.928203230275507885, -85.00000000000000000, -4.000000000000001776 ) ) ;
#105423 = CARTESIAN_POINT ( 'NONE',  ( 0.5682334480337650762, 34.21852722572099736, 29.61650315422764379 ) ) ;
#105424 = CARTESIAN_POINT ( 'NONE',  ( -7.922811899608408481, -4.628803996615327598, -8.057669882367651581 ) ) ;
#105425 =( LENGTH_UNIT ( ) NAMED_UNIT ( * ) SI_UNIT ( .MILLI., .METRE. ) );
#105426 = EDGE_CURVE ( 'NONE', #70974, #88567, #81105, .T. ) ;
#105427 = ORIENTED_EDGE ( 'NONE', *, *, #43770, .F. ) ;
#105428 = CARTESIAN_POINT ( 'NONE',  ( -6.503373625913253520, 41.93912930209143042, -59.84719177782724131 ) ) ;
#105429 =( GEOMETRIC_REPRESENTATION_CONTEXT ( 3 ) GLOBAL_UNCERTAINTY_ASSIGNED_CONTEXT ( ( #91525 ) ) GLOBAL_UNIT_ASSIGNED_CONTEXT ( ( #60614, #60088, #102103 ) ) REPRESENTATION_CONTEXT ( 'NONE', 'WORKASPACE' ) );
#105431 = CARTESIAN_POINT ( 'NONE',  ( 29.45595439878422184, -32.53657559208932071, 31.71262922621859204 ) ) ;
#105430 = CARTESIAN_POINT ( 'NONE',  ( 0.000000000000000000, -30.00000000000000000, 8.000000000000000000 ) ) ;
#105432 = DIRECTION ( 'NONE',  ( -1.000000000000000000, 0.000000000000000000, 0.000000000000000000 ) ) ;
#105433 = ORIENTED_EDGE ( 'NONE', *, *, #88842, .T. ) ;
#105434 = ADVANCED_FACE ( 'NONE', ( #88290 ), #53633, .T. ) ;
#105435 = ORIENTED_EDGE ( 'NONE', *, *, #46407, .F. ) ;
#105437 = CARTESIAN_POINT ( 'NONE',  ( 5.581309233574441675E-23, 43.17555810750860701, -18.75000000000000355 ) ) ;
#105436 = DIRECTION ( 'NONE',  ( 0.000000000000000000, 1.000000000000000000, 0.000000000000000000 ) ) ;
#105438 = DIRECTION ( 'NONE',  ( 0.000000000000000000, 1.000000000000000000, 0.000000000000000000 ) ) ;
#105439 = SURFACE_STYLE_FILL_AREA ( #71465 ) ;
#105440 = CARTESIAN_POINT ( 'NONE',  ( 0.000000000000000000, 35.00000000000000000, -8.000000000000000000 ) ) ;
#105441 = ADVANCED_FACE ( 'NONE', ( #104998 ), #77745, .T. ) ;
#105442 = CARTESIAN_POINT ( 'NONE',  ( 9.684147237222786586, 2.793897972684820985, 14.73931554192828663 ) ) ;
#105443 = ORIENTED_EDGE ( 'NONE', *, *, #4151, .T. ) ;
#105444 = CARTESIAN_POINT ( 'NONE',  ( 57.01351239614803745, -60.00000000000001421, -36.42612028841926275 ) ) ;
#105445 = DIRECTION ( 'NONE',  ( 0.000000000000000000, -1.000000000000000000, 0.000000000000000000 ) ) ;
#105446 = CARTESIAN_POINT ( 'NONE',  ( 0.000000000000000000, 70.00000000000000000, 5.000000000000000000 ) ) ;
#105447 = FACE_OUTER_BOUND ( 'NONE', #32106, .T. ) ;
#105448 = CARTESIAN_POINT ( 'NONE',  ( 0.000000000000000000, 0.000000000000000000, -0.7256075382097185722 ) ) ;
#105449 = VERTEX_POINT ( 'NONE', #80173 ) ;
#105450 = EDGE_LOOP ( 'NONE', ( #22199, #34596, #39251 ) ) ;
#105451 = VERTEX_POINT ( 'NONE', #69061 ) ;
#105452 = DIRECTION ( 'NONE',  ( -1.000000000000000000, -0.000000000000000000, -0.000000000000000000 ) ) ;
#105453 = CARTESIAN_POINT ( 'NONE',  ( -35.75984758101135697, 439.1067915602654352, 24.04383837159262782 ) ) ;
#105454 = CARTESIAN_POINT ( 'NONE',  ( 21.43353486660526031, 303.0521706313907089, 9.980247409275479598 ) ) ;
#105455 = AXIS2_PLACEMENT_3D ( 'NONE', #7782, #40688, #65508 ) ;
#105456 = CARTESIAN_POINT ( 'NONE',  ( -43.63759230290430224, 379.1247326692748061, 14.86908692522124831 ) ) ;
#105457 = CARTESIAN_POINT ( 'NONE',  ( -3.088900377613861270, -69.43752249126038123, 13.34077525874367076 ) ) ;
#105458 = CARTESIAN_POINT ( 'NONE',  ( 0.000000000000000000, 0.000000000000000000, 5.000000000000002665 ) ) ;
#105459 = DIRECTION ( 'NONE',  ( -0.000000000000000000, -0.000000000000000000, -1.000000000000000000 ) ) ;
#105460 = ORIENTED_EDGE ( 'NONE', *, *, #30526, .F. ) ;
#105461 = CARTESIAN_POINT ( 'NONE',  ( 0.000000000000000000, 0.000000000000000000, -2.716724522925831220 ) ) ;
#105462 = AXIS2_PLACEMENT_3D ( 'NONE', #60572, #93462, #91852 ) ;
#105463 = ORIENTED_EDGE ( 'NONE', *, *, #65246, .F. ) ;
#105464 = DIRECTION ( 'NONE',  ( -1.000000000000000000, 0.000000000000000000, 0.000000000000000000 ) ) ;
#105465 = CARTESIAN_POINT ( 'NONE',  ( 12.19423397773156736, 304.5852035401753710, 9.880331998383338643 ) ) ;
#105466 = CARTESIAN_POINT ( 'NONE',  ( -40.34962789288057650, 485.8327705809454642, -4.928685277735865178 ) ) ;
#105467 = CARTESIAN_POINT ( 'NONE',  ( -54.47640052782665521, -60.00000000000000000, 67.52253231662828625 ) ) ;
#105468 = CARTESIAN_POINT ( 'NONE',  ( 65.92109651114007818, -60.33495006274211647, 100.3550901629334362 ) ) ;
#105469 = VERTEX_POINT ( 'NONE', #31141 ) ;
#105470 = DIRECTION ( 'NONE',  ( -1.000000000000000000, -0.000000000000000000, -0.000000000000000000 ) ) ;
#105471 = FACE_OUTER_BOUND ( 'NONE', #14077, .T. ) ;
#105472 = PRESENTATION_STYLE_ASSIGNMENT (( #96863 ) ) ;
#105473 = ADVANCED_FACE ( 'NONE', ( #53399 ), #43315, .T. ) ;
#105474 = ORIENTED_EDGE ( 'NONE', *, *, #55213, .F. ) ;
#105475 = DIRECTION ( 'NONE',  ( -1.000000000000000000, 0.000000000000000000, 0.000000000000000000 ) ) ;
#105476 = EDGE_CURVE ( 'NONE', #91423, #41373, #101934, .T. ) ;
#105477 = DIRECTION ( 'NONE',  ( 0.000000000000000000, 0.000000000000000000, -1.000000000000000000 ) ) ;
#105478 = ADVANCED_FACE ( 'NONE', ( #86320 ), #72617, .F. ) ;
#105479 = CARTESIAN_POINT ( 'NONE',  ( -5.656854249492381470, -28.25000000409677270, 5.656854249492379694 ) ) ;
#105480 = CARTESIAN_POINT ( 'NONE',  ( -7.137815226411302838, -3.000000000000000000, -4.175893272573455661 ) ) ;
#105481 = CARTESIAN_POINT ( 'NONE',  ( 9.537291425704623293, 247.3559562266722480, 3.012810007366010012 ) ) ;
#105482 = ADVANCED_FACE ( 'NONE', ( #23039 ), #24418, .T. ) ;
#105483 = DIRECTION ( 'NONE',  ( 0.000000000000000000, 0.000000000000000000, 1.000000000000000000 ) ) ;
#105484 = CARTESIAN_POINT ( 'NONE',  ( -10.00190353424524226, 7.497281471361841199, 4.999999999999998224 ) ) ;
#105485 = CARTESIAN_POINT ( 'NONE',  ( 7.744991119775239241, -6.535612145748712187, -2.016316005557097668 ) ) ;
#105486 = ADVANCED_FACE ( 'NONE', ( #36192 ), #3677, .T. ) ;
#105487 = CIRCLE ( 'NONE', #46884, 4.000000000000007105 ) ;
#105488 = CARTESIAN_POINT ( 'NONE',  ( -43.27459526351814389, 485.1620945307481634, -2.264801863400593529 ) ) ;
#105489 = ORIENTED_EDGE ( 'NONE', *, *, #30725, .F. ) ;
#105490 = DIRECTION ( 'NONE',  ( 0.000000000000000000, 0.000000000000000000, 1.000000000000000000 ) ) ;
#105491 = ADVANCED_FACE ( 'NONE', ( #11857, #56953 ), #99543, .F. ) ;
#105492 = CARTESIAN_POINT ( 'NONE',  ( 0.4037800551813687799, 4.058962678540087410, -5.969670414742687115 ) ) ;
#105493 = CARTESIAN_POINT ( 'NONE',  ( 17.04897055569503905, -60.00000000000000711, 39.92612883515686661 ) ) ;
#105494 = CARTESIAN_POINT ( 'NONE',  ( -96.99361400851853432, -30.00000000000001066, 191.0864438644175891 ) ) ;
#105495 = LINE ( 'NONE', #106009, #43457 ) ;
#105496 =( GEOMETRIC_REPRESENTATION_CONTEXT ( 3 ) GLOBAL_UNCERTAINTY_ASSIGNED_CONTEXT ( ( #59015 ) ) GLOBAL_UNIT_ASSIGNED_CONTEXT ( ( #89263, #38604, #15361 ) ) REPRESENTATION_CONTEXT ( 'NONE', 'WORKASPACE' ) );
#105497 = CARTESIAN_POINT ( 'NONE',  ( 52.36026450593488590, -57.67644934183336147, 83.70945018486365541 ) ) ;
#105499 = FACE_OUTER_BOUND ( 'NONE', #95864, .T. ) ;
#105498 = CARTESIAN_POINT ( 'NONE',  ( 15.26476282643411864, -0.4519630325742635679, 14.99528456596575232 ) ) ;
#105500 = CARTESIAN_POINT ( 'NONE',  ( -14.91339176601161043, 41.98696008795855050, -86.62219925848557978 ) ) ;
#105501 = CARTESIAN_POINT ( 'NONE',  ( -30.00000000000000355, 462.0097303356245106, 12.67201001741399047 ) ) ;
#105502 = FACE_OUTER_BOUND ( 'NONE', #76774, .T. ) ;
#105503 = B_SPLINE_CURVE_WITH_KNOTS ( 'NONE', 3,
 ( #52063, #37527, #11597, #2448, #102218, #27850, #93066, #28915, #19233, #84978, #28366, #86597, #101155, #70391, #60719, #77947, #4061, #20832, #61244, #3531, #2983, #76871, #76335, #77414 ),
 .UNSPECIFIED., .F., .F.,
 ( 4, 2, 2, 2, 2, 2, 2, 2, 2, 2, 2, 4 ),
 ( 0.002986045904103195626, 0.003488698368484360358, 0.003740024600674948796, 0.003991350832865537233, 0.004242677065056125671, 0.004494003297246713241, 0.004996655761627886647, 0.005499308226009059185, 0.005750634458199645888, 0.006001960690390231723, 0.006504613154771410333, 0.007007265619152588075 ),
 .UNSPECIFIED. ) ;
#105504 = DIRECTION ( 'NONE',  ( 0.000000000000000000, 0.000000000000000000, 1.000000000000000000 ) ) ;
#105505 = CARTESIAN_POINT ( 'NONE',  ( -12.42807525731150164, -60.00000000000000711, 39.69786023814224762 ) ) ;
#105506 = CARTESIAN_POINT ( 'NONE',  ( 12.82140450591726299, 18.88705565487690308, 8.090819087176381430 ) ) ;
#105507 = CARTESIAN_POINT ( 'NONE',  ( -85.66156584027689291, -61.06605174068531028, 194.0559517944926995 ) ) ;
#105508 = ORIENTED_EDGE ( 'NONE', *, *, #25025, .T. ) ;
#105509 = CARTESIAN_POINT ( 'NONE',  ( 17.50000000000006040, 51.01864103016391994, 63.17274301512998136 ) ) ;
#105510 = CARTESIAN_POINT ( 'NONE',  ( -14.88112861571068279, -60.36545018808638474, 34.08850901830101066 ) ) ;
#105511 = CARTESIAN_POINT ( 'NONE',  ( -2.499999999999997780, -30.00000000000000000, 14.79019945774903810 ) ) ;
#105513 = SURFACE_SIDE_STYLE ('',( #47270 ) ) ;
#105512 = CARTESIAN_POINT ( 'NONE',  ( 26.84999999999999787, 3.309500000000003439, 0.000000000000000000 ) ) ;
#105514 = ORIENTED_EDGE ( 'NONE', *, *, #19204, .T. ) ;
#105515 = LINE ( 'NONE', #46231, #76525 ) ;
#105516 =( GEOMETRIC_REPRESENTATION_CONTEXT ( 3 ) GLOBAL_UNCERTAINTY_ASSIGNED_CONTEXT ( ( #18373 ) ) GLOBAL_UNIT_ASSIGNED_CONTEXT ( ( #3066, #60794, #44066 ) ) REPRESENTATION_CONTEXT ( 'NONE', 'WORKASPACE' ) );
#105517 = CARTESIAN_POINT ( 'NONE',  ( -6.793650603639286523, -4.999999999999960920, -15.34177241507040002 ) ) ;
#105518 = CARTESIAN_POINT ( 'NONE',  ( -7.344505440741525781, 32.44618927298703426, -3.175463080953007111 ) ) ;
#105519 =( GEOMETRIC_REPRESENTATION_CONTEXT ( 3 ) GLOBAL_UNCERTAINTY_ASSIGNED_CONTEXT ( ( #42723 ) ) GLOBAL_UNIT_ASSIGNED_CONTEXT ( ( #82239, #72561, #96855 ) ) REPRESENTATION_CONTEXT ( 'NONE', 'WORKASPACE' ) );
#105520 = DIRECTION ( 'NONE',  ( 0.000000000000000000, -1.000000000000000000, 0.000000000000000000 ) ) ;
#105521 = EDGE_CURVE ( 'NONE', #52776, #55265, #13961, .T. ) ;
#105522 = DIRECTION ( 'NONE',  ( 1.000000000000000000, 0.000000000000000000, 0.000000000000000000 ) ) ;
#105523 = CARTESIAN_POINT ( 'NONE',  ( 66.11079172910912405, -60.00000000000000000, 122.8458817101759308 ) ) ;
#105524 = CARTESIAN_POINT ( 'NONE',  ( -1.221393050841994787, 53.71071939966033426, -9.310417747113787001 ) ) ;
#105525 = ORIENTED_EDGE ( 'NONE', *, *, #17773, .T. ) ;
#105526 = CARTESIAN_POINT ( 'NONE',  ( 4.250000000000000000, 0.000000000000000000, -1.971869939371574620 ) ) ;
#105527 = CARTESIAN_POINT ( 'NONE',  ( -34.50218234403093476, 434.5102366699516097, 9.485624649973072309 ) ) ;
#105529 = CARTESIAN_POINT ( 'NONE',  ( -37.83758010121304238, 485.6941950553117522, -4.518273513594293078 ) ) ;
#105528 =( NAMED_UNIT ( * ) PLANE_ANGLE_UNIT ( ) SI_UNIT ( $, .RADIAN. ) );
#105530 = CARTESIAN_POINT ( 'NONE',  ( -5.603804764709576780, -2.702239074867451407, 103.9691152301460590 ) ) ;
#105531 = ORIENTED_EDGE ( 'NONE', *, *, #21550, .T. ) ;
#105532 = CARTESIAN_POINT ( 'NONE',  ( -29.85808249604284370, 330.9700016804235361, 16.31510691329269847 ) ) ;
#105533 = ORIENTED_EDGE ( 'NONE', *, *, #43815, .F. ) ;
#105534 = CARTESIAN_POINT ( 'NONE',  ( 20.55501430260233420, 303.9056691006283586, 9.948455458498445481 ) ) ;
#105535 = SURFACE_STYLE_FILL_AREA ( #24127 ) ;
#105536 = LINE ( 'NONE', #31677, #2678 ) ;
#105537 = PRESENTATION_STYLE_ASSIGNMENT (( #56437 ) ) ;
#105538 = ORIENTED_EDGE ( 'NONE', *, *, #47870, .T. ) ;
#105539 = SURFACE_STYLE_USAGE ( .BOTH. , #16003 ) ;
#105540 = CARTESIAN_POINT ( 'NONE',  ( -9.973779925059078622, 7.480996659792954695, -0.6547794009576259899 ) ) ;
#105541 = CARTESIAN_POINT ( 'NONE',  ( -77.30691964702137398, -59.99999999999513989, 196.7061328158951596 ) ) ;
#105542 = B_SPLINE_CURVE_WITH_KNOTS ( 'NONE', 3,
 ( #49741, #105849, #83697, #82650, #24967, #73473 ),
 .UNSPECIFIED., .F., .F.,
 ( 4, 2, 4 ),
 ( 2.611104600503255956E-18, 0.0003916983043530442889, 0.0007833966087060859756 ),
 .UNSPECIFIED. ) ;
#105543 = CARTESIAN_POINT ( 'NONE',  ( 43.02621584241283870, 434.6128289108255558, 16.97888786058996402 ) ) ;
#105544 = CARTESIAN_POINT ( 'NONE',  ( 44.97999590490915978, -60.00000000000000000, 60.55235333090226391 ) ) ;
#105545 = DIRECTION ( 'NONE',  ( -1.000000000000000000, -2.168404344971008868E-17, 0.000000000000000000 ) ) ;
#105546 = CARTESIAN_POINT ( 'NONE',  ( 0.3378009397522571122, 26.06497163046132926, -38.28498976926001518 ) ) ;
#105548 = CARTESIAN_POINT ( 'NONE',  ( 16.37553332807584994, -18.58809198569462495, 27.19376126714132624 ) ) ;
#105547 = CARTESIAN_POINT ( 'NONE',  ( -114.5930292407900879, -59.99999999999997868, 172.8116974628616163 ) ) ;
#105549 = CARTESIAN_POINT ( 'NONE',  ( 34.83349330513380693, 1.593028355512270962E-15, 0.000000000000000000 ) ) ;
#105550 = PLANE ( 'NONE',  #13840 ) ;
#105551 = CARTESIAN_POINT ( 'NONE',  ( -47.01439492264584885, -46.44460756023540426, 48.25956263889609232 ) ) ;
#105552 = CARTESIAN_POINT ( 'NONE',  ( -0.6415681314778590716, 35.01575306882282490, -27.42406975498120403 ) ) ;
#105553 = ORIENTED_EDGE ( 'NONE', *, *, #28831, .T. ) ;
#105554 = CARTESIAN_POINT ( 'NONE',  ( -17.49999999999995737, 47.99999999999999289, 62.61753806507838505 ) ) ;
#105555 = CARTESIAN_POINT ( 'NONE',  ( -1.226412146326429475, -69.63306384108153679, 12.78930087777542646 ) ) ;
#105556 = EDGE_CURVE ( 'NONE', #34171, #43396, #157, .T. ) ;
#105557 = SURFACE_SIDE_STYLE ('',( #79158 ) ) ;
#105558 = CARTESIAN_POINT ( 'NONE',  ( 26.27902093981875709, 306.9027577142574614, -9.548073367147230428 ) ) ;
#105559 = ORIENTED_EDGE ( 'NONE', *, *, #57369, .T. ) ;
#105560 = ORIENTED_EDGE ( 'NONE', *, *, #82735, .F. ) ;
#105561 = CARTESIAN_POINT ( 'NONE',  ( 103.9866713306733743, -29.99999999999896616, 196.5747536251343206 ) ) ;
#105562 = CARTESIAN_POINT ( 'NONE',  ( 46.00000000000001421, 460.3170374101630955, 7.034854880083544870 ) ) ;
#105563 = CONICAL_SURFACE ( 'NONE', #5628, 5.000000000000010658, 0.9599310885968697082 ) ;
#105564 = CARTESIAN_POINT ( 'NONE',  ( 6.777273857537102764, 41.87254887207789267, -59.70743237412717974 ) ) ;
#105565 = CARTESIAN_POINT ( 'NONE',  ( -29.99397490504468067, 1.005902684993158047, 14.99698745252235099 ) ) ;
#105566 = CARTESIAN_POINT ( 'NONE',  ( 100.5837132263118292, -30.00000000000000000, 160.2813360046134505 ) ) ;
#105567 = PRESENTATION_LAYER_ASSIGNMENT (  '', '', ( #45297 ) ) ;
#105568 = CARTESIAN_POINT ( 'NONE',  ( 7.744991119775237465, 101.5356121457486722, -2.016316005557098556 ) ) ;
#105569 = ORIENTED_EDGE ( 'NONE', *, *, #84968, .T. ) ;
#105570 = VERTEX_POINT ( 'NONE', #41315 ) ;
#105571 = ORIENTED_EDGE ( 'NONE', *, *, #86311, .T. ) ;
#105572 = CARTESIAN_POINT ( 'NONE',  ( 16.08349330513380337, -7.703719777548943412E-31, 4.000000000000001776 ) ) ;
#105573 = CARTESIAN_POINT ( 'NONE',  ( 23.05087275028312277, 25.28743397255878023, 33.20617127781017786 ) ) ;
#105574 = CIRCLE ( 'NONE', #24606, 5.000000000000010658 ) ;
#105575 = FACE_OUTER_BOUND ( 'NONE', #61925, .T. ) ;
#105576 = ORIENTED_EDGE ( 'NONE', *, *, #76562, .F. ) ;
#105577 = CARTESIAN_POINT ( 'NONE',  ( 9.333555687487613994, 106.7810269660896836, 3.591168747312690090 ) ) ;
#105578 = EDGE_LOOP ( 'NONE', ( #25160, #25648, #75847, #13862 ) ) ;
#105579 = CARTESIAN_POINT ( 'NONE',  ( 43.00000000000000000, 450.0000000000002274, 13.20242257375370976 ) ) ;
#105580 = CARTESIAN_POINT ( 'NONE',  ( 82.02875481936112578, -38.83883151105103337, 195.9167761120497460 ) ) ;
#105581 = DIRECTION ( 'NONE',  ( -1.000000000000000000, -0.000000000000000000, -0.000000000000000000 ) ) ;
#105582 = PRODUCT_DEFINITION ( 'UNKNOWN', '', #47376, #76901 ) ;
#105583 = CARTESIAN_POINT ( 'NONE',  ( 18.00000000000000355, 12.99999999999999289, -9.500000000000000000 ) ) ;
#105584 = CARTESIAN_POINT ( 'NONE',  ( 31.09748479556632006, 323.2603612422993251, 14.95832153367667772 ) ) ;
#105585 = DIRECTION ( 'NONE',  ( 0.000000000000000000, 1.000000000000000000, 0.000000000000000000 ) ) ;
#105586 = SURFACE_SIDE_STYLE ('',( #98029 ) ) ;
#105587 = CARTESIAN_POINT ( 'NONE',  ( -41.18500240987163608, 460.1236783698128647, 2.133705300515147840 ) ) ;
#105588 = CARTESIAN_POINT ( 'NONE',  ( -4.464768147783013674, -48.00301508167383702, 102.6740199126133888 ) ) ;
#105589 = CIRCLE ( 'NONE', #9108, 3.309499999999999886 ) ;
#105590 = DIRECTION ( 'NONE',  ( -1.000000000000000000, 0.000000000000000000, 0.000000000000000000 ) ) ;
#105591 = ORIENTED_EDGE ( 'NONE', *, *, #14502, .F. ) ;
#105592 = FACE_OUTER_BOUND ( 'NONE', #95309, .T. ) ;
#105593 = CARTESIAN_POINT ( 'NONE',  ( -33.82446905678677496, 302.9270370839546445, 11.79982883588897913 ) ) ;
#105594 = CARTESIAN_POINT ( 'NONE',  ( 8.399149604396622948, 53.73754273787561431, -4.031152949375367278 ) ) ;
#105595 = UNCERTAINTY_MEASURE_WITH_UNIT (LENGTH_MEASURE( 1.000000000000000082E-05 ), #11210, 'distance_accuracy_value', 'NONE');
#105596 = ADVANCED_FACE ( 'NONE', ( #81750 ), #81226, .T. ) ;
#105597 = DIRECTION ( 'NONE',  ( -1.000000000000000000, -0.000000000000000000, -0.000000000000000000 ) ) ;
#105598 = CARTESIAN_POINT ( 'NONE',  ( -5.656854249492379694, -13.43749999999999112, -5.656854249492380582 ) ) ;
#105599 = CIRCLE ( 'NONE', #45333, 3.981862520314373377 ) ;
#105600 = CARTESIAN_POINT ( 'NONE',  ( 43.23783249438958620, -38.30607820824091903, 54.77471611439175092 ) ) ;
#105601 = EDGE_CURVE ( 'NONE', #81108, #30000, #60516, .T. ) ;
#105602 = SURFACE_STYLE_FILL_AREA ( #40875 ) ;
#105603 = VERTEX_POINT ( 'NONE', #32179 ) ;
#105604 = CARTESIAN_POINT ( 'NONE',  ( 84.53280797509962952, -50.18428614998399695, 188.2537912682702768 ) ) ;
#105605 = CARTESIAN_POINT ( 'NONE',  ( 1.128183577527849701, 300.9492746658232818, 9.936156289954276133 ) ) ;
#105606 = CARTESIAN_POINT ( 'NONE',  ( 4.335182740490085784, -1.119534022499610426, 104.3855524028841160 ) ) ;
#105607 = ORIENTED_EDGE ( 'NONE', *, *, #78316, .F. ) ;
#105608 = CARTESIAN_POINT ( 'NONE',  ( 94.41737687008979663, -57.67086643237934851, -0.3944160041198634947 ) ) ;
#105609 = DIRECTION ( 'NONE',  ( -0.000000000000000000, -0.000000000000000000, 1.000000000000000000 ) ) ;
#105610 = CARTESIAN_POINT ( 'NONE',  ( 0.000000000000000000, 0.000000000000000000, 0.000000000000000000 ) ) ;
#105611 = ADVANCED_FACE ( 'NONE', ( #16508 ), #7345, .T. ) ;
#105612 = CARTESIAN_POINT ( 'NONE',  ( 28.43259016867768452, 12.18852863928164076, 40.99039043055278597 ) ) ;
#105613 =( BOUNDED_SURFACE ( )  B_SPLINE_SURFACE ( 3, 2, ( 
 ( #88257, #47242, #50950 ),
 ( #67696, #66087, #25128 ),
 ( #57988, #40746, #73634 ),
 ( #26215, #82806, #7840 ),
 ( #100047, #74697, #9976 ),
 ( #65561, #57446, #98450 ),
 ( #42879, #59074, #66621 ),
 ( #106539, #24073, #9423 ),
 ( #74170, #32694, #24598 ),
 ( #42343, #50421, #25680 ) ),
 .UNSPECIFIED., .F., .F., .F. ) 
 B_SPLINE_SURFACE_WITH_KNOTS ( ( 4, 2, 2, 2, 4 ),
 ( 3, 3 ),
 ( 0.002450517525418896905, 0.003060732775749463834, 0.003670948026080030763, 0.004891378526741164620, 0.007332239528063431468 ),
 ( 0.000000000000000000, 1.000000000000000000 ),
 .UNSPECIFIED. ) 
 GEOMETRIC_REPRESENTATION_ITEM ( )  RATIONAL_B_SPLINE_SURFACE ( (
 ( 1.000000000000000000, 0.7071067811865481278, 1.000000000000000000),
 ( 1.000000000000000000, 0.7344063550101855853, 1.000000000000000000),
 ( 1.000000000000000000, 0.7590375248711127565, 1.000000000000000000),
 ( 1.000000000000000000, 0.8038331608703981335, 1.000000000000000000),
 ( 1.000000000000000000, 0.8240352460865911777, 1.000000000000000000),
 ( 1.000000000000000000, 0.8791017378333240151, 1.000000000000000000),
 ( 1.000000000000000000, 0.9085032776980892510, 1.000000000000000000),
 ( 1.000000000000000000, 0.9784170511696808070, 1.000000000000000000),
 ( 1.000000000000000000, 0.9996598051696607978, 1.000000000000000000),
 ( 1.000000000000000000, 1.000000000000000000, 1.000000000000000000) ) ) 
 REPRESENTATION_ITEM ( '' )  SURFACE ( )  );
#105614 = ADVANCED_FACE ( 'NONE', ( #9465 ), #281, .F. ) ;
#105615 = ADVANCED_FACE ( 'NONE', ( #89351 ), #15442, .T. ) ;
#105616 = CARTESIAN_POINT ( 'NONE',  ( -83.62938647969347983, -37.99999999999996447, 173.4280063321390060 ) ) ;
#105617 = CARTESIAN_POINT ( 'NONE',  ( -8.000000000000003553, -3.000000000000000000, -2.094395098902523511 ) ) ;
#105618 = DIRECTION ( 'NONE',  ( -1.000000000000000000, -1.224606353822377258E-16, -0.000000000000000000 ) ) ;
#105619 = CARTESIAN_POINT ( 'NONE',  ( -14.23923521226553035, 6.526093643864192551, 7.639870307848205755 ) ) ;
#105620 = ORIENTED_EDGE ( 'NONE', *, *, #87798, .T. ) ;
#105621 = CARTESIAN_POINT ( 'NONE',  ( 9.740083726526258090, 294.6493269980091441, -10.04303756037257322 ) ) ;
#105622 = CARTESIAN_POINT ( 'NONE',  ( -10.50000000000000000, -5.000000000000000000, -34.12705337366766400 ) ) ;
#105623 =( NAMED_UNIT ( * ) PLANE_ANGLE_UNIT ( ) SI_UNIT ( $, .RADIAN. ) );
#105624 = CARTESIAN_POINT ( 'NONE',  ( 6.123233995736766282E-16, 0.000000000000000000, -5.000000000000000000 ) ) ;
#105625 = CARTESIAN_POINT ( 'NONE',  ( -0.4000000000000045186, 0.000000000000000000, 0.000000000000000000 ) ) ;
#105626 = CARTESIAN_POINT ( 'NONE',  ( 67.97786962772167385, -29.92019613139300205, -21.73453229204871207 ) ) ;
#105627 = ORIENTED_EDGE ( 'NONE', *, *, #103751, .F. ) ;
#105628 = CARTESIAN_POINT ( 'NONE',  ( 6.333820801332779915, -6.982605850969665795, -0.9057718968909265200 ) ) ;
#105629 = FACE_OUTER_BOUND ( 'NONE', #72629, .T. ) ;
#105630 = VECTOR ( 'NONE', #1085, 1000.000000000000114 ) ;
#105631 = CARTESIAN_POINT ( 'NONE',  ( -1.895665647442401625, -15.39481678902619244, -35.22747512624398780 ) ) ;
#105633 = CARTESIAN_POINT ( 'NONE',  ( -29.14298834304714703, -60.22827824258391871, -35.25025982252484624 ) ) ;
#105632 = LINE ( 'NONE', #38795, #13941 ) ;
#105634 = ORIENTED_EDGE ( 'NONE', *, *, #8817, .T. ) ;
#105636 = VERTEX_POINT ( 'NONE', #8413 ) ;
#105635 = AXIS2_PLACEMENT_3D ( 'NONE', #2096, #54353, #70582 ) ;
#105637 = EDGE_CURVE ( 'NONE', #97430, #40622, #69286, .T. ) ;
#105638 = CARTESIAN_POINT ( 'NONE',  ( 18.86650669486618881, 4.000000000000003553, 4.898587196589414801E-16 ) ) ;
#105639 = LINE ( 'NONE', #65190, #89063 ) ;
#105640 = CARTESIAN_POINT ( 'NONE',  ( -92.53829303969855857, -60.00000000000000711, -1.819294454048275167 ) ) ;
#105641 = ORIENTED_EDGE ( 'NONE', *, *, #14814, .F. ) ;
#105642 = CARTESIAN_POINT ( 'NONE',  ( 6.211901734583654466, -22.42181773049501814, -30.53157825004622694 ) ) ;
#105643 = DIRECTION ( 'NONE',  ( -1.000000000000000000, -1.224606353822377258E-16, -0.000000000000000000 ) ) ;
#105644 = CARTESIAN_POINT ( 'NONE',  ( 99.00120839754166013, -45.26735151141791391, 193.3245999471389212 ) ) ;
#105646 = CARTESIAN_POINT ( 'NONE',  ( -46.79755470960070340, 13.68519846643612503, 15.37381431200659243 ) ) ;
#105645 = CARTESIAN_POINT ( 'NONE',  ( 16.33361799548379523, 5.000000000000002665, 0.000000000000000000 ) ) ;
#105647 = CARTESIAN_POINT ( 'NONE',  ( -84.12721481491040265, -25.59031489470379483, 158.2850513293658423 ) ) ;
#105648 = EDGE_LOOP ( 'NONE', ( #64604, #49752, #92350, #28035 ) ) ;
#105649 = CIRCLE ( 'NONE', #93586, 12.00000000000003908 ) ;
#105650 = VERTEX_POINT ( 'NONE', #40780 ) ;
#105651 = ORIENTED_EDGE ( 'NONE', *, *, #36786, .F. ) ;
#105652 = CARTESIAN_POINT ( 'NONE',  ( 33.85195725564128821, 465.2464970902066739, 17.18122764674265568 ) ) ;
#105653 = AXIS2_PLACEMENT_3D ( 'NONE', #79196, #62493, #78130 ) ;
#105654 = EDGE_CURVE ( 'NONE', #96476, #96036, #66660, .T. ) ;
#105655 = CARTESIAN_POINT ( 'NONE',  ( -4.999999999999920952, -12.45789892056845716, 11.15956302481699502 ) ) ;
#105656 = CYLINDRICAL_SURFACE ( 'NONE', #10491, 1.250000000000001110 ) ;
#105657 = EDGE_LOOP ( 'NONE', ( #41054, #100345, #55490 ) ) ;
#105658 =( GEOMETRIC_REPRESENTATION_CONTEXT ( 3 ) GLOBAL_UNCERTAINTY_ASSIGNED_CONTEXT ( ( #65090 ) ) GLOBAL_UNIT_ASSIGNED_CONTEXT ( ( #7699, #6110, #71918 ) ) REPRESENTATION_CONTEXT ( 'NONE', 'WORKASPACE' ) );
#105659 = CARTESIAN_POINT ( 'NONE',  ( -2.399209547574902217E-15, 57.18445727710329862, 19.59103268995865221 ) ) ;
#105660 = AXIS2_PLACEMENT_3D ( 'NONE', #4365, #61028, #11917 ) ;
#105661 = DIRECTION ( 'NONE',  ( -0.6297424739189366738, -0.1980345732161221117, 0.7511369544587498392 ) ) ;
#105662 = CARTESIAN_POINT ( 'NONE',  ( -112.9456993887476415, -57.67119592114509175, 187.6412086615824535 ) ) ;
#105663 = CARTESIAN_POINT ( 'NONE',  ( -5.728413875956868573, -68.58064226453402057, 1.802282772585249715 ) ) ;
#105664 = DIRECTION ( 'NONE',  ( -1.000000000000000000, -0.000000000000000000, -0.000000000000000000 ) ) ;
#105665 = CIRCLE ( 'NONE', #59198, 9.000000000000000000 ) ;
#105666 = DIRECTION ( 'NONE',  ( 0.5735764363510554853, 0.8191520442889852482, 0.000000000000000000 ) ) ;
#105667 = CARTESIAN_POINT ( 'NONE',  ( 0.000000000000000000, 15.00000000000000000, -9.999999999999998224 ) ) ;
#105668 = CARTESIAN_POINT ( 'NONE',  ( -60.75193363616918418, -14.21045842199437281, -29.98592940458554779 ) ) ;
#105669 = DIRECTION ( 'NONE',  ( -0.5735764363510494901, -0.8191520442889894671, 0.000000000000000000 ) ) ;
#105670 = CARTESIAN_POINT ( 'NONE',  ( -52.09024895363909735, -32.57805271825053950, 51.93362379009405316 ) ) ;
#105671 = FACE_OUTER_BOUND ( 'NONE', #12672, .T. ) ;
#105672 = EDGE_LOOP ( 'NONE', ( #19847, #81013, #35953, #28781, #92314, #101961, #12396, #91759 ) ) ;
#105673 = CARTESIAN_POINT ( 'NONE',  ( -96.81022089726320701, -52.81206184454612895, 195.3521687869499601 ) ) ;
#105674 = CARTESIAN_POINT ( 'NONE',  ( -3.396983858844193183, 299.9646488656019869, -10.00714413801434333 ) ) ;
#105675 = EDGE_CURVE ( 'NONE', #6993, #43441, #65652, .T. ) ;
#105676 = EDGE_LOOP ( 'NONE', ( #38616, #34812, #66366, #47151 ) ) ;
#105677 = CARTESIAN_POINT ( 'NONE',  ( -17.53729400407423000, 34.16830424740683725, -24.04411209734885801 ) ) ;
#105678 = CARTESIAN_POINT ( 'NONE',  ( 110.9724741510028991, -38.35616282069194938, 175.3757637281809423 ) ) ;
#105679 = CARTESIAN_POINT ( 'NONE',  ( 49.10072971674808429, 12.98664841672423798, 16.25083509556763417 ) ) ;
#105680 = CARTESIAN_POINT ( 'NONE',  ( -7.188101187500002709, -9.687500002048384573, 2.977408999572648707 ) ) ;
#105681 = CARTESIAN_POINT ( 'NONE',  ( -15.57846540788180434, 302.5584973853110569, 9.874655226133899788 ) ) ;
#105682 = LINE ( 'NONE', #49031, #66921 ) ;
#105683 = CARTESIAN_POINT ( 'NONE',  ( 85.25163243476666253, -30.00000000000000355, 172.6556488447312177 ) ) ;
#105684 = EDGE_CURVE ( 'NONE', #10713, #1566, #24634, .T. ) ;
#105685 = CARTESIAN_POINT ( 'NONE',  ( 6.795673391948847453, 303.7372862655386143, -10.02434351962803838 ) ) ;
#105686 = CARTESIAN_POINT ( 'NONE',  ( 36.65199127662912559, 490.9971735395452583, 12.47305305857692304 ) ) ;
#105687 = FACE_OUTER_BOUND ( 'NONE', #71722, .T. ) ;
#105688 = AXIS2_PLACEMENT_3D ( 'NONE', #80462, #97182, #96668 ) ;
#105689 = ORIENTED_EDGE ( 'NONE', *, *, #42271, .F. ) ;
#105690 = ORIENTED_EDGE ( 'NONE', *, *, #22741, .T. ) ;
#105691 = CARTESIAN_POINT ( 'NONE',  ( 50.37465153049131317, -32.58476194434919648, 49.03543699400612610 ) ) ;
#105692 = CARTESIAN_POINT ( 'NONE',  ( 5.658904754127976666, 41.71506038590904808, -58.75003921181337319 ) ) ;
#105693 = CARTESIAN_POINT ( 'NONE',  ( 36.95381392810918442, 27.83278920306690551, -13.30708169601276403 ) ) ;
#105694 = ORIENTED_EDGE ( 'NONE', *, *, #62702, .F. ) ;
#105695 = CARTESIAN_POINT ( 'NONE',  ( -110.8996023805193545, -38.35620705874759295, 168.0205389799528461 ) ) ;
#105696 = ORIENTED_EDGE ( 'NONE', *, *, #37072, .T. ) ;
#105697 = CARTESIAN_POINT ( 'NONE',  ( 27.10511071441176156, 34.47735702144343861, -10.05698433968637673 ) ) ;
#105698 = CARTESIAN_POINT ( 'NONE',  ( 92.29851316895251045, -38.35437613414789126, 37.52047800107067133 ) ) ;
#105699 = CARTESIAN_POINT ( 'NONE',  ( 11.94629484552446286, 10.83030812042046520, -9.765882283547693277 ) ) ;
#105700 = CARTESIAN_POINT ( 'NONE',  ( 27.59999999999999787, 1.411358822780289120E-15, 0.000000000000000000 ) ) ;
#105701 = CARTESIAN_POINT ( 'NONE',  ( 100.5956480701022144, -45.28263325919924398, 134.9964452043381016 ) ) ;
#105702 = FILL_AREA_STYLE_COLOUR ( '', #77331 ) ;
#105703 = CARTESIAN_POINT ( 'NONE',  ( 21.96569361886355765, 28.02808497942503507, 31.91099187246623714 ) ) ;
#105704 = CARTESIAN_POINT ( 'NONE',  ( -36.51065643851772080, 361.8862209142205870, 2.816516898780279998 ) ) ;
#105705 = AXIS2_PLACEMENT_3D ( 'NONE', #55852, #38154, #86695 ) ;
#105706 = DIRECTION ( 'NONE',  ( -1.000000000000000000, -0.000000000000000000, 0.000000000000000000 ) ) ;
#105707 = CARTESIAN_POINT ( 'NONE',  ( 80.05528450392095863, -60.00000000000001421, 196.0545680023233501 ) ) ;
#105708 = PRESENTATION_LAYER_ASSIGNMENT (  '', '', ( #19615 ) ) ;
#105709 = ADVANCED_FACE ( 'NONE', ( #50457 ), #17462, .T. ) ;
#105710 = CARTESIAN_POINT ( 'NONE',  ( -15.61321260267626521, 35.02176863298834064, 22.53469681359418075 ) ) ;
#105711 = VERTEX_POINT ( 'NONE', #31660 ) ;
#105712 = CARTESIAN_POINT ( 'NONE',  ( 58.02861234676127822, -42.96355013425112190, 68.81395379777194421 ) ) ;
#105713 = CARTESIAN_POINT ( 'NONE',  ( -31.09938947669733267, 298.5175562217006586, -1.189641983160760308 ) ) ;
#105714 = DIRECTION ( 'NONE',  ( 0.000000000000000000, 0.000000000000000000, -1.000000000000000000 ) ) ;
#105715 = CARTESIAN_POINT ( 'NONE',  ( -7.450977790876272877, -5.000000000000000000, -15.56369424074723895 ) ) ;
#105716 = ORIENTED_EDGE ( 'NONE', *, *, #11199, .T. ) ;
#105718 = CARTESIAN_POINT ( 'NONE',  ( -9.287587386881233087, -52.21912220077189914, 30.70844757271691350 ) ) ;
#105717 = CARTESIAN_POINT ( 'NONE',  ( -77.30345793199742843, -30.00000000002674838, 177.7601236066231536 ) ) ;
#105719 = CARTESIAN_POINT ( 'NONE',  ( 20.59999999999999787, 1.533819458162526451E-15, 0.000000000000000000 ) ) ;
#105720 = CARTESIAN_POINT ( 'NONE',  ( 30.23373458370678790, 333.1884278479437285, 15.82348625706909573 ) ) ;
#105721 = CARTESIAN_POINT ( 'NONE',  ( -10.00000000000000000, 15.00000000000000000, 10.00000000000000000 ) ) ;
#105722 = CARTESIAN_POINT ( 'NONE',  ( -8.000000000000001776, -32.65625000000000000, 3.313708498984758943 ) ) ;
#105723 = CARTESIAN_POINT ( 'NONE',  ( -17.49999999999996803, 47.99999999999999289, 64.09953197957064219 ) ) ;
#105724 = CARTESIAN_POINT ( 'NONE',  ( 7.908030677224555660, -3.059924800338351236, -7.792662696733370531 ) ) ;
#105725 = ORIENTED_EDGE ( 'NONE', *, *, #7201, .T. ) ;
#105726 = CARTESIAN_POINT ( 'NONE',  ( 82.63461646052759590, -46.48100528357909411, 177.1123106745573637 ) ) ;
#105727 = LINE ( 'NONE', #7554, #104907 ) ;
#105728 = B_SPLINE_CURVE_WITH_KNOTS ( 'NONE', 3,
 ( #69625, #105555, #31695, #86356, #53940, #95478, #21109, #72657, #23608, #48374, #94972, #94438, #62081, #13479, #4346, #86876, #3823, #11898, #87404, #7378, #21623, #80741, #15484, #20598 ),
 .UNSPECIFIED., .F., .F.,
 ( 4, 2, 2, 2, 2, 2, 2, 2, 2, 2, 2, 4 ),
 ( 2.105069348217797382E-15, 0.0006796014968221845759, 0.001019402245232224483, 0.001359202993642264065, 0.002038804490462343879, 0.002718405987282424344, 0.003398007484102504375, 0.004077608980922584406, 0.005436811974562746202, 0.006796014968202907132, 0.008155217961843066327, 0.01087362394912343155 ),
 .UNSPECIFIED. ) ;
#105729 = CARTESIAN_POINT ( 'NONE',  ( 36.34528775465977901, 28.20980455253403463, 11.89180145376659326 ) ) ;
#105730 = VERTEX_POINT ( 'NONE', #10011 ) ;
#105731 = CARTESIAN_POINT ( 'NONE',  ( 0.000000000000000000, -100.0000000000000000, -8.000000000000007105 ) ) ;
#105732 = CIRCLE ( 'NONE', #81609, 4.000000000000007105 ) ;
#105733 = CARTESIAN_POINT ( 'NONE',  ( 25.86069633001730139, 35.07357202603378710, -8.661875674703953365 ) ) ;
#105734 = CARTESIAN_POINT ( 'NONE',  ( -7.360438360673518865, 50.00000000000000711, -75.39006186639038276 ) ) ;
#105735 = CYLINDRICAL_SURFACE ( 'NONE', #85047, 1.249999999999999334 ) ;
#105736 = ADVANCED_FACE ( 'NONE', ( #43982 ), #84261, .F. ) ;
#105737 = DIRECTION ( 'NONE',  ( 1.000000000000000000, 0.000000000000000000, 0.000000000000000000 ) ) ;
#105738 = STYLED_ITEM ( 'NONE', ( #29623 ), #97546 ) ;
#105739 = EDGE_CURVE ( 'NONE', #17510, #28693, #94125, .T. ) ;
#105740 = ORIENTED_EDGE ( 'NONE', *, *, #55334, .F. ) ;
#105741 = MECHANICAL_DESIGN_GEOMETRIC_PRESENTATION_REPRESENTATION (  '', ( #78181 ), #43772 ) ;
#105743 = AXIS2_PLACEMENT_3D ( 'NONE', #54499, #22188, #79854 ) ;
#105742 = FILL_AREA_STYLE_COLOUR ( '', #28193 ) ;
#105744 = B_SPLINE_CURVE_WITH_KNOTS ( 'NONE', 3,
 ( #49183, #57807, #72923, #40049, #64853, #81020, #105834, #24952, #49726, #56196, #603, #82633, #33568, #91275, #7138, #31977, #73457, #8735, #99324, #25498, #50260, #83162, #23901, #106355, #56743, #98281, #90193, #16295, #1698, #93917, #68039, #58905, #51849, #51308, #42703, #52378, #75600, #34654, #84761, #36255, #50769, #67523, #101478, #59980, #17916, #68593, #100404, #10844, #69124, #19005 ),
 .UNSPECIFIED., .F., .F.,
 ( 4, 2, 2, 2, 2, 2, 2, 2, 2, 2, 2, 2, 2, 2, 2, 2, 2, 2, 2, 2, 2, 2, 2, 2, 4 ),
 ( 0.0001642028872464954957, 0.008867656351590888150, 0.01757110981593528257, 0.03497801674462389793, 0.05238492367331251676, 0.06979183060200115640, 0.08719873753068978217, 0.09590219099503416444, 0.1046056444593785467, 0.1089573711915507448, 0.1133090979237229429, 0.1176608246558951409, 0.1220125513880673390, 0.1263642781202395371, 0.1285401414863256431, 0.1307160048524117213, 0.1328918682184978273, 0.1339797999015408803, 0.1345237657430624068, 0.1350677315845839332, 0.1356116974261054597, 0.1361556632676269862, 0.1372435949506700947, 0.1383315266337132032, 0.1394194583167563117 ),
 .UNSPECIFIED. ) ;
#105745 = ADVANCED_FACE ( 'NONE', ( #100081 ), #26248, .F. ) ;
#105746 = CARTESIAN_POINT ( 'NONE',  ( 6.499999999999998224, -4.012858516023022126, -6.470130706010832178 ) ) ;
#105747 = CARTESIAN_POINT ( 'NONE',  ( 4.684274960302871098E-15, 26.07813853931757464, 38.25000000000000000 ) ) ;
#105749 = CARTESIAN_POINT ( 'NONE',  ( -10.64016296546354923, 13.00014743456769928, -10.01963642081249617 ) ) ;
#105748 = CARTESIAN_POINT ( 'NONE',  ( -19.42089550010631172, -25.33333743194299359, 36.70181951355001360 ) ) ;
#105750 = CARTESIAN_POINT ( 'NONE',  ( 2.977408999572650927, -11.37500000204838813, -7.188101187500001821 ) ) ;
#105751 = CARTESIAN_POINT ( 'NONE',  ( 6.400000000000000355, 0.000000000000000000, -5.400000000000001243 ) ) ;
#105752 = CARTESIAN_POINT ( 'NONE',  ( -16.75187969033554936, -1.200000000000000030E-05, -23.05698433968595751 ) ) ;
#105753 = VERTEX_POINT ( 'NONE', #12659 ) ;
#105754 = CARTESIAN_POINT ( 'NONE',  ( 30.00000000000000000, 450.0000000000002274, 13.20242257375370976 ) ) ;
#105755 = DIRECTION ( 'NONE',  ( -1.000000000000000000, -0.000000000000000000, -0.000000000000000000 ) ) ;
#105756 = CARTESIAN_POINT ( 'NONE',  ( -8.618528913669065261, 129.1314578643986408, -4.999999999998729017 ) ) ;
#105757 = CARTESIAN_POINT ( 'NONE',  ( -7.758748231291410669, -5.000000000000001776, -73.00623724569611284 ) ) ;
#105758 = CARTESIAN_POINT ( 'NONE',  ( -15.39795322966403290, 3.054092008348469722, 2.852131183246390034 ) ) ;
#105759 = CONICAL_SURFACE ( 'NONE', #73030, 4.000000000000001776, 0.9599310885968774798 ) ;
#105760 = VERTEX_POINT ( 'NONE', #87111 ) ;
#105761 = CYLINDRICAL_SURFACE ( 'NONE', #67057, 13.27631144943088515 ) ;
#105762 = DIRECTION ( 'NONE',  ( -1.000000000000000000, -1.224606353822377258E-16, -0.000000000000000000 ) ) ;
#105763 = ORIENTED_EDGE ( 'NONE', *, *, #54901, .F. ) ;
#105765 = EDGE_CURVE ( 'NONE', #80889, #103547, #63371, .T. ) ;
#105764 = B_SPLINE_CURVE_WITH_KNOTS ( 'NONE', 3,
 ( #71232, #104128, #31348, #22721, #7023, #56630, #72811, #97100, #55559, #15117, #88495, #31861, #23782, #22184, #89551, #15647 ),
 .UNSPECIFIED., .F., .F.,
 ( 4, 2, 2, 2, 2, 2, 2, 4 ),
 ( 2.111010400649636311E-15, 0.003002507059513599523, 0.004503760589269341537, 0.006005014119025082683, 0.006755640883902953690, 0.007506267648780824697, 0.009007521178536564976, 0.01201002823804804380 ),
 .UNSPECIFIED. ) ;
#105766 = DIRECTION ( 'NONE',  ( -1.000000000000000000, -0.000000000000000000, -0.000000000000000000 ) ) ;
#105767 = CARTESIAN_POINT ( 'NONE',  ( -42.65225745549071235, 39.48366440724160498, -49.42417087154653643 ) ) ;
#105768 = CIRCLE ( 'NONE', #14693, 5.000000000000002665 ) ;
#105769 = CARTESIAN_POINT ( 'NONE',  ( -112.0884059626418860, -60.00000000000000711, 178.1755789913165984 ) ) ;
#105770 = CARTESIAN_POINT ( 'NONE',  ( 29.50962187807837012, 13.72866526111394947, -42.09567151085946790 ) ) ;
#105771 = CARTESIAN_POINT ( 'NONE',  ( 6.087340769098095516E-05, -60.36594248999337964, 33.95064037460127793 ) ) ;
#105772 = CIRCLE ( 'NONE', #64462, 4.000000000000001776 ) ;
#105773 = CARTESIAN_POINT ( 'NONE',  ( 21.25502769577498796, 305.0480251235313176, 9.978840188629131802 ) ) ;
#105774 = DIRECTION ( 'NONE',  ( -1.000000000000000000, -1.224606353822377258E-16, -0.000000000000000000 ) ) ;
#105776 = CARTESIAN_POINT ( 'NONE',  ( 0.000000000000000000, 0.5000000000000000000, 0.000000000000000000 ) ) ;
#105775 = CARTESIAN_POINT ( 'NONE',  ( 11.68767211932355998, -5.000000000000002665, -81.85902538600510070 ) ) ;
#105777 = ADVANCED_FACE ( 'NONE', ( #71423 ), #58808, .T. ) ;
#105778 = CARTESIAN_POINT ( 'NONE',  ( -83.17772658434090260, -42.98067204979764000, 176.6392034412271528 ) ) ;
#105779 = VERTEX_POINT ( 'NONE', #96268 ) ;
#105780 = CONICAL_SURFACE ( 'NONE', #69621, 4.000000000000001776, 0.9599310885968774798 ) ;
#105781 =( NAMED_UNIT ( * ) PLANE_ANGLE_UNIT ( ) SI_UNIT ( $, .RADIAN. ) );
#105782 = VERTEX_POINT ( 'NONE', #104327 ) ;
#105783 = ORIENTED_EDGE ( 'NONE', *, *, #16953, .F. ) ;
#105784 = CARTESIAN_POINT ( 'NONE',  ( -16.75187969033554936, 37.11970326878314097, -21.80698433968595751 ) ) ;
#105785 = EDGE_CURVE ( 'NONE', #104590, #14360, #56440, .T. ) ;
#105786 = CARTESIAN_POINT ( 'NONE',  ( 12.61650669486618881, -3.999999999999998224, 0.000000000000000000 ) ) ;
#105787 = CARTESIAN_POINT ( 'NONE',  ( 0.000000000000000000, 38.67090180175566871, 0.000000000000000000 ) ) ;
#105788 =( LENGTH_UNIT ( ) NAMED_UNIT ( * ) SI_UNIT ( .MILLI., .METRE. ) );
#105789 = CARTESIAN_POINT ( 'NONE',  ( 8.830661707067434918, 18.20374273969088819, -5.000000000000000888 ) ) ;
#105790 = CARTESIAN_POINT ( 'NONE',  ( 0.000000000000000000, 0.000000000000000000, 0.000000000000000000 ) ) ;
#105791 = CARTESIAN_POINT ( 'NONE',  ( 0.4969600502617480542, 4.995646404165275278, -7.347286611336972584 ) ) ;
#105792 = CARTESIAN_POINT ( 'NONE',  ( 114.0746655879125200, -59.99999999999997158, 159.9914145889356121 ) ) ;
#105793 = CARTESIAN_POINT ( 'NONE',  ( -113.8519240760089133, -60.00000000000002842, 157.1483645435538108 ) ) ;
#105794 = CARTESIAN_POINT ( 'NONE',  ( -63.00954343448449180, -39.48637485122225144, 80.42972209915033943 ) ) ;
#105795 = ORIENTED_EDGE ( 'NONE', *, *, #74405, .T. ) ;
#105796 = CARTESIAN_POINT ( 'NONE',  ( -53.90990825086682037, 38.95404129820931161, 33.99650454723879278 ) ) ;
#105797 = CARTESIAN_POINT ( 'NONE',  ( 113.3142912537098539, -60.00000000000000000, 187.7786430344451674 ) ) ;
#105798 = EDGE_LOOP ( 'NONE', ( #68668, #92163 ) ) ;
#105799 = CARTESIAN_POINT ( 'NONE',  ( 4.363475717344336561E-05, -49.91581431533978019, 32.20895234549234232 ) ) ;
#105800 = CARTESIAN_POINT ( 'NONE',  ( -7.188101187500002709, -14.18750000204838457, 2.977408999572647819 ) ) ;
#105801 = CARTESIAN_POINT ( 'NONE',  ( -43.94716957228371967, 463.1429429498322747, 4.278538522888820417 ) ) ;
#105802 = ORIENTED_EDGE ( 'NONE', *, *, #86276, .F. ) ;
#105803 = CARTESIAN_POINT ( 'NONE',  ( 35.03615891056482923, 464.5070978657896035, 18.87180892930519605 ) ) ;
#105804 = ORIENTED_EDGE ( 'NONE', *, *, #104559, .T. ) ;
#105805 = DIRECTION ( 'NONE',  ( -0.000000000000000000, -1.000000000000000000, -0.000000000000000000 ) ) ;
#105806 = AXIS2_PLACEMENT_3D ( 'NONE', #80264, #56518, #73770 ) ;
#105807 = CARTESIAN_POINT ( 'NONE',  ( -1.320432766682874540E-15, -28.90625000204838813, 7.188101187500000044 ) ) ;
#105808 = CARTESIAN_POINT ( 'NONE',  ( -87.83100605766939850, -59.99999999999994316, 201.3292211320413401 ) ) ;
#105809 = CARTESIAN_POINT ( 'NONE',  ( 9.981808881366681874, -57.97224676535203969, 27.65604031336897251 ) ) ;
#105810 = CARTESIAN_POINT ( 'NONE',  ( -2.977408999572654480, -26.00000000204839168, 7.188101187499999156 ) ) ;
#105811 = CARTESIAN_POINT ( 'NONE',  ( 46.00000000000000000, 462.1625373399974137, 5.827014411081228751 ) ) ;
#105812 = AXIS2_PLACEMENT_3D ( 'NONE', #40473, #72314, #23798 ) ;
#105813 = CARTESIAN_POINT ( 'NONE',  ( -3.788334298886703255, 19.16274404829667688, -5.887494290764028193 ) ) ;
#105814 = LINE ( 'NONE', #72904, #34052 ) ;
#105815 = EDGE_CURVE ( 'NONE', #5290, #39650, #3755, .T. ) ;
#105816 = CARTESIAN_POINT ( 'NONE',  ( -7.343637806710344051, 107.4436312190061784, 3.177475076494675310 ) ) ;
#105817 = CARTESIAN_POINT ( 'NONE',  ( -42.68011869748734455, 337.5389550235125284, 8.263828678100116676 ) ) ;
#105818 = CARTESIAN_POINT ( 'NONE',  ( 103.2567985417785650, -60.00000000000000000, 192.3623435299448090 ) ) ;
#105819 = CARTESIAN_POINT ( 'NONE',  ( -34.09410029386582863, -56.83839777928749015, 38.12311633126902422 ) ) ;
#105820 = DIRECTION ( 'NONE',  ( -0.000000000000000000, 1.000000000000000000, -0.000000000000000000 ) ) ;
#105821 = CARTESIAN_POINT ( 'NONE',  ( 39.17175573955607604, -39.51526351848063001, 38.04212958671963207 ) ) ;
#105822 = CARTESIAN_POINT ( 'NONE',  ( 2.083846472846741813E-15, -1.734723475976807094E-15, 17.01589776168603407 ) ) ;
#105823 = ORIENTED_EDGE ( 'NONE', *, *, #67144, .T. ) ;
#105824 = FACE_OUTER_BOUND ( 'NONE', #52713, .T. ) ;
#105825 = CARTESIAN_POINT ( 'NONE',  ( -73.89011895107292105, -38.32652016529552697, 159.4283385861867259 ) ) ;
#105826 = VERTEX_POINT ( 'NONE', #82170 ) ;
#105828 = CARTESIAN_POINT ( 'NONE',  ( 44.43774958859658142, 337.2802145563449017, 0.2445019049555710311 ) ) ;
#105827 = CARTESIAN_POINT ( 'NONE',  ( 46.08349330513379982, 1.593028355512270567E-15, 0.000000000000000000 ) ) ;
#105830 = EDGE_CURVE ( 'NONE', #104368, #35586, #8813, .T. ) ;
#105829 = CARTESIAN_POINT ( 'NONE',  ( -33.08902662346056900, 439.4144565034866901, 23.84226355454047663 ) ) ;
#105831 = CARTESIAN_POINT ( 'NONE',  ( -6.831363903021532735, 41.73171925724633979, -59.17722475679354233 ) ) ;
#105832 = DIRECTION ( 'NONE',  ( -1.000000000000000000, 0.000000000000000000, 0.000000000000000000 ) ) ;
#105833 = CARTESIAN_POINT ( 'NONE',  ( 11.89131030317610183, 5.000000000000002665, 0.000000000000000000 ) ) ;
#105834 = CARTESIAN_POINT ( 'NONE',  ( -31.43654312788580896, 409.1921748638893064, 24.49080981961512293 ) ) ;
#105835 = CARTESIAN_POINT ( 'NONE',  ( 0.3167204509598374740, -8.479269695850863542, 1.313474075707213640 ) ) ;
#105836 = CARTESIAN_POINT ( 'NONE',  ( 95.45595281539657151, -60.00000000000001421, 52.28868166623287550 ) ) ;
#105837 = CARTESIAN_POINT ( 'NONE',  ( 0.7145311798161605443, -4.618802153517258979, -8.000000000000001776 ) ) ;
#105838 = CARTESIAN_POINT ( 'NONE',  ( 32.33349330513380693, 1.593028355512270962E-15, 0.000000000000000000 ) ) ;
#105839 = CARTESIAN_POINT ( 'NONE',  ( -46.00000000000000000, 500.0000000000002274, 12.00000000000000711 ) ) ;
#105840 = ORIENTED_EDGE ( 'NONE', *, *, #88580, .T. ) ;
#105841 = AXIS2_PLACEMENT_3D ( 'NONE', #44165, #2084, #75454 ) ;
#105842 = CARTESIAN_POINT ( 'NONE',  ( -88.54670987746852973, -29.99999999999983302, -15.93061657816609333 ) ) ;
#105843 = VERTEX_POINT ( 'NONE', #24518 ) ;
#105844 = CARTESIAN_POINT ( 'NONE',  ( 53.78349330513380266, 6.975173280561618775E-15, 0.000000000000000000 ) ) ;
#105845 = CARTESIAN_POINT ( 'NONE',  ( -15.20081118350138993, 3.404146808183821982, -3.872164105968183279 ) ) ;
#105846 = CARTESIAN_POINT ( 'NONE',  ( 4.898587196589412829E-16, -13.81250000409676915, -8.000000000000000000 ) ) ;
#105847 = CARTESIAN_POINT ( 'NONE',  ( -33.47652930794097870, 484.3276552595484077, 3.198545968219471458 ) ) ;
#105848 = CARTESIAN_POINT ( 'NONE',  ( 4.401442555609581635E-16, -26.65625000204838813, -7.188101187500000044 ) ) ;
#105849 = CARTESIAN_POINT ( 'NONE',  ( -3.778364440264291524, -1.120180266064636276, 103.2432911248131120 ) ) ;
#105850 = CARTESIAN_POINT ( 'NONE',  ( 7.069742150690450089, 41.66287055390499461, -69.58314084581829206 ) ) ;
#105851 = B_SPLINE_CURVE_WITH_KNOTS ( 'NONE', 3,
 ( #98766, #73427, #17356, #1117, #46, #50230 ),
 .UNSPECIFIED., .F., .F.,
 ( 4, 2, 4 ),
 ( 0.003841072314098388854, 0.005765657563962199410, 0.007690242813826009965 ),
 .UNSPECIFIED. ) ;
#105852 = EDGE_LOOP ( 'NONE', ( #102267, #91572, #45273, #102085 ) ) ;
#105853 = AXIS2_PLACEMENT_3D ( 'NONE', #96856, #22982, #54773 ) ;
#105854 = PRESENTATION_LAYER_ASSIGNMENT (  '', '', ( #23197 ) ) ;
#105855 = APPLICATION_CONTEXT ( 'automotive_design' ) ;
#105857 = VERTEX_POINT ( 'NONE', #7221 ) ;
#105856 = CARTESIAN_POINT ( 'NONE',  ( 7.000000000000000000, 0.000000000000000000, -9.975036109638290682 ) ) ;
#105858 = CARTESIAN_POINT ( 'NONE',  ( 83.89881790786340332, -18.68023142264728520, 147.1895477365627585 ) ) ;
#105859 = VECTOR ( 'NONE', #27081, 1000.000000000000114 ) ;
#105860 = LINE ( 'NONE', #97762, #72941 ) ;
#105861 = ORIENTED_EDGE ( 'NONE', *, *, #94630, .T. ) ;
#105862 = CARTESIAN_POINT ( 'NONE',  ( -54.98704968389372993, 50.00000000000000711, 30.77402402440401019 ) ) ;
#105863 = CARTESIAN_POINT ( 'NONE',  ( 7.344361273354515163, -87.44560530588523761, -3.175733139645588121 ) ) ;
#105864 = CARTESIAN_POINT ( 'NONE',  ( -7.188101187500000044, -12.40625000204838635, -8.802885111219163269E-16 ) ) ;
#105865 = CARTESIAN_POINT ( 'NONE',  ( 4.699999999999999289, 5.629165124598843661, -3.250000000000011990 ) ) ;
#105866 = CARTESIAN_POINT ( 'NONE',  ( -42.46252528007325111, -57.68686955033432895, 59.97785686028149854 ) ) ;
#105867 = CARTESIAN_POINT ( 'NONE',  ( 6.562974947121713143, -7.579827465851456836, -0.5629870116737628605 ) ) ;
#105868 = EDGE_CURVE ( 'NONE', #58075, #21912, #55098, .T. ) ;
#105869 = VERTEX_POINT ( 'NONE', #82714 ) ;
#105870 = CARTESIAN_POINT ( 'NONE',  ( 2.955787000303755185, 98.65688599150308846, 5.000000000000000000 ) ) ;
#105871 = EDGE_CURVE ( 'NONE', #20011, #66540, #66531, .T. ) ;
#105872 = CARTESIAN_POINT ( 'NONE',  ( 7.417432790609828963, 41.15875988143464781, -59.49136470043579550 ) ) ;
#105873 = CARTESIAN_POINT ( 'NONE',  ( 48.28140683493008822, 14.38570471689693875, -16.83761797438825525 ) ) ;
#105874 = ORIENTED_EDGE ( 'NONE', *, *, #13911, .F. ) ;
#105875 = CARTESIAN_POINT ( 'NONE',  ( -3.313708498984765161, -10.15625000409677092, 7.999999999999998224 ) ) ;
#105876 = CARTESIAN_POINT ( 'NONE',  ( -11.00522668414577154, -14.01981851350334018, 31.84261960800534297 ) ) ;
#105877 = CARTESIAN_POINT ( 'NONE',  ( 9.910377230549926253, 15.23810023151367155, 1.510421413154057424 ) ) ;
#105878 = CARTESIAN_POINT ( 'NONE',  ( -2.500000000000011990, -30.00000000000000000, -31.87333704504306908 ) ) ;
#105879 = DIRECTION ( 'NONE',  ( 0.000000000000000000, 0.000000000000000000, 1.000000000000000000 ) ) ;
#105880 = APPLICATION_PROTOCOL_DEFINITION ( 'draft international standard', 'automotive_design', 1998, #23198 ) ;
#105881 = CARTESIAN_POINT ( 'NONE',  ( -9.176645556628255207, 30.52739032406730502, 3.973966573947708802 ) ) ;
#105882 = ORIENTED_EDGE ( 'NONE', *, *, #15856, .F. ) ;
#105883 = CARTESIAN_POINT ( 'NONE',  ( 3.250000000000015099, 5.629165124598843661, 1.734723475976807094E-15 ) ) ;
#105884 = CARTESIAN_POINT ( 'NONE',  ( 12.76511086933744998, 42.41840947608824308, -92.95087395602729430 ) ) ;
#105885 = CIRCLE ( 'NONE', #49056, 8.605212085995399107 ) ;
#105886 = CARTESIAN_POINT ( 'NONE',  ( -62.60825180612043539, -37.65708592411966293, -33.50786494313757657 ) ) ;
#105887 = CARTESIAN_POINT ( 'NONE',  ( -3.857142857142847880, -48.79941684889506348, 103.1763305333244318 ) ) ;
#105888 = ADVANCED_FACE ( 'NONE', ( #39622 ), #41845, .T. ) ;
#105889 = ORIENTED_EDGE ( 'NONE', *, *, #91415, .F. ) ;
#105890 = CARTESIAN_POINT ( 'NONE',  ( -7.000000000000000000, 8.572527594031473190E-16, -9.975036109638290682 ) ) ;
#105891 = CARTESIAN_POINT ( 'NONE',  ( 106.3456735113185374, -57.65092651592087236, 200.6602391493835285 ) ) ;
#105892 = CARTESIAN_POINT ( 'NONE',  ( 37.04971407824480423, 463.3105192861256114, 20.11836016812624806 ) ) ;
#105893 = EDGE_CURVE ( 'NONE', #103460, #106458, #76029, .T. ) ;
#105894 = CARTESIAN_POINT ( 'NONE',  ( -9.761574416223039563, 51.33888487989963778, -2.428418878555363314 ) ) ;
#105895 = CARTESIAN_POINT ( 'NONE',  ( -6.536939020983855819, 53.59930666568121183, 7.161232122323571758 ) ) ;
#105896 = CARTESIAN_POINT ( 'NONE',  ( -74.34434612437654266, -60.00000000000000000, 175.6378450051794573 ) ) ;
#105897 = CARTESIAN_POINT ( 'NONE',  ( -40.95420997525301487, 387.0967036739339164, 27.26945002580065136 ) ) ;
#105898 = CARTESIAN_POINT ( 'NONE',  ( -29.50756122520733271, 297.9063904818165724, 10.61050061783298126 ) ) ;
#105899 = CARTESIAN_POINT ( 'NONE',  ( -85.39200440104596623, -35.72338773939898715, 183.0114852614501331 ) ) ;
#105900 = ORIENTED_EDGE ( 'NONE', *, *, #22127, .F. ) ;
#105901 = CARTESIAN_POINT ( 'NONE',  ( 28.01912030120706021, 308.6873964030780257, -8.131358077288096453 ) ) ;
#105902 = ORIENTED_EDGE ( 'NONE', *, *, #37660, .T. ) ;
#105903 = CARTESIAN_POINT ( 'NONE',  ( 16.04705908622415933, 4.602417526209643839, -3.432813300957220815 ) ) ;
#105904 = EDGE_CURVE ( 'NONE', #26151, #23846, #34813, .T. ) ;
#105905 = AXIS2_PLACEMENT_3D ( 'NONE', #68043, #100941, #20081 ) ;
#105906 = DIRECTION ( 'NONE',  ( -0.000000000000000000, -0.000000000000000000, -1.000000000000000000 ) ) ;
#105907 = CARTESIAN_POINT ( 'NONE',  ( 13.09999999999999787, 1.533819458162526451E-15, 0.000000000000000000 ) ) ;
#105908 = CARTESIAN_POINT ( 'NONE',  ( -44.57115381837943602, 434.3516557708484243, 14.78613344168394583 ) ) ;
#105909 = ORIENTED_EDGE ( 'NONE', *, *, #85776, .T. ) ;
#105910 = AXIS2_PLACEMENT_3D ( 'NONE', #1692, #59431, #9781 ) ;
#105911 = CARTESIAN_POINT ( 'NONE',  ( 27.42311158548955419, 36.77212537659387692, -7.587845593855179871 ) ) ;
#105912 = CARTESIAN_POINT ( 'NONE',  ( 5.694238939648077036, 41.34481830655865764, -58.37580827183571586 ) ) ;
#105913 = CARTESIAN_POINT ( 'NONE',  ( 2.910977163136224011, -8.673617379884035472E-16, 22.23822744035697241 ) ) ;
#105914 = CARTESIAN_POINT ( 'NONE',  ( -37.06716861312675348, 464.0035714960436621, 19.58716087303068676 ) ) ;
#105915 = CARTESIAN_POINT ( 'NONE',  ( 88.04031092259528180, -30.00000000000002842, -17.07720529721093072 ) ) ;
#105916 = CARTESIAN_POINT ( 'NONE',  ( -78.57144265810380546, -39.49830219292440603, 137.4485770626870362 ) ) ;
#105917 = STYLED_ITEM ( 'NONE', ( #77931 ), #87591 ) ;
#105918 = ORIENTED_EDGE ( 'NONE', *, *, #103276, .F. ) ;
#105919 = CARTESIAN_POINT ( 'NONE',  ( 34.60434289261801410, -60.00000000000002842, 49.20687062438629056 ) ) ;
#105920 = CARTESIAN_POINT ( 'NONE',  ( 14.29190075645216851, 12.99999999999999289, 0.000000000000000000 ) ) ;
#105921 = CARTESIAN_POINT ( 'NONE',  ( 93.43194010991950904, -57.65434931037806621, -16.06956276475861145 ) ) ;
#105922 = AXIS2_PLACEMENT_3D ( 'NONE', #22557, #14400, #6312 ) ;
#105923 = COLOUR_RGB ( '', 0.72549020, 0.75294118, 0.79215686) ;
#105924 = CARTESIAN_POINT ( 'NONE',  ( 0.000000000000000000, -30.00000000000000000, 0.000000000000000000 ) ) ;
#105925 = CONICAL_SURFACE ( 'NONE', #47407, 6.500000000000000000, 1.047197551196600296 ) ;
#105926 = FACE_OUTER_BOUND ( 'NONE', #15788, .T. ) ;
#105927 = ORIENTED_EDGE ( 'NONE', *, *, #9871, .T. ) ;
#105928 = AXIS2_PLACEMENT_3D ( 'NONE', #15607, #88457, #14533 ) ;
#105929 = DIRECTION ( 'NONE',  ( 0.000000000000000000, 1.000000000000000000, 0.000000000000000000 ) ) ;
#105930 = FACE_OUTER_BOUND ( 'NONE', #11241, .T. ) ;
#105931 = CARTESIAN_POINT ( 'NONE',  ( 15.66273129163408484, 43.86900239055839990, 6.199110369967553602 ) ) ;
#105932 = CARTESIAN_POINT ( 'NONE',  ( -5.082755093536325042, -20.09375000204838457, -5.082755093536325930 ) ) ;
#105933 = CARTESIAN_POINT ( 'NONE',  ( 28.17977184163764193, 6.123233995736772199E-16, -5.000000000000001776 ) ) ;
#105934 =( GEOMETRIC_REPRESENTATION_CONTEXT ( 3 ) GLOBAL_UNCERTAINTY_ASSIGNED_CONTEXT ( ( #71719 ) ) GLOBAL_UNIT_ASSIGNED_CONTEXT ( ( #85879, #36287, #29775 ) ) REPRESENTATION_CONTEXT ( 'NONE', 'WORKASPACE' ) );
#105935 =( BOUNDED_CURVE ( )  B_SPLINE_CURVE ( 2, ( #78254, #14032, #4907, #53458, #79836, #30255, #61566, #4367, #5942 ),
 .UNSPECIFIED., .F., .F. ) 
 B_SPLINE_CURVE_WITH_KNOTS ( ( 3, 2, 2, 2, 3 ),
 ( 0.2794117647058823040, 0.2867647058823528661, 0.2941176470588234837, 0.3014705882352940458, 0.3088235294117646634 ),
 .UNSPECIFIED. ) 
 CURVE ( )  GEOMETRIC_REPRESENTATION_ITEM ( )  RATIONAL_B_SPLINE_CURVE ( ( 1.000000000000000666, 0.9238795325112861834, 1.000000000000000000, 0.9238795325112867385, 1.000000000000000000, 0.9238795325112867385, 1.000000000000000000, 0.9238795325112872936, 0.9999999999999994449 ) ) 
 REPRESENTATION_ITEM ( '' )  );
#105936 = CARTESIAN_POINT ( 'NONE',  ( 9.989435848181784650, 81.02619707471572497, -0.5278651953176017875 ) ) ;
#105937 = DIRECTION ( 'NONE',  ( 0.000000000000000000, 0.000000000000000000, 1.000000000000000000 ) ) ;
#105938 = EDGE_CURVE ( 'NONE', #96258, #106589, #15826, .T. ) ;
#105939 = CARTESIAN_POINT ( 'NONE',  ( -17.62344211657769577, 45.49768958935467822, -4.615364168318502713 ) ) ;
#105940 = DIRECTION ( 'NONE',  ( 0.000000000000000000, -0.5000000000000018874, -0.8660254037844374864 ) ) ;
#105941 = ORIENTED_EDGE ( 'NONE', *, *, #98530, .F. ) ;
#105942 = DIRECTION ( 'NONE',  ( 0.000000000000000000, -1.000000000000000000, 0.000000000000000000 ) ) ;
#105944 = CARTESIAN_POINT ( 'NONE',  ( 29.28785219392642603, -29.06229949932505363, 31.04084042630147877 ) ) ;
#105943 = CARTESIAN_POINT ( 'NONE',  ( 0.4969600502617519400, 8.860760056385744932, 0.6527133886630308579 ) ) ;
#105945 = CARTESIAN_POINT ( 'NONE',  ( 24.43733964430219530, 27.40365649514079038, -32.24112188980117111 ) ) ;
#105946 = VERTEX_POINT ( 'NONE', #72364 ) ;
#105947 = EDGE_CURVE ( 'NONE', #82322, #81756, #60582, .T. ) ;
#105948 = ORIENTED_EDGE ( 'NONE', *, *, #106341, .T. ) ;
#105950 = FACE_BOUND ( 'NONE', #41340, .T. ) ;
#105949 = SURFACE_SIDE_STYLE ('',( #48241 ) ) ;
#105951 = CARTESIAN_POINT ( 'NONE',  ( 13.58349330513380515, 1.593028355512270962E-15, 0.000000000000000000 ) ) ;
#105952 = CARTESIAN_POINT ( 'NONE',  ( 6.900000000000000355, 0.000000000000000000, -0.7702282920306786629 ) ) ;
#105953 = CARTESIAN_POINT ( 'NONE',  ( -5.656854249492381470, -19.25000000409677270, 5.656854249492379694 ) ) ;
#105954 = CARTESIAN_POINT ( 'NONE',  ( 0.7768295077518341252, 46.10996703314370393, 16.51725890612300418 ) ) ;
#105955 = VERTEX_POINT ( 'NONE', #73950 ) ;
#105956 = CARTESIAN_POINT ( 'NONE',  ( 65.77608706097059610, -60.00000000000001421, -33.96223278568422899 ) ) ;
#105957 = CARTESIAN_POINT ( 'NONE',  ( 32.91772945487191038, 464.9199415683442567, 10.91424143556163351 ) ) ;
#105959 = EDGE_CURVE ( 'NONE', #20, #5264, #65340, .T. ) ;
#105958 = CARTESIAN_POINT ( 'NONE',  ( 0.000000000000000000, 60.33964880548970200, -13.06657876680918662 ) ) ;
#105960 = CARTESIAN_POINT ( 'NONE',  ( -3.122594241999163689, -5.000000000000000888, -96.69514296588273794 ) ) ;
#105961 = AXIS2_PLACEMENT_3D ( 'NONE', #99914, #76166, #26607 ) ;
#105962 = CARTESIAN_POINT ( 'NONE',  ( 47.07197767030555724, 13.48831169381993256, -14.79015211622768788 ) ) ;
#105963 = VERTEX_POINT ( 'NONE', #41065 ) ;
#105964 = ORIENTED_EDGE ( 'NONE', *, *, #71142, .T. ) ;
#105965 = ORIENTED_EDGE ( 'NONE', *, *, #28617, .F. ) ;
#105966 = FACE_OUTER_BOUND ( 'NONE', #81526, .T. ) ;
#105967 = CARTESIAN_POINT ( 'NONE',  ( 19.51720561627331918, 41.98713188461248080, -83.66827837336637685 ) ) ;
#105968 = CARTESIAN_POINT ( 'NONE',  ( 31.48211130897418641, 326.9585451694341600, 15.85107797452106659 ) ) ;
#105969 = CARTESIAN_POINT ( 'NONE',  ( -45.39376174025734656, 370.9991130468319511, 6.147894588093572921 ) ) ;
#105970 = CARTESIAN_POINT ( 'NONE',  ( -5.076380833017271499, -61.76466786245471496, 13.90212445768889360 ) ) ;
#105971 = DIRECTION ( 'NONE',  ( -1.000000000000000000, -1.224606353822377258E-16, -0.000000000000000000 ) ) ;
#105972 = DIRECTION ( 'NONE',  ( -0.5735764363510494901, -0.8191520442889894671, 0.000000000000000000 ) ) ;
#105973 = VERTEX_POINT ( 'NONE', #105268 ) ;
#105974 = CARTESIAN_POINT ( 'NONE',  ( 30.64306277920978516, 7.829637822906585498, 41.65859565436451817 ) ) ;
#105975 = ORIENTED_EDGE ( 'NONE', *, *, #9145, .T. ) ;
#105976 = DIRECTION ( 'NONE',  ( -1.000000000000000000, 0.000000000000000000, 0.000000000000000000 ) ) ;
#105977 = CARTESIAN_POINT ( 'NONE',  ( -6.500000000000000000, -3.752776749732588346, -6.177802698399963433 ) ) ;
#105978 = LINE ( 'NONE', #70978, #21514 ) ;
#105979 = CARTESIAN_POINT ( 'NONE',  ( -10.43488688844078993, -60.00000000000002132, 33.89243132277722736 ) ) ;
#105980 = CARTESIAN_POINT ( 'NONE',  ( 65.36469853637363769, -29.05439105967825952, 81.83063248125246503 ) ) ;
#105981 =( GEOMETRIC_REPRESENTATION_CONTEXT ( 3 ) GLOBAL_UNCERTAINTY_ASSIGNED_CONTEXT ( ( #60210 ) ) GLOBAL_UNIT_ASSIGNED_CONTEXT ( ( #39591, #14746, #104842 ) ) REPRESENTATION_CONTEXT ( 'NONE', 'WORKASPACE' ) );
#105982 = ORIENTED_EDGE ( 'NONE', *, *, #86457, .T. ) ;
#105983 = CARTESIAN_POINT ( 'NONE',  ( 55.63518754870391803, 38.95383793067261990, 32.06611684423706521 ) ) ;
#105984 = CARTESIAN_POINT ( 'NONE',  ( 0.1061556211655389909, -6.421950209808288790, -1.876855952934451510 ) ) ;
#105985 = CARTESIAN_POINT ( 'NONE',  ( -57.15598917327103834, -57.67115757216583205, -38.38010944898898202 ) ) ;
#105986 = ADVANCED_FACE ( 'NONE', ( #80975 ), #12236, .F. ) ;
#105987 = CIRCLE ( 'NONE', #105905, 5.000000000000002665 ) ;
#105988 = ORIENTED_EDGE ( 'NONE', *, *, #27017, .T. ) ;
#105989 = CARTESIAN_POINT ( 'NONE',  ( 47.18437091044133069, 18.47854193719496152, 14.68206053360883878 ) ) ;
#105990 = AXIS2_PLACEMENT_3D ( 'NONE', #52623, #85553, #95235 ) ;
#105991 = EDGE_CURVE ( 'NONE', #99690, #69241, #24492, .T. ) ;
#105992 = CARTESIAN_POINT ( 'NONE',  ( -36.50840931122232291, 491.4427145161785120, 12.32866606332187942 ) ) ;
#105993 = CARTESIAN_POINT ( 'NONE',  ( 5.656854249492378806, -27.87500000409677270, 5.656854249492381470 ) ) ;
#105994 = VECTOR ( 'NONE', #95112, 1000.000000000000000 ) ;
#105995 = CARTESIAN_POINT ( 'NONE',  ( -8.000000000000000000, -4.999999999999998224, -2.094395098902523955 ) ) ;
#105996 = CARTESIAN_POINT ( 'NONE',  ( 9.842984802582154913, 246.4093040952433853, 1.781981959250515946 ) ) ;
#105997 = AXIS2_PLACEMENT_3D ( 'NONE', #34722, #76725, #35791 ) ;
#105998 = CARTESIAN_POINT ( 'NONE',  ( -10.00190353424524048, 7.497281471361842087, 0.000000000000000000 ) ) ;
#105999 = AXIS2_PLACEMENT_3D ( 'NONE', #27383, #60263, #86129 ) ;
#106000 = CARTESIAN_POINT ( 'NONE',  ( 6.928203230275510549, -10.00000000000000888, 4.000000000000000000 ) ) ;
#106001 = CARTESIAN_POINT ( 'NONE',  ( -42.63514723966559927, 485.0526260718492040, -1.920325882447441179 ) ) ;
#106002 = ORIENTED_EDGE ( 'NONE', *, *, #91724, .T. ) ;
#106003 =( NAMED_UNIT ( * ) SI_UNIT ( $, .STERADIAN. ) SOLID_ANGLE_UNIT ( ) );
#106004 = CARTESIAN_POINT ( 'NONE',  ( 0.06682554136337624795, 4.993536075455413226, -4.350941807883113022 ) ) ;
#106005 = AXIS2_PLACEMENT_3D ( 'NONE', #84264, #27669, #43275 ) ;
#106006 = DIRECTION ( 'NONE',  ( 1.000000000000000000, 1.224606353822377258E-16, 0.000000000000000000 ) ) ;
#106007 = CARTESIAN_POINT ( 'NONE',  ( -98.17474337771899684, -29.99999999999999645, 190.3296048190805152 ) ) ;
#106008 = EDGE_CURVE ( 'NONE', #45973, #9203, #82250, .T. ) ;
#106009 = CARTESIAN_POINT ( 'NONE',  ( -46.00000000000000000, 500.0000000000002274, -15.00000000000000711 ) ) ;
#106010 = CARTESIAN_POINT ( 'NONE',  ( 53.89377858532357379, -57.67595397426320147, 88.10897076158549623 ) ) ;
#106012 = CARTESIAN_POINT ( 'NONE',  ( -9.806140579452332418, 53.43725138183724255, 2.590315439319800461 ) ) ;
#106011 = DIRECTION ( 'NONE',  ( -1.000000000000000000, 0.000000000000000000, 0.000000000000000000 ) ) ;
#106013 = ADVANCED_FACE ( 'NONE', ( #47549 ), #36518, .T. ) ;
#106014 = CARTESIAN_POINT ( 'NONE',  ( 22.63357787059576864, -26.81694554740444048, -38.43512209275669278 ) ) ;
#106015 = CARTESIAN_POINT ( 'NONE',  ( -7.500000000000000000, -2.571118828324945760, -0.3627527587569074896 ) ) ;
#106016 = CARTESIAN_POINT ( 'NONE',  ( -16.88293466221169581, -60.00000000000001421, 39.91355644712231765 ) ) ;
#106017 = SURFACE_STYLE_FILL_AREA ( #88797 ) ;
#106018 = CARTESIAN_POINT ( 'NONE',  ( 6.517579295440401488, 53.49311649283862380, 7.569470789138253330 ) ) ;
#106019 = CARTESIAN_POINT ( 'NONE',  ( -86.84244699270934120, -46.46287268932884018, 190.7113349457623883 ) ) ;
#106020 = ORIENTED_EDGE ( 'NONE', *, *, #3686, .T. ) ;
#106021 = CARTESIAN_POINT ( 'NONE',  ( 17.49999999999435119, 50.00908096117762369, 61.65219700478674270 ) ) ;
#106022 = CARTESIAN_POINT ( 'NONE',  ( 81.84444444444444855, -4.171999999999998820, 5.616230220889773285E-16 ) ) ;
#106023 = CARTESIAN_POINT ( 'NONE',  ( -5.173845848792242741, -60.36574285059159450, 33.93991560295228282 ) ) ;
#106024 = CIRCLE ( 'NONE', #23390, 1.000000000000002665 ) ;
#106025 = DIRECTION ( 'NONE',  ( -1.000000000000000000, -0.000000000000000000, -0.000000000000000000 ) ) ;
#106027 =( NAMED_UNIT ( * ) PLANE_ANGLE_UNIT ( ) SI_UNIT ( $, .RADIAN. ) );
#106026 = CARTESIAN_POINT ( 'NONE',  ( 1.098735407078442972, -7.248058225758801321, -6.326622577870249842 ) ) ;
#106028 = VERTEX_POINT ( 'NONE', #7092 ) ;
#106029 = CARTESIAN_POINT ( 'NONE',  ( 5.129365358145452802, 41.91296950070222493, -69.99827769498368468 ) ) ;
#106030 = CARTESIAN_POINT ( 'NONE',  ( -7.253185102483167945, -3.609892095628724373, -18.04361009490900614 ) ) ;
#106031 = CARTESIAN_POINT ( 'NONE',  ( -29.87444201908918728, 8.057352084660356795, -42.09618695302987845 ) ) ;
#106032 = CARTESIAN_POINT ( 'NONE',  ( 32.44539866313899523, 299.6034349815453766, -0.9399606259422752519 ) ) ;
#106033 = CARTESIAN_POINT ( 'NONE',  ( 0.000000000000000000, 0.000000000000000000, 0.000000000000000000 ) ) ;
#106034 = CARTESIAN_POINT ( 'NONE',  ( -7.212994264445060644, -82.98288655659962387, 3.463766307298588032 ) ) ;
#106035 = CARTESIAN_POINT ( 'NONE',  ( 61.54478197300144160, -59.99999999999999289, 105.7065446260163526 ) ) ;
#106036 = CARTESIAN_POINT ( 'NONE',  ( -34.72474116627837759, 338.3618661353910966, -1.881472242819908436 ) ) ;
#106037 = EDGE_LOOP ( 'NONE', ( #19386, #38448, #30081, #34865, #41267 ) ) ;
#106038 = CARTESIAN_POINT ( 'NONE',  ( -42.51801476543344194, 435.0274750839319609, 8.236762145195060114 ) ) ;
#106039 = CARTESIAN_POINT ( 'NONE',  ( -9.948181520647874976, 253.8689280276036868, 1.049088206181511662 ) ) ;
#106041 = CARTESIAN_POINT ( 'NONE',  ( -33.11369981515483119, 485.0096198691158520, 0.6282636062397999321 ) ) ;
#106040 = CARTESIAN_POINT ( 'NONE',  ( 36.05900422978820075, -60.00000000000002132, 50.77828662454974307 ) ) ;
#106042 =( LENGTH_UNIT ( ) NAMED_UNIT ( * ) SI_UNIT ( .MILLI., .METRE. ) );
#106043 = CARTESIAN_POINT ( 'NONE',  ( -5.000000000093224095, -3.772466818847465042, 103.2791840072271015 ) ) ;
#106044 = ORIENTED_EDGE ( 'NONE', *, *, #61304, .F. ) ;
#106045 = CIRCLE ( 'NONE', #69964, 5.000000000000001776 ) ;
#106046 = CARTESIAN_POINT ( 'NONE',  ( -25.03733421107493129, 305.9738044749904589, 10.41262473261235044 ) ) ;
#106047 = ORIENTED_EDGE ( 'NONE', *, *, #41000, .T. ) ;
#106048 = CARTESIAN_POINT ( 'NONE',  ( 37.21746376929104372, 485.5895280773364675, -4.183112156774711821 ) ) ;
#106049 = CARTESIAN_POINT ( 'NONE',  ( 31.03678703375144821, 438.6650838204807314, 21.86890379897223013 ) ) ;
#106050 = CARTESIAN_POINT ( 'NONE',  ( -33.00000000000000000, 435.0774731480752848, 11.67986145722080948 ) ) ;
#106051 = ORIENTED_EDGE ( 'NONE', *, *, #45419, .F. ) ;
#106052 = EDGE_CURVE ( 'NONE', #96657, #29420, #57158, .T. ) ;
#106053 = CARTESIAN_POINT ( 'NONE',  ( 65.26738680894031575, 49.99999999999999289, 0.8120011905333047730 ) ) ;
#106054 = CARTESIAN_POINT ( 'NONE',  ( -36.75617418030669370, -59.99999999999754152, 51.65163013687570981 ) ) ;
#106055 = DIRECTION ( 'NONE',  ( -1.000000000000000000, -1.224606353822377258E-16, -0.000000000000000000 ) ) ;
#106056 = CARTESIAN_POINT ( 'NONE',  ( 89.54885025292163903, -60.00000000000002132, 201.8582137258730143 ) ) ;
#106057 = CARTESIAN_POINT ( 'NONE',  ( 16.08349330513380337, 1.593028355512270567E-15, 0.000000000000000000 ) ) ;
#106058 = MECHANICAL_DESIGN_GEOMETRIC_PRESENTATION_REPRESENTATION (  '', ( #35449 ), #100919 ) ;
#106060 = CARTESIAN_POINT ( 'NONE',  ( 17.02384506383146245, -53.39628896086755816, 33.04942014297441943 ) ) ;
#106059 = CARTESIAN_POINT ( 'NONE',  ( -108.2763249159406769, -59.99999999999986500, 199.3718883026843116 ) ) ;
#106062 = CARTESIAN_POINT ( 'NONE',  ( 100.9474370845066176, -38.00000000000000711, 146.8126285005432408 ) ) ;
#106061 = PRODUCT_DEFINITION_CONTEXT ( 'detailed design', #74819, 'design' ) ;
#106063 = CARTESIAN_POINT ( 'NONE',  ( 1.249203303865451753, 53.88099106177547526, -8.834200927035483986 ) ) ;
#106064 = EDGE_CURVE ( 'NONE', #91520, #44907, #96651, .T. ) ;
#106065 = CARTESIAN_POINT ( 'NONE',  ( -43.92060318859008561, -39.52985988317308141, 42.42323198190868538 ) ) ;
#106066 = CARTESIAN_POINT ( 'NONE',  ( 2.985641311035224431E-22, 35.08181111624585213, -27.25000000000000000 ) ) ;
#106067 = AXIS2_PLACEMENT_3D ( 'NONE', #31048, #32088, #80078 ) ;
#106068 = VERTEX_POINT ( 'NONE', #82036 ) ;
#106069 = AXIS2_PLACEMENT_3D ( 'NONE', #45474, #13601, #96139 ) ;
#106070 = CARTESIAN_POINT ( 'NONE',  ( -13.00000000000003730, -10.00000000000000888, 4.000000000000000000 ) ) ;
#106071 = CARTESIAN_POINT ( 'NONE',  ( 0.000000000000000000, 5.629165124598847214, -3.250000000000007550 ) ) ;
#106072 = CIRCLE ( 'NONE', #26907, 5.000000000000001776 ) ;
#106073 = CARTESIAN_POINT ( 'NONE',  ( 4.521127550501230274, -9.323897594723373317, 3.944701057164355706 ) ) ;
#106074 = CYLINDRICAL_SURFACE ( 'NONE', #64176, 6.000000000000000888 ) ;
#106075 = VERTEX_POINT ( 'NONE', #88560 ) ;
#106076 = CARTESIAN_POINT ( 'NONE',  ( 5.833333333333327708, -46.00000000000000000, 103.8776713793258608 ) ) ;
#106077 = ORIENTED_EDGE ( 'NONE', *, *, #82333, .F. ) ;
#106078 = CARTESIAN_POINT ( 'NONE',  ( 92.35295832812823846, -30.00000000007834089, 199.7455495689326312 ) ) ;
#106079 = CARTESIAN_POINT ( 'NONE',  ( 22.96637035739885135, 41.68994590335805839, -75.70120662748654183 ) ) ;
#106081 = EDGE_CURVE ( 'NONE', #85790, #1493, #2033, .T. ) ;
#106080 = CARTESIAN_POINT ( 'NONE',  ( 5.420470438621152631, 41.88321586334136981, -59.04137885805278785 ) ) ;
#106082 = CIRCLE ( 'NONE', #81981, 4.000000000000001776 ) ;
#106083 = DIRECTION ( 'NONE',  ( 1.000000000000000000, 1.224606353822377258E-16, 0.000000000000000000 ) ) ;
#106084 = CARTESIAN_POINT ( 'NONE',  ( 97.43685538820150782, -30.00000000000000000, 133.5638869304015088 ) ) ;
#106085 = CARTESIAN_POINT ( 'NONE',  ( 7.619701877737480977, 101.8255784046723562, -2.447562251315980486 ) ) ;
#106086 = EDGE_LOOP ( 'NONE', ( #64329, #12665, #63886, #75187, #105651, #68941 ) ) ;
#106087 = ORIENTED_EDGE ( 'NONE', *, *, #72083, .T. ) ;
#106088 = ORIENTED_EDGE ( 'NONE', *, *, #19066, .F. ) ;
#106089 = CIRCLE ( 'NONE', #18285, 2.000000000000000444 ) ;
#106090 = CARTESIAN_POINT ( 'NONE',  ( 0.000000000000000000, 0.000000000000000000, 0.000000000000000000 ) ) ;
#106091 = CARTESIAN_POINT ( 'NONE',  ( -6.697922209380616110, -13.04455172910126137, -7.429582257095876052 ) ) ;
#106092 = CARTESIAN_POINT ( 'NONE',  ( 0.000000000000000000, 0.000000000000000000, 0.000000000000000000 ) ) ;
#106093 = ORIENTED_EDGE ( 'NONE', *, *, #62908, .F. ) ;
#106094 = CARTESIAN_POINT ( 'NONE',  ( 42.99999999999998579, 436.5989882784185738, 19.94133085611157341 ) ) ;
#106095 = ORIENTED_EDGE ( 'NONE', *, *, #58791, .F. ) ;
#106096 = CARTESIAN_POINT ( 'NONE',  ( -1.469576158976823947E-15, -17.56250000409676915, 8.000000000000000000 ) ) ;
#106097 = CARTESIAN_POINT ( 'NONE',  ( 85.26653421436701308, -38.68462227007306353, 198.6437487644617761 ) ) ;
#106098 = CARTESIAN_POINT ( 'NONE',  ( 13.67695886415361350, 5.027398151725734010, 6.085592534666677267 ) ) ;
#106100 = CARTESIAN_POINT ( 'NONE',  ( 86.49569524121002928, -38.00000000000003553, 187.7518329194348894 ) ) ;
#106099 = B_SPLINE_CURVE_WITH_KNOTS ( 'NONE', 3,
 ( #36336, #2305, #44386, #99952, #84310, #19625, #10405, #59513, #2845, #52458, #69205, #35797, #68121, #75673, #34732, #102074, #101556, #28235, #27712, #85375, #101017, #67603 ),
 .UNSPECIFIED., .F., .F.,
 ( 4, 2, 2, 2, 2, 2, 2, 2, 2, 2, 4 ),
 ( 5.553824967135426632E-18, 0.001048074399358199906, 0.002096148798716394174, 0.003144223198074588659, 0.004192297597432782276, 0.005240371996790976761, 0.005764409196470074437, 0.006288446396149171246, 0.006812483595828268054, 0.007336520795507365730, 0.008384595194865552409 ),
 .UNSPECIFIED. ) ;
#106101 = CARTESIAN_POINT ( 'NONE',  ( 29.07017008048624618, 312.2030387978562089, 12.19116356018488823 ) ) ;
#106102 = DIRECTION ( 'NONE',  ( 1.224646799147349509E-16, 0.000000000000000000, -1.000000000000000000 ) ) ;
#106103 = LINE ( 'NONE', #72687, #7965 ) ;
#106104 = AXIS2_PLACEMENT_3D ( 'NONE', #71317, #62716, #54583 ) ;
#106105 = CARTESIAN_POINT ( 'NONE',  ( -27.71720361241088426, 34.52917361415862985, -7.705544253522235820 ) ) ;
#106106 = CARTESIAN_POINT ( 'NONE',  ( -4.750186375024242125, -48.62189236691707350, 104.3180500829685258 ) ) ;
#106107 = PRESENTATION_STYLE_ASSIGNMENT (( #23641 ) ) ;
#106108 = EDGE_CURVE ( 'NONE', #40649, #35868, #74329, .T. ) ;
#106109 = ORIENTED_EDGE ( 'NONE', *, *, #91161, .T. ) ;
#106110 = CARTESIAN_POINT ( 'NONE',  ( -43.50377727019363761, 435.9167426301696651, 18.24083946424744340 ) ) ;
#106111 = CARTESIAN_POINT ( 'NONE',  ( -24.36065331428383374, 304.1491164910331122, 10.22124288038939710 ) ) ;
#106112 = DIRECTION ( 'NONE',  ( 0.000000000000000000, 0.000000000000000000, -1.000000000000000000 ) ) ;
#106113 = CARTESIAN_POINT ( 'NONE',  ( 21.08349330513380693, 4.000000000000003553, 0.000000000000000000 ) ) ;
#106114 = CARTESIAN_POINT ( 'NONE',  ( -5.656854249492381470, -17.56249999999999645, 5.656854249492379694 ) ) ;
#106115 = FACE_OUTER_BOUND ( 'NONE', #76567, .T. ) ;
#106116 = EDGE_CURVE ( 'NONE', #34913, #45114, #31930, .T. ) ;
#106117 = EDGE_CURVE ( 'NONE', #54340, #38992, #72639, .T. ) ;
#106118 = CARTESIAN_POINT ( 'NONE',  ( -7.896254658894421574, 101.2107081724580127, 1.307282859663298602 ) ) ;
#106119 = CARTESIAN_POINT ( 'NONE',  ( 18.18910696884454126, 303.6388988518723977, 9.891725748637984594 ) ) ;
#106120 = ORIENTED_EDGE ( 'NONE', *, *, #57156, .F. ) ;
#106121 = CARTESIAN_POINT ( 'NONE',  ( 83.75659386667784645, -61.01700501349375116, 191.9530215260792829 ) ) ;
#106122 = CARTESIAN_POINT ( 'NONE',  ( 2.470381878726035567E-14, 18.87382441218300144, 49.24999999999992184 ) ) ;
#106123 = VECTOR ( 'NONE', #37058, 1000.000000000000000 ) ;
#106124 = CARTESIAN_POINT ( 'NONE',  ( -9.514607630182533526, 142.5277189163442415, -2.884741510313297714E-12 ) ) ;
#106125 = ORIENTED_EDGE ( 'NONE', *, *, #98081, .F. ) ;
#106126 = CARTESIAN_POINT ( 'NONE',  ( 83.06228876499081082, -57.67107222564732893, -28.36318629505660738 ) ) ;
#106127 = CARTESIAN_POINT ( 'NONE',  ( 36.50546997061839249, 437.5879066196142162, 4.249723241246290861 ) ) ;
#106128 = SURFACE_STYLE_USAGE ( .BOTH. , #23666 ) ;
#106129 = CARTESIAN_POINT ( 'NONE',  ( -81.36319491956838590, -30.00000000000000711, -1.421388179323267220 ) ) ;
#106130 = ADVANCED_FACE ( 'NONE', ( #6555 ), #90683, .T. ) ;
#106131 = CARTESIAN_POINT ( 'NONE',  ( 28.54518584606585563, 18.48129625438336276, 40.33591358207591071 ) ) ;
#106132 = CARTESIAN_POINT ( 'NONE',  ( 8.000000000000000000, -3.000000000000000000, 2.094395098902537722 ) ) ;
#106133 = DIRECTION ( 'NONE',  ( 1.000000000000000000, 0.000000000000000000, 0.000000000000000000 ) ) ;
#106134 = CARTESIAN_POINT ( 'NONE',  ( 33.58349330513380693, -4.000000000000000000, 4.898587196589415787E-16 ) ) ;
#106135 = CARTESIAN_POINT ( 'NONE',  ( 0.000000000000000000, 0.000000000000000000, 0.000000000000000000 ) ) ;
#106136 = DIRECTION ( 'NONE',  ( 0.8191520442889924647, 0.000000000000000000, 0.5735764363510451602 ) ) ;
#106137 = VECTOR ( 'NONE', #16494, 1000.000000000000000 ) ;
#106138 = DIRECTION ( 'NONE',  ( -1.000000000000000000, -0.000000000000000000, -0.000000000000000000 ) ) ;
#106139 = AXIS2_PLACEMENT_3D ( 'NONE', #98279, #31974, #31456 ) ;
#106140 = CARTESIAN_POINT ( 'NONE',  ( -7.000000000000000000, 8.572527594031471218E-16, -3.024963890361733743 ) ) ;
#106141 = CARTESIAN_POINT ( 'NONE',  ( -1.000000000000000666, 0.000000000000000000, 42.58845726811989607 ) ) ;
#106142 = DIRECTION ( 'NONE',  ( 0.000000000000000000, -1.000000000000000000, 0.000000000000000000 ) ) ;
#106143 = MECHANICAL_DESIGN_GEOMETRIC_PRESENTATION_REPRESENTATION (  '', ( #75114 ), #73417 ) ;
#106144 = CONICAL_SURFACE ( 'NONE', #64818, 4.000000000000000000, 0.9599310885968912466 ) ;
#106145 = EDGE_CURVE ( 'NONE', #30348, #95128, #79578, .T. ) ;
#106146 = CARTESIAN_POINT ( 'NONE',  ( 33.86867596911348954, 484.1347864990123639, 1.565332731468491945 ) ) ;
#106147 = EDGE_LOOP ( 'NONE', ( #16956, #49453, #68685, #54108 ) ) ;
#106148 = DIRECTION ( 'NONE',  ( 0.000000000000000000, -1.000000000000000000, 0.000000000000000000 ) ) ;
#106149 = DIRECTION ( 'NONE',  ( 0.000000000000000000, 0.000000000000000000, 1.000000000000000000 ) ) ;
#106150 = AXIS2_PLACEMENT_3D ( 'NONE', #9854, #42766, #60573 ) ;
#106151 = CARTESIAN_POINT ( 'NONE',  ( -17.87520619753193429, -17.95932086966949015, -34.00109537085095468 ) ) ;
#106153 = CARTESIAN_POINT ( 'NONE',  ( -25.91394795060947942, -60.22836619208757014, -35.60171098623400354 ) ) ;
#106152 = CARTESIAN_POINT ( 'NONE',  ( 17.33349330513380337, 4.000000000000002665, 0.000000000000000000 ) ) ;
#106154 = VERTEX_POINT ( 'NONE', #17871 ) ;
#106155 = CONICAL_SURFACE ( 'NONE', #102725, 8.000000000000000000, 1.047197551196600296 ) ;
#106156 = ORIENTED_EDGE ( 'NONE', *, *, #74880, .F. ) ;
#106157 = CARTESIAN_POINT ( 'NONE',  ( 33.84761347220318584, 488.7471039746334895, 11.01988148152525504 ) ) ;
#106158 = CARTESIAN_POINT ( 'NONE',  ( 0.000000000000000000, 0.000000000000000000, 0.000000000000000000 ) ) ;
#106159 = CARTESIAN_POINT ( 'NONE',  ( -66.81167781205434153, -60.00000000000000711, -33.62895559939038037 ) ) ;
#106160 = VERTEX_POINT ( 'NONE', #58308 ) ;
#106161 = CARTESIAN_POINT ( 'NONE',  ( 25.47402648759802446, -28.38081445280734982, -30.30612721234350815 ) ) ;
#106162 = CARTESIAN_POINT ( 'NONE',  ( 68.70539558375507738, 6.856755485862130937E-15, 0.000000000000000000 ) ) ;
#106163 = CARTESIAN_POINT ( 'NONE',  ( 98.11478003982226426, -60.34325407385573214, 196.5388644659511783 ) ) ;
#106165 = CARTESIAN_POINT ( 'NONE',  ( -47.36504548439823736, 12.99580092579919999, 14.54285468146515470 ) ) ;
#106164 = SURFACE_STYLE_USAGE ( .BOTH. , #57611 ) ;
#106166 = CIRCLE ( 'NONE', #30391, 4.000000000000001776 ) ;
#106167 = CARTESIAN_POINT ( 'NONE',  ( -81.52096736789169995, -42.97176952543888717, 161.5648495392605923 ) ) ;
#106168 = ORIENTED_EDGE ( 'NONE', *, *, #14782, .T. ) ;
#106169 = VERTEX_POINT ( 'NONE', #25455 ) ;
#106170 = ORIENTED_EDGE ( 'NONE', *, *, #5294, .F. ) ;
#106171 = CARTESIAN_POINT ( 'NONE',  ( 29.96324721583764727, 332.4108250884644349, 16.64494553332287907 ) ) ;
#106172 = CARTESIAN_POINT ( 'NONE',  ( -5.000000000000039968, -14.19087030044497943, 13.37859801193910769 ) ) ;
#106173 = ORIENTED_EDGE ( 'NONE', *, *, #93847, .T. ) ;
#106174 = EDGE_CURVE ( 'NONE', #29960, #90588, #42119, .T. ) ;
#106175 = DIRECTION ( 'NONE',  ( -0.000000000000000000, -1.000000000000000000, 0.000000000000000000 ) ) ;
#106176 = CARTESIAN_POINT ( 'NONE',  ( 18.09999999999999787, 1.533819458162526451E-15, 0.000000000000000000 ) ) ;
#106177 = CARTESIAN_POINT ( 'NONE',  ( -111.5786317092108533, -57.67087409935591324, 192.6842770035980834 ) ) ;
#106178 = CARTESIAN_POINT ( 'NONE',  ( -1.320432766682874540E-15, -31.53125000204838457, 7.188101187500000044 ) ) ;
#106179 = CARTESIAN_POINT ( 'NONE',  ( -59.99387666504471639, 48.00000000000000711, 25.54086645653091026 ) ) ;
#106180 = CARTESIAN_POINT ( 'NONE',  ( 6.231493956936422940, 4.173545622688802581, 0.000000000000000000 ) ) ;
#106181 = DIRECTION ( 'NONE',  ( 0.9488877907218276064, 0.1950364375161156294, -0.2481385674579254796 ) ) ;
#106182 = CARTESIAN_POINT ( 'NONE',  ( 8.309465130445103043, -30.00000000000003197, -39.88086614825118659 ) ) ;
#106183 = EDGE_CURVE ( 'NONE', #65536, #34458, #5092, .T. ) ;
#106184 = CARTESIAN_POINT ( 'NONE',  ( -4.155049527179308200, -30.00000000000002842, 36.99135516471767460 ) ) ;
#106185 = EDGE_CURVE ( 'NONE', #92197, #32538, #96760, .T. ) ;
#106186 = CARTESIAN_POINT ( 'NONE',  ( -53.18781749681305371, -56.84782064553103709, 63.26121515912522142 ) ) ;
#106187 = DIRECTION ( 'NONE',  ( -1.000000000000000000, -1.224606353822377258E-16, -0.000000000000000000 ) ) ;
#106188 = ORIENTED_EDGE ( 'NONE', *, *, #14725, .T. ) ;
#106189 = CARTESIAN_POINT ( 'NONE',  ( -97.18938212093779327, -37.69980210926051001, 192.7882013891335191 ) ) ;
#106190 = STYLED_ITEM ( 'NONE', ( #88129 ), #6831 ) ;
#106191 = CARTESIAN_POINT ( 'NONE',  ( -0.5082004254278419397, 295.8543628274115918, -10.00017741440582242 ) ) ;
#106192 = EDGE_LOOP ( 'NONE', ( #65986, #88949, #41253, #67096, #67101 ) ) ;
#106193 = DIRECTION ( 'NONE',  ( -1.000000000000000000, 0.000000000000000000, 0.000000000000000000 ) ) ;
#106194 = CARTESIAN_POINT ( 'NONE',  ( 91.24927989895878966, -38.36004604005931640, -1.395253234482411786 ) ) ;
#106195 = LINE ( 'NONE', #16139, #14051 ) ;
#106196 = CARTESIAN_POINT ( 'NONE',  ( 0.000000000000000000, -5.000000000000000000, 10.00000000000000000 ) ) ;
#106198 = EDGE_CURVE ( 'NONE', #77127, #231, #29651, .T. ) ;
#106197 = CARTESIAN_POINT ( 'NONE',  ( -10.24592498679531261, 302.6397288294038503, 9.891918830032325971 ) ) ;
#106199 = CARTESIAN_POINT ( 'NONE',  ( -34.92499999999994742, 0.000000000000000000, 0.000000000000000000 ) ) ;
#106200 = CARTESIAN_POINT ( 'NONE',  ( 83.93844488845637386, -29.99999999999999645, 160.4690723128815932 ) ) ;
#106201 = CARTESIAN_POINT ( 'NONE',  ( 0.7145311798163210826, 4.618802153517001408, -8.000000000000000000 ) ) ;
#106202 = CARTESIAN_POINT ( 'NONE',  ( -28.98676785243937815, 9.652684557211548722, 41.90074509620628618 ) ) ;
#106203 = DIRECTION ( 'NONE',  ( 0.000000000000000000, -1.000000000000000000, 0.000000000000000000 ) ) ;
#106204 = VERTEX_POINT ( 'NONE', #68001 ) ;
#106205 = VERTEX_POINT ( 'NONE', #1649 ) ;
#106206 = CARTESIAN_POINT ( 'NONE',  ( 49.59389593497978410, -22.20511380567462112, 44.49589264220691831 ) ) ;
#106207 = VECTOR ( 'NONE', #27026, 1000.000000000000000 ) ;
#106208 = CARTESIAN_POINT ( 'NONE',  ( -3.010552705096329440, 299.5657579542672693, -10.00571845265126214 ) ) ;
#106209 = AXIS2_PLACEMENT_3D ( 'NONE', #87631, #37519, #36464 ) ;
#106210 = CARTESIAN_POINT ( 'NONE',  ( 37.56673239365841255, 27.88554838446202311, -10.95617127781092037 ) ) ;
#106211 = ORIENTED_EDGE ( 'NONE', *, *, #100436, .F. ) ;
#106212 = CARTESIAN_POINT ( 'NONE',  ( -98.34829155932973777, -38.35547239742750492, 78.70912769862152913 ) ) ;
#106213 = EDGE_LOOP ( 'NONE', ( #2069, #65927, #45202, #63742 ) ) ;
#106214 = CARTESIAN_POINT ( 'NONE',  ( 20.59999999999999787, -3.309499999999999886, 4.475777889183790779E-16 ) ) ;
#106215 = CARTESIAN_POINT ( 'NONE',  ( 110.3578795809912094, -38.35604999599375020, 158.7521924589690627 ) ) ;
#106216 = CARTESIAN_POINT ( 'NONE',  ( 13.16427862254860770, 19.50489605903024426, -7.599932435955482291 ) ) ;
#106217 = CARTESIAN_POINT ( 'NONE',  ( -37.48682946491119594, 25.78511199397625830, -10.95617127781024180 ) ) ;
#106219 = CARTESIAN_POINT ( 'NONE',  ( 101.8269878747205723, -52.71687279565823303, 134.8528526430313832 ) ) ;
#106218 = TOROIDAL_SURFACE ( 'NONE', #56242, 12.00000000000001066, 3.000000000000000000 ) ;
#106220 = AXIS2_PLACEMENT_3D ( 'NONE', #44096, #42486, #76982 ) ;
#106221 = CARTESIAN_POINT ( 'NONE',  ( -31.84138247899937468, 438.9968886095898029, 23.56020719208648373 ) ) ;
#106222 = CARTESIAN_POINT ( 'NONE',  ( 21.97121321732691257, 28.05118154993452961, 31.83013537814891691 ) ) ;
#106224 = AXIS2_PLACEMENT_3D ( 'NONE', #94283, #86211, #87259 ) ;
#106223 = CARTESIAN_POINT ( 'NONE',  ( -32.66601306147397565, 321.4771002738425523, -4.939848896245494281 ) ) ;
#106225 = CARTESIAN_POINT ( 'NONE',  ( 8.000000000000000000, 9.797174393178825657E-16, -0.02540000000000007530 ) ) ;
#106226 = CARTESIAN_POINT ( 'NONE',  ( 75.46095339194756946, -60.00000000000001421, 184.2592822936660184 ) ) ;
#106227 = VECTOR ( 'NONE', #7353, 1000.000000000000000 ) ;
#106228 = CIRCLE ( 'NONE', #90784, 4.000000000000001776 ) ;
#106229 = CARTESIAN_POINT ( 'NONE',  ( 17.53291882538153601, 45.00000000000002132, 63.43016343176445559 ) ) ;
#106230 = EDGE_LOOP ( 'NONE', ( #26012, #72521, #15919, #68535, #22908, #77968, #29495 ) ) ;
#106231 = CARTESIAN_POINT ( 'NONE',  ( 55.73253904170881157, -29.08777573428741547, 57.64467041135599601 ) ) ;
#106232 = CARTESIAN_POINT ( 'NONE',  ( -23.92380886547979557, 303.5731447498800435, -9.844749896117946264 ) ) ;
#106233 = DIRECTION ( 'NONE',  ( -0.000000000000000000, -1.000000000000000000, -0.000000000000000000 ) ) ;
#106234 = CARTESIAN_POINT ( 'NONE',  ( 0.000000000000000000, -2.000000000000000000, 10.00000000000000000 ) ) ;
#106235 = ORIENTED_EDGE ( 'NONE', *, *, #64471, .F. ) ;
#106237 = CARTESIAN_POINT ( 'NONE',  ( -9.171168021175072127, -52.95225154708963800, 30.98659277684255997 ) ) ;
#106236 = CARTESIAN_POINT ( 'NONE',  ( -79.13986484937814225, -29.99999999996501998, 187.8162035005837254 ) ) ;
#106238 = CARTESIAN_POINT ( 'NONE',  ( 4.028951842967195773, -3.000000000000000444, -6.990291106834061630 ) ) ;
#106239 = CARTESIAN_POINT ( 'NONE',  ( 22.56511519009970002, 305.4508729011461128, 9.066418547683744222 ) ) ;
#106240 = CARTESIAN_POINT ( 'NONE',  ( 26.11923076923076792, 1.411358822780289120E-15, 0.000000000000000000 ) ) ;
#106241 = CARTESIAN_POINT ( 'NONE',  ( 3.313708498984762052, -34.71875000000000000, -8.000000000000000000 ) ) ;
#106242 = FACE_OUTER_BOUND ( 'NONE', #2302, .T. ) ;
#106243 = EDGE_CURVE ( 'NONE', #7878, #95368, #83635, .T. ) ;
#106244 = B_SPLINE_CURVE_WITH_KNOTS ( 'NONE', 3,
 ( #26703, #18056, #84373, #83297, #34790, #51986, #43382, #34254, #101077, #66587, #50914, #35318, #26179, #18598, #99467, #57946, #27237, #98930, #83824, #68182, #43906, #100539 ),
 .UNSPECIFIED., .F., .F.,
 ( 4, 2, 2, 2, 2, 2, 2, 2, 2, 2, 4 ),
 ( 0.003049572450201245167, 0.003553926186014261940, 0.003806103053920776615, 0.004058279921827292157, 0.004562633657640314568, 0.005066987393453339580, 0.005571341129266364593, 0.006075694865079388739, 0.006580048600892413752, 0.006832225468798924090, 0.007084402336705432693 ),
 .UNSPECIFIED. ) ;
#106245 = CARTESIAN_POINT ( 'NONE',  ( 63.27102371193946340, 48.00000000000000711, 15.76003347376319574 ) ) ;
#106246 = ORIENTED_EDGE ( 'NONE', *, *, #76130, .F. ) ;
#106247 = CARTESIAN_POINT ( 'NONE',  ( 85.70055246076826450, -21.88621194787217306, 168.6156743441144954 ) ) ;
#106249 = CIRCLE ( 'NONE', #28792, 8.000000000000000000 ) ;
#106248 = CARTESIAN_POINT ( 'NONE',  ( 5.596957125887387363, -47.31575451833740686, 103.9718581041641698 ) ) ;
#106250 = CARTESIAN_POINT ( 'NONE',  ( 33.47652930794067316, 484.3276552595487487, 3.198545968220822378 ) ) ;
#106251 = ORIENTED_EDGE ( 'NONE', *, *, #47123, .F. ) ;
#106252 = CARTESIAN_POINT ( 'NONE',  ( 106.4000000000000057, 0.000000000000000000, 0.000000000000000000 ) ) ;
#106253 = CARTESIAN_POINT ( 'NONE',  ( 4.649486852896263400, -4.999999999999983125, -15.66810684149982258 ) ) ;
#106254 = CARTESIAN_POINT ( 'NONE',  ( 26.94627380994484156, 34.81398319875323466, -7.556984339686200869 ) ) ;
#106255 = CARTESIAN_POINT ( 'NONE',  ( 1.469576158976823356E-15, 50.00000000000000000, -73.00000000000001421 ) ) ;
#106256 = CARTESIAN_POINT ( 'NONE',  ( -43.51845134567530238, 41.44193902626327031, -50.67202077435701568 ) ) ;
#106257 = AXIS2_PLACEMENT_3D ( 'NONE', #103461, #38227, #62482 ) ;
#106258 = DIRECTION ( 'NONE',  ( -1.000000000000000000, -1.224606353822377258E-16, -0.000000000000000000 ) ) ;
#106259 = EDGE_CURVE ( 'NONE', #45933, #99558, #238, .T. ) ;
#106260 = SURFACE_STYLE_FILL_AREA ( #48560 ) ;
#106261 = CARTESIAN_POINT ( 'NONE',  ( 6.499999999999999112, 3.402385889607431046, -5.998095356498420294 ) ) ;
#106262 = CARTESIAN_POINT ( 'NONE',  ( -4.382959417677086300, -48.13794921561773776, 102.7400018439556533 ) ) ;
#106264 = CARTESIAN_POINT ( 'NONE',  ( -11.43824633007028702, 13.06272204673569703, -10.01661281870972786 ) ) ;
#106263 = CARTESIAN_POINT ( 'NONE',  ( -5.931024892954755323, -18.81772794593000953, 35.12675206171071807 ) ) ;
#106265 = CARTESIAN_POINT ( 'NONE',  ( -5.082755093536325042, -12.59375000204838280, -5.082755093536325930 ) ) ;
#106266 = CARTESIAN_POINT ( 'NONE',  ( -29.68315524077005207, 18.29184282782459547, -39.60535821593474282 ) ) ;
#106267 = ADVANCED_FACE ( 'NONE', ( #18962 ), #81249, .F. ) ;
#106268 = EDGE_CURVE ( 'NONE', #63495, #63262, #58951, .T. ) ;
#106269 = PRESENTATION_LAYER_ASSIGNMENT (  '', '', ( #39178 ) ) ;
#106270 = ORIENTED_EDGE ( 'NONE', *, *, #60688, .T. ) ;
#106271 = CARTESIAN_POINT ( 'NONE',  ( -17.49999999999997868, 50.03360497985113398, 63.82236279035413418 ) ) ;
#106272 = CARTESIAN_POINT ( 'NONE',  ( 24.41529588775463111, 25.25633621354825564, 32.32316270052714913 ) ) ;
#106273 = CARTESIAN_POINT ( 'NONE',  ( -2.844395363893353235, 79.54923207833792276, -5.000000000000000000 ) ) ;
#106274 = CARTESIAN_POINT ( 'NONE',  ( -43.00000000000000000, 488.0336798547363628, -0.8984331811837273918 ) ) ;
#106275 = CARTESIAN_POINT ( 'NONE',  ( 2.499999999999970690, -27.33278124259516773, -31.42875788144166549 ) ) ;
#106276 = ORIENTED_EDGE ( 'NONE', *, *, #73541, .T. ) ;
#106277 = CARTESIAN_POINT ( 'NONE',  ( -4.590682673078522846, -86.06791757312156221, 3.864023243754608483 ) ) ;
#106278 = DIRECTION ( 'NONE',  ( 0.000000000000000000, 0.000000000000000000, 1.000000000000000000 ) ) ;
#106279 = AXIS2_PLACEMENT_3D ( 'NONE', #64660, #97536, #23697 ) ;
#106280 = VERTEX_POINT ( 'NONE', #26522 ) ;
#106281 = PLANE ( 'NONE',  #12323 ) ;
#106282 = CARTESIAN_POINT ( 'NONE',  ( -33.64072208462274460, 40.62798226556378012, -61.41639582985341406 ) ) ;
#106283 = CARTESIAN_POINT ( 'NONE',  ( -106.4944820610378855, -60.00000000000000711, 119.4794274787003161 ) ) ;
#106284 = VECTOR ( 'NONE', #98823, 1000.000000000000000 ) ;
#106285 = B_SPLINE_CURVE_WITH_KNOTS ( 'NONE', 3,
 ( #101548, #28228, #3919, #10916, #36852, #85365, #93986, #3385, #86456, #102069, #20148, #43834, #61648, #68110, #11454, #94539, #61099, #101009, #53000, #44379, #85920, #11992 ),
 .UNSPECIFIED., .F., .F.,
 ( 4, 2, 2, 2, 2, 2, 2, 2, 2, 2, 4 ),
 ( 0.003083058008555213027, 0.003587558145623166543, 0.003839808214157141783, 0.004092058282691117023, 0.004596558419759062299, 0.004848808488293035804, 0.005101058556827008442, 0.006110058830962918075, 0.006614558968030872024, 0.006866809036564852468, 0.007119059105098832912 ),
 .UNSPECIFIED. ) ;
#106286 = COLOUR_RGB ( '', 0.31764706, 0.68627451, 0.89019608) ;
#106287 = CARTESIAN_POINT ( 'NONE',  ( 19.83349330513380693, -3.851859888774471706E-31, 4.000000000000001776 ) ) ;
#106288 = CARTESIAN_POINT ( 'NONE',  ( 43.69218681961980622, 484.4816931224910945, 2.431261704629519294 ) ) ;
#106289 = VECTOR ( 'NONE', #92824, 1000.000000000000000 ) ;
#106290 = DIRECTION ( 'NONE',  ( -1.000000000000000000, -1.224606353822377258E-16, -0.000000000000000000 ) ) ;
#106291 = CARTESIAN_POINT ( 'NONE',  ( -13.27939269558071622, 1.397586449971225164, 14.93522390679500234 ) ) ;
#106293 = CARTESIAN_POINT ( 'NONE',  ( -15.19414944962576186, 3.422781246270885536, -3.910013010457076721 ) ) ;
#106292 = CARTESIAN_POINT ( 'NONE',  ( 5.036189802309102070, -5.000000000000015099, -93.73786388411730286 ) ) ;
#106294 = CARTESIAN_POINT ( 'NONE',  ( -81.41272853779376817, -60.59700324890057033, 185.5284586587616502 ) ) ;
#106295 = ORIENTED_EDGE ( 'NONE', *, *, #64000, .T. ) ;
#106296 = CARTESIAN_POINT ( 'NONE',  ( 7.500000000000005329, 41.41666666666666430, -71.71180648257555390 ) ) ;
#106297 = ORIENTED_EDGE ( 'NONE', *, *, #64968, .T. ) ;
#106298 = ORIENTED_EDGE ( 'NONE', *, *, #24718, .F. ) ;
#106299 = VECTOR ( 'NONE', #84607, 1000.000000000000000 ) ;
#106300 = CARTESIAN_POINT ( 'NONE',  ( 8.000000000000000000, 9.797174393178825657E-16, -5.575057142857143155 ) ) ;
#106301 = DIRECTION ( 'NONE',  ( 0.5735764363510462704, 0.8191520442889915765, 0.000000000000000000 ) ) ;
#106302 = CARTESIAN_POINT ( 'NONE',  ( 16.08349330513380337, 1.593028355512270567E-15, 0.000000000000000000 ) ) ;
#106303 = FILL_AREA_STYLE_COLOUR ( '', #84040 ) ;
#106304 = CARTESIAN_POINT ( 'NONE',  ( 53.29999999999999716, 3.309500000000014541, 0.000000000000000000 ) ) ;
#106305 = CARTESIAN_POINT ( 'NONE',  ( 10.36974794996676508, -5.000000000000000000, -92.92756386271756242 ) ) ;
#106306 = DIRECTION ( 'NONE',  ( -1.000000000000000000, -1.224606353822377258E-16, -0.000000000000000000 ) ) ;
#106307 = CARTESIAN_POINT ( 'NONE',  ( 107.5810510768942549, -30.00000000000001066, 145.3411688640341879 ) ) ;
#106308 = CARTESIAN_POINT ( 'NONE',  ( -104.0091953780157752, -14.21045842199432663, 192.0632730704776066 ) ) ;
#106309 = CARTESIAN_POINT ( 'NONE',  ( -60.83465437253532571, -46.44060695584406062, 77.79315034241348314 ) ) ;
#106310 = AXIS2_PLACEMENT_3D ( 'NONE', #31983, #39541, #17787 ) ;
#106311 = VERTEX_POINT ( 'NONE', #91233 ) ;
#106312 = CARTESIAN_POINT ( 'NONE',  ( -61.12177193198483138, 38.95340872388008790, 18.06307752582379678 ) ) ;
#106313 = CARTESIAN_POINT ( 'NONE',  ( 114.2967361943732953, -59.99999999999019451, 163.3079217394894727 ) ) ;
#106314 = EDGE_LOOP ( 'NONE', ( #62437, #74100, #33757, #106702 ) ) ;
#106315 = CARTESIAN_POINT ( 'NONE',  ( 1.010365562846486931, -46.43475217007103595, 31.62877532128088731 ) ) ;
#106316 = CARTESIAN_POINT ( 'NONE',  ( -7.188101187500002709, -11.18750000204838457, 2.977408999572647819 ) ) ;
#106317 = EDGE_LOOP ( 'NONE', ( #69817, #20325, #76147, #37251, #96296, #52794 ) ) ;
#106318 = CARTESIAN_POINT ( 'NONE',  ( 7.070208275066456771, -30.00000000000001776, 1.379431653863122387 ) ) ;
#106319 = ORIENTED_EDGE ( 'NONE', *, *, #36377, .T. ) ;
#106320 = FACE_OUTER_BOUND ( 'NONE', #52527, .T. ) ;
#106321 = CARTESIAN_POINT ( 'NONE',  ( 80.00000000000000000, -52.00000000000000000, -23.09707704303352926 ) ) ;
#106322 = CARTESIAN_POINT ( 'NONE',  ( -108.2569967048411002, -60.00000000000000000, 195.1947638852328168 ) ) ;
#106323 = CARTESIAN_POINT ( 'NONE',  ( 9.499205784528923502, -56.64306915247485819, 30.13083833152229829 ) ) ;
#106324 = CARTESIAN_POINT ( 'NONE',  ( 2.977408999572651815, -25.81250000204838813, 7.188101187500000933 ) ) ;
#106325 = CARTESIAN_POINT ( 'NONE',  ( 44.16394502333565697, 464.2849401354476413, 9.200602954361984942 ) ) ;
#106326 = COLOUR_RGB ( '', 0.09019608, 0.27058824, 0.51372549) ;
#106328 = EDGE_CURVE ( 'NONE', #56342, #95728, #5443, .T. ) ;
#106327 = CARTESIAN_POINT ( 'NONE',  ( 8.866506694866188809, 4.000000000000003553, 4.898587196589414801E-16 ) ) ;
#106329 = CARTESIAN_POINT ( 'NONE',  ( -13.12258126849660478, 19.43509895603041215, 7.664272855090029424 ) ) ;
#106330 = CARTESIAN_POINT ( 'NONE',  ( -11.03328975971281345, -4.986640933236349049, -12.57657944225302593 ) ) ;
#106331 = CARTESIAN_POINT ( 'NONE',  ( -32.25199865210507255, 464.6771562214397022, 10.60479922511891893 ) ) ;
#106332 = EDGE_CURVE ( 'NONE', #69972, #19762, #80695, .T. ) ;
#106333 = CARTESIAN_POINT ( 'NONE',  ( 8.238879630815576505, -5.127845683665249510, 14.25497928744678333 ) ) ;
#106334 = LINE ( 'NONE', #75031, #37556 ) ;
#106335 = CARTESIAN_POINT ( 'NONE',  ( 106.3131009653180001, -59.99999999999999289, 178.6139974719857832 ) ) ;
#106336 = CARTESIAN_POINT ( 'NONE',  ( -32.18409987042326037, -32.55419226210070605, 32.69844470122687596 ) ) ;
#106337 = CARTESIAN_POINT ( 'NONE',  ( 2.723397405354400211E-15, -8.673617379884035472E-16, 22.23822744035697241 ) ) ;
#106338 = AXIS2_PLACEMENT_3D ( 'NONE', #14031, #63143, #39404 ) ;
#106339 = CARTESIAN_POINT ( 'NONE',  ( 41.05623627240671425, -36.06612582573725234, 38.79247790458893519 ) ) ;
#106340 = FACE_OUTER_BOUND ( 'NONE', #65314, .T. ) ;
#106341 = EDGE_CURVE ( 'NONE', #5362, #36063, #45950, .T. ) ;
#106342 = ORIENTED_EDGE ( 'NONE', *, *, #29778, .F. ) ;
#106344 = CIRCLE ( 'NONE', #80553, 4.000000000000001776 ) ;
#106343 = CARTESIAN_POINT ( 'NONE',  ( -7.986539162393901492, 88.97327171057456496, -0.5321833565149907130 ) ) ;
#106345 = B_SPLINE_CURVE_WITH_KNOTS ( 'NONE', 3,
 ( #39448, #7049, #31374, #71780, #78817, #37878, #72837, #14596 ),
 .UNSPECIFIED., .F., .F.,
 ( 4, 2, 2, 4 ),
 ( 0.000000000000000000, 0.5000000000000000000, 0.7500000000000000000, 1.000000000000000000 ),
 .UNSPECIFIED. ) ;
#106346 = CARTESIAN_POINT ( 'NONE',  ( -76.87893151430891692, -38.44669289976816628, 183.7668099329592906 ) ) ;
#106347 = ORIENTED_EDGE ( 'NONE', *, *, #105426, .F. ) ;
#106349 = CARTESIAN_POINT ( 'NONE',  ( -31.19652432992544888, 378.3327707670021027, 24.28948218791313707 ) ) ;
#106348 = CARTESIAN_POINT ( 'NONE',  ( 4.852941176470595863, 39.99999999999999289, -70.80672828634229177 ) ) ;
#106350 = CARTESIAN_POINT ( 'NONE',  ( -12.29976574085473473, 22.32620736666799033, -6.386862290538014797 ) ) ;
#106351 = FACE_BOUND ( 'NONE', #102015, .T. ) ;
#106352 = CARTESIAN_POINT ( 'NONE',  ( 6.288680569791143427, 0.6514782672944290365, 6.828922012436084543 ) ) ;
#106353 = CARTESIAN_POINT ( 'NONE',  ( 1.130678585943547532, 43.42148124859406977, -18.03896404153940125 ) ) ;
#106354 = CARTESIAN_POINT ( 'NONE',  ( -37.85084083633361729, 438.0234350436313093, 4.171260309356204843 ) ) ;
#106356 = AXIS2_PLACEMENT_3D ( 'NONE', #101132, #20271, #34839 ) ;
#106355 = CARTESIAN_POINT ( 'NONE',  ( -28.96386208545641594, 320.5436640882624033, 12.80660157965214729 ) ) ;
#106357 = CARTESIAN_POINT ( 'NONE',  ( 92.37230681663571374, -60.00000000000000711, 25.27844034073237012 ) ) ;
#106358 = AXIS2_PLACEMENT_3D ( 'NONE', #55708, #15277, #8241 ) ;
#106359 = CARTESIAN_POINT ( 'NONE',  ( -6.736021983150922487, -48.35471770697892424, 39.27387210330255840 ) ) ;
#106360 = ORIENTED_EDGE ( 'NONE', *, *, #35133, .T. ) ;
#106361 = CARTESIAN_POINT ( 'NONE',  ( -97.81687375994280842, -30.00000000000000711, 190.6942671029864016 ) ) ;
#106362 = ORIENTED_EDGE ( 'NONE', *, *, #28208, .F. ) ;
#106363 = CARTESIAN_POINT ( 'NONE',  ( -9.498520115305538525, -56.64062589231861011, 30.13282173121349317 ) ) ;
#106364 = CARTESIAN_POINT ( 'NONE',  ( -16.01541666090353999, 3.834101040397206894, 1.299565945660708710 ) ) ;
#106365 = CARTESIAN_POINT ( 'NONE',  ( 3.646183794693278024, 22.19690050403223225, 5.000000000000000000 ) ) ;
#106366 = CARTESIAN_POINT ( 'NONE',  ( 14.29190075645217028, 21.26710225494214157, 5.626279437277407425 ) ) ;
#106368 = CARTESIAN_POINT ( 'NONE',  ( -1.469576158976823947E-15, -23.56250000409677270, 8.000000000000000000 ) ) ;
#106367 = MECHANICAL_DESIGN_GEOMETRIC_PRESENTATION_REPRESENTATION (  '', ( #25419 ), #4764 ) ;
#106369 = VECTOR ( 'NONE', #75957, 1000.000000000000000 ) ;
#106370 = CARTESIAN_POINT ( 'NONE',  ( 2.977408999572650927, -25.25000000204839523, -7.188101187500001821 ) ) ;
#106371 = PRESENTATION_STYLE_ASSIGNMENT (( #98297 ) ) ;
#106372 = CARTESIAN_POINT ( 'NONE',  ( 6.965116047733301841, 41.61856606189723351, -70.00485699918137072 ) ) ;
#106373 = EDGE_LOOP ( 'NONE', ( #34248, #30520, #19249, #73492, #7474 ) ) ;
#106374 = EDGE_CURVE ( 'NONE', #79406, #75687, #70961, .T. ) ;
#106375 =( GEOMETRIC_REPRESENTATION_CONTEXT ( 3 ) GLOBAL_UNCERTAINTY_ASSIGNED_CONTEXT ( ( #89069 ) ) GLOBAL_UNIT_ASSIGNED_CONTEXT ( ( #17184, #47532, #64274 ) ) REPRESENTATION_CONTEXT ( 'NONE', 'WORKASPACE' ) );
#106377 = ORIENTED_EDGE ( 'NONE', *, *, #97029, .T. ) ;
#106376 = CARTESIAN_POINT ( 'NONE',  ( 4.628159615119684211, -2.310801729693849005, 102.5435725457685976 ) ) ;
#106378 = CARTESIAN_POINT ( 'NONE',  ( 81.68119091632517836, -32.56014869712902993, 148.9471023736466861 ) ) ;
#106379 = CARTESIAN_POINT ( 'NONE',  ( -39.12903940714779338, 38.95383793066859113, 50.91589357089002732 ) ) ;
#106380 = CARTESIAN_POINT ( 'NONE',  ( 0.000000000000000000, 152.0000000000000000, 0.000000000000000000 ) ) ;
#106381 = ORIENTED_EDGE ( 'NONE', *, *, #7280, .T. ) ;
#106382 = CARTESIAN_POINT ( 'NONE',  ( -37.18423191224957947, 49.99999999999998579, 51.09921067703984221 ) ) ;
#106383 = CARTESIAN_POINT ( 'NONE',  ( 0.000000000000000000, 15.00000000000000000, -8.000000000000000000 ) ) ;
#106384 = CARTESIAN_POINT ( 'NONE',  ( 5.082755093536325930, -14.46875000204838457, -5.082755093536325042 ) ) ;
#106385 = DIRECTION ( 'NONE',  ( 0.000000000000000000, -1.000000000000000000, 0.000000000000000000 ) ) ;
#106386 = FACE_OUTER_BOUND ( 'NONE', #61675, .T. ) ;
#106387 = CARTESIAN_POINT ( 'NONE',  ( -41.14701979708251400, -57.68941641447864299, 57.58229189354211286 ) ) ;
#106388 = DIRECTION ( 'NONE',  ( -0.9915366780650377576, 0.1269898409407599904, 0.02699252395738913415 ) ) ;
#106389 = EDGE_CURVE ( 'NONE', #76782, #40039, #26201, .T. ) ;
#106390 = VERTEX_POINT ( 'NONE', #3805 ) ;
#106391 =( NAMED_UNIT ( * ) SI_UNIT ( $, .STERADIAN. ) SOLID_ANGLE_UNIT ( ) );
#106392 = AXIS2_PLACEMENT_3D ( 'NONE', #58948, #84277, #30851 ) ;
#106393 = FACE_OUTER_BOUND ( 'NONE', #25343, .T. ) ;
#106394 = CARTESIAN_POINT ( 'NONE',  ( -5.656854249492381470, -19.06249999999999289, 5.656854249492379694 ) ) ;
#106395 = CARTESIAN_POINT ( 'NONE',  ( -2.352990130084491319E-16, 8.660254037844390851, -7.422398894150036064 ) ) ;
#106396 = CIRCLE ( 'NONE', #68555, 11.00000000000000000 ) ;
#106397 = ORIENTED_EDGE ( 'NONE', *, *, #76707, .T. ) ;
#106398 = CARTESIAN_POINT ( 'NONE',  ( -7.188101187500000044, -31.90625000204838813, -8.802885111219163269E-16 ) ) ;
#106399 = CARTESIAN_POINT ( 'NONE',  ( 25.33765615706812824, -29.26986317732292875, 38.39381496285782447 ) ) ;
#106400 = CARTESIAN_POINT ( 'NONE',  ( -40.01928047903233931, 489.9206396166244417, 11.12040978472883879 ) ) ;
#106401 = CARTESIAN_POINT ( 'NONE',  ( 8.099999999999999645, 0.000000000000000000, 0.000000000000000000 ) ) ;
#106402 = AXIS2_PLACEMENT_3D ( 'NONE', #104231, #79432, #79953 ) ;
#106403 = EDGE_CURVE ( 'NONE', #45933, #76580, #98439, .T. ) ;
#106404 = CARTESIAN_POINT ( 'NONE',  ( 36.86311888821725091, 438.9044241143811860, 23.87836450218838635 ) ) ;
#106405 = APPLICATION_PROTOCOL_DEFINITION ( 'draft international standard', 'automotive_design', 1998, #34237 ) ;
#106406 = CARTESIAN_POINT ( 'NONE',  ( 48.76867190053936696, 8.289666503167284262, 16.61714170247970657 ) ) ;
#106407 = ORIENTED_EDGE ( 'NONE', *, *, #101985, .T. ) ;
#106408 = CARTESIAN_POINT ( 'NONE',  ( 0.000000000000000000, 0.000000000000000000, 0.000000000000000000 ) ) ;
#106409 = DIRECTION ( 'NONE',  ( -0.000000000000000000, 0.000000000000000000, 1.000000000000000000 ) ) ;
#106410 = CARTESIAN_POINT ( 'NONE',  ( 34.43512893958828869, -31.17098412693171738, -37.93505368340076700 ) ) ;
#106411 = FACE_OUTER_BOUND ( 'NONE', #9168, .T. ) ;
#106412 = ADVANCED_FACE ( 'NONE', ( #5396 ), #5330, .F. ) ;
#106413 = DIRECTION ( 'NONE',  ( -1.000000000000000000, -1.224606353822377258E-16, -0.000000000000000000 ) ) ;
#106414 = ORIENTED_EDGE ( 'NONE', *, *, #82009, .T. ) ;
#106415 = CIRCLE ( 'NONE', #23783, 8.142857142857131691 ) ;
#106416 = DIRECTION ( 'NONE',  ( 0.000000000000000000, 0.000000000000000000, 1.000000000000000000 ) ) ;
#106417 = CARTESIAN_POINT ( 'NONE',  ( 98.12606319475514738, -57.67113334830845162, 57.02791250460963823 ) ) ;
#106418 = VECTOR ( 'NONE', #61010, 1000.000000000000227 ) ;
#106419 = CARTESIAN_POINT ( 'NONE',  ( 36.69951191943477653, 463.3005535825504353, 20.13750663043823863 ) ) ;
#106420 = CARTESIAN_POINT ( 'NONE',  ( -9.812526520939238495, 51.27367565803530169, -2.925190231983776368 ) ) ;
#106421 = CARTESIAN_POINT ( 'NONE',  ( 8.673617379884035472E-16, 7.505553499465148271, -0.7999999999999977129 ) ) ;
#106422 = CARTESIAN_POINT ( 'NONE',  ( 0.000000000000000000, -6.928203230275503444, 4.000000000000010658 ) ) ;
#106423 = CARTESIAN_POINT ( 'NONE',  ( -73.46981879484900446, -60.00000000000000711, 166.8934759688809493 ) ) ;
#106424 = ADVANCED_FACE ( 'NONE', ( #47426 ), #32345, .F. ) ;
#106426 = AXIS2_PLACEMENT_3D ( 'NONE', #68547, #78726, #35669 ) ;
#106425 = FILL_AREA_STYLE_COLOUR ( '', #40730 ) ;
#106427 = CARTESIAN_POINT ( 'NONE',  ( -53.52139369739177255, 50.00000000000000000, 33.73130704865319274 ) ) ;
#106428 = VECTOR ( 'NONE', #97123, 1000.000000000000000 ) ;
#106429 = EDGE_CURVE ( 'NONE', #89689, #696, #51921, .T. ) ;
#106430 = CARTESIAN_POINT ( 'NONE',  ( -86.24395819885462799, -21.22842368464919360, 178.4804303958884191 ) ) ;
#106431 = ORIENTED_EDGE ( 'NONE', *, *, #4837, .F. ) ;
#106432 = CARTESIAN_POINT ( 'NONE',  ( 27.24829532723339653, 307.7585719329687208, -9.350284670461302738 ) ) ;
#106433 = B_SPLINE_CURVE_WITH_KNOTS ( 'NONE', 3,
 ( #3160, #4756, #3705, #11230, #60879, #44698, #36104, #101848, #36631, #62468, #20990, #53310, #27481, #70559, #101329, #44155 ),
 .UNSPECIFIED., .F., .F.,
 ( 4, 2, 2, 2, 2, 2, 2, 4 ),
 ( 0.000000000000000000, 0.001820320936770163881, 0.003640641873540327762, 0.005460962810310492077, 0.007281283747080655525, 0.01092192562062098415, 0.01274224655739114760, 0.01456256749416131105 ),
 .UNSPECIFIED. ) ;
#106434 = ORIENTED_EDGE ( 'NONE', *, *, #6254, .F. ) ;
#106435 = CARTESIAN_POINT ( 'NONE',  ( -7.343637806710343163, -12.44363121900618729, 3.177475076494673534 ) ) ;
#106436 = CYLINDRICAL_SURFACE ( 'NONE', #102406, 4.000000000000000000 ) ;
#106437 = CARTESIAN_POINT ( 'NONE',  ( -84.47593557506488082, -45.26840861548302541, -7.721260587021224531 ) ) ;
#106438 = CARTESIAN_POINT ( 'NONE',  ( -42.54181027564564488, 465.0722614357791258, 13.76085909083398739 ) ) ;
#106439 = CARTESIAN_POINT ( 'NONE',  ( 6.563035550597769330, 3.302680408004402324, -6.845819698387219709 ) ) ;
#106440 = AXIS2_PLACEMENT_3D ( 'NONE', #43068, #27455, #26920 ) ;
#106441 = ORIENTED_EDGE ( 'NONE', *, *, #93977, .T. ) ;
#106442 = CIRCLE ( 'NONE', #41018, 4.000000000000007105 ) ;
#106444 = CARTESIAN_POINT ( 'NONE',  ( 14.85284876471456350, 1.482358050883964840E-15, 0.000000000000000000 ) ) ;
#106443 = CIRCLE ( 'NONE', #15223, 4.000000000000000888 ) ;
#106445 = CARTESIAN_POINT ( 'NONE',  ( 10.14577494216288400, 12.16872942106264865, -10.55611388860419453 ) ) ;
#106446 = CARTESIAN_POINT ( 'NONE',  ( 14.86825985028009711, -3.469446951953614189E-15, -8.569529079650944681 ) ) ;
#106447 = FILL_AREA_STYLE ('',( #75680 ) ) ;
#106448 = CARTESIAN_POINT ( 'NONE',  ( 56.79302105626919683, -14.21045842199427867, -31.02814365720875500 ) ) ;
#106449 = CARTESIAN_POINT ( 'NONE',  ( -77.12671445486094512, -46.43767849076631649, 136.1084143596141018 ) ) ;
#106450 = ORIENTED_EDGE ( 'NONE', *, *, #102113, .F. ) ;
#106451 = CARTESIAN_POINT ( 'NONE',  ( 39.04758850296788353, -59.99999999999992184, 54.77506993285218329 ) ) ;
#106452 = CARTESIAN_POINT ( 'NONE',  ( 7.003653396366580353, 86.05706205559677358, -3.866846144092868531 ) ) ;
#106453 = CARTESIAN_POINT ( 'NONE',  ( 98.20513577084435042, -57.67132909654652906, 57.59918237178697353 ) ) ;
#106454 = AXIS2_PLACEMENT_3D ( 'NONE', #36283, #60533, #101503 ) ;
#106455 = ORIENTED_EDGE ( 'NONE', *, *, #74003, .F. ) ;
#106456 = CARTESIAN_POINT ( 'NONE',  ( 27.42411589273523731, 34.37229030169084609, 10.02668682424727287 ) ) ;
#106457 = CARTESIAN_POINT ( 'NONE',  ( 18.13561277374696701, -5.000000000000000000, 0.000000000000000000 ) ) ;
#106458 = VERTEX_POINT ( 'NONE', #80317 ) ;
#106459 = DIRECTION ( 'NONE',  ( 0.000000000000000000, -1.000000000000000000, 0.000000000000000000 ) ) ;
#106460 = CARTESIAN_POINT ( 'NONE',  ( 72.37206225042174879, 6.856755485862130937E-15, 0.000000000000000000 ) ) ;
#106461 = CARTESIAN_POINT ( 'NONE',  ( -6.999999999999994671, -46.00000000000000000, 102.2532056551910387 ) ) ;
#106462 = CARTESIAN_POINT ( 'NONE',  ( -5.082755093536325042, -17.09375000204838813, -5.082755093536325930 ) ) ;
#106463 = CARTESIAN_POINT ( 'NONE',  ( 43.69141235712699967, 485.1129823701804185, 2.341835213797379467 ) ) ;
#106464 = CARTESIAN_POINT ( 'NONE',  ( 9.798380800342661345, 81.53199345684495825, -2.010350564680322361 ) ) ;
#106465 =( NAMED_UNIT ( * ) PLANE_ANGLE_UNIT ( ) SI_UNIT ( $, .RADIAN. ) );
#106466 = EDGE_CURVE ( 'NONE', #32281, #8358, #93291, .T. ) ;
#106467 = CARTESIAN_POINT ( 'NONE',  ( 5.000000000000000000, 6.123233995736766282E-16, -5.710657142857142432 ) ) ;
#106468 = CARTESIAN_POINT ( 'NONE',  ( 0.000000000000000000, 45.89575828009193259, 0.000000000000000000 ) ) ;
#106469 = EDGE_LOOP ( 'NONE', ( #53150, #12131, #5910, #46164, #74447 ) ) ;
#106470 = CARTESIAN_POINT ( 'NONE',  ( -7.493261935387684147, 40.00000000000277822, -69.66936203106251924 ) ) ;
#106472 = CARTESIAN_POINT ( 'NONE',  ( 30.76658144297569208, -60.32562095059588358, 37.11897213549833907 ) ) ;
#106471 = CARTESIAN_POINT ( 'NONE',  ( -29.53202096672922039, -60.00000000000010658, 45.26681583358117678 ) ) ;
#106473 = CARTESIAN_POINT ( 'NONE',  ( 25.09730810927034739, 306.2366149690730595, -8.697816624931766327 ) ) ;
#106474 = ADVANCED_FACE ( 'NONE', ( #56576, #48485, #16126, #64690, #39886 ), #8027, .F. ) ;
#106475 = ORIENTED_EDGE ( 'NONE', *, *, #17288, .T. ) ;
#106476 = CIRCLE ( 'NONE', #35937, 4.250000000000000000 ) ;
#106477 = EDGE_LOOP ( 'NONE', ( #104827, #25638, #50761, #44904, #70820 ) ) ;
#106479 = CARTESIAN_POINT ( 'NONE',  ( 0.1702502393396320146, 51.26930509877140452, 10.25000000000000178 ) ) ;
#106478 = CARTESIAN_POINT ( 'NONE',  ( 0.000000000000000000, -5.629165124598850767, -3.249999999999999556 ) ) ;
#106480 = DIRECTION ( 'NONE',  ( -0.000000000000000000, 1.000000000000000000, 0.000000000000000000 ) ) ;
#106481 = CARTESIAN_POINT ( 'NONE',  ( -17.14862568216160099, 294.5838465266265302, -10.05695664460883521 ) ) ;
#106482 = APPLICATION_CONTEXT ( 'automotive_design' ) ;
#106483 = CARTESIAN_POINT ( 'NONE',  ( -5.000000000000000000, -15.93202192939577344, -5.930487099830192399 ) ) ;
#106484 = EDGE_CURVE ( 'NONE', #82046, #25659, #81378, .T. ) ;
#106485 = CARTESIAN_POINT ( 'NONE',  ( 0.8390624637001048436, 46.08972068689292456, 16.56986929762893013 ) ) ;
#106486 = CARTESIAN_POINT ( 'NONE',  ( -36.18016141387858653, 463.3220971514191433, 20.09605424492809433 ) ) ;
#106488 = ORIENTED_EDGE ( 'NONE', *, *, #100977, .T. ) ;
#106487 = VECTOR ( 'NONE', #47333, 1000.000000000000000 ) ;
#106489 = CARTESIAN_POINT ( 'NONE',  ( 0.000000000000000000, -100.0000000000000000, 0.000000000000000000 ) ) ;
#106490 = CARTESIAN_POINT ( 'NONE',  ( 32.93681933017204955, 464.9081438944968454, 10.83352224628442251 ) ) ;
#106491 = CARTESIAN_POINT ( 'NONE',  ( 32.03075683730855161, 464.8596926554154152, 12.88957819155500850 ) ) ;
#106492 = CARTESIAN_POINT ( 'NONE',  ( 76.77425057322363955, -30.00000000000000355, -16.81280392441903615 ) ) ;
#106493 = DIRECTION ( 'NONE',  ( -0.000000000000000000, 1.000000000000000000, -0.000000000000000000 ) ) ;
#106494 = ORIENTED_EDGE ( 'NONE', *, *, #90616, .T. ) ;
#106495 = EDGE_CURVE ( 'NONE', #478, #104331, #52010, .T. ) ;
#106496 = DIRECTION ( 'NONE',  ( 0.000000000000000000, 0.000000000000000000, 1.000000000000000000 ) ) ;
#106497 = ORIENTED_EDGE ( 'NONE', *, *, #99066, .F. ) ;
#106498 = CONICAL_SURFACE ( 'NONE', #60037, 5.000000000000001776, 0.9599310885968803664 ) ;
#106499 = EDGE_LOOP ( 'NONE', ( #78939, #41513 ) ) ;
#106500 = CARTESIAN_POINT ( 'NONE',  ( 0.7761051413992605674, 54.19697142896034592, 8.016680439112649381 ) ) ;
#106501 = SURFACE_SIDE_STYLE ('',( #31593 ) ) ;
#106502 = SURFACE_STYLE_FILL_AREA ( #48262 ) ;
#106503 = DIRECTION ( 'NONE',  ( 0.000000000000000000, -1.000000000000000000, 0.000000000000000000 ) ) ;
#106504 = CARTESIAN_POINT ( 'NONE',  ( -44.56312866057822930, 339.9956215472535632, 0.8225827590551298973 ) ) ;
#106505 = CARTESIAN_POINT ( 'NONE',  ( -4.990218406113974936, -61.74584101121605784, 12.75302187936684994 ) ) ;
#106506 = CARTESIAN_POINT ( 'NONE',  ( -30.00000000000000000, -54.00000000000000711, 23.11721482942554928 ) ) ;
#106507 = CARTESIAN_POINT ( 'NONE',  ( 12.50000000000000355, 39.76653967993013339, -65.06879462632775812 ) ) ;
#106508 = EDGE_LOOP ( 'NONE', ( #59205, #2717, #11150, #12271, #45629 ) ) ;
#106509 = CARTESIAN_POINT ( 'NONE',  ( -9.522512062097407082, 43.48390578715350330, 15.16028251901261648 ) ) ;
#106510 = ORIENTED_EDGE ( 'NONE', *, *, #51531, .F. ) ;
#106511 = EDGE_CURVE ( 'NONE', #45114, #38179, #25554, .T. ) ;
#106512 = DIRECTION ( 'NONE',  ( -1.000000000000000000, -0.000000000000000000, -0.000000000000000000 ) ) ;
#106513 = CYLINDRICAL_SURFACE ( 'NONE', #9115, 4.250000000000000000 ) ;
#106514 =( LENGTH_UNIT ( ) NAMED_UNIT ( * ) SI_UNIT ( .MILLI., .METRE. ) );
#106515 = AXIS2_PLACEMENT_3D ( 'NONE', #32872, #83514, #92136 ) ;
#106516 = DIRECTION ( 'NONE',  ( 0.000000000000000000, 0.000000000000000000, -1.000000000000000000 ) ) ;
#106517 = CARTESIAN_POINT ( 'NONE',  ( 67.10493487639952548, -60.33315822119670457, 104.4191278749690213 ) ) ;
#106518 = CIRCLE ( 'NONE', #79045, 4.172000000000009479 ) ;
#106519 = ORIENTED_EDGE ( 'NONE', *, *, #41026, .F. ) ;
#106520 = CARTESIAN_POINT ( 'NONE',  ( 17.50000000000003197, 48.94931827546790970, 64.05766423107181140 ) ) ;
#106521 = CARTESIAN_POINT ( 'NONE',  ( 7.188101187500000044, -29.65625000204838813, 0.000000000000000000 ) ) ;
#106522 = FACE_OUTER_BOUND ( 'NONE', #98864, .T. ) ;
#106523 = ADVANCED_FACE ( 'NONE', ( #22665, #56033 ), #88964, .T. ) ;
#106524 = ORIENTED_EDGE ( 'NONE', *, *, #46273, .T. ) ;
#106525 = SURFACE_STYLE_FILL_AREA ( #32139 ) ;
#106526 = STYLED_ITEM ( 'NONE', ( #88831 ), #27291 ) ;
#106527 = STYLED_ITEM ( 'NONE', ( #3397 ), #41370 ) ;
#106528 = CIRCLE ( 'NONE', #67050, 0.9999999999999977796 ) ;
#106529 = CARTESIAN_POINT ( 'NONE',  ( -35.80932576323957761, 491.2997492151604888, 12.22805875982552948 ) ) ;
#106530 = LINE ( 'NONE', #91438, #11953 ) ;
#106531 = CARTESIAN_POINT ( 'NONE',  ( -5.656854249492381470, -23.75000000409677270, 5.656854249492379694 ) ) ;
#106532 =( LENGTH_UNIT ( ) NAMED_UNIT ( * ) SI_UNIT ( .MILLI., .METRE. ) );
#106533 = CYLINDRICAL_SURFACE ( 'NONE', #93895, 8.000000000000000000 ) ;
#106534 = CARTESIAN_POINT ( 'NONE',  ( 0.000000000000000000, 5.629165124598848102, 3.250000000000005329 ) ) ;
#106535 = CARTESIAN_POINT ( 'NONE',  ( -10.01627249115706775, 7.476760474189256378, 0.000000000000000000 ) ) ;
#106536 = CARTESIAN_POINT ( 'NONE',  ( 0.000000000000000000, 304.8518027762758038, 9.936999415352289589 ) ) ;
#106537 = B_SPLINE_CURVE_WITH_KNOTS ( 'NONE', 3,
 ( #76461, #60318, #77542, #35519, #52186, #34984 ),
 .UNSPECIFIED., .F., .F.,
 ( 4, 2, 4 ),
 ( 0.01067228061038544978, 0.01257272967564229335, 0.01447317874089913692 ),
 .UNSPECIFIED. ) ;
#106538 =( NAMED_UNIT ( * ) SI_UNIT ( $, .STERADIAN. ) SOLID_ANGLE_UNIT ( ) );
#106539 = CARTESIAN_POINT ( 'NONE',  ( -1.544939622599253326, 15.00000000000000000, -9.999999999999998224 ) ) ;
#106540 = VERTEX_POINT ( 'NONE', #100233 ) ;
#106541 = CARTESIAN_POINT ( 'NONE',  ( -3.999994092537668244, -10.00072617203139203, 6.928206640937045080 ) ) ;
#106542 = FACE_OUTER_BOUND ( 'NONE', #692, .T. ) ;
#106543 = CARTESIAN_POINT ( 'NONE',  ( -97.61356772442498198, -30.00000000000000000, 190.8259052030175837 ) ) ;
#106544 = EDGE_CURVE ( 'NONE', #7582, #37996, #70413, .T. ) ;
#106545 = AXIS2_PLACEMENT_3D ( 'NONE', #77133, #84167, #25976 ) ;
#106546 = CIRCLE ( 'NONE', #91104, 5.000000000000001776 ) ;
#106547 = CARTESIAN_POINT ( 'NONE',  ( 39.83349330513380693, 4.898587196589405926E-16, -4.000000000000001776 ) ) ;
#106548 = CARTESIAN_POINT ( 'NONE',  ( 73.67851877562725349, -57.62598256385592776, 185.4460714352483137 ) ) ;
#106550 = CARTESIAN_POINT ( 'NONE',  ( -6.222225870502539280, 4.750888635085242839, 4.991891345689136728 ) ) ;
#106549 = CARTESIAN_POINT ( 'NONE',  ( 4.898587196589412829E-16, -15.31250000409677092, -8.000000000000000000 ) ) ;
#106551 = EDGE_CURVE ( 'NONE', #96401, #54339, #25319, .T. ) ;
#106552 = AXIS2_PLACEMENT_3D ( 'NONE', #79817, #56047, #39903 ) ;
#106553 = CARTESIAN_POINT ( 'NONE',  ( 16.84999999999999787, -3.309499999999999886, 4.475777889183790779E-16 ) ) ;
#106554 = CARTESIAN_POINT ( 'NONE',  ( 32.61650669486618881, 4.000000000000003553, 4.898587196589414801E-16 ) ) ;
#106555 = UNCERTAINTY_MEASURE_WITH_UNIT (LENGTH_MEASURE( 1.000000000000000082E-05 ), #76735, 'distance_accuracy_value', 'NONE');
#106556 = CARTESIAN_POINT ( 'NONE',  ( -3.616699737053585828, -60.00000000000002132, 39.63238166876963930 ) ) ;
#106557 = SURFACE_SIDE_STYLE ('',( #106017 ) ) ;
#106558 = AXIS2_PLACEMENT_3D ( 'NONE', #42117, #24902, #83113 ) ;
#106559 = CARTESIAN_POINT ( 'NONE',  ( 6.497272336416993532, 53.67373393826039774, 6.919306612608417062 ) ) ;
#106560 = CARTESIAN_POINT ( 'NONE',  ( -86.96504166901752342, -31.71858355094692072, 187.3098402634578861 ) ) ;
#106561 = EDGE_CURVE ( 'NONE', #54371, #93985, #15903, .T. ) ;
#106562 = ORIENTED_EDGE ( 'NONE', *, *, #29212, .T. ) ;
#106563 = CARTESIAN_POINT ( 'NONE',  ( 17.50000000000003197, 51.85440564192877844, 61.62473156926930073 ) ) ;
#106564 = DIRECTION ( 'NONE',  ( 0.000000000000000000, 0.8660254037844379305, -0.5000000000000014433 ) ) ;
#106565 = CARTESIAN_POINT ( 'NONE',  ( -7.255220592255878564, -56.88418264328358021, 33.36068424955863065 ) ) ;
#106566 =( BOUNDED_CURVE ( )  B_SPLINE_CURVE ( 2, ( #87829, #22590, #55427, #78642, #71618, #13377, #104520, #4781, #21520 ),
 .UNSPECIFIED., .F., .F. ) 
 B_SPLINE_CURVE_WITH_KNOTS ( ( 3, 2, 2, 2, 3 ),
 ( 0.3382352941176470229, 0.3455882352941175850, 0.3529411764705882026, 0.3602941176470587648, 0.3676470588235293824 ),
 .UNSPECIFIED. ) 
 CURVE ( )  GEOMETRIC_REPRESENTATION_ITEM ( )  RATIONAL_B_SPLINE_CURVE ( ( 1.000000000000000666, 0.9238795325112861834, 1.000000000000000000, 0.9238795325112867385, 1.000000000000000000, 0.9238795325112867385, 1.000000000000000000, 0.9238795325112872936, 0.9999999999999994449 ) ) 
 REPRESENTATION_ITEM ( '' )  );
#106568 = CARTESIAN_POINT ( 'NONE',  ( -8.398963767913890877, 53.73760393018520887, 4.031152949374985361 ) ) ;
#106567 = CARTESIAN_POINT ( 'NONE',  ( 5.619193549421241052, -4.261310591078192545, -5.875704392893802641 ) ) ;
#106569 = EDGE_LOOP ( 'NONE', ( #104361, #16173, #85662, #52715, #103911 ) ) ;
#106570 = CARTESIAN_POINT ( 'NONE',  ( 26.94447279565465792, 34.53217287173363559, 10.05698433968570527 ) ) ;
#106571 = COLOUR_RGB ( '', 0.72549020, 0.75294118, 0.79215686) ;
#106572 = CARTESIAN_POINT ( 'NONE',  ( -9.474439531904259582, -5.000000000000035527, -19.39817504953388294 ) ) ;
#106573 = CARTESIAN_POINT ( 'NONE',  ( -7.801339272325197527, 33.58731471959700343, -1.788609912539670166 ) ) ;
#106574 = CARTESIAN_POINT ( 'NONE',  ( 29.99261461565485476, 297.7707857721058531, -1.359080099825844989 ) ) ;
#106575 = DIRECTION ( 'NONE',  ( 0.000000000000000000, -1.000000000000000000, 0.000000000000000000 ) ) ;
#106576 = CLOSED_SHELL ( 'NONE', ( #54019, #87346, #82390, #70720, #89137, #60828, #81516, #35992, #15052, #50574, #106474, #93156, #43767, #78831, #67436, #100105, #48239, #65303, #97874, #55371, #44737, #20263, #100573, #58517, #9895, #4465, #13484, #105745, #102386, #58495, #25899, #23149 ) ) ;
#106577 = CARTESIAN_POINT ( 'NONE',  ( -7.934996450857311423, -81.13137543527469120, -1.050865690281774345 ) ) ;
#106578 = SURFACE_STYLE_FILL_AREA ( #42378 ) ;
#106579 = CARTESIAN_POINT ( 'NONE',  ( 114.2391797980453276, -59.99999999999998579, 181.3573912910646015 ) ) ;
#106580 = CARTESIAN_POINT ( 'NONE',  ( -35.66932529116966322, 438.9565575286536045, 4.011496722538590909 ) ) ;
#106581 = VERTEX_POINT ( 'NONE', #82994 ) ;
#106582 = CARTESIAN_POINT ( 'NONE',  ( -7.912393634621968097, -29.99999999999999645, -0.8598757053164162167 ) ) ;
#106583 = CARTESIAN_POINT ( 'NONE',  ( -9.381593208289404018, 252.0143863811949529, -3.465401811657791598 ) ) ;
#106584 = COLOUR_RGB ( '', 0.09019608, 0.27058824, 0.51372549) ;
#106585 = CARTESIAN_POINT ( 'NONE',  ( -33.00000000000000000, 485.0303364503728289, 0.9535057477320436625 ) ) ;
#106586 = CARTESIAN_POINT ( 'NONE',  ( 3.991147588110782074, -1.050389752018302314, 104.5610969444638556 ) ) ;
#106587 = CONICAL_SURFACE ( 'NONE', #34343, 8.000000000000007105, 0.7853981633974509435 ) ;
#106588 = DIRECTION ( 'NONE',  ( 0.000000000000000000, 0.000000000000000000, -1.000000000000000000 ) ) ;
#106589 = VERTEX_POINT ( 'NONE', #27461 ) ;
#106590 = UNCERTAINTY_MEASURE_WITH_UNIT (LENGTH_MEASURE( 1.000000000000000082E-05 ), #18472, 'distance_accuracy_value', 'NONE');
#106591 = CARTESIAN_POINT ( 'NONE',  ( -22.40060265138178153, 305.3960761985100021, 9.054534321561812149 ) ) ;
#106592 = ORIENTED_EDGE ( 'NONE', *, *, #55462, .F. ) ;
#106593 = CARTESIAN_POINT ( 'NONE',  ( 38.69275568812178534, 485.6230355318868988, -4.306148472021496865 ) ) ;
#106594 = CARTESIAN_POINT ( 'NONE',  ( 31.00201403163103819, 438.8339473355226801, 22.04021393888145042 ) ) ;
#106595 = SURFACE_SIDE_STYLE ('',( #71566 ) ) ;
#106596 = CARTESIAN_POINT ( 'NONE',  ( 9.508921847869231669, 46.21454289499525458, 13.17524946764673643 ) ) ;
#106597 = ORIENTED_EDGE ( 'NONE', *, *, #84767, .T. ) ;
#106598 = EDGE_CURVE ( 'NONE', #1084, #92669, #31410, .T. ) ;
#106599 = CARTESIAN_POINT ( 'NONE',  ( -9.999999999999982236, 7.499999999999973355, 0.000000000000000000 ) ) ;
#106600 = CARTESIAN_POINT ( 'NONE',  ( -28.88003843141569149, -59.99999999999504752, 45.10078281693999003 ) ) ;
#106601 = LINE ( 'NONE', #65624, #6655 ) ;
#106602 = CARTESIAN_POINT ( 'NONE',  ( 92.77553358407693906, -60.00000000000002132, 30.03680362789697611 ) ) ;
#106604 = CARTESIAN_POINT ( 'NONE',  ( 16.44069842872639597, -22.06891279552154472, 27.77928941714268518 ) ) ;
#106603 = CARTESIAN_POINT ( 'NONE',  ( -109.5675793427969040, -29.99999999999999289, 170.1817020036065742 ) ) ;
#106605 = CIRCLE ( 'NONE', #60150, 62.00000000000000000 ) ;
#106607 = EDGE_CURVE ( 'NONE', #52182, #87322, #45185, .T. ) ;
#106606 = CARTESIAN_POINT ( 'NONE',  ( 0.000000000000000000, 0.000000000000000000, 0.000000000000000000 ) ) ;
#106608 = CARTESIAN_POINT ( 'NONE',  ( -44.36511314976974063, -18.78910562120168137, 37.46626611847334942 ) ) ;
#106609 = CARTESIAN_POINT ( 'NONE',  ( -0.5677851517752953159, 35.03120528833704128, -27.38325881563803676 ) ) ;
#106610 = VERTEX_POINT ( 'NONE', #75427 ) ;
#106611 = SURFACE_STYLE_USAGE ( .BOTH. , #98519 ) ;
#106612 = STYLED_ITEM ( 'NONE', ( #25273 ), #39919 ) ;
#106613 = DIRECTION ( 'NONE',  ( -0.1091179629862816802, 0.9940288075069678708, 0.000000000000000000 ) ) ;
#106614 = CARTESIAN_POINT ( 'NONE',  ( 6.594225035609136754, -11.92007582869072735, 9.808253832663687888 ) ) ;
#106615 = CARTESIAN_POINT ( 'NONE',  ( 2.500000000000001776, -13.08383851101123163, -21.61544523615733482 ) ) ;
#106616 = CARTESIAN_POINT ( 'NONE',  ( 13.58423288633485804, 304.5480220053966605, -10.06457059527332376 ) ) ;
#106617 = CARTESIAN_POINT ( 'NONE',  ( 24.80105969489321893, 306.0237540681346218, -9.745911707960095427 ) ) ;
#106618 = ORIENTED_EDGE ( 'NONE', *, *, #52493, .T. ) ;
#106619 = CARTESIAN_POINT ( 'NONE',  ( 4.999999999999993783, -45.99999999999999289, 103.2791840072761858 ) ) ;
#106620 = EDGE_LOOP ( 'NONE', ( #24527, #51956, #18369, #35608 ) ) ;
#106621 = CARTESIAN_POINT ( 'NONE',  ( 74.76569601199581427, -30.00000000009216805, 154.8922564148840877 ) ) ;
#106622 = CARTESIAN_POINT ( 'NONE',  ( 23.88591914974023211, 41.62762614956155005, -74.45994044123901290 ) ) ;
#106623 = CARTESIAN_POINT ( 'NONE',  ( 24.41576965198462190, 25.25667818450425273, -32.32162735095537442 ) ) ;
#106624 = DIRECTION ( 'NONE',  ( -1.000000000000000000, -1.224606353822377258E-16, -0.000000000000000000 ) ) ;
#106625 = CARTESIAN_POINT ( 'NONE',  ( 92.05506390259360217, -30.00000000000000355, 100.4937872494486015 ) ) ;
#106626 = CARTESIAN_POINT ( 'NONE',  ( 18.13561277374696701, 0.000000000000000000, 5.000000000000002665 ) ) ;
#106627 = ORIENTED_EDGE ( 'NONE', *, *, #52751, .F. ) ;
#106628 = EDGE_CURVE ( 'NONE', #60384, #103201, #17615, .T. ) ;
#106629 = PRESENTATION_LAYER_ASSIGNMENT (  '', '', ( #72218 ) ) ;
#106630 = ORIENTED_EDGE ( 'NONE', *, *, #25927, .T. ) ;
#106631 = ORIENTED_EDGE ( 'NONE', *, *, #78732, .F. ) ;
#106633 = AXIS2_PLACEMENT_3D ( 'NONE', #9567, #82411, #74309 ) ;
#106632 = DIRECTION ( 'NONE',  ( 0.000000000000000000, -1.000000000000000000, 0.000000000000000000 ) ) ;
#106634 = CARTESIAN_POINT ( 'NONE',  ( -6.689297301784361771, 41.36669071757170713, -70.70516774815108363 ) ) ;
#106635 = CARTESIAN_POINT ( 'NONE',  ( -39.39457526263961995, 464.0483451943321143, 18.48383133219108032 ) ) ;
#106636 = ORIENTED_EDGE ( 'NONE', *, *, #24617, .F. ) ;
#106637 = CARTESIAN_POINT ( 'NONE',  ( 9.842984802582135373, 108.5906959047565010, 1.781981959250507064 ) ) ;
#106638 = EDGE_LOOP ( 'NONE', ( #50874, #59272, #34242, #81842 ) ) ;
#106639 = DIRECTION ( 'NONE',  ( -1.000000000000000000, -1.224606353822377258E-16, -0.000000000000000000 ) ) ;
#106640 = CARTESIAN_POINT ( 'NONE',  ( 87.39133433791327832, -38.57836354491904274, 199.7233327510910499 ) ) ;
#106641 = CARTESIAN_POINT ( 'NONE',  ( 30.13260911416876908, 316.8380131115717404, 13.36150501092329534 ) ) ;
#106642 = CARTESIAN_POINT ( 'NONE',  ( 1.380949872273418154E-15, 45.89575828009193259, 11.27631144943088337 ) ) ;
#106643 = CIRCLE ( 'NONE', #1530, 4.000000000000001776 ) ;
#106644 = CARTESIAN_POINT ( 'NONE',  ( 21.84999999999999787, 3.309500000000003439, 0.000000000000000000 ) ) ;
#106645 = CARTESIAN_POINT ( 'NONE',  ( -41.02721008360138910, 460.5398098099256572, 2.518281297462771295 ) ) ;
#106646 = CARTESIAN_POINT ( 'NONE',  ( -4.399054598113077752, -48.11244280224737935, 102.7269706464928021 ) ) ;
#106647 = DIRECTION ( 'NONE',  ( 0.000000000000000000, -1.000000000000000000, 0.000000000000000000 ) ) ;
#106648 = CARTESIAN_POINT ( 'NONE',  ( -5.956988534971662475, 4.556784786910193397, 5.000000000000000000 ) ) ;
#106649 = ORIENTED_EDGE ( 'NONE', *, *, #58884, .T. ) ;
#106650 = CARTESIAN_POINT ( 'NONE',  ( 3.040134639727833044, -49.16875784325965526, 104.0101424759970428 ) ) ;
#106652 = CARTESIAN_POINT ( 'NONE',  ( -26.60267441690067258, 296.3168466367462202, 10.25441967244310071 ) ) ;
#106651 = CYLINDRICAL_SURFACE ( 'NONE', #14109, 2.000000000000000000 ) ;
#106653 = PRESENTATION_STYLE_ASSIGNMENT (( #16591 ) ) ;
#106654 = UNCERTAINTY_MEASURE_WITH_UNIT (LENGTH_MEASURE( 1.000000000000000082E-05 ), #61638, 'distance_accuracy_value', 'NONE');
#106655 = CARTESIAN_POINT ( 'NONE',  ( 0.000000000000000000, 0.000000000000000000, 0.000000000000000000 ) ) ;
#106656 = DIRECTION ( 'NONE',  ( 0.000000000000000000, -1.000000000000000000, 0.000000000000000000 ) ) ;
#106657 = CARTESIAN_POINT ( 'NONE',  ( -6.499999999999999112, 3.752776749732556816, -6.064240316920397333 ) ) ;
#106658 = DIRECTION ( 'NONE',  ( -1.000000000000000000, -1.224606353822377258E-16, -0.000000000000000000 ) ) ;
#106659 = VECTOR ( 'NONE', #58463, 1000.000000000000000 ) ;
#106660 = DIRECTION ( 'NONE',  ( 0.000000000000000000, 1.000000000000000000, 0.000000000000000000 ) ) ;
#106661 = ORIENTED_EDGE ( 'NONE', *, *, #86082, .T. ) ;
#106662 = CARTESIAN_POINT ( 'NONE',  ( 84.17059686059378976, -61.05527343651194627, 192.5408628639999051 ) ) ;
#106663 = DIRECTION ( 'NONE',  ( 0.000000000000000000, 1.000000000000000000, 0.000000000000000000 ) ) ;
#106664 = CIRCLE ( 'NONE', #65328, 6.999999999999992895 ) ;
#106665 = DIRECTION ( 'NONE',  ( 0.000000000000000000, 0.000000000000000000, -1.000000000000000000 ) ) ;
#106666 = ORIENTED_EDGE ( 'NONE', *, *, #48029, .F. ) ;
#106667 = CARTESIAN_POINT ( 'NONE',  ( 79.56493839289275627, -57.67121238173562148, -30.45972677269765327 ) ) ;
#106668 = CARTESIAN_POINT ( 'NONE',  ( -17.49999999999999645, 2.500000000000000444, 0.000000000000000000 ) ) ;
#106669 = DIRECTION ( 'NONE',  ( 1.000000000000000000, 1.224606353822377258E-16, 0.000000000000000000 ) ) ;
#106670 = CARTESIAN_POINT ( 'NONE',  ( 25.11650669486618881, 1.474610560812782335E-15, 0.000000000000000000 ) ) ;
#106671 = CARTESIAN_POINT ( 'NONE',  ( -81.37744105750925883, -30.00000000000000711, -10.21548990795500522 ) ) ;
#106672 = EDGE_CURVE ( 'NONE', #71545, #91694, #76175, .T. ) ;
#106673 = ADVANCED_FACE ( 'NONE', ( #67355 ), #64128, .T. ) ;
#106674 = CARTESIAN_POINT ( 'NONE',  ( -83.79209681126675946, -37.99999999999999289, 174.8870184814763036 ) ) ;
#106675 = CARTESIAN_POINT ( 'NONE',  ( -2.617993873628169599, -5.000000000000000000, -10.00000000000000000 ) ) ;
#106676 = CARTESIAN_POINT ( 'NONE',  ( 0.000000000000000000, 80.00000000000000000, -65.50000000000000000 ) ) ;
#106677 = COLOUR_RGB ( '', 0.66274510, 0.83137255, 0.94901961) ;
#106678 = DIRECTION ( 'NONE',  ( 0.000000000000000000, 1.000000000000000000, 0.000000000000000000 ) ) ;
#106679 = EDGE_CURVE ( 'NONE', #76929, #42491, #36586, .T. ) ;
#106680 = DIRECTION ( 'NONE',  ( -1.000000000000000000, 0.000000000000000000, 0.000000000000000000 ) ) ;
#106681 = CARTESIAN_POINT ( 'NONE',  ( -28.46824965450743150, 18.16842165451065227, 40.55076743663460093 ) ) ;
#106682 =( LENGTH_UNIT ( ) NAMED_UNIT ( * ) SI_UNIT ( .MILLI., .METRE. ) );
#106683 = DIRECTION ( 'NONE',  ( -1.000000000000000000, -1.224606353822377258E-16, -0.000000000000000000 ) ) ;
#106684 = CARTESIAN_POINT ( 'NONE',  ( -21.96339186788464204, 25.92483237897061699, 31.82890721654192845 ) ) ;
#106685 = CIRCLE ( 'NONE', #87769, 8.000000000000000000 ) ;
#106686 = CARTESIAN_POINT ( 'NONE',  ( -99.45001380552274384, -38.00000000000004974, 191.4583679090391684 ) ) ;
#106687 = ADVANCED_FACE ( 'NONE', ( #434 ), #67894, .T. ) ;
#106688 = ORIENTED_EDGE ( 'NONE', *, *, #12154, .F. ) ;
#106689 = DIRECTION ( 'NONE',  ( -1.000000000000000000, -1.224606353822377258E-16, -0.000000000000000000 ) ) ;
#106690 = CARTESIAN_POINT ( 'NONE',  ( 4.590682673078522846, -63.93208242687840936, 3.864023243754609371 ) ) ;
#106692 = CARTESIAN_POINT ( 'NONE',  ( -66.35739722136700891, -34.58948124108970745, -23.23708708512139509 ) ) ;
#106691 = LINE ( 'NONE', #32841, #98339 ) ;
#106693 = EDGE_LOOP ( 'NONE', ( #46642, #27334, #75865, #49272, #102054, #79035 ) ) ;
#106694 = AXIS2_PLACEMENT_3D ( 'NONE', #60202, #91486, #18135 ) ;
#106695 = VECTOR ( 'NONE', #67820, 1000.000000000000000 ) ;
#106696 = VERTEX_POINT ( 'NONE', #44140 ) ;
#106697 = CARTESIAN_POINT ( 'NONE',  ( 11.08349330513380515, 4.000000000000003553, 0.000000000000000000 ) ) ;
#106698 = VECTOR ( 'NONE', #58980, 1000.000000000000000 ) ;
#106699 = SURFACE_SIDE_STYLE ('',( #64659 ) ) ;
#106700 = CARTESIAN_POINT ( 'NONE',  ( 15.90614609307868577, -4.000000000000003553, 18.57417562100670949 ) ) ;
#106701 = CARTESIAN_POINT ( 'NONE',  ( -66.14035079976200393, -60.00000000000000000, -33.84619808995684309 ) ) ;
#106702 = ORIENTED_EDGE ( 'NONE', *, *, #33654, .F. ) ;
#106703 = CARTESIAN_POINT ( 'NONE',  ( -1.469576158976823947E-15, -17.37499999999999289, 8.000000000000000000 ) ) ;
#106704 = CARTESIAN_POINT ( 'NONE',  ( -9.789044728060147804, 294.6486233851416614, -2.043184600577789833 ) ) ;
#106705 = CARTESIAN_POINT ( 'NONE',  ( 99.19867269638797325, -45.26832955309748030, 193.2066468836933382 ) ) ;
#106707 = CARTESIAN_POINT ( 'NONE',  ( -47.29368197624727088, 13.12573487771091152, 14.58950938768687777 ) ) ;
#106706 = FACE_OUTER_BOUND ( 'NONE', #9950, .T. ) ;
#106708 = CIRCLE ( 'NONE', #37861, 7.981862520314372489 ) ;
#106709 = ORIENTED_EDGE ( 'NONE', *, *, #14362, .F. ) ;
#106710 = EDGE_LOOP ( 'NONE', ( #10660, #45193 ) ) ;
#106711 = ORIENTED_EDGE ( 'NONE', *, *, #53240, .F. ) ;
#106712 = CARTESIAN_POINT ( 'NONE',  ( 28.62099872728884264, 319.6015458412052794, 13.57403514487685392 ) ) ;
#106713 = TOROIDAL_SURFACE ( 'NONE', #46525, 11.00000000000000000, 2.000000000000000000 ) ;
#106714 = CARTESIAN_POINT ( 'NONE',  ( -5.000000000000000000, -13.96166769374574024, 11.51022196660654195 ) ) ;
#106715 = DIRECTION ( 'NONE',  ( -1.000000000000000000, -1.224606353822377258E-16, -0.000000000000000000 ) ) ;
#106716 = ORIENTED_EDGE ( 'NONE', *, *, #65794, .F. ) ;
#106717 = EDGE_CURVE ( 'NONE', #21366, #17909, #7267, .T. ) ;
#106718 = CARTESIAN_POINT ( 'NONE',  ( 15.64519568958359308, 46.18931709473498159, -4.637408661950145117 ) ) ;
#106719 = CARTESIAN_POINT ( 'NONE',  ( -6.011841252072293477E-15, 27.55047179872464724, 49.09040922050319011 ) ) ;
#106720 = CARTESIAN_POINT ( 'NONE',  ( 0.000000000000000000, -6.928203230275509661, -3.999999999999999112 ) ) ;
#106721 = CARTESIAN_POINT ( 'NONE',  ( -61.06992298392258078, -57.67755795743399716, 111.0944920020532862 ) ) ;
#106722 = CARTESIAN_POINT ( 'NONE',  ( -7.188101187500000044, -33.40625000204838813, -8.802885111219163269E-16 ) ) ;
#106723 = CARTESIAN_POINT ( 'NONE',  ( -29.99961410214337576, 17.76511157208308234, 39.64372791628625947 ) ) ;
#106724 = CARTESIAN_POINT ( 'NONE',  ( -24.80105969489321893, 306.0237540681346218, -9.745911707960095427 ) ) ;
#106725 = CARTESIAN_POINT ( 'NONE',  ( 1.093227907231550722, 27.52357886411307319, -40.11142487546388935 ) ) ;
#106726 = CARTESIAN_POINT ( 'NONE',  ( 8.180134260905338905, -14.21045842199436926, -37.25106736021741227 ) ) ;
#106727 = EDGE_CURVE ( 'NONE', #27940, #88651, #15181, .T. ) ;
#106729 = ADVANCED_FACE ( 'NONE', ( #60861 ), #55455, .T. ) ;
#106728 = CARTESIAN_POINT ( 'NONE',  ( -43.55333112596419909, 465.2342844084849389, 9.238213423004411951 ) ) ;
#106730 = CARTESIAN_POINT ( 'NONE',  ( -51.87710858498652300, -39.51066125304492260, 54.03131810460910600 ) ) ;
#106731 = CIRCLE ( 'NONE', #105062, 10.00000000000000178 ) ;
#106732 = ORIENTED_EDGE ( 'NONE', *, *, #43628, .T. ) ;
#106733 = CARTESIAN_POINT ( 'NONE',  ( -98.99772353281480264, -45.25013960604325547, 193.3232175602864231 ) ) ;
#106734 = CARTESIAN_POINT ( 'NONE',  ( -0.1244055672601159790, 295.1039051330173493, -10.00000000000143530 ) ) ;
#106735 = CIRCLE ( 'NONE', #53333, 5.000000000000001776 ) ;
#106736 = CARTESIAN_POINT ( 'NONE',  ( 15.00756260254757990, -0.09903668703488825720, 15.00122431754954810 ) ) ;
#106737 = ORIENTED_EDGE ( 'NONE', *, *, #82665, .T. ) ;
#106738 = CARTESIAN_POINT ( 'NONE',  ( -16.64348903516517098, 43.75610143575153899, 4.157797401561652784 ) ) ;
#106739 = CARTESIAN_POINT ( 'NONE',  ( 89.50843841616533325, -38.52256170111905220, 200.4442316066328260 ) ) ;
#106740 = LINE ( 'NONE', #23204, #70967 ) ;
#106741 = CARTESIAN_POINT ( 'NONE',  ( 95.42421628608209971, 1.030564683017419500E-14, 0.000000000000000000 ) ) ;
#106742 = DIRECTION ( 'NONE',  ( 0.000000000000000000, 0.000000000000000000, 1.000000000000000000 ) ) ;
#106743 = FACE_OUTER_BOUND ( 'NONE', #101214, .T. ) ;
#106744 = CARTESIAN_POINT ( 'NONE',  ( 82.54044539369691336, -30.00000000000000355, 149.6189146675613415 ) ) ;
#106745 = CARTESIAN_POINT ( 'NONE',  ( 36.94051212421975805, 491.4300504572173054, 12.31983948577891397 ) ) ;
#106746 = CARTESIAN_POINT ( 'NONE',  ( -29.68315524076956180, 8.302504244945341227, 42.10535821593508388 ) ) ;
#106747 = DIRECTION ( 'NONE',  ( 1.000000000000000000, 0.000000000000000000, 0.000000000000000000 ) ) ;
#106748 = EDGE_CURVE ( 'NONE', #78599, #31379, #73054, .T. ) ;
#106749 = EDGE_LOOP ( 'NONE', ( #79340, #12594, #64870, #20560, #45820 ) ) ;
#106750 = EDGE_LOOP ( 'NONE', ( #49878, #95777, #4271, #71821, #33968 ) ) ;
#106751 = CARTESIAN_POINT ( 'NONE',  ( 49.43331438854296778, -32.59166132229344726, 47.58368122656079890 ) ) ;
#106752 = CARTESIAN_POINT ( 'NONE',  ( 6.232496355896458340, 41.83455062734740437, -59.02481358918409171 ) ) ;
#106753 = CIRCLE ( 'NONE', #34514, 5.000000000000001776 ) ;
#106754 = CARTESIAN_POINT ( 'NONE',  ( 37.24671046105844852, 27.99421627048664973, -10.98692623331827356 ) ) ;
#106755 = EDGE_CURVE ( 'NONE', #74216, #68599, #38710, .T. ) ;
#106756 = VERTEX_POINT ( 'NONE', #72644 ) ;
#106757 = CARTESIAN_POINT ( 'NONE',  ( -92.64360711281031513, -38.35495908042472024, 40.47194345170088070 ) ) ;
#106758 = ORIENTED_EDGE ( 'NONE', *, *, #73892, .F. ) ;
#106759 = FILL_AREA_STYLE_COLOUR ( '', #20617 ) ;
#106760 = CARTESIAN_POINT ( 'NONE',  ( 98.46909904549914927, -38.35583610091571671, 79.42329170081190171 ) ) ;
#106761 = CARTESIAN_POINT ( 'NONE',  ( 15.57101515226550958, 22.98847347788403539, 0.5602172340486083479 ) ) ;
#106762 = CARTESIAN_POINT ( 'NONE',  ( 103.0583287818154048, -60.15111231639958334, 134.7092673011946147 ) ) ;
#106763 = DIRECTION ( 'NONE',  ( 1.000000000000000000, 1.224606353822377258E-16, 0.000000000000000000 ) ) ;
#106764 = CARTESIAN_POINT ( 'NONE',  ( 22.89193641261745427, 27.46073252125953701, 33.16577871831020730 ) ) ;
#106765 = CARTESIAN_POINT ( 'NONE',  ( -32.90191502941880231, 322.8794145886470233, -4.587724655176066868 ) ) ;
#106766 = FACE_OUTER_BOUND ( 'NONE', #55004, .T. ) ;
#106767 = EDGE_CURVE ( 'NONE', #39668, #60839, #15469, .T. ) ;
#106768 = CARTESIAN_POINT ( 'NONE',  ( 74.39885652900197499, -60.00000000000000000, 176.1565043745205230 ) ) ;
#106769 = CARTESIAN_POINT ( 'NONE',  ( -43.28401190482631478, 435.3393147692558500, 9.722488360058175516 ) ) ;
#106770 = ORIENTED_EDGE ( 'NONE', *, *, #8287, .T. ) ;
#106771 = CARTESIAN_POINT ( 'NONE',  ( 60.51310404470154225, -39.48713381824052959, 73.58315150410720662 ) ) ;
#106772 = CARTESIAN_POINT ( 'NONE',  ( -23.31543317473521526, 295.1959631832629043, -1.926156989552331167 ) ) ;
#106773 = CARTESIAN_POINT ( 'NONE',  ( 9.822490609848976817, -50.52957752397126967, 25.11095637839896000 ) ) ;
#106774 = CARTESIAN_POINT ( 'NONE',  ( -9.483106265414438241, -5.000000000000000000, -19.87317390814893869 ) ) ;
#106776 = CARTESIAN_POINT ( 'NONE',  ( -4.329583349659062996, 54.29296960176466058, 6.476735382064108926 ) ) ;
#106775 = CARTESIAN_POINT ( 'NONE',  ( -64.15115902790869029, -29.99999999991991828, 104.9769517853171976 ) ) ;
#106777 = CARTESIAN_POINT ( 'NONE',  ( -32.17878052566634750, 336.4077344679339490, 18.01554293220755909 ) ) ;
#106778 = DIRECTION ( 'NONE',  ( 0.000000000000000000, 0.000000000000000000, 1.000000000000000000 ) ) ;
#106779 = CARTESIAN_POINT ( 'NONE',  ( -42.25157195694011136, 464.6564439579760801, 16.40419412090410134 ) ) ;
#106780 = CARTESIAN_POINT ( 'NONE',  ( 5.656854249492380582, -33.31249999999999289, -5.656854249492379694 ) ) ;
#106781 = CARTESIAN_POINT ( 'NONE',  ( -8.737863884121843228, -3.000000000000002665, -79.96381019768948306 ) ) ;
#106782 = AXIS2_PLACEMENT_3D ( 'NONE', #64521, #104979, #38662 ) ;
#106783 = B_SPLINE_CURVE_WITH_KNOTS ( 'NONE', 3,
 ( #21426, #54807, #94234, #87739 ),
 .UNSPECIFIED., .F., .F.,
 ( 4, 4 ),
 ( 0.000000000000000000, 0.001019617110105292294 ),
 .UNSPECIFIED. ) ;
#106784 = FACE_OUTER_BOUND ( 'NONE', #8006, .T. ) ;
#2565 = CARTESIAN_POINT ( 'NONE',  ( 18.58349330513380337, -7.703719777548943412E-31, 4.000000000000001776 ) ) ;
#106786 = NEXT_ASSEMBLY_USAGE_OCCURRENCE ( 'NAUO1', ' ', ' ', #102301, #17933, $ ) ;
#106787 = NEXT_ASSEMBLY_USAGE_OCCURRENCE ( 'NAUO2', ' ', ' ', #102301, #73291, $ ) ;
#106788 = NEXT_ASSEMBLY_USAGE_OCCURRENCE ( 'NAUO3', ' ', ' ', #102301, #30479, $ ) ;
#106789 = NEXT_ASSEMBLY_USAGE_OCCURRENCE ( 'NAUO4', ' ', ' ', #102301, #27211, $ ) ;
#106790 = NEXT_ASSEMBLY_USAGE_OCCURRENCE ( 'NAUO5', ' ', ' ', #102301, #65408, $ ) ;
#106791 = NEXT_ASSEMBLY_USAGE_OCCURRENCE ( 'NAUO6', ' ', ' ', #102301, #15959, $ ) ;
#106792 = NEXT_ASSEMBLY_USAGE_OCCURRENCE ( 'NAUO7', ' ', ' ', #102301, #19320, $ ) ;
#106793 = NEXT_ASSEMBLY_USAGE_OCCURRENCE ( 'NAUO8', ' ', ' ', #102301, #23923, $ ) ;
#106794 = NEXT_ASSEMBLY_USAGE_OCCURRENCE ( 'NAUO9', ' ', ' ', #102301, #8033, $ ) ;
#106795 = NEXT_ASSEMBLY_USAGE_OCCURRENCE ( 'NAUO10', ' ', ' ', #102301, #76584, $ ) ;
#106796 = NEXT_ASSEMBLY_USAGE_OCCURRENCE ( 'NAUO11', ' ', ' ', #102301, #39722, $ ) ;
#106797 = NEXT_ASSEMBLY_USAGE_OCCURRENCE ( 'NAUO12', ' ', ' ', #102301, #76584, $ ) ;
#106798 = NEXT_ASSEMBLY_USAGE_OCCURRENCE ( 'NAUO13', ' ', ' ', #102301, #39722, $ ) ;
#106799 = NEXT_ASSEMBLY_USAGE_OCCURRENCE ( 'NAUO14', ' ', ' ', #102301, #43009, $ ) ;
#106800 = NEXT_ASSEMBLY_USAGE_OCCURRENCE ( 'NAUO15', ' ', ' ', #102301, #12664, $ ) ;
#106801 = NEXT_ASSEMBLY_USAGE_OCCURRENCE ( 'NAUO16', ' ', ' ', #102301, #12664, $ ) ;
#106802 = NEXT_ASSEMBLY_USAGE_OCCURRENCE ( 'NAUO17', ' ', ' ', #102301, #95727, $ ) ;
#106803 = NEXT_ASSEMBLY_USAGE_OCCURRENCE ( 'NAUO18', ' ', ' ', #102301, #105582, $ ) ;
#106804 = NEXT_ASSEMBLY_USAGE_OCCURRENCE ( 'NAUO19', ' ', ' ', #102301, #52852, $ ) ;
#106805 = NEXT_ASSEMBLY_USAGE_OCCURRENCE ( 'NAUO20', ' ', ' ', #102301, #39722, $ ) ;
#106806 = NEXT_ASSEMBLY_USAGE_OCCURRENCE ( 'NAUO21', ' ', ' ', #102301, #98978, $ ) ;
#106807 = NEXT_ASSEMBLY_USAGE_OCCURRENCE ( 'NAUO22', ' ', ' ', #102301, #81205, $ ) ;
#106808 = NEXT_ASSEMBLY_USAGE_OCCURRENCE ( 'NAUO23', ' ', ' ', #102301, #50892, $ ) ;
#106809 = NEXT_ASSEMBLY_USAGE_OCCURRENCE ( 'NAUO24', ' ', ' ', #102301, #39722, $ ) ;
#106810 = NEXT_ASSEMBLY_USAGE_OCCURRENCE ( 'NAUO25', ' ', ' ', #102301, #54175, $ ) ;
#106811 = NEXT_ASSEMBLY_USAGE_OCCURRENCE ( 'NAUO26', ' ', ' ', #102301, #54175, $ ) ;
#106812 = NEXT_ASSEMBLY_USAGE_OCCURRENCE ( 'NAUO27', ' ', ' ', #102301, #98978, $ ) ;
#106813 = NEXT_ASSEMBLY_USAGE_OCCURRENCE ( 'NAUO28', ' ', ' ', #102301, #98978, $ ) ;
#106814 = NEXT_ASSEMBLY_USAGE_OCCURRENCE ( 'NAUO29', ' ', ' ', #102301, #103634, $ ) ;
#106815 = NEXT_ASSEMBLY_USAGE_OCCURRENCE ( 'NAUO30', ' ', ' ', #102301, #58835, $ ) ;
#106816 = NEXT_ASSEMBLY_USAGE_OCCURRENCE ( 'NAUO31', ' ', ' ', #102301, #25882, $ ) ;
#106817 = NEXT_ASSEMBLY_USAGE_OCCURRENCE ( 'NAUO32', ' ', ' ', #102301, #6702, $ ) ;
#106818 = NEXT_ASSEMBLY_USAGE_OCCURRENCE ( 'NAUO33', ' ', ' ', #102301, #6702, $ ) ;
#106819 = NEXT_ASSEMBLY_USAGE_OCCURRENCE ( 'NAUO34', ' ', ' ', #102301, #6702, $ ) ;
#106820 = NEXT_ASSEMBLY_USAGE_OCCURRENCE ( 'NAUO35', ' ', ' ', #102301, #6702, $ ) ;
ENDSEC;
END-ISO-10303-21;
